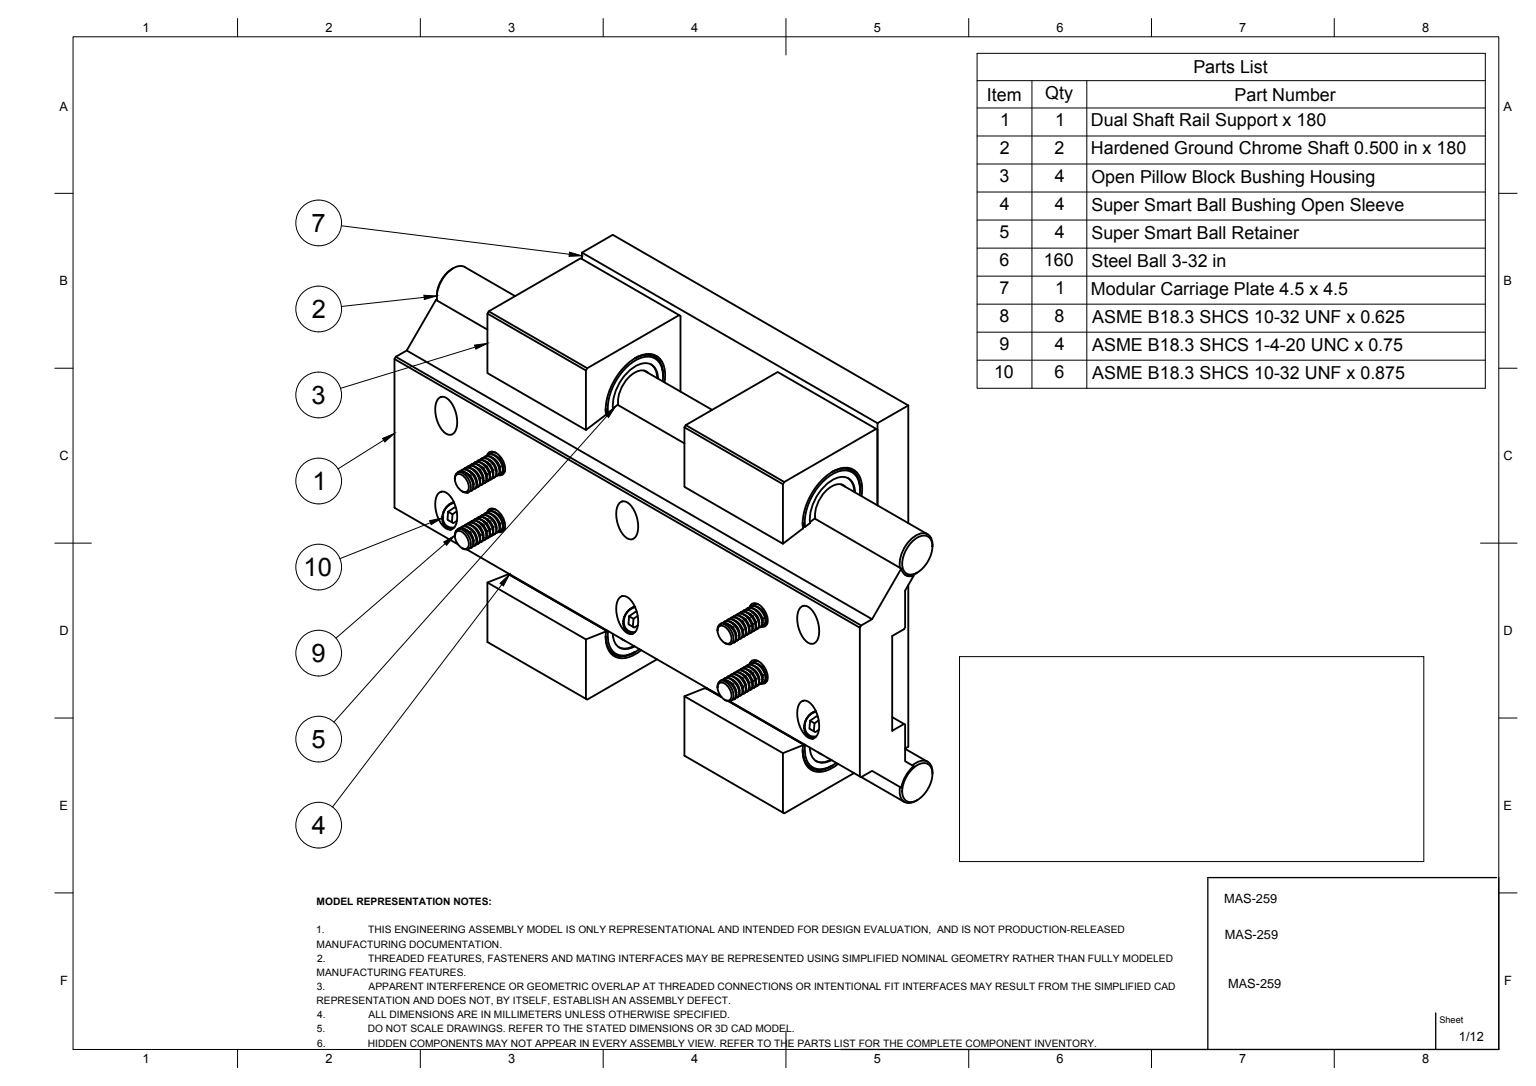
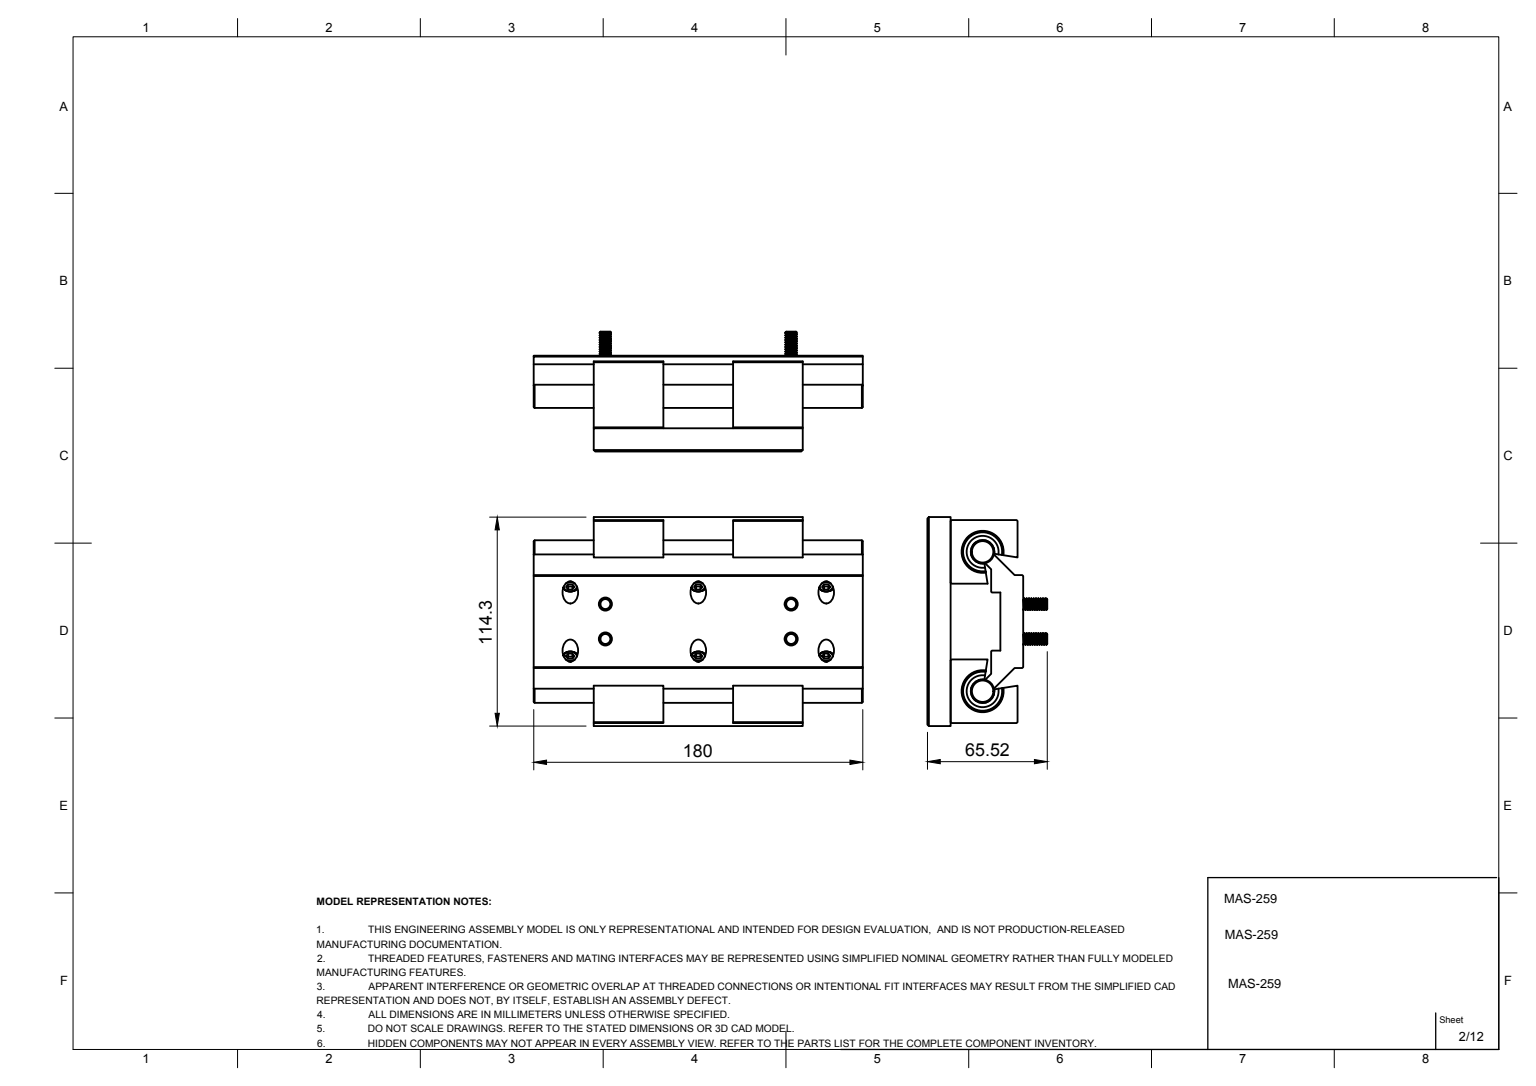
ISO-10303-21;
HEADER;
/* Generated by software containing ST-Developer
 * from STEP Tools, Inc. (www.steptools.com) 
 */

FILE_DESCRIPTION(
/* description */ (''),
/* implementation_level */ '2;1');

FILE_NAME(
/* name */ 'MAS-259',
/* time_stamp */ '2026-10-15T13:30:17-07:00',
/* author */ (''),
/* organization */ (''),
/* preprocessor_version */ 'ST-DEVELOPER v20.2',
/* originating_system */ 'Autodesk Translation Framework v15.15.0.0',
/* authorisation */ '');

FILE_SCHEMA (('AUTOMOTIVE_DESIGN { 1 0 10303 214 3 1 1 }'));
ENDSEC;

DATA;
#10=MECHANICAL_DESIGN_GEOMETRIC_PRESENTATION_REPRESENTATION('',(#1033,#1034,
#1035,#1036,#1037,#1038,#1039,#1040,#1041,#1042),#71795);
#11=ITEM_DEFINED_TRANSFORMATION($,$,#13757,#14849);
#12=ITEM_DEFINED_TRANSFORMATION($,$,#13993,#14850);
#13=ITEM_DEFINED_TRANSFORMATION($,$,#14012,#14851);
#14=ITEM_DEFINED_TRANSFORMATION($,$,#14045,#14852);
#15=ITEM_DEFINED_TRANSFORMATION($,$,#14060,#14853);
#16=ITEM_DEFINED_TRANSFORMATION($,$,#14111,#14854);
#17=ITEM_DEFINED_TRANSFORMATION($,$,#13854,#14855);
#18=ITEM_DEFINED_TRANSFORMATION($,$,#14114,#14856);
#19=ITEM_DEFINED_TRANSFORMATION($,$,#14610,#14857);
#20=ITEM_DEFINED_TRANSFORMATION($,$,#14358,#14858);
#21=ITEM_DEFINED_TRANSFORMATION($,$,#13993,#14859);
#22=ITEM_DEFINED_TRANSFORMATION($,$,#14012,#14860);
#23=ITEM_DEFINED_TRANSFORMATION($,$,#14012,#14861);
#24=ITEM_DEFINED_TRANSFORMATION($,$,#14012,#14862);
#25=ITEM_DEFINED_TRANSFORMATION($,$,#14045,#14863);
#26=ITEM_DEFINED_TRANSFORMATION($,$,#14045,#14864);
#27=ITEM_DEFINED_TRANSFORMATION($,$,#14045,#14865);
#28=ITEM_DEFINED_TRANSFORMATION($,$,#14060,#14866);
#29=ITEM_DEFINED_TRANSFORMATION($,$,#14060,#14867);
#30=ITEM_DEFINED_TRANSFORMATION($,$,#14060,#14868);
#31=ITEM_DEFINED_TRANSFORMATION($,$,#14111,#14869);
#32=ITEM_DEFINED_TRANSFORMATION($,$,#14111,#14870);
#33=ITEM_DEFINED_TRANSFORMATION($,$,#14111,#14871);
#34=ITEM_DEFINED_TRANSFORMATION($,$,#14111,#14872);
#35=ITEM_DEFINED_TRANSFORMATION($,$,#14111,#14873);
#36=ITEM_DEFINED_TRANSFORMATION($,$,#14111,#14874);
#37=ITEM_DEFINED_TRANSFORMATION($,$,#14111,#14875);
#38=ITEM_DEFINED_TRANSFORMATION($,$,#14111,#14876);
#39=ITEM_DEFINED_TRANSFORMATION($,$,#14111,#14877);
#40=ITEM_DEFINED_TRANSFORMATION($,$,#14111,#14878);
#41=ITEM_DEFINED_TRANSFORMATION($,$,#14111,#14879);
#42=ITEM_DEFINED_TRANSFORMATION($,$,#14111,#14880);
#43=ITEM_DEFINED_TRANSFORMATION($,$,#14111,#14881);
#44=ITEM_DEFINED_TRANSFORMATION($,$,#14111,#14882);
#45=ITEM_DEFINED_TRANSFORMATION($,$,#14111,#14883);
#46=ITEM_DEFINED_TRANSFORMATION($,$,#14111,#14884);
#47=ITEM_DEFINED_TRANSFORMATION($,$,#14111,#14885);
#48=ITEM_DEFINED_TRANSFORMATION($,$,#14111,#14886);
#49=ITEM_DEFINED_TRANSFORMATION($,$,#14111,#14887);
#50=ITEM_DEFINED_TRANSFORMATION($,$,#14111,#14888);
#51=ITEM_DEFINED_TRANSFORMATION($,$,#14111,#14889);
#52=ITEM_DEFINED_TRANSFORMATION($,$,#14111,#14890);
#53=ITEM_DEFINED_TRANSFORMATION($,$,#14111,#14891);
#54=ITEM_DEFINED_TRANSFORMATION($,$,#14111,#14892);
#55=ITEM_DEFINED_TRANSFORMATION($,$,#14111,#14893);
#56=ITEM_DEFINED_TRANSFORMATION($,$,#14111,#14894);
#57=ITEM_DEFINED_TRANSFORMATION($,$,#14111,#14895);
#58=ITEM_DEFINED_TRANSFORMATION($,$,#14111,#14896);
#59=ITEM_DEFINED_TRANSFORMATION($,$,#14111,#14897);
#60=ITEM_DEFINED_TRANSFORMATION($,$,#14111,#14898);
#61=ITEM_DEFINED_TRANSFORMATION($,$,#14111,#14899);
#62=ITEM_DEFINED_TRANSFORMATION($,$,#14111,#14900);
#63=ITEM_DEFINED_TRANSFORMATION($,$,#14111,#14901);
#64=ITEM_DEFINED_TRANSFORMATION($,$,#14111,#14902);
#65=ITEM_DEFINED_TRANSFORMATION($,$,#14111,#14903);
#66=ITEM_DEFINED_TRANSFORMATION($,$,#14111,#14904);
#67=ITEM_DEFINED_TRANSFORMATION($,$,#14111,#14905);
#68=ITEM_DEFINED_TRANSFORMATION($,$,#14111,#14906);
#69=ITEM_DEFINED_TRANSFORMATION($,$,#14111,#14907);
#70=ITEM_DEFINED_TRANSFORMATION($,$,#14111,#14908);
#71=ITEM_DEFINED_TRANSFORMATION($,$,#14111,#14909);
#72=ITEM_DEFINED_TRANSFORMATION($,$,#14111,#14910);
#73=ITEM_DEFINED_TRANSFORMATION($,$,#14111,#14911);
#74=ITEM_DEFINED_TRANSFORMATION($,$,#14111,#14912);
#75=ITEM_DEFINED_TRANSFORMATION($,$,#14111,#14913);
#76=ITEM_DEFINED_TRANSFORMATION($,$,#14111,#14914);
#77=ITEM_DEFINED_TRANSFORMATION($,$,#14111,#14915);
#78=ITEM_DEFINED_TRANSFORMATION($,$,#14111,#14916);
#79=ITEM_DEFINED_TRANSFORMATION($,$,#14111,#14917);
#80=ITEM_DEFINED_TRANSFORMATION($,$,#14111,#14918);
#81=ITEM_DEFINED_TRANSFORMATION($,$,#14111,#14919);
#82=ITEM_DEFINED_TRANSFORMATION($,$,#14111,#14920);
#83=ITEM_DEFINED_TRANSFORMATION($,$,#14111,#14921);
#84=ITEM_DEFINED_TRANSFORMATION($,$,#14111,#14922);
#85=ITEM_DEFINED_TRANSFORMATION($,$,#14111,#14923);
#86=ITEM_DEFINED_TRANSFORMATION($,$,#14111,#14924);
#87=ITEM_DEFINED_TRANSFORMATION($,$,#14111,#14925);
#88=ITEM_DEFINED_TRANSFORMATION($,$,#14111,#14926);
#89=ITEM_DEFINED_TRANSFORMATION($,$,#14111,#14927);
#90=ITEM_DEFINED_TRANSFORMATION($,$,#14111,#14928);
#91=ITEM_DEFINED_TRANSFORMATION($,$,#14111,#14929);
#92=ITEM_DEFINED_TRANSFORMATION($,$,#14111,#14930);
#93=ITEM_DEFINED_TRANSFORMATION($,$,#14111,#14931);
#94=ITEM_DEFINED_TRANSFORMATION($,$,#14111,#14932);
#95=ITEM_DEFINED_TRANSFORMATION($,$,#14111,#14933);
#96=ITEM_DEFINED_TRANSFORMATION($,$,#14111,#14934);
#97=ITEM_DEFINED_TRANSFORMATION($,$,#14111,#14935);
#98=ITEM_DEFINED_TRANSFORMATION($,$,#14111,#14936);
#99=ITEM_DEFINED_TRANSFORMATION($,$,#14111,#14937);
#100=ITEM_DEFINED_TRANSFORMATION($,$,#14111,#14938);
#101=ITEM_DEFINED_TRANSFORMATION($,$,#14111,#14939);
#102=ITEM_DEFINED_TRANSFORMATION($,$,#14111,#14940);
#103=ITEM_DEFINED_TRANSFORMATION($,$,#14111,#14941);
#104=ITEM_DEFINED_TRANSFORMATION($,$,#14111,#14942);
#105=ITEM_DEFINED_TRANSFORMATION($,$,#14111,#14943);
#106=ITEM_DEFINED_TRANSFORMATION($,$,#14111,#14944);
#107=ITEM_DEFINED_TRANSFORMATION($,$,#14111,#14945);
#108=ITEM_DEFINED_TRANSFORMATION($,$,#14111,#14946);
#109=ITEM_DEFINED_TRANSFORMATION($,$,#14111,#14947);
#110=ITEM_DEFINED_TRANSFORMATION($,$,#14111,#14948);
#111=ITEM_DEFINED_TRANSFORMATION($,$,#14111,#14949);
#112=ITEM_DEFINED_TRANSFORMATION($,$,#14111,#14950);
#113=ITEM_DEFINED_TRANSFORMATION($,$,#14111,#14951);
#114=ITEM_DEFINED_TRANSFORMATION($,$,#14111,#14952);
#115=ITEM_DEFINED_TRANSFORMATION($,$,#14111,#14953);
#116=ITEM_DEFINED_TRANSFORMATION($,$,#14111,#14954);
#117=ITEM_DEFINED_TRANSFORMATION($,$,#14111,#14955);
#118=ITEM_DEFINED_TRANSFORMATION($,$,#14111,#14956);
#119=ITEM_DEFINED_TRANSFORMATION($,$,#14111,#14957);
#120=ITEM_DEFINED_TRANSFORMATION($,$,#14111,#14958);
#121=ITEM_DEFINED_TRANSFORMATION($,$,#14111,#14959);
#122=ITEM_DEFINED_TRANSFORMATION($,$,#14111,#14960);
#123=ITEM_DEFINED_TRANSFORMATION($,$,#14111,#14961);
#124=ITEM_DEFINED_TRANSFORMATION($,$,#14111,#14962);
#125=ITEM_DEFINED_TRANSFORMATION($,$,#14111,#14963);
#126=ITEM_DEFINED_TRANSFORMATION($,$,#14111,#14964);
#127=ITEM_DEFINED_TRANSFORMATION($,$,#14111,#14965);
#128=ITEM_DEFINED_TRANSFORMATION($,$,#14111,#14966);
#129=ITEM_DEFINED_TRANSFORMATION($,$,#14111,#14967);
#130=ITEM_DEFINED_TRANSFORMATION($,$,#14111,#14968);
#131=ITEM_DEFINED_TRANSFORMATION($,$,#14111,#14969);
#132=ITEM_DEFINED_TRANSFORMATION($,$,#14111,#14970);
#133=ITEM_DEFINED_TRANSFORMATION($,$,#14111,#14971);
#134=ITEM_DEFINED_TRANSFORMATION($,$,#14111,#14972);
#135=ITEM_DEFINED_TRANSFORMATION($,$,#14111,#14973);
#136=ITEM_DEFINED_TRANSFORMATION($,$,#14111,#14974);
#137=ITEM_DEFINED_TRANSFORMATION($,$,#14111,#14975);
#138=ITEM_DEFINED_TRANSFORMATION($,$,#14111,#14976);
#139=ITEM_DEFINED_TRANSFORMATION($,$,#14111,#14977);
#140=ITEM_DEFINED_TRANSFORMATION($,$,#14111,#14978);
#141=ITEM_DEFINED_TRANSFORMATION($,$,#14111,#14979);
#142=ITEM_DEFINED_TRANSFORMATION($,$,#14111,#14980);
#143=ITEM_DEFINED_TRANSFORMATION($,$,#14111,#14981);
#144=ITEM_DEFINED_TRANSFORMATION($,$,#14111,#14982);
#145=ITEM_DEFINED_TRANSFORMATION($,$,#14111,#14983);
#146=ITEM_DEFINED_TRANSFORMATION($,$,#14111,#14984);
#147=ITEM_DEFINED_TRANSFORMATION($,$,#14111,#14985);
#148=ITEM_DEFINED_TRANSFORMATION($,$,#14111,#14986);
#149=ITEM_DEFINED_TRANSFORMATION($,$,#14111,#14987);
#150=ITEM_DEFINED_TRANSFORMATION($,$,#14111,#14988);
#151=ITEM_DEFINED_TRANSFORMATION($,$,#14111,#14989);
#152=ITEM_DEFINED_TRANSFORMATION($,$,#14111,#14990);
#153=ITEM_DEFINED_TRANSFORMATION($,$,#14111,#14991);
#154=ITEM_DEFINED_TRANSFORMATION($,$,#14111,#14992);
#155=ITEM_DEFINED_TRANSFORMATION($,$,#14111,#14993);
#156=ITEM_DEFINED_TRANSFORMATION($,$,#14111,#14994);
#157=ITEM_DEFINED_TRANSFORMATION($,$,#14111,#14995);
#158=ITEM_DEFINED_TRANSFORMATION($,$,#14111,#14996);
#159=ITEM_DEFINED_TRANSFORMATION($,$,#14111,#14997);
#160=ITEM_DEFINED_TRANSFORMATION($,$,#14111,#14998);
#161=ITEM_DEFINED_TRANSFORMATION($,$,#14111,#14999);
#162=ITEM_DEFINED_TRANSFORMATION($,$,#14111,#15000);
#163=ITEM_DEFINED_TRANSFORMATION($,$,#14111,#15001);
#164=ITEM_DEFINED_TRANSFORMATION($,$,#14111,#15002);
#165=ITEM_DEFINED_TRANSFORMATION($,$,#14111,#15003);
#166=ITEM_DEFINED_TRANSFORMATION($,$,#14111,#15004);
#167=ITEM_DEFINED_TRANSFORMATION($,$,#14111,#15005);
#168=ITEM_DEFINED_TRANSFORMATION($,$,#14111,#15006);
#169=ITEM_DEFINED_TRANSFORMATION($,$,#14111,#15007);
#170=ITEM_DEFINED_TRANSFORMATION($,$,#14111,#15008);
#171=ITEM_DEFINED_TRANSFORMATION($,$,#14111,#15009);
#172=ITEM_DEFINED_TRANSFORMATION($,$,#14111,#15010);
#173=ITEM_DEFINED_TRANSFORMATION($,$,#14111,#15011);
#174=ITEM_DEFINED_TRANSFORMATION($,$,#14111,#15012);
#175=ITEM_DEFINED_TRANSFORMATION($,$,#14111,#15013);
#176=ITEM_DEFINED_TRANSFORMATION($,$,#14111,#15014);
#177=ITEM_DEFINED_TRANSFORMATION($,$,#14111,#15015);
#178=ITEM_DEFINED_TRANSFORMATION($,$,#14111,#15016);
#179=ITEM_DEFINED_TRANSFORMATION($,$,#14111,#15017);
#180=ITEM_DEFINED_TRANSFORMATION($,$,#14111,#15018);
#181=ITEM_DEFINED_TRANSFORMATION($,$,#14111,#15019);
#182=ITEM_DEFINED_TRANSFORMATION($,$,#14111,#15020);
#183=ITEM_DEFINED_TRANSFORMATION($,$,#14111,#15021);
#184=ITEM_DEFINED_TRANSFORMATION($,$,#14111,#15022);
#185=ITEM_DEFINED_TRANSFORMATION($,$,#14111,#15023);
#186=ITEM_DEFINED_TRANSFORMATION($,$,#14111,#15024);
#187=ITEM_DEFINED_TRANSFORMATION($,$,#14111,#15025);
#188=ITEM_DEFINED_TRANSFORMATION($,$,#14111,#15026);
#189=ITEM_DEFINED_TRANSFORMATION($,$,#14111,#15027);
#190=ITEM_DEFINED_TRANSFORMATION($,$,#14114,#15028);
#191=ITEM_DEFINED_TRANSFORMATION($,$,#14114,#15029);
#192=ITEM_DEFINED_TRANSFORMATION($,$,#14114,#15030);
#193=ITEM_DEFINED_TRANSFORMATION($,$,#14114,#15031);
#194=ITEM_DEFINED_TRANSFORMATION($,$,#14114,#15032);
#195=ITEM_DEFINED_TRANSFORMATION($,$,#14114,#15033);
#196=ITEM_DEFINED_TRANSFORMATION($,$,#14114,#15034);
#197=ITEM_DEFINED_TRANSFORMATION($,$,#14358,#15035);
#198=ITEM_DEFINED_TRANSFORMATION($,$,#14358,#15036);
#199=ITEM_DEFINED_TRANSFORMATION($,$,#14358,#15037);
#200=ITEM_DEFINED_TRANSFORMATION($,$,#14358,#15038);
#201=ITEM_DEFINED_TRANSFORMATION($,$,#14358,#15039);
#202=ITEM_DEFINED_TRANSFORMATION($,$,#14610,#15040);
#203=ITEM_DEFINED_TRANSFORMATION($,$,#14610,#15041);
#204=ITEM_DEFINED_TRANSFORMATION($,$,#14610,#15042);
#205=(
REPRESENTATION_RELATIONSHIP($,$,#72017,#72016)
REPRESENTATION_RELATIONSHIP_WITH_TRANSFORMATION(#11)
SHAPE_REPRESENTATION_RELATIONSHIP()
);
#206=(
REPRESENTATION_RELATIONSHIP($,$,#72019,#72016)
REPRESENTATION_RELATIONSHIP_WITH_TRANSFORMATION(#12)
SHAPE_REPRESENTATION_RELATIONSHIP()
);
#207=(
REPRESENTATION_RELATIONSHIP($,$,#72020,#72016)
REPRESENTATION_RELATIONSHIP_WITH_TRANSFORMATION(#13)
SHAPE_REPRESENTATION_RELATIONSHIP()
);
#208=(
REPRESENTATION_RELATIONSHIP($,$,#72021,#72016)
REPRESENTATION_RELATIONSHIP_WITH_TRANSFORMATION(#14)
SHAPE_REPRESENTATION_RELATIONSHIP()
);
#209=(
REPRESENTATION_RELATIONSHIP($,$,#72022,#72016)
REPRESENTATION_RELATIONSHIP_WITH_TRANSFORMATION(#15)
SHAPE_REPRESENTATION_RELATIONSHIP()
);
#210=(
REPRESENTATION_RELATIONSHIP($,$,#72023,#72016)
REPRESENTATION_RELATIONSHIP_WITH_TRANSFORMATION(#16)
SHAPE_REPRESENTATION_RELATIONSHIP()
);
#211=(
REPRESENTATION_RELATIONSHIP($,$,#72018,#72016)
REPRESENTATION_RELATIONSHIP_WITH_TRANSFORMATION(#17)
SHAPE_REPRESENTATION_RELATIONSHIP()
);
#212=(
REPRESENTATION_RELATIONSHIP($,$,#72024,#72016)
REPRESENTATION_RELATIONSHIP_WITH_TRANSFORMATION(#18)
SHAPE_REPRESENTATION_RELATIONSHIP()
);
#213=(
REPRESENTATION_RELATIONSHIP($,$,#72026,#72016)
REPRESENTATION_RELATIONSHIP_WITH_TRANSFORMATION(#19)
SHAPE_REPRESENTATION_RELATIONSHIP()
);
#214=(
REPRESENTATION_RELATIONSHIP($,$,#72025,#72016)
REPRESENTATION_RELATIONSHIP_WITH_TRANSFORMATION(#20)
SHAPE_REPRESENTATION_RELATIONSHIP()
);
#215=(
REPRESENTATION_RELATIONSHIP($,$,#72019,#72016)
REPRESENTATION_RELATIONSHIP_WITH_TRANSFORMATION(#21)
SHAPE_REPRESENTATION_RELATIONSHIP()
);
#216=(
REPRESENTATION_RELATIONSHIP($,$,#72020,#72016)
REPRESENTATION_RELATIONSHIP_WITH_TRANSFORMATION(#22)
SHAPE_REPRESENTATION_RELATIONSHIP()
);
#217=(
REPRESENTATION_RELATIONSHIP($,$,#72020,#72016)
REPRESENTATION_RELATIONSHIP_WITH_TRANSFORMATION(#23)
SHAPE_REPRESENTATION_RELATIONSHIP()
);
#218=(
REPRESENTATION_RELATIONSHIP($,$,#72020,#72016)
REPRESENTATION_RELATIONSHIP_WITH_TRANSFORMATION(#24)
SHAPE_REPRESENTATION_RELATIONSHIP()
);
#219=(
REPRESENTATION_RELATIONSHIP($,$,#72021,#72016)
REPRESENTATION_RELATIONSHIP_WITH_TRANSFORMATION(#25)
SHAPE_REPRESENTATION_RELATIONSHIP()
);
#220=(
REPRESENTATION_RELATIONSHIP($,$,#72021,#72016)
REPRESENTATION_RELATIONSHIP_WITH_TRANSFORMATION(#26)
SHAPE_REPRESENTATION_RELATIONSHIP()
);
#221=(
REPRESENTATION_RELATIONSHIP($,$,#72021,#72016)
REPRESENTATION_RELATIONSHIP_WITH_TRANSFORMATION(#27)
SHAPE_REPRESENTATION_RELATIONSHIP()
);
#222=(
REPRESENTATION_RELATIONSHIP($,$,#72022,#72016)
REPRESENTATION_RELATIONSHIP_WITH_TRANSFORMATION(#28)
SHAPE_REPRESENTATION_RELATIONSHIP()
);
#223=(
REPRESENTATION_RELATIONSHIP($,$,#72022,#72016)
REPRESENTATION_RELATIONSHIP_WITH_TRANSFORMATION(#29)
SHAPE_REPRESENTATION_RELATIONSHIP()
);
#224=(
REPRESENTATION_RELATIONSHIP($,$,#72022,#72016)
REPRESENTATION_RELATIONSHIP_WITH_TRANSFORMATION(#30)
SHAPE_REPRESENTATION_RELATIONSHIP()
);
#225=(
REPRESENTATION_RELATIONSHIP($,$,#72023,#72016)
REPRESENTATION_RELATIONSHIP_WITH_TRANSFORMATION(#31)
SHAPE_REPRESENTATION_RELATIONSHIP()
);
#226=(
REPRESENTATION_RELATIONSHIP($,$,#72023,#72016)
REPRESENTATION_RELATIONSHIP_WITH_TRANSFORMATION(#32)
SHAPE_REPRESENTATION_RELATIONSHIP()
);
#227=(
REPRESENTATION_RELATIONSHIP($,$,#72023,#72016)
REPRESENTATION_RELATIONSHIP_WITH_TRANSFORMATION(#33)
SHAPE_REPRESENTATION_RELATIONSHIP()
);
#228=(
REPRESENTATION_RELATIONSHIP($,$,#72023,#72016)
REPRESENTATION_RELATIONSHIP_WITH_TRANSFORMATION(#34)
SHAPE_REPRESENTATION_RELATIONSHIP()
);
#229=(
REPRESENTATION_RELATIONSHIP($,$,#72023,#72016)
REPRESENTATION_RELATIONSHIP_WITH_TRANSFORMATION(#35)
SHAPE_REPRESENTATION_RELATIONSHIP()
);
#230=(
REPRESENTATION_RELATIONSHIP($,$,#72023,#72016)
REPRESENTATION_RELATIONSHIP_WITH_TRANSFORMATION(#36)
SHAPE_REPRESENTATION_RELATIONSHIP()
);
#231=(
REPRESENTATION_RELATIONSHIP($,$,#72023,#72016)
REPRESENTATION_RELATIONSHIP_WITH_TRANSFORMATION(#37)
SHAPE_REPRESENTATION_RELATIONSHIP()
);
#232=(
REPRESENTATION_RELATIONSHIP($,$,#72023,#72016)
REPRESENTATION_RELATIONSHIP_WITH_TRANSFORMATION(#38)
SHAPE_REPRESENTATION_RELATIONSHIP()
);
#233=(
REPRESENTATION_RELATIONSHIP($,$,#72023,#72016)
REPRESENTATION_RELATIONSHIP_WITH_TRANSFORMATION(#39)
SHAPE_REPRESENTATION_RELATIONSHIP()
);
#234=(
REPRESENTATION_RELATIONSHIP($,$,#72023,#72016)
REPRESENTATION_RELATIONSHIP_WITH_TRANSFORMATION(#40)
SHAPE_REPRESENTATION_RELATIONSHIP()
);
#235=(
REPRESENTATION_RELATIONSHIP($,$,#72023,#72016)
REPRESENTATION_RELATIONSHIP_WITH_TRANSFORMATION(#41)
SHAPE_REPRESENTATION_RELATIONSHIP()
);
#236=(
REPRESENTATION_RELATIONSHIP($,$,#72023,#72016)
REPRESENTATION_RELATIONSHIP_WITH_TRANSFORMATION(#42)
SHAPE_REPRESENTATION_RELATIONSHIP()
);
#237=(
REPRESENTATION_RELATIONSHIP($,$,#72023,#72016)
REPRESENTATION_RELATIONSHIP_WITH_TRANSFORMATION(#43)
SHAPE_REPRESENTATION_RELATIONSHIP()
);
#238=(
REPRESENTATION_RELATIONSHIP($,$,#72023,#72016)
REPRESENTATION_RELATIONSHIP_WITH_TRANSFORMATION(#44)
SHAPE_REPRESENTATION_RELATIONSHIP()
);
#239=(
REPRESENTATION_RELATIONSHIP($,$,#72023,#72016)
REPRESENTATION_RELATIONSHIP_WITH_TRANSFORMATION(#45)
SHAPE_REPRESENTATION_RELATIONSHIP()
);
#240=(
REPRESENTATION_RELATIONSHIP($,$,#72023,#72016)
REPRESENTATION_RELATIONSHIP_WITH_TRANSFORMATION(#46)
SHAPE_REPRESENTATION_RELATIONSHIP()
);
#241=(
REPRESENTATION_RELATIONSHIP($,$,#72023,#72016)
REPRESENTATION_RELATIONSHIP_WITH_TRANSFORMATION(#47)
SHAPE_REPRESENTATION_RELATIONSHIP()
);
#242=(
REPRESENTATION_RELATIONSHIP($,$,#72023,#72016)
REPRESENTATION_RELATIONSHIP_WITH_TRANSFORMATION(#48)
SHAPE_REPRESENTATION_RELATIONSHIP()
);
#243=(
REPRESENTATION_RELATIONSHIP($,$,#72023,#72016)
REPRESENTATION_RELATIONSHIP_WITH_TRANSFORMATION(#49)
SHAPE_REPRESENTATION_RELATIONSHIP()
);
#244=(
REPRESENTATION_RELATIONSHIP($,$,#72023,#72016)
REPRESENTATION_RELATIONSHIP_WITH_TRANSFORMATION(#50)
SHAPE_REPRESENTATION_RELATIONSHIP()
);
#245=(
REPRESENTATION_RELATIONSHIP($,$,#72023,#72016)
REPRESENTATION_RELATIONSHIP_WITH_TRANSFORMATION(#51)
SHAPE_REPRESENTATION_RELATIONSHIP()
);
#246=(
REPRESENTATION_RELATIONSHIP($,$,#72023,#72016)
REPRESENTATION_RELATIONSHIP_WITH_TRANSFORMATION(#52)
SHAPE_REPRESENTATION_RELATIONSHIP()
);
#247=(
REPRESENTATION_RELATIONSHIP($,$,#72023,#72016)
REPRESENTATION_RELATIONSHIP_WITH_TRANSFORMATION(#53)
SHAPE_REPRESENTATION_RELATIONSHIP()
);
#248=(
REPRESENTATION_RELATIONSHIP($,$,#72023,#72016)
REPRESENTATION_RELATIONSHIP_WITH_TRANSFORMATION(#54)
SHAPE_REPRESENTATION_RELATIONSHIP()
);
#249=(
REPRESENTATION_RELATIONSHIP($,$,#72023,#72016)
REPRESENTATION_RELATIONSHIP_WITH_TRANSFORMATION(#55)
SHAPE_REPRESENTATION_RELATIONSHIP()
);
#250=(
REPRESENTATION_RELATIONSHIP($,$,#72023,#72016)
REPRESENTATION_RELATIONSHIP_WITH_TRANSFORMATION(#56)
SHAPE_REPRESENTATION_RELATIONSHIP()
);
#251=(
REPRESENTATION_RELATIONSHIP($,$,#72023,#72016)
REPRESENTATION_RELATIONSHIP_WITH_TRANSFORMATION(#57)
SHAPE_REPRESENTATION_RELATIONSHIP()
);
#252=(
REPRESENTATION_RELATIONSHIP($,$,#72023,#72016)
REPRESENTATION_RELATIONSHIP_WITH_TRANSFORMATION(#58)
SHAPE_REPRESENTATION_RELATIONSHIP()
);
#253=(
REPRESENTATION_RELATIONSHIP($,$,#72023,#72016)
REPRESENTATION_RELATIONSHIP_WITH_TRANSFORMATION(#59)
SHAPE_REPRESENTATION_RELATIONSHIP()
);
#254=(
REPRESENTATION_RELATIONSHIP($,$,#72023,#72016)
REPRESENTATION_RELATIONSHIP_WITH_TRANSFORMATION(#60)
SHAPE_REPRESENTATION_RELATIONSHIP()
);
#255=(
REPRESENTATION_RELATIONSHIP($,$,#72023,#72016)
REPRESENTATION_RELATIONSHIP_WITH_TRANSFORMATION(#61)
SHAPE_REPRESENTATION_RELATIONSHIP()
);
#256=(
REPRESENTATION_RELATIONSHIP($,$,#72023,#72016)
REPRESENTATION_RELATIONSHIP_WITH_TRANSFORMATION(#62)
SHAPE_REPRESENTATION_RELATIONSHIP()
);
#257=(
REPRESENTATION_RELATIONSHIP($,$,#72023,#72016)
REPRESENTATION_RELATIONSHIP_WITH_TRANSFORMATION(#63)
SHAPE_REPRESENTATION_RELATIONSHIP()
);
#258=(
REPRESENTATION_RELATIONSHIP($,$,#72023,#72016)
REPRESENTATION_RELATIONSHIP_WITH_TRANSFORMATION(#64)
SHAPE_REPRESENTATION_RELATIONSHIP()
);
#259=(
REPRESENTATION_RELATIONSHIP($,$,#72023,#72016)
REPRESENTATION_RELATIONSHIP_WITH_TRANSFORMATION(#65)
SHAPE_REPRESENTATION_RELATIONSHIP()
);
#260=(
REPRESENTATION_RELATIONSHIP($,$,#72023,#72016)
REPRESENTATION_RELATIONSHIP_WITH_TRANSFORMATION(#66)
SHAPE_REPRESENTATION_RELATIONSHIP()
);
#261=(
REPRESENTATION_RELATIONSHIP($,$,#72023,#72016)
REPRESENTATION_RELATIONSHIP_WITH_TRANSFORMATION(#67)
SHAPE_REPRESENTATION_RELATIONSHIP()
);
#262=(
REPRESENTATION_RELATIONSHIP($,$,#72023,#72016)
REPRESENTATION_RELATIONSHIP_WITH_TRANSFORMATION(#68)
SHAPE_REPRESENTATION_RELATIONSHIP()
);
#263=(
REPRESENTATION_RELATIONSHIP($,$,#72023,#72016)
REPRESENTATION_RELATIONSHIP_WITH_TRANSFORMATION(#69)
SHAPE_REPRESENTATION_RELATIONSHIP()
);
#264=(
REPRESENTATION_RELATIONSHIP($,$,#72023,#72016)
REPRESENTATION_RELATIONSHIP_WITH_TRANSFORMATION(#70)
SHAPE_REPRESENTATION_RELATIONSHIP()
);
#265=(
REPRESENTATION_RELATIONSHIP($,$,#72023,#72016)
REPRESENTATION_RELATIONSHIP_WITH_TRANSFORMATION(#71)
SHAPE_REPRESENTATION_RELATIONSHIP()
);
#266=(
REPRESENTATION_RELATIONSHIP($,$,#72023,#72016)
REPRESENTATION_RELATIONSHIP_WITH_TRANSFORMATION(#72)
SHAPE_REPRESENTATION_RELATIONSHIP()
);
#267=(
REPRESENTATION_RELATIONSHIP($,$,#72023,#72016)
REPRESENTATION_RELATIONSHIP_WITH_TRANSFORMATION(#73)
SHAPE_REPRESENTATION_RELATIONSHIP()
);
#268=(
REPRESENTATION_RELATIONSHIP($,$,#72023,#72016)
REPRESENTATION_RELATIONSHIP_WITH_TRANSFORMATION(#74)
SHAPE_REPRESENTATION_RELATIONSHIP()
);
#269=(
REPRESENTATION_RELATIONSHIP($,$,#72023,#72016)
REPRESENTATION_RELATIONSHIP_WITH_TRANSFORMATION(#75)
SHAPE_REPRESENTATION_RELATIONSHIP()
);
#270=(
REPRESENTATION_RELATIONSHIP($,$,#72023,#72016)
REPRESENTATION_RELATIONSHIP_WITH_TRANSFORMATION(#76)
SHAPE_REPRESENTATION_RELATIONSHIP()
);
#271=(
REPRESENTATION_RELATIONSHIP($,$,#72023,#72016)
REPRESENTATION_RELATIONSHIP_WITH_TRANSFORMATION(#77)
SHAPE_REPRESENTATION_RELATIONSHIP()
);
#272=(
REPRESENTATION_RELATIONSHIP($,$,#72023,#72016)
REPRESENTATION_RELATIONSHIP_WITH_TRANSFORMATION(#78)
SHAPE_REPRESENTATION_RELATIONSHIP()
);
#273=(
REPRESENTATION_RELATIONSHIP($,$,#72023,#72016)
REPRESENTATION_RELATIONSHIP_WITH_TRANSFORMATION(#79)
SHAPE_REPRESENTATION_RELATIONSHIP()
);
#274=(
REPRESENTATION_RELATIONSHIP($,$,#72023,#72016)
REPRESENTATION_RELATIONSHIP_WITH_TRANSFORMATION(#80)
SHAPE_REPRESENTATION_RELATIONSHIP()
);
#275=(
REPRESENTATION_RELATIONSHIP($,$,#72023,#72016)
REPRESENTATION_RELATIONSHIP_WITH_TRANSFORMATION(#81)
SHAPE_REPRESENTATION_RELATIONSHIP()
);
#276=(
REPRESENTATION_RELATIONSHIP($,$,#72023,#72016)
REPRESENTATION_RELATIONSHIP_WITH_TRANSFORMATION(#82)
SHAPE_REPRESENTATION_RELATIONSHIP()
);
#277=(
REPRESENTATION_RELATIONSHIP($,$,#72023,#72016)
REPRESENTATION_RELATIONSHIP_WITH_TRANSFORMATION(#83)
SHAPE_REPRESENTATION_RELATIONSHIP()
);
#278=(
REPRESENTATION_RELATIONSHIP($,$,#72023,#72016)
REPRESENTATION_RELATIONSHIP_WITH_TRANSFORMATION(#84)
SHAPE_REPRESENTATION_RELATIONSHIP()
);
#279=(
REPRESENTATION_RELATIONSHIP($,$,#72023,#72016)
REPRESENTATION_RELATIONSHIP_WITH_TRANSFORMATION(#85)
SHAPE_REPRESENTATION_RELATIONSHIP()
);
#280=(
REPRESENTATION_RELATIONSHIP($,$,#72023,#72016)
REPRESENTATION_RELATIONSHIP_WITH_TRANSFORMATION(#86)
SHAPE_REPRESENTATION_RELATIONSHIP()
);
#281=(
REPRESENTATION_RELATIONSHIP($,$,#72023,#72016)
REPRESENTATION_RELATIONSHIP_WITH_TRANSFORMATION(#87)
SHAPE_REPRESENTATION_RELATIONSHIP()
);
#282=(
REPRESENTATION_RELATIONSHIP($,$,#72023,#72016)
REPRESENTATION_RELATIONSHIP_WITH_TRANSFORMATION(#88)
SHAPE_REPRESENTATION_RELATIONSHIP()
);
#283=(
REPRESENTATION_RELATIONSHIP($,$,#72023,#72016)
REPRESENTATION_RELATIONSHIP_WITH_TRANSFORMATION(#89)
SHAPE_REPRESENTATION_RELATIONSHIP()
);
#284=(
REPRESENTATION_RELATIONSHIP($,$,#72023,#72016)
REPRESENTATION_RELATIONSHIP_WITH_TRANSFORMATION(#90)
SHAPE_REPRESENTATION_RELATIONSHIP()
);
#285=(
REPRESENTATION_RELATIONSHIP($,$,#72023,#72016)
REPRESENTATION_RELATIONSHIP_WITH_TRANSFORMATION(#91)
SHAPE_REPRESENTATION_RELATIONSHIP()
);
#286=(
REPRESENTATION_RELATIONSHIP($,$,#72023,#72016)
REPRESENTATION_RELATIONSHIP_WITH_TRANSFORMATION(#92)
SHAPE_REPRESENTATION_RELATIONSHIP()
);
#287=(
REPRESENTATION_RELATIONSHIP($,$,#72023,#72016)
REPRESENTATION_RELATIONSHIP_WITH_TRANSFORMATION(#93)
SHAPE_REPRESENTATION_RELATIONSHIP()
);
#288=(
REPRESENTATION_RELATIONSHIP($,$,#72023,#72016)
REPRESENTATION_RELATIONSHIP_WITH_TRANSFORMATION(#94)
SHAPE_REPRESENTATION_RELATIONSHIP()
);
#289=(
REPRESENTATION_RELATIONSHIP($,$,#72023,#72016)
REPRESENTATION_RELATIONSHIP_WITH_TRANSFORMATION(#95)
SHAPE_REPRESENTATION_RELATIONSHIP()
);
#290=(
REPRESENTATION_RELATIONSHIP($,$,#72023,#72016)
REPRESENTATION_RELATIONSHIP_WITH_TRANSFORMATION(#96)
SHAPE_REPRESENTATION_RELATIONSHIP()
);
#291=(
REPRESENTATION_RELATIONSHIP($,$,#72023,#72016)
REPRESENTATION_RELATIONSHIP_WITH_TRANSFORMATION(#97)
SHAPE_REPRESENTATION_RELATIONSHIP()
);
#292=(
REPRESENTATION_RELATIONSHIP($,$,#72023,#72016)
REPRESENTATION_RELATIONSHIP_WITH_TRANSFORMATION(#98)
SHAPE_REPRESENTATION_RELATIONSHIP()
);
#293=(
REPRESENTATION_RELATIONSHIP($,$,#72023,#72016)
REPRESENTATION_RELATIONSHIP_WITH_TRANSFORMATION(#99)
SHAPE_REPRESENTATION_RELATIONSHIP()
);
#294=(
REPRESENTATION_RELATIONSHIP($,$,#72023,#72016)
REPRESENTATION_RELATIONSHIP_WITH_TRANSFORMATION(#100)
SHAPE_REPRESENTATION_RELATIONSHIP()
);
#295=(
REPRESENTATION_RELATIONSHIP($,$,#72023,#72016)
REPRESENTATION_RELATIONSHIP_WITH_TRANSFORMATION(#101)
SHAPE_REPRESENTATION_RELATIONSHIP()
);
#296=(
REPRESENTATION_RELATIONSHIP($,$,#72023,#72016)
REPRESENTATION_RELATIONSHIP_WITH_TRANSFORMATION(#102)
SHAPE_REPRESENTATION_RELATIONSHIP()
);
#297=(
REPRESENTATION_RELATIONSHIP($,$,#72023,#72016)
REPRESENTATION_RELATIONSHIP_WITH_TRANSFORMATION(#103)
SHAPE_REPRESENTATION_RELATIONSHIP()
);
#298=(
REPRESENTATION_RELATIONSHIP($,$,#72023,#72016)
REPRESENTATION_RELATIONSHIP_WITH_TRANSFORMATION(#104)
SHAPE_REPRESENTATION_RELATIONSHIP()
);
#299=(
REPRESENTATION_RELATIONSHIP($,$,#72023,#72016)
REPRESENTATION_RELATIONSHIP_WITH_TRANSFORMATION(#105)
SHAPE_REPRESENTATION_RELATIONSHIP()
);
#300=(
REPRESENTATION_RELATIONSHIP($,$,#72023,#72016)
REPRESENTATION_RELATIONSHIP_WITH_TRANSFORMATION(#106)
SHAPE_REPRESENTATION_RELATIONSHIP()
);
#301=(
REPRESENTATION_RELATIONSHIP($,$,#72023,#72016)
REPRESENTATION_RELATIONSHIP_WITH_TRANSFORMATION(#107)
SHAPE_REPRESENTATION_RELATIONSHIP()
);
#302=(
REPRESENTATION_RELATIONSHIP($,$,#72023,#72016)
REPRESENTATION_RELATIONSHIP_WITH_TRANSFORMATION(#108)
SHAPE_REPRESENTATION_RELATIONSHIP()
);
#303=(
REPRESENTATION_RELATIONSHIP($,$,#72023,#72016)
REPRESENTATION_RELATIONSHIP_WITH_TRANSFORMATION(#109)
SHAPE_REPRESENTATION_RELATIONSHIP()
);
#304=(
REPRESENTATION_RELATIONSHIP($,$,#72023,#72016)
REPRESENTATION_RELATIONSHIP_WITH_TRANSFORMATION(#110)
SHAPE_REPRESENTATION_RELATIONSHIP()
);
#305=(
REPRESENTATION_RELATIONSHIP($,$,#72023,#72016)
REPRESENTATION_RELATIONSHIP_WITH_TRANSFORMATION(#111)
SHAPE_REPRESENTATION_RELATIONSHIP()
);
#306=(
REPRESENTATION_RELATIONSHIP($,$,#72023,#72016)
REPRESENTATION_RELATIONSHIP_WITH_TRANSFORMATION(#112)
SHAPE_REPRESENTATION_RELATIONSHIP()
);
#307=(
REPRESENTATION_RELATIONSHIP($,$,#72023,#72016)
REPRESENTATION_RELATIONSHIP_WITH_TRANSFORMATION(#113)
SHAPE_REPRESENTATION_RELATIONSHIP()
);
#308=(
REPRESENTATION_RELATIONSHIP($,$,#72023,#72016)
REPRESENTATION_RELATIONSHIP_WITH_TRANSFORMATION(#114)
SHAPE_REPRESENTATION_RELATIONSHIP()
);
#309=(
REPRESENTATION_RELATIONSHIP($,$,#72023,#72016)
REPRESENTATION_RELATIONSHIP_WITH_TRANSFORMATION(#115)
SHAPE_REPRESENTATION_RELATIONSHIP()
);
#310=(
REPRESENTATION_RELATIONSHIP($,$,#72023,#72016)
REPRESENTATION_RELATIONSHIP_WITH_TRANSFORMATION(#116)
SHAPE_REPRESENTATION_RELATIONSHIP()
);
#311=(
REPRESENTATION_RELATIONSHIP($,$,#72023,#72016)
REPRESENTATION_RELATIONSHIP_WITH_TRANSFORMATION(#117)
SHAPE_REPRESENTATION_RELATIONSHIP()
);
#312=(
REPRESENTATION_RELATIONSHIP($,$,#72023,#72016)
REPRESENTATION_RELATIONSHIP_WITH_TRANSFORMATION(#118)
SHAPE_REPRESENTATION_RELATIONSHIP()
);
#313=(
REPRESENTATION_RELATIONSHIP($,$,#72023,#72016)
REPRESENTATION_RELATIONSHIP_WITH_TRANSFORMATION(#119)
SHAPE_REPRESENTATION_RELATIONSHIP()
);
#314=(
REPRESENTATION_RELATIONSHIP($,$,#72023,#72016)
REPRESENTATION_RELATIONSHIP_WITH_TRANSFORMATION(#120)
SHAPE_REPRESENTATION_RELATIONSHIP()
);
#315=(
REPRESENTATION_RELATIONSHIP($,$,#72023,#72016)
REPRESENTATION_RELATIONSHIP_WITH_TRANSFORMATION(#121)
SHAPE_REPRESENTATION_RELATIONSHIP()
);
#316=(
REPRESENTATION_RELATIONSHIP($,$,#72023,#72016)
REPRESENTATION_RELATIONSHIP_WITH_TRANSFORMATION(#122)
SHAPE_REPRESENTATION_RELATIONSHIP()
);
#317=(
REPRESENTATION_RELATIONSHIP($,$,#72023,#72016)
REPRESENTATION_RELATIONSHIP_WITH_TRANSFORMATION(#123)
SHAPE_REPRESENTATION_RELATIONSHIP()
);
#318=(
REPRESENTATION_RELATIONSHIP($,$,#72023,#72016)
REPRESENTATION_RELATIONSHIP_WITH_TRANSFORMATION(#124)
SHAPE_REPRESENTATION_RELATIONSHIP()
);
#319=(
REPRESENTATION_RELATIONSHIP($,$,#72023,#72016)
REPRESENTATION_RELATIONSHIP_WITH_TRANSFORMATION(#125)
SHAPE_REPRESENTATION_RELATIONSHIP()
);
#320=(
REPRESENTATION_RELATIONSHIP($,$,#72023,#72016)
REPRESENTATION_RELATIONSHIP_WITH_TRANSFORMATION(#126)
SHAPE_REPRESENTATION_RELATIONSHIP()
);
#321=(
REPRESENTATION_RELATIONSHIP($,$,#72023,#72016)
REPRESENTATION_RELATIONSHIP_WITH_TRANSFORMATION(#127)
SHAPE_REPRESENTATION_RELATIONSHIP()
);
#322=(
REPRESENTATION_RELATIONSHIP($,$,#72023,#72016)
REPRESENTATION_RELATIONSHIP_WITH_TRANSFORMATION(#128)
SHAPE_REPRESENTATION_RELATIONSHIP()
);
#323=(
REPRESENTATION_RELATIONSHIP($,$,#72023,#72016)
REPRESENTATION_RELATIONSHIP_WITH_TRANSFORMATION(#129)
SHAPE_REPRESENTATION_RELATIONSHIP()
);
#324=(
REPRESENTATION_RELATIONSHIP($,$,#72023,#72016)
REPRESENTATION_RELATIONSHIP_WITH_TRANSFORMATION(#130)
SHAPE_REPRESENTATION_RELATIONSHIP()
);
#325=(
REPRESENTATION_RELATIONSHIP($,$,#72023,#72016)
REPRESENTATION_RELATIONSHIP_WITH_TRANSFORMATION(#131)
SHAPE_REPRESENTATION_RELATIONSHIP()
);
#326=(
REPRESENTATION_RELATIONSHIP($,$,#72023,#72016)
REPRESENTATION_RELATIONSHIP_WITH_TRANSFORMATION(#132)
SHAPE_REPRESENTATION_RELATIONSHIP()
);
#327=(
REPRESENTATION_RELATIONSHIP($,$,#72023,#72016)
REPRESENTATION_RELATIONSHIP_WITH_TRANSFORMATION(#133)
SHAPE_REPRESENTATION_RELATIONSHIP()
);
#328=(
REPRESENTATION_RELATIONSHIP($,$,#72023,#72016)
REPRESENTATION_RELATIONSHIP_WITH_TRANSFORMATION(#134)
SHAPE_REPRESENTATION_RELATIONSHIP()
);
#329=(
REPRESENTATION_RELATIONSHIP($,$,#72023,#72016)
REPRESENTATION_RELATIONSHIP_WITH_TRANSFORMATION(#135)
SHAPE_REPRESENTATION_RELATIONSHIP()
);
#330=(
REPRESENTATION_RELATIONSHIP($,$,#72023,#72016)
REPRESENTATION_RELATIONSHIP_WITH_TRANSFORMATION(#136)
SHAPE_REPRESENTATION_RELATIONSHIP()
);
#331=(
REPRESENTATION_RELATIONSHIP($,$,#72023,#72016)
REPRESENTATION_RELATIONSHIP_WITH_TRANSFORMATION(#137)
SHAPE_REPRESENTATION_RELATIONSHIP()
);
#332=(
REPRESENTATION_RELATIONSHIP($,$,#72023,#72016)
REPRESENTATION_RELATIONSHIP_WITH_TRANSFORMATION(#138)
SHAPE_REPRESENTATION_RELATIONSHIP()
);
#333=(
REPRESENTATION_RELATIONSHIP($,$,#72023,#72016)
REPRESENTATION_RELATIONSHIP_WITH_TRANSFORMATION(#139)
SHAPE_REPRESENTATION_RELATIONSHIP()
);
#334=(
REPRESENTATION_RELATIONSHIP($,$,#72023,#72016)
REPRESENTATION_RELATIONSHIP_WITH_TRANSFORMATION(#140)
SHAPE_REPRESENTATION_RELATIONSHIP()
);
#335=(
REPRESENTATION_RELATIONSHIP($,$,#72023,#72016)
REPRESENTATION_RELATIONSHIP_WITH_TRANSFORMATION(#141)
SHAPE_REPRESENTATION_RELATIONSHIP()
);
#336=(
REPRESENTATION_RELATIONSHIP($,$,#72023,#72016)
REPRESENTATION_RELATIONSHIP_WITH_TRANSFORMATION(#142)
SHAPE_REPRESENTATION_RELATIONSHIP()
);
#337=(
REPRESENTATION_RELATIONSHIP($,$,#72023,#72016)
REPRESENTATION_RELATIONSHIP_WITH_TRANSFORMATION(#143)
SHAPE_REPRESENTATION_RELATIONSHIP()
);
#338=(
REPRESENTATION_RELATIONSHIP($,$,#72023,#72016)
REPRESENTATION_RELATIONSHIP_WITH_TRANSFORMATION(#144)
SHAPE_REPRESENTATION_RELATIONSHIP()
);
#339=(
REPRESENTATION_RELATIONSHIP($,$,#72023,#72016)
REPRESENTATION_RELATIONSHIP_WITH_TRANSFORMATION(#145)
SHAPE_REPRESENTATION_RELATIONSHIP()
);
#340=(
REPRESENTATION_RELATIONSHIP($,$,#72023,#72016)
REPRESENTATION_RELATIONSHIP_WITH_TRANSFORMATION(#146)
SHAPE_REPRESENTATION_RELATIONSHIP()
);
#341=(
REPRESENTATION_RELATIONSHIP($,$,#72023,#72016)
REPRESENTATION_RELATIONSHIP_WITH_TRANSFORMATION(#147)
SHAPE_REPRESENTATION_RELATIONSHIP()
);
#342=(
REPRESENTATION_RELATIONSHIP($,$,#72023,#72016)
REPRESENTATION_RELATIONSHIP_WITH_TRANSFORMATION(#148)
SHAPE_REPRESENTATION_RELATIONSHIP()
);
#343=(
REPRESENTATION_RELATIONSHIP($,$,#72023,#72016)
REPRESENTATION_RELATIONSHIP_WITH_TRANSFORMATION(#149)
SHAPE_REPRESENTATION_RELATIONSHIP()
);
#344=(
REPRESENTATION_RELATIONSHIP($,$,#72023,#72016)
REPRESENTATION_RELATIONSHIP_WITH_TRANSFORMATION(#150)
SHAPE_REPRESENTATION_RELATIONSHIP()
);
#345=(
REPRESENTATION_RELATIONSHIP($,$,#72023,#72016)
REPRESENTATION_RELATIONSHIP_WITH_TRANSFORMATION(#151)
SHAPE_REPRESENTATION_RELATIONSHIP()
);
#346=(
REPRESENTATION_RELATIONSHIP($,$,#72023,#72016)
REPRESENTATION_RELATIONSHIP_WITH_TRANSFORMATION(#152)
SHAPE_REPRESENTATION_RELATIONSHIP()
);
#347=(
REPRESENTATION_RELATIONSHIP($,$,#72023,#72016)
REPRESENTATION_RELATIONSHIP_WITH_TRANSFORMATION(#153)
SHAPE_REPRESENTATION_RELATIONSHIP()
);
#348=(
REPRESENTATION_RELATIONSHIP($,$,#72023,#72016)
REPRESENTATION_RELATIONSHIP_WITH_TRANSFORMATION(#154)
SHAPE_REPRESENTATION_RELATIONSHIP()
);
#349=(
REPRESENTATION_RELATIONSHIP($,$,#72023,#72016)
REPRESENTATION_RELATIONSHIP_WITH_TRANSFORMATION(#155)
SHAPE_REPRESENTATION_RELATIONSHIP()
);
#350=(
REPRESENTATION_RELATIONSHIP($,$,#72023,#72016)
REPRESENTATION_RELATIONSHIP_WITH_TRANSFORMATION(#156)
SHAPE_REPRESENTATION_RELATIONSHIP()
);
#351=(
REPRESENTATION_RELATIONSHIP($,$,#72023,#72016)
REPRESENTATION_RELATIONSHIP_WITH_TRANSFORMATION(#157)
SHAPE_REPRESENTATION_RELATIONSHIP()
);
#352=(
REPRESENTATION_RELATIONSHIP($,$,#72023,#72016)
REPRESENTATION_RELATIONSHIP_WITH_TRANSFORMATION(#158)
SHAPE_REPRESENTATION_RELATIONSHIP()
);
#353=(
REPRESENTATION_RELATIONSHIP($,$,#72023,#72016)
REPRESENTATION_RELATIONSHIP_WITH_TRANSFORMATION(#159)
SHAPE_REPRESENTATION_RELATIONSHIP()
);
#354=(
REPRESENTATION_RELATIONSHIP($,$,#72023,#72016)
REPRESENTATION_RELATIONSHIP_WITH_TRANSFORMATION(#160)
SHAPE_REPRESENTATION_RELATIONSHIP()
);
#355=(
REPRESENTATION_RELATIONSHIP($,$,#72023,#72016)
REPRESENTATION_RELATIONSHIP_WITH_TRANSFORMATION(#161)
SHAPE_REPRESENTATION_RELATIONSHIP()
);
#356=(
REPRESENTATION_RELATIONSHIP($,$,#72023,#72016)
REPRESENTATION_RELATIONSHIP_WITH_TRANSFORMATION(#162)
SHAPE_REPRESENTATION_RELATIONSHIP()
);
#357=(
REPRESENTATION_RELATIONSHIP($,$,#72023,#72016)
REPRESENTATION_RELATIONSHIP_WITH_TRANSFORMATION(#163)
SHAPE_REPRESENTATION_RELATIONSHIP()
);
#358=(
REPRESENTATION_RELATIONSHIP($,$,#72023,#72016)
REPRESENTATION_RELATIONSHIP_WITH_TRANSFORMATION(#164)
SHAPE_REPRESENTATION_RELATIONSHIP()
);
#359=(
REPRESENTATION_RELATIONSHIP($,$,#72023,#72016)
REPRESENTATION_RELATIONSHIP_WITH_TRANSFORMATION(#165)
SHAPE_REPRESENTATION_RELATIONSHIP()
);
#360=(
REPRESENTATION_RELATIONSHIP($,$,#72023,#72016)
REPRESENTATION_RELATIONSHIP_WITH_TRANSFORMATION(#166)
SHAPE_REPRESENTATION_RELATIONSHIP()
);
#361=(
REPRESENTATION_RELATIONSHIP($,$,#72023,#72016)
REPRESENTATION_RELATIONSHIP_WITH_TRANSFORMATION(#167)
SHAPE_REPRESENTATION_RELATIONSHIP()
);
#362=(
REPRESENTATION_RELATIONSHIP($,$,#72023,#72016)
REPRESENTATION_RELATIONSHIP_WITH_TRANSFORMATION(#168)
SHAPE_REPRESENTATION_RELATIONSHIP()
);
#363=(
REPRESENTATION_RELATIONSHIP($,$,#72023,#72016)
REPRESENTATION_RELATIONSHIP_WITH_TRANSFORMATION(#169)
SHAPE_REPRESENTATION_RELATIONSHIP()
);
#364=(
REPRESENTATION_RELATIONSHIP($,$,#72023,#72016)
REPRESENTATION_RELATIONSHIP_WITH_TRANSFORMATION(#170)
SHAPE_REPRESENTATION_RELATIONSHIP()
);
#365=(
REPRESENTATION_RELATIONSHIP($,$,#72023,#72016)
REPRESENTATION_RELATIONSHIP_WITH_TRANSFORMATION(#171)
SHAPE_REPRESENTATION_RELATIONSHIP()
);
#366=(
REPRESENTATION_RELATIONSHIP($,$,#72023,#72016)
REPRESENTATION_RELATIONSHIP_WITH_TRANSFORMATION(#172)
SHAPE_REPRESENTATION_RELATIONSHIP()
);
#367=(
REPRESENTATION_RELATIONSHIP($,$,#72023,#72016)
REPRESENTATION_RELATIONSHIP_WITH_TRANSFORMATION(#173)
SHAPE_REPRESENTATION_RELATIONSHIP()
);
#368=(
REPRESENTATION_RELATIONSHIP($,$,#72023,#72016)
REPRESENTATION_RELATIONSHIP_WITH_TRANSFORMATION(#174)
SHAPE_REPRESENTATION_RELATIONSHIP()
);
#369=(
REPRESENTATION_RELATIONSHIP($,$,#72023,#72016)
REPRESENTATION_RELATIONSHIP_WITH_TRANSFORMATION(#175)
SHAPE_REPRESENTATION_RELATIONSHIP()
);
#370=(
REPRESENTATION_RELATIONSHIP($,$,#72023,#72016)
REPRESENTATION_RELATIONSHIP_WITH_TRANSFORMATION(#176)
SHAPE_REPRESENTATION_RELATIONSHIP()
);
#371=(
REPRESENTATION_RELATIONSHIP($,$,#72023,#72016)
REPRESENTATION_RELATIONSHIP_WITH_TRANSFORMATION(#177)
SHAPE_REPRESENTATION_RELATIONSHIP()
);
#372=(
REPRESENTATION_RELATIONSHIP($,$,#72023,#72016)
REPRESENTATION_RELATIONSHIP_WITH_TRANSFORMATION(#178)
SHAPE_REPRESENTATION_RELATIONSHIP()
);
#373=(
REPRESENTATION_RELATIONSHIP($,$,#72023,#72016)
REPRESENTATION_RELATIONSHIP_WITH_TRANSFORMATION(#179)
SHAPE_REPRESENTATION_RELATIONSHIP()
);
#374=(
REPRESENTATION_RELATIONSHIP($,$,#72023,#72016)
REPRESENTATION_RELATIONSHIP_WITH_TRANSFORMATION(#180)
SHAPE_REPRESENTATION_RELATIONSHIP()
);
#375=(
REPRESENTATION_RELATIONSHIP($,$,#72023,#72016)
REPRESENTATION_RELATIONSHIP_WITH_TRANSFORMATION(#181)
SHAPE_REPRESENTATION_RELATIONSHIP()
);
#376=(
REPRESENTATION_RELATIONSHIP($,$,#72023,#72016)
REPRESENTATION_RELATIONSHIP_WITH_TRANSFORMATION(#182)
SHAPE_REPRESENTATION_RELATIONSHIP()
);
#377=(
REPRESENTATION_RELATIONSHIP($,$,#72023,#72016)
REPRESENTATION_RELATIONSHIP_WITH_TRANSFORMATION(#183)
SHAPE_REPRESENTATION_RELATIONSHIP()
);
#378=(
REPRESENTATION_RELATIONSHIP($,$,#72023,#72016)
REPRESENTATION_RELATIONSHIP_WITH_TRANSFORMATION(#184)
SHAPE_REPRESENTATION_RELATIONSHIP()
);
#379=(
REPRESENTATION_RELATIONSHIP($,$,#72023,#72016)
REPRESENTATION_RELATIONSHIP_WITH_TRANSFORMATION(#185)
SHAPE_REPRESENTATION_RELATIONSHIP()
);
#380=(
REPRESENTATION_RELATIONSHIP($,$,#72023,#72016)
REPRESENTATION_RELATIONSHIP_WITH_TRANSFORMATION(#186)
SHAPE_REPRESENTATION_RELATIONSHIP()
);
#381=(
REPRESENTATION_RELATIONSHIP($,$,#72023,#72016)
REPRESENTATION_RELATIONSHIP_WITH_TRANSFORMATION(#187)
SHAPE_REPRESENTATION_RELATIONSHIP()
);
#382=(
REPRESENTATION_RELATIONSHIP($,$,#72023,#72016)
REPRESENTATION_RELATIONSHIP_WITH_TRANSFORMATION(#188)
SHAPE_REPRESENTATION_RELATIONSHIP()
);
#383=(
REPRESENTATION_RELATIONSHIP($,$,#72023,#72016)
REPRESENTATION_RELATIONSHIP_WITH_TRANSFORMATION(#189)
SHAPE_REPRESENTATION_RELATIONSHIP()
);
#384=(
REPRESENTATION_RELATIONSHIP($,$,#72024,#72016)
REPRESENTATION_RELATIONSHIP_WITH_TRANSFORMATION(#190)
SHAPE_REPRESENTATION_RELATIONSHIP()
);
#385=(
REPRESENTATION_RELATIONSHIP($,$,#72024,#72016)
REPRESENTATION_RELATIONSHIP_WITH_TRANSFORMATION(#191)
SHAPE_REPRESENTATION_RELATIONSHIP()
);
#386=(
REPRESENTATION_RELATIONSHIP($,$,#72024,#72016)
REPRESENTATION_RELATIONSHIP_WITH_TRANSFORMATION(#192)
SHAPE_REPRESENTATION_RELATIONSHIP()
);
#387=(
REPRESENTATION_RELATIONSHIP($,$,#72024,#72016)
REPRESENTATION_RELATIONSHIP_WITH_TRANSFORMATION(#193)
SHAPE_REPRESENTATION_RELATIONSHIP()
);
#388=(
REPRESENTATION_RELATIONSHIP($,$,#72024,#72016)
REPRESENTATION_RELATIONSHIP_WITH_TRANSFORMATION(#194)
SHAPE_REPRESENTATION_RELATIONSHIP()
);
#389=(
REPRESENTATION_RELATIONSHIP($,$,#72024,#72016)
REPRESENTATION_RELATIONSHIP_WITH_TRANSFORMATION(#195)
SHAPE_REPRESENTATION_RELATIONSHIP()
);
#390=(
REPRESENTATION_RELATIONSHIP($,$,#72024,#72016)
REPRESENTATION_RELATIONSHIP_WITH_TRANSFORMATION(#196)
SHAPE_REPRESENTATION_RELATIONSHIP()
);
#391=(
REPRESENTATION_RELATIONSHIP($,$,#72025,#72016)
REPRESENTATION_RELATIONSHIP_WITH_TRANSFORMATION(#197)
SHAPE_REPRESENTATION_RELATIONSHIP()
);
#392=(
REPRESENTATION_RELATIONSHIP($,$,#72025,#72016)
REPRESENTATION_RELATIONSHIP_WITH_TRANSFORMATION(#198)
SHAPE_REPRESENTATION_RELATIONSHIP()
);
#393=(
REPRESENTATION_RELATIONSHIP($,$,#72025,#72016)
REPRESENTATION_RELATIONSHIP_WITH_TRANSFORMATION(#199)
SHAPE_REPRESENTATION_RELATIONSHIP()
);
#394=(
REPRESENTATION_RELATIONSHIP($,$,#72025,#72016)
REPRESENTATION_RELATIONSHIP_WITH_TRANSFORMATION(#200)
SHAPE_REPRESENTATION_RELATIONSHIP()
);
#395=(
REPRESENTATION_RELATIONSHIP($,$,#72025,#72016)
REPRESENTATION_RELATIONSHIP_WITH_TRANSFORMATION(#201)
SHAPE_REPRESENTATION_RELATIONSHIP()
);
#396=(
REPRESENTATION_RELATIONSHIP($,$,#72026,#72016)
REPRESENTATION_RELATIONSHIP_WITH_TRANSFORMATION(#202)
SHAPE_REPRESENTATION_RELATIONSHIP()
);
#397=(
REPRESENTATION_RELATIONSHIP($,$,#72026,#72016)
REPRESENTATION_RELATIONSHIP_WITH_TRANSFORMATION(#203)
SHAPE_REPRESENTATION_RELATIONSHIP()
);
#398=(
REPRESENTATION_RELATIONSHIP($,$,#72026,#72016)
REPRESENTATION_RELATIONSHIP_WITH_TRANSFORMATION(#204)
SHAPE_REPRESENTATION_RELATIONSHIP()
);
#399=CONTEXT_DEPENDENT_SHAPE_REPRESENTATION(#205,#71822);
#400=CONTEXT_DEPENDENT_SHAPE_REPRESENTATION(#206,#71823);
#401=CONTEXT_DEPENDENT_SHAPE_REPRESENTATION(#207,#71824);
#402=CONTEXT_DEPENDENT_SHAPE_REPRESENTATION(#208,#71825);
#403=CONTEXT_DEPENDENT_SHAPE_REPRESENTATION(#209,#71826);
#404=CONTEXT_DEPENDENT_SHAPE_REPRESENTATION(#210,#71827);
#405=CONTEXT_DEPENDENT_SHAPE_REPRESENTATION(#211,#71828);
#406=CONTEXT_DEPENDENT_SHAPE_REPRESENTATION(#212,#71829);
#407=CONTEXT_DEPENDENT_SHAPE_REPRESENTATION(#213,#71830);
#408=CONTEXT_DEPENDENT_SHAPE_REPRESENTATION(#214,#71831);
#409=CONTEXT_DEPENDENT_SHAPE_REPRESENTATION(#215,#71832);
#410=CONTEXT_DEPENDENT_SHAPE_REPRESENTATION(#216,#71833);
#411=CONTEXT_DEPENDENT_SHAPE_REPRESENTATION(#217,#71834);
#412=CONTEXT_DEPENDENT_SHAPE_REPRESENTATION(#218,#71835);
#413=CONTEXT_DEPENDENT_SHAPE_REPRESENTATION(#219,#71836);
#414=CONTEXT_DEPENDENT_SHAPE_REPRESENTATION(#220,#71837);
#415=CONTEXT_DEPENDENT_SHAPE_REPRESENTATION(#221,#71838);
#416=CONTEXT_DEPENDENT_SHAPE_REPRESENTATION(#222,#71839);
#417=CONTEXT_DEPENDENT_SHAPE_REPRESENTATION(#223,#71840);
#418=CONTEXT_DEPENDENT_SHAPE_REPRESENTATION(#224,#71841);
#419=CONTEXT_DEPENDENT_SHAPE_REPRESENTATION(#225,#71842);
#420=CONTEXT_DEPENDENT_SHAPE_REPRESENTATION(#226,#71843);
#421=CONTEXT_DEPENDENT_SHAPE_REPRESENTATION(#227,#71844);
#422=CONTEXT_DEPENDENT_SHAPE_REPRESENTATION(#228,#71845);
#423=CONTEXT_DEPENDENT_SHAPE_REPRESENTATION(#229,#71846);
#424=CONTEXT_DEPENDENT_SHAPE_REPRESENTATION(#230,#71847);
#425=CONTEXT_DEPENDENT_SHAPE_REPRESENTATION(#231,#71848);
#426=CONTEXT_DEPENDENT_SHAPE_REPRESENTATION(#232,#71849);
#427=CONTEXT_DEPENDENT_SHAPE_REPRESENTATION(#233,#71850);
#428=CONTEXT_DEPENDENT_SHAPE_REPRESENTATION(#234,#71851);
#429=CONTEXT_DEPENDENT_SHAPE_REPRESENTATION(#235,#71852);
#430=CONTEXT_DEPENDENT_SHAPE_REPRESENTATION(#236,#71853);
#431=CONTEXT_DEPENDENT_SHAPE_REPRESENTATION(#237,#71854);
#432=CONTEXT_DEPENDENT_SHAPE_REPRESENTATION(#238,#71855);
#433=CONTEXT_DEPENDENT_SHAPE_REPRESENTATION(#239,#71856);
#434=CONTEXT_DEPENDENT_SHAPE_REPRESENTATION(#240,#71857);
#435=CONTEXT_DEPENDENT_SHAPE_REPRESENTATION(#241,#71858);
#436=CONTEXT_DEPENDENT_SHAPE_REPRESENTATION(#242,#71859);
#437=CONTEXT_DEPENDENT_SHAPE_REPRESENTATION(#243,#71860);
#438=CONTEXT_DEPENDENT_SHAPE_REPRESENTATION(#244,#71861);
#439=CONTEXT_DEPENDENT_SHAPE_REPRESENTATION(#245,#71862);
#440=CONTEXT_DEPENDENT_SHAPE_REPRESENTATION(#246,#71863);
#441=CONTEXT_DEPENDENT_SHAPE_REPRESENTATION(#247,#71864);
#442=CONTEXT_DEPENDENT_SHAPE_REPRESENTATION(#248,#71865);
#443=CONTEXT_DEPENDENT_SHAPE_REPRESENTATION(#249,#71866);
#444=CONTEXT_DEPENDENT_SHAPE_REPRESENTATION(#250,#71867);
#445=CONTEXT_DEPENDENT_SHAPE_REPRESENTATION(#251,#71868);
#446=CONTEXT_DEPENDENT_SHAPE_REPRESENTATION(#252,#71869);
#447=CONTEXT_DEPENDENT_SHAPE_REPRESENTATION(#253,#71870);
#448=CONTEXT_DEPENDENT_SHAPE_REPRESENTATION(#254,#71871);
#449=CONTEXT_DEPENDENT_SHAPE_REPRESENTATION(#255,#71872);
#450=CONTEXT_DEPENDENT_SHAPE_REPRESENTATION(#256,#71873);
#451=CONTEXT_DEPENDENT_SHAPE_REPRESENTATION(#257,#71874);
#452=CONTEXT_DEPENDENT_SHAPE_REPRESENTATION(#258,#71875);
#453=CONTEXT_DEPENDENT_SHAPE_REPRESENTATION(#259,#71876);
#454=CONTEXT_DEPENDENT_SHAPE_REPRESENTATION(#260,#71877);
#455=CONTEXT_DEPENDENT_SHAPE_REPRESENTATION(#261,#71878);
#456=CONTEXT_DEPENDENT_SHAPE_REPRESENTATION(#262,#71879);
#457=CONTEXT_DEPENDENT_SHAPE_REPRESENTATION(#263,#71880);
#458=CONTEXT_DEPENDENT_SHAPE_REPRESENTATION(#264,#71881);
#459=CONTEXT_DEPENDENT_SHAPE_REPRESENTATION(#265,#71882);
#460=CONTEXT_DEPENDENT_SHAPE_REPRESENTATION(#266,#71883);
#461=CONTEXT_DEPENDENT_SHAPE_REPRESENTATION(#267,#71884);
#462=CONTEXT_DEPENDENT_SHAPE_REPRESENTATION(#268,#71885);
#463=CONTEXT_DEPENDENT_SHAPE_REPRESENTATION(#269,#71886);
#464=CONTEXT_DEPENDENT_SHAPE_REPRESENTATION(#270,#71887);
#465=CONTEXT_DEPENDENT_SHAPE_REPRESENTATION(#271,#71888);
#466=CONTEXT_DEPENDENT_SHAPE_REPRESENTATION(#272,#71889);
#467=CONTEXT_DEPENDENT_SHAPE_REPRESENTATION(#273,#71890);
#468=CONTEXT_DEPENDENT_SHAPE_REPRESENTATION(#274,#71891);
#469=CONTEXT_DEPENDENT_SHAPE_REPRESENTATION(#275,#71892);
#470=CONTEXT_DEPENDENT_SHAPE_REPRESENTATION(#276,#71893);
#471=CONTEXT_DEPENDENT_SHAPE_REPRESENTATION(#277,#71894);
#472=CONTEXT_DEPENDENT_SHAPE_REPRESENTATION(#278,#71895);
#473=CONTEXT_DEPENDENT_SHAPE_REPRESENTATION(#279,#71896);
#474=CONTEXT_DEPENDENT_SHAPE_REPRESENTATION(#280,#71897);
#475=CONTEXT_DEPENDENT_SHAPE_REPRESENTATION(#281,#71898);
#476=CONTEXT_DEPENDENT_SHAPE_REPRESENTATION(#282,#71899);
#477=CONTEXT_DEPENDENT_SHAPE_REPRESENTATION(#283,#71900);
#478=CONTEXT_DEPENDENT_SHAPE_REPRESENTATION(#284,#71901);
#479=CONTEXT_DEPENDENT_SHAPE_REPRESENTATION(#285,#71902);
#480=CONTEXT_DEPENDENT_SHAPE_REPRESENTATION(#286,#71903);
#481=CONTEXT_DEPENDENT_SHAPE_REPRESENTATION(#287,#71904);
#482=CONTEXT_DEPENDENT_SHAPE_REPRESENTATION(#288,#71905);
#483=CONTEXT_DEPENDENT_SHAPE_REPRESENTATION(#289,#71906);
#484=CONTEXT_DEPENDENT_SHAPE_REPRESENTATION(#290,#71907);
#485=CONTEXT_DEPENDENT_SHAPE_REPRESENTATION(#291,#71908);
#486=CONTEXT_DEPENDENT_SHAPE_REPRESENTATION(#292,#71909);
#487=CONTEXT_DEPENDENT_SHAPE_REPRESENTATION(#293,#71910);
#488=CONTEXT_DEPENDENT_SHAPE_REPRESENTATION(#294,#71911);
#489=CONTEXT_DEPENDENT_SHAPE_REPRESENTATION(#295,#71912);
#490=CONTEXT_DEPENDENT_SHAPE_REPRESENTATION(#296,#71913);
#491=CONTEXT_DEPENDENT_SHAPE_REPRESENTATION(#297,#71914);
#492=CONTEXT_DEPENDENT_SHAPE_REPRESENTATION(#298,#71915);
#493=CONTEXT_DEPENDENT_SHAPE_REPRESENTATION(#299,#71916);
#494=CONTEXT_DEPENDENT_SHAPE_REPRESENTATION(#300,#71917);
#495=CONTEXT_DEPENDENT_SHAPE_REPRESENTATION(#301,#71918);
#496=CONTEXT_DEPENDENT_SHAPE_REPRESENTATION(#302,#71919);
#497=CONTEXT_DEPENDENT_SHAPE_REPRESENTATION(#303,#71920);
#498=CONTEXT_DEPENDENT_SHAPE_REPRESENTATION(#304,#71921);
#499=CONTEXT_DEPENDENT_SHAPE_REPRESENTATION(#305,#71922);
#500=CONTEXT_DEPENDENT_SHAPE_REPRESENTATION(#306,#71923);
#501=CONTEXT_DEPENDENT_SHAPE_REPRESENTATION(#307,#71924);
#502=CONTEXT_DEPENDENT_SHAPE_REPRESENTATION(#308,#71925);
#503=CONTEXT_DEPENDENT_SHAPE_REPRESENTATION(#309,#71926);
#504=CONTEXT_DEPENDENT_SHAPE_REPRESENTATION(#310,#71927);
#505=CONTEXT_DEPENDENT_SHAPE_REPRESENTATION(#311,#71928);
#506=CONTEXT_DEPENDENT_SHAPE_REPRESENTATION(#312,#71929);
#507=CONTEXT_DEPENDENT_SHAPE_REPRESENTATION(#313,#71930);
#508=CONTEXT_DEPENDENT_SHAPE_REPRESENTATION(#314,#71931);
#509=CONTEXT_DEPENDENT_SHAPE_REPRESENTATION(#315,#71932);
#510=CONTEXT_DEPENDENT_SHAPE_REPRESENTATION(#316,#71933);
#511=CONTEXT_DEPENDENT_SHAPE_REPRESENTATION(#317,#71934);
#512=CONTEXT_DEPENDENT_SHAPE_REPRESENTATION(#318,#71935);
#513=CONTEXT_DEPENDENT_SHAPE_REPRESENTATION(#319,#71936);
#514=CONTEXT_DEPENDENT_SHAPE_REPRESENTATION(#320,#71937);
#515=CONTEXT_DEPENDENT_SHAPE_REPRESENTATION(#321,#71938);
#516=CONTEXT_DEPENDENT_SHAPE_REPRESENTATION(#322,#71939);
#517=CONTEXT_DEPENDENT_SHAPE_REPRESENTATION(#323,#71940);
#518=CONTEXT_DEPENDENT_SHAPE_REPRESENTATION(#324,#71941);
#519=CONTEXT_DEPENDENT_SHAPE_REPRESENTATION(#325,#71942);
#520=CONTEXT_DEPENDENT_SHAPE_REPRESENTATION(#326,#71943);
#521=CONTEXT_DEPENDENT_SHAPE_REPRESENTATION(#327,#71944);
#522=CONTEXT_DEPENDENT_SHAPE_REPRESENTATION(#328,#71945);
#523=CONTEXT_DEPENDENT_SHAPE_REPRESENTATION(#329,#71946);
#524=CONTEXT_DEPENDENT_SHAPE_REPRESENTATION(#330,#71947);
#525=CONTEXT_DEPENDENT_SHAPE_REPRESENTATION(#331,#71948);
#526=CONTEXT_DEPENDENT_SHAPE_REPRESENTATION(#332,#71949);
#527=CONTEXT_DEPENDENT_SHAPE_REPRESENTATION(#333,#71950);
#528=CONTEXT_DEPENDENT_SHAPE_REPRESENTATION(#334,#71951);
#529=CONTEXT_DEPENDENT_SHAPE_REPRESENTATION(#335,#71952);
#530=CONTEXT_DEPENDENT_SHAPE_REPRESENTATION(#336,#71953);
#531=CONTEXT_DEPENDENT_SHAPE_REPRESENTATION(#337,#71954);
#532=CONTEXT_DEPENDENT_SHAPE_REPRESENTATION(#338,#71955);
#533=CONTEXT_DEPENDENT_SHAPE_REPRESENTATION(#339,#71956);
#534=CONTEXT_DEPENDENT_SHAPE_REPRESENTATION(#340,#71957);
#535=CONTEXT_DEPENDENT_SHAPE_REPRESENTATION(#341,#71958);
#536=CONTEXT_DEPENDENT_SHAPE_REPRESENTATION(#342,#71959);
#537=CONTEXT_DEPENDENT_SHAPE_REPRESENTATION(#343,#71960);
#538=CONTEXT_DEPENDENT_SHAPE_REPRESENTATION(#344,#71961);
#539=CONTEXT_DEPENDENT_SHAPE_REPRESENTATION(#345,#71962);
#540=CONTEXT_DEPENDENT_SHAPE_REPRESENTATION(#346,#71963);
#541=CONTEXT_DEPENDENT_SHAPE_REPRESENTATION(#347,#71964);
#542=CONTEXT_DEPENDENT_SHAPE_REPRESENTATION(#348,#71965);
#543=CONTEXT_DEPENDENT_SHAPE_REPRESENTATION(#349,#71966);
#544=CONTEXT_DEPENDENT_SHAPE_REPRESENTATION(#350,#71967);
#545=CONTEXT_DEPENDENT_SHAPE_REPRESENTATION(#351,#71968);
#546=CONTEXT_DEPENDENT_SHAPE_REPRESENTATION(#352,#71969);
#547=CONTEXT_DEPENDENT_SHAPE_REPRESENTATION(#353,#71970);
#548=CONTEXT_DEPENDENT_SHAPE_REPRESENTATION(#354,#71971);
#549=CONTEXT_DEPENDENT_SHAPE_REPRESENTATION(#355,#71972);
#550=CONTEXT_DEPENDENT_SHAPE_REPRESENTATION(#356,#71973);
#551=CONTEXT_DEPENDENT_SHAPE_REPRESENTATION(#357,#71974);
#552=CONTEXT_DEPENDENT_SHAPE_REPRESENTATION(#358,#71975);
#553=CONTEXT_DEPENDENT_SHAPE_REPRESENTATION(#359,#71976);
#554=CONTEXT_DEPENDENT_SHAPE_REPRESENTATION(#360,#71977);
#555=CONTEXT_DEPENDENT_SHAPE_REPRESENTATION(#361,#71978);
#556=CONTEXT_DEPENDENT_SHAPE_REPRESENTATION(#362,#71979);
#557=CONTEXT_DEPENDENT_SHAPE_REPRESENTATION(#363,#71980);
#558=CONTEXT_DEPENDENT_SHAPE_REPRESENTATION(#364,#71981);
#559=CONTEXT_DEPENDENT_SHAPE_REPRESENTATION(#365,#71982);
#560=CONTEXT_DEPENDENT_SHAPE_REPRESENTATION(#366,#71983);
#561=CONTEXT_DEPENDENT_SHAPE_REPRESENTATION(#367,#71984);
#562=CONTEXT_DEPENDENT_SHAPE_REPRESENTATION(#368,#71985);
#563=CONTEXT_DEPENDENT_SHAPE_REPRESENTATION(#369,#71986);
#564=CONTEXT_DEPENDENT_SHAPE_REPRESENTATION(#370,#71987);
#565=CONTEXT_DEPENDENT_SHAPE_REPRESENTATION(#371,#71988);
#566=CONTEXT_DEPENDENT_SHAPE_REPRESENTATION(#372,#71989);
#567=CONTEXT_DEPENDENT_SHAPE_REPRESENTATION(#373,#71990);
#568=CONTEXT_DEPENDENT_SHAPE_REPRESENTATION(#374,#71991);
#569=CONTEXT_DEPENDENT_SHAPE_REPRESENTATION(#375,#71992);
#570=CONTEXT_DEPENDENT_SHAPE_REPRESENTATION(#376,#71993);
#571=CONTEXT_DEPENDENT_SHAPE_REPRESENTATION(#377,#71994);
#572=CONTEXT_DEPENDENT_SHAPE_REPRESENTATION(#378,#71995);
#573=CONTEXT_DEPENDENT_SHAPE_REPRESENTATION(#379,#71996);
#574=CONTEXT_DEPENDENT_SHAPE_REPRESENTATION(#380,#71997);
#575=CONTEXT_DEPENDENT_SHAPE_REPRESENTATION(#381,#71998);
#576=CONTEXT_DEPENDENT_SHAPE_REPRESENTATION(#382,#71999);
#577=CONTEXT_DEPENDENT_SHAPE_REPRESENTATION(#383,#72000);
#578=CONTEXT_DEPENDENT_SHAPE_REPRESENTATION(#384,#72001);
#579=CONTEXT_DEPENDENT_SHAPE_REPRESENTATION(#385,#72002);
#580=CONTEXT_DEPENDENT_SHAPE_REPRESENTATION(#386,#72003);
#581=CONTEXT_DEPENDENT_SHAPE_REPRESENTATION(#387,#72004);
#582=CONTEXT_DEPENDENT_SHAPE_REPRESENTATION(#388,#72005);
#583=CONTEXT_DEPENDENT_SHAPE_REPRESENTATION(#389,#72006);
#584=CONTEXT_DEPENDENT_SHAPE_REPRESENTATION(#390,#72007);
#585=CONTEXT_DEPENDENT_SHAPE_REPRESENTATION(#391,#72008);
#586=CONTEXT_DEPENDENT_SHAPE_REPRESENTATION(#392,#72009);
#587=CONTEXT_DEPENDENT_SHAPE_REPRESENTATION(#393,#72010);
#588=CONTEXT_DEPENDENT_SHAPE_REPRESENTATION(#394,#72011);
#589=CONTEXT_DEPENDENT_SHAPE_REPRESENTATION(#395,#72012);
#590=CONTEXT_DEPENDENT_SHAPE_REPRESENTATION(#396,#72013);
#591=CONTEXT_DEPENDENT_SHAPE_REPRESENTATION(#397,#72014);
#592=CONTEXT_DEPENDENT_SHAPE_REPRESENTATION(#398,#72015);
#593=NEXT_ASSEMBLY_USAGE_OCCURRENCE('Dual Shaft Rail Support x 180:1',
'Dual Shaft Rail Support x 180:1','Dual Shaft Rail Support x 180:1',#72028,
#72029,'Dual Shaft Rail Support x 180:1');
#594=NEXT_ASSEMBLY_USAGE_OCCURRENCE(
'Hardened Ground Chrome Shaft 0.500 in x 180:1',
'Hardened Ground Chrome Shaft 0.500 in x 180:1',
'Hardened Ground Chrome Shaft 0.500 in x 180:1',#72028,#72031,
'Hardened Ground Chrome Shaft 0.500 in x 180:1');
#595=NEXT_ASSEMBLY_USAGE_OCCURRENCE(
'Open Pillow Block Bushing Housing:1',
'Open Pillow Block Bushing Housing:1',
'Open Pillow Block Bushing Housing:1',#72028,#72032,
'Open Pillow Block Bushing Housing:1');
#596=NEXT_ASSEMBLY_USAGE_OCCURRENCE(
'Super Smart Ball Bushing Open Sleeve:1',
'Super Smart Ball Bushing Open Sleeve:1',
'Super Smart Ball Bushing Open Sleeve:1',#72028,#72033,
'Super Smart Ball Bushing Open Sleeve:1');
#597=NEXT_ASSEMBLY_USAGE_OCCURRENCE('Super Smart Ball Retainer:1',
'Super Smart Ball Retainer:1','Super Smart Ball Retainer:1',#72028,#72034,
'Super Smart Ball Retainer:1');
#598=NEXT_ASSEMBLY_USAGE_OCCURRENCE('Steel Ball 3-32 in:1',
'Steel Ball 3-32 in:1','Steel Ball 3-32 in:1',#72028,#72035,
'Steel Ball 3-32 in:1');
#599=NEXT_ASSEMBLY_USAGE_OCCURRENCE(
'Modular Carriage Plate 4.5 x 4.5:1',
'Modular Carriage Plate 4.5 x 4.5:1',
'Modular Carriage Plate 4.5 x 4.5:1',#72028,#72030,
'Modular Carriage Plate 4.5 x 4.5:1');
#600=NEXT_ASSEMBLY_USAGE_OCCURRENCE(
'ASME B18.3 SHCS 10-32 UNF x 0.625:1',
'ASME B18.3 SHCS 10-32 UNF x 0.625:1',
'ASME B18.3 SHCS 10-32 UNF x 0.625:1',#72028,#72036,
'ASME B18.3 SHCS 10-32 UNF x 0.625:1');
#601=NEXT_ASSEMBLY_USAGE_OCCURRENCE(
'ASME B18.3 SHCS 1-4-20 UNC x 0.75:1',
'ASME B18.3 SHCS 1-4-20 UNC x 0.75:1',
'ASME B18.3 SHCS 1-4-20 UNC x 0.75:1',#72028,#72038,
'ASME B18.3 SHCS 1-4-20 UNC x 0.75:1');
#602=NEXT_ASSEMBLY_USAGE_OCCURRENCE(
'ASME B18.3 SHCS 10-32 UNF x 0.875:1',
'ASME B18.3 SHCS 10-32 UNF x 0.875:1',
'ASME B18.3 SHCS 10-32 UNF x 0.875:1',#72028,#72037,
'ASME B18.3 SHCS 10-32 UNF x 0.875:1');
#603=NEXT_ASSEMBLY_USAGE_OCCURRENCE(
'Hardened Ground Chrome Shaft 0.500 in x 180:2',
'Hardened Ground Chrome Shaft 0.500 in x 180:2',
'Hardened Ground Chrome Shaft 0.500 in x 180:2',#72028,#72031,
'Hardened Ground Chrome Shaft 0.500 in x 180:2');
#604=NEXT_ASSEMBLY_USAGE_OCCURRENCE(
'Open Pillow Block Bushing Housing:2',
'Open Pillow Block Bushing Housing:2',
'Open Pillow Block Bushing Housing:2',#72028,#72032,
'Open Pillow Block Bushing Housing:2');
#605=NEXT_ASSEMBLY_USAGE_OCCURRENCE(
'Open Pillow Block Bushing Housing:3',
'Open Pillow Block Bushing Housing:3',
'Open Pillow Block Bushing Housing:3',#72028,#72032,
'Open Pillow Block Bushing Housing:3');
#606=NEXT_ASSEMBLY_USAGE_OCCURRENCE(
'Open Pillow Block Bushing Housing:4',
'Open Pillow Block Bushing Housing:4',
'Open Pillow Block Bushing Housing:4',#72028,#72032,
'Open Pillow Block Bushing Housing:4');
#607=NEXT_ASSEMBLY_USAGE_OCCURRENCE(
'Super Smart Ball Bushing Open Sleeve:2',
'Super Smart Ball Bushing Open Sleeve:2',
'Super Smart Ball Bushing Open Sleeve:2',#72028,#72033,
'Super Smart Ball Bushing Open Sleeve:2');
#608=NEXT_ASSEMBLY_USAGE_OCCURRENCE(
'Super Smart Ball Bushing Open Sleeve:3',
'Super Smart Ball Bushing Open Sleeve:3',
'Super Smart Ball Bushing Open Sleeve:3',#72028,#72033,
'Super Smart Ball Bushing Open Sleeve:3');
#609=NEXT_ASSEMBLY_USAGE_OCCURRENCE(
'Super Smart Ball Bushing Open Sleeve:4',
'Super Smart Ball Bushing Open Sleeve:4',
'Super Smart Ball Bushing Open Sleeve:4',#72028,#72033,
'Super Smart Ball Bushing Open Sleeve:4');
#610=NEXT_ASSEMBLY_USAGE_OCCURRENCE('Super Smart Ball Retainer:2',
'Super Smart Ball Retainer:2','Super Smart Ball Retainer:2',#72028,#72034,
'Super Smart Ball Retainer:2');
#611=NEXT_ASSEMBLY_USAGE_OCCURRENCE('Super Smart Ball Retainer:3',
'Super Smart Ball Retainer:3','Super Smart Ball Retainer:3',#72028,#72034,
'Super Smart Ball Retainer:3');
#612=NEXT_ASSEMBLY_USAGE_OCCURRENCE('Super Smart Ball Retainer:4',
'Super Smart Ball Retainer:4','Super Smart Ball Retainer:4',#72028,#72034,
'Super Smart Ball Retainer:4');
#613=NEXT_ASSEMBLY_USAGE_OCCURRENCE('Steel Ball 3-32 in:2',
'Steel Ball 3-32 in:2','Steel Ball 3-32 in:2',#72028,#72035,
'Steel Ball 3-32 in:2');
#614=NEXT_ASSEMBLY_USAGE_OCCURRENCE('Steel Ball 3-32 in:3',
'Steel Ball 3-32 in:3','Steel Ball 3-32 in:3',#72028,#72035,
'Steel Ball 3-32 in:3');
#615=NEXT_ASSEMBLY_USAGE_OCCURRENCE('Steel Ball 3-32 in:4',
'Steel Ball 3-32 in:4','Steel Ball 3-32 in:4',#72028,#72035,
'Steel Ball 3-32 in:4');
#616=NEXT_ASSEMBLY_USAGE_OCCURRENCE('Steel Ball 3-32 in:5',
'Steel Ball 3-32 in:5','Steel Ball 3-32 in:5',#72028,#72035,
'Steel Ball 3-32 in:5');
#617=NEXT_ASSEMBLY_USAGE_OCCURRENCE('Steel Ball 3-32 in:6',
'Steel Ball 3-32 in:6','Steel Ball 3-32 in:6',#72028,#72035,
'Steel Ball 3-32 in:6');
#618=NEXT_ASSEMBLY_USAGE_OCCURRENCE('Steel Ball 3-32 in:7',
'Steel Ball 3-32 in:7','Steel Ball 3-32 in:7',#72028,#72035,
'Steel Ball 3-32 in:7');
#619=NEXT_ASSEMBLY_USAGE_OCCURRENCE('Steel Ball 3-32 in:8',
'Steel Ball 3-32 in:8','Steel Ball 3-32 in:8',#72028,#72035,
'Steel Ball 3-32 in:8');
#620=NEXT_ASSEMBLY_USAGE_OCCURRENCE('Steel Ball 3-32 in:9',
'Steel Ball 3-32 in:9','Steel Ball 3-32 in:9',#72028,#72035,
'Steel Ball 3-32 in:9');
#621=NEXT_ASSEMBLY_USAGE_OCCURRENCE('Steel Ball 3-32 in:10',
'Steel Ball 3-32 in:10','Steel Ball 3-32 in:10',#72028,#72035,
'Steel Ball 3-32 in:10');
#622=NEXT_ASSEMBLY_USAGE_OCCURRENCE('Steel Ball 3-32 in:11',
'Steel Ball 3-32 in:11','Steel Ball 3-32 in:11',#72028,#72035,
'Steel Ball 3-32 in:11');
#623=NEXT_ASSEMBLY_USAGE_OCCURRENCE('Steel Ball 3-32 in:12',
'Steel Ball 3-32 in:12','Steel Ball 3-32 in:12',#72028,#72035,
'Steel Ball 3-32 in:12');
#624=NEXT_ASSEMBLY_USAGE_OCCURRENCE('Steel Ball 3-32 in:13',
'Steel Ball 3-32 in:13','Steel Ball 3-32 in:13',#72028,#72035,
'Steel Ball 3-32 in:13');
#625=NEXT_ASSEMBLY_USAGE_OCCURRENCE('Steel Ball 3-32 in:14',
'Steel Ball 3-32 in:14','Steel Ball 3-32 in:14',#72028,#72035,
'Steel Ball 3-32 in:14');
#626=NEXT_ASSEMBLY_USAGE_OCCURRENCE('Steel Ball 3-32 in:15',
'Steel Ball 3-32 in:15','Steel Ball 3-32 in:15',#72028,#72035,
'Steel Ball 3-32 in:15');
#627=NEXT_ASSEMBLY_USAGE_OCCURRENCE('Steel Ball 3-32 in:16',
'Steel Ball 3-32 in:16','Steel Ball 3-32 in:16',#72028,#72035,
'Steel Ball 3-32 in:16');
#628=NEXT_ASSEMBLY_USAGE_OCCURRENCE('Steel Ball 3-32 in:17',
'Steel Ball 3-32 in:17','Steel Ball 3-32 in:17',#72028,#72035,
'Steel Ball 3-32 in:17');
#629=NEXT_ASSEMBLY_USAGE_OCCURRENCE('Steel Ball 3-32 in:18',
'Steel Ball 3-32 in:18','Steel Ball 3-32 in:18',#72028,#72035,
'Steel Ball 3-32 in:18');
#630=NEXT_ASSEMBLY_USAGE_OCCURRENCE('Steel Ball 3-32 in:19',
'Steel Ball 3-32 in:19','Steel Ball 3-32 in:19',#72028,#72035,
'Steel Ball 3-32 in:19');
#631=NEXT_ASSEMBLY_USAGE_OCCURRENCE('Steel Ball 3-32 in:20',
'Steel Ball 3-32 in:20','Steel Ball 3-32 in:20',#72028,#72035,
'Steel Ball 3-32 in:20');
#632=NEXT_ASSEMBLY_USAGE_OCCURRENCE('Steel Ball 3-32 in:21',
'Steel Ball 3-32 in:21','Steel Ball 3-32 in:21',#72028,#72035,
'Steel Ball 3-32 in:21');
#633=NEXT_ASSEMBLY_USAGE_OCCURRENCE('Steel Ball 3-32 in:22',
'Steel Ball 3-32 in:22','Steel Ball 3-32 in:22',#72028,#72035,
'Steel Ball 3-32 in:22');
#634=NEXT_ASSEMBLY_USAGE_OCCURRENCE('Steel Ball 3-32 in:23',
'Steel Ball 3-32 in:23','Steel Ball 3-32 in:23',#72028,#72035,
'Steel Ball 3-32 in:23');
#635=NEXT_ASSEMBLY_USAGE_OCCURRENCE('Steel Ball 3-32 in:24',
'Steel Ball 3-32 in:24','Steel Ball 3-32 in:24',#72028,#72035,
'Steel Ball 3-32 in:24');
#636=NEXT_ASSEMBLY_USAGE_OCCURRENCE('Steel Ball 3-32 in:25',
'Steel Ball 3-32 in:25','Steel Ball 3-32 in:25',#72028,#72035,
'Steel Ball 3-32 in:25');
#637=NEXT_ASSEMBLY_USAGE_OCCURRENCE('Steel Ball 3-32 in:26',
'Steel Ball 3-32 in:26','Steel Ball 3-32 in:26',#72028,#72035,
'Steel Ball 3-32 in:26');
#638=NEXT_ASSEMBLY_USAGE_OCCURRENCE('Steel Ball 3-32 in:27',
'Steel Ball 3-32 in:27','Steel Ball 3-32 in:27',#72028,#72035,
'Steel Ball 3-32 in:27');
#639=NEXT_ASSEMBLY_USAGE_OCCURRENCE('Steel Ball 3-32 in:28',
'Steel Ball 3-32 in:28','Steel Ball 3-32 in:28',#72028,#72035,
'Steel Ball 3-32 in:28');
#640=NEXT_ASSEMBLY_USAGE_OCCURRENCE('Steel Ball 3-32 in:29',
'Steel Ball 3-32 in:29','Steel Ball 3-32 in:29',#72028,#72035,
'Steel Ball 3-32 in:29');
#641=NEXT_ASSEMBLY_USAGE_OCCURRENCE('Steel Ball 3-32 in:30',
'Steel Ball 3-32 in:30','Steel Ball 3-32 in:30',#72028,#72035,
'Steel Ball 3-32 in:30');
#642=NEXT_ASSEMBLY_USAGE_OCCURRENCE('Steel Ball 3-32 in:31',
'Steel Ball 3-32 in:31','Steel Ball 3-32 in:31',#72028,#72035,
'Steel Ball 3-32 in:31');
#643=NEXT_ASSEMBLY_USAGE_OCCURRENCE('Steel Ball 3-32 in:32',
'Steel Ball 3-32 in:32','Steel Ball 3-32 in:32',#72028,#72035,
'Steel Ball 3-32 in:32');
#644=NEXT_ASSEMBLY_USAGE_OCCURRENCE('Steel Ball 3-32 in:33',
'Steel Ball 3-32 in:33','Steel Ball 3-32 in:33',#72028,#72035,
'Steel Ball 3-32 in:33');
#645=NEXT_ASSEMBLY_USAGE_OCCURRENCE('Steel Ball 3-32 in:34',
'Steel Ball 3-32 in:34','Steel Ball 3-32 in:34',#72028,#72035,
'Steel Ball 3-32 in:34');
#646=NEXT_ASSEMBLY_USAGE_OCCURRENCE('Steel Ball 3-32 in:35',
'Steel Ball 3-32 in:35','Steel Ball 3-32 in:35',#72028,#72035,
'Steel Ball 3-32 in:35');
#647=NEXT_ASSEMBLY_USAGE_OCCURRENCE('Steel Ball 3-32 in:36',
'Steel Ball 3-32 in:36','Steel Ball 3-32 in:36',#72028,#72035,
'Steel Ball 3-32 in:36');
#648=NEXT_ASSEMBLY_USAGE_OCCURRENCE('Steel Ball 3-32 in:37',
'Steel Ball 3-32 in:37','Steel Ball 3-32 in:37',#72028,#72035,
'Steel Ball 3-32 in:37');
#649=NEXT_ASSEMBLY_USAGE_OCCURRENCE('Steel Ball 3-32 in:38',
'Steel Ball 3-32 in:38','Steel Ball 3-32 in:38',#72028,#72035,
'Steel Ball 3-32 in:38');
#650=NEXT_ASSEMBLY_USAGE_OCCURRENCE('Steel Ball 3-32 in:39',
'Steel Ball 3-32 in:39','Steel Ball 3-32 in:39',#72028,#72035,
'Steel Ball 3-32 in:39');
#651=NEXT_ASSEMBLY_USAGE_OCCURRENCE('Steel Ball 3-32 in:40',
'Steel Ball 3-32 in:40','Steel Ball 3-32 in:40',#72028,#72035,
'Steel Ball 3-32 in:40');
#652=NEXT_ASSEMBLY_USAGE_OCCURRENCE('Steel Ball 3-32 in:41',
'Steel Ball 3-32 in:41','Steel Ball 3-32 in:41',#72028,#72035,
'Steel Ball 3-32 in:41');
#653=NEXT_ASSEMBLY_USAGE_OCCURRENCE('Steel Ball 3-32 in:42',
'Steel Ball 3-32 in:42','Steel Ball 3-32 in:42',#72028,#72035,
'Steel Ball 3-32 in:42');
#654=NEXT_ASSEMBLY_USAGE_OCCURRENCE('Steel Ball 3-32 in:43',
'Steel Ball 3-32 in:43','Steel Ball 3-32 in:43',#72028,#72035,
'Steel Ball 3-32 in:43');
#655=NEXT_ASSEMBLY_USAGE_OCCURRENCE('Steel Ball 3-32 in:44',
'Steel Ball 3-32 in:44','Steel Ball 3-32 in:44',#72028,#72035,
'Steel Ball 3-32 in:44');
#656=NEXT_ASSEMBLY_USAGE_OCCURRENCE('Steel Ball 3-32 in:45',
'Steel Ball 3-32 in:45','Steel Ball 3-32 in:45',#72028,#72035,
'Steel Ball 3-32 in:45');
#657=NEXT_ASSEMBLY_USAGE_OCCURRENCE('Steel Ball 3-32 in:46',
'Steel Ball 3-32 in:46','Steel Ball 3-32 in:46',#72028,#72035,
'Steel Ball 3-32 in:46');
#658=NEXT_ASSEMBLY_USAGE_OCCURRENCE('Steel Ball 3-32 in:47',
'Steel Ball 3-32 in:47','Steel Ball 3-32 in:47',#72028,#72035,
'Steel Ball 3-32 in:47');
#659=NEXT_ASSEMBLY_USAGE_OCCURRENCE('Steel Ball 3-32 in:48',
'Steel Ball 3-32 in:48','Steel Ball 3-32 in:48',#72028,#72035,
'Steel Ball 3-32 in:48');
#660=NEXT_ASSEMBLY_USAGE_OCCURRENCE('Steel Ball 3-32 in:49',
'Steel Ball 3-32 in:49','Steel Ball 3-32 in:49',#72028,#72035,
'Steel Ball 3-32 in:49');
#661=NEXT_ASSEMBLY_USAGE_OCCURRENCE('Steel Ball 3-32 in:50',
'Steel Ball 3-32 in:50','Steel Ball 3-32 in:50',#72028,#72035,
'Steel Ball 3-32 in:50');
#662=NEXT_ASSEMBLY_USAGE_OCCURRENCE('Steel Ball 3-32 in:51',
'Steel Ball 3-32 in:51','Steel Ball 3-32 in:51',#72028,#72035,
'Steel Ball 3-32 in:51');
#663=NEXT_ASSEMBLY_USAGE_OCCURRENCE('Steel Ball 3-32 in:52',
'Steel Ball 3-32 in:52','Steel Ball 3-32 in:52',#72028,#72035,
'Steel Ball 3-32 in:52');
#664=NEXT_ASSEMBLY_USAGE_OCCURRENCE('Steel Ball 3-32 in:53',
'Steel Ball 3-32 in:53','Steel Ball 3-32 in:53',#72028,#72035,
'Steel Ball 3-32 in:53');
#665=NEXT_ASSEMBLY_USAGE_OCCURRENCE('Steel Ball 3-32 in:54',
'Steel Ball 3-32 in:54','Steel Ball 3-32 in:54',#72028,#72035,
'Steel Ball 3-32 in:54');
#666=NEXT_ASSEMBLY_USAGE_OCCURRENCE('Steel Ball 3-32 in:55',
'Steel Ball 3-32 in:55','Steel Ball 3-32 in:55',#72028,#72035,
'Steel Ball 3-32 in:55');
#667=NEXT_ASSEMBLY_USAGE_OCCURRENCE('Steel Ball 3-32 in:56',
'Steel Ball 3-32 in:56','Steel Ball 3-32 in:56',#72028,#72035,
'Steel Ball 3-32 in:56');
#668=NEXT_ASSEMBLY_USAGE_OCCURRENCE('Steel Ball 3-32 in:57',
'Steel Ball 3-32 in:57','Steel Ball 3-32 in:57',#72028,#72035,
'Steel Ball 3-32 in:57');
#669=NEXT_ASSEMBLY_USAGE_OCCURRENCE('Steel Ball 3-32 in:58',
'Steel Ball 3-32 in:58','Steel Ball 3-32 in:58',#72028,#72035,
'Steel Ball 3-32 in:58');
#670=NEXT_ASSEMBLY_USAGE_OCCURRENCE('Steel Ball 3-32 in:59',
'Steel Ball 3-32 in:59','Steel Ball 3-32 in:59',#72028,#72035,
'Steel Ball 3-32 in:59');
#671=NEXT_ASSEMBLY_USAGE_OCCURRENCE('Steel Ball 3-32 in:60',
'Steel Ball 3-32 in:60','Steel Ball 3-32 in:60',#72028,#72035,
'Steel Ball 3-32 in:60');
#672=NEXT_ASSEMBLY_USAGE_OCCURRENCE('Steel Ball 3-32 in:61',
'Steel Ball 3-32 in:61','Steel Ball 3-32 in:61',#72028,#72035,
'Steel Ball 3-32 in:61');
#673=NEXT_ASSEMBLY_USAGE_OCCURRENCE('Steel Ball 3-32 in:62',
'Steel Ball 3-32 in:62','Steel Ball 3-32 in:62',#72028,#72035,
'Steel Ball 3-32 in:62');
#674=NEXT_ASSEMBLY_USAGE_OCCURRENCE('Steel Ball 3-32 in:63',
'Steel Ball 3-32 in:63','Steel Ball 3-32 in:63',#72028,#72035,
'Steel Ball 3-32 in:63');
#675=NEXT_ASSEMBLY_USAGE_OCCURRENCE('Steel Ball 3-32 in:64',
'Steel Ball 3-32 in:64','Steel Ball 3-32 in:64',#72028,#72035,
'Steel Ball 3-32 in:64');
#676=NEXT_ASSEMBLY_USAGE_OCCURRENCE('Steel Ball 3-32 in:65',
'Steel Ball 3-32 in:65','Steel Ball 3-32 in:65',#72028,#72035,
'Steel Ball 3-32 in:65');
#677=NEXT_ASSEMBLY_USAGE_OCCURRENCE('Steel Ball 3-32 in:66',
'Steel Ball 3-32 in:66','Steel Ball 3-32 in:66',#72028,#72035,
'Steel Ball 3-32 in:66');
#678=NEXT_ASSEMBLY_USAGE_OCCURRENCE('Steel Ball 3-32 in:67',
'Steel Ball 3-32 in:67','Steel Ball 3-32 in:67',#72028,#72035,
'Steel Ball 3-32 in:67');
#679=NEXT_ASSEMBLY_USAGE_OCCURRENCE('Steel Ball 3-32 in:68',
'Steel Ball 3-32 in:68','Steel Ball 3-32 in:68',#72028,#72035,
'Steel Ball 3-32 in:68');
#680=NEXT_ASSEMBLY_USAGE_OCCURRENCE('Steel Ball 3-32 in:69',
'Steel Ball 3-32 in:69','Steel Ball 3-32 in:69',#72028,#72035,
'Steel Ball 3-32 in:69');
#681=NEXT_ASSEMBLY_USAGE_OCCURRENCE('Steel Ball 3-32 in:70',
'Steel Ball 3-32 in:70','Steel Ball 3-32 in:70',#72028,#72035,
'Steel Ball 3-32 in:70');
#682=NEXT_ASSEMBLY_USAGE_OCCURRENCE('Steel Ball 3-32 in:71',
'Steel Ball 3-32 in:71','Steel Ball 3-32 in:71',#72028,#72035,
'Steel Ball 3-32 in:71');
#683=NEXT_ASSEMBLY_USAGE_OCCURRENCE('Steel Ball 3-32 in:72',
'Steel Ball 3-32 in:72','Steel Ball 3-32 in:72',#72028,#72035,
'Steel Ball 3-32 in:72');
#684=NEXT_ASSEMBLY_USAGE_OCCURRENCE('Steel Ball 3-32 in:73',
'Steel Ball 3-32 in:73','Steel Ball 3-32 in:73',#72028,#72035,
'Steel Ball 3-32 in:73');
#685=NEXT_ASSEMBLY_USAGE_OCCURRENCE('Steel Ball 3-32 in:74',
'Steel Ball 3-32 in:74','Steel Ball 3-32 in:74',#72028,#72035,
'Steel Ball 3-32 in:74');
#686=NEXT_ASSEMBLY_USAGE_OCCURRENCE('Steel Ball 3-32 in:75',
'Steel Ball 3-32 in:75','Steel Ball 3-32 in:75',#72028,#72035,
'Steel Ball 3-32 in:75');
#687=NEXT_ASSEMBLY_USAGE_OCCURRENCE('Steel Ball 3-32 in:76',
'Steel Ball 3-32 in:76','Steel Ball 3-32 in:76',#72028,#72035,
'Steel Ball 3-32 in:76');
#688=NEXT_ASSEMBLY_USAGE_OCCURRENCE('Steel Ball 3-32 in:77',
'Steel Ball 3-32 in:77','Steel Ball 3-32 in:77',#72028,#72035,
'Steel Ball 3-32 in:77');
#689=NEXT_ASSEMBLY_USAGE_OCCURRENCE('Steel Ball 3-32 in:78',
'Steel Ball 3-32 in:78','Steel Ball 3-32 in:78',#72028,#72035,
'Steel Ball 3-32 in:78');
#690=NEXT_ASSEMBLY_USAGE_OCCURRENCE('Steel Ball 3-32 in:79',
'Steel Ball 3-32 in:79','Steel Ball 3-32 in:79',#72028,#72035,
'Steel Ball 3-32 in:79');
#691=NEXT_ASSEMBLY_USAGE_OCCURRENCE('Steel Ball 3-32 in:80',
'Steel Ball 3-32 in:80','Steel Ball 3-32 in:80',#72028,#72035,
'Steel Ball 3-32 in:80');
#692=NEXT_ASSEMBLY_USAGE_OCCURRENCE('Steel Ball 3-32 in:81',
'Steel Ball 3-32 in:81','Steel Ball 3-32 in:81',#72028,#72035,
'Steel Ball 3-32 in:81');
#693=NEXT_ASSEMBLY_USAGE_OCCURRENCE('Steel Ball 3-32 in:82',
'Steel Ball 3-32 in:82','Steel Ball 3-32 in:82',#72028,#72035,
'Steel Ball 3-32 in:82');
#694=NEXT_ASSEMBLY_USAGE_OCCURRENCE('Steel Ball 3-32 in:83',
'Steel Ball 3-32 in:83','Steel Ball 3-32 in:83',#72028,#72035,
'Steel Ball 3-32 in:83');
#695=NEXT_ASSEMBLY_USAGE_OCCURRENCE('Steel Ball 3-32 in:84',
'Steel Ball 3-32 in:84','Steel Ball 3-32 in:84',#72028,#72035,
'Steel Ball 3-32 in:84');
#696=NEXT_ASSEMBLY_USAGE_OCCURRENCE('Steel Ball 3-32 in:85',
'Steel Ball 3-32 in:85','Steel Ball 3-32 in:85',#72028,#72035,
'Steel Ball 3-32 in:85');
#697=NEXT_ASSEMBLY_USAGE_OCCURRENCE('Steel Ball 3-32 in:86',
'Steel Ball 3-32 in:86','Steel Ball 3-32 in:86',#72028,#72035,
'Steel Ball 3-32 in:86');
#698=NEXT_ASSEMBLY_USAGE_OCCURRENCE('Steel Ball 3-32 in:87',
'Steel Ball 3-32 in:87','Steel Ball 3-32 in:87',#72028,#72035,
'Steel Ball 3-32 in:87');
#699=NEXT_ASSEMBLY_USAGE_OCCURRENCE('Steel Ball 3-32 in:88',
'Steel Ball 3-32 in:88','Steel Ball 3-32 in:88',#72028,#72035,
'Steel Ball 3-32 in:88');
#700=NEXT_ASSEMBLY_USAGE_OCCURRENCE('Steel Ball 3-32 in:89',
'Steel Ball 3-32 in:89','Steel Ball 3-32 in:89',#72028,#72035,
'Steel Ball 3-32 in:89');
#701=NEXT_ASSEMBLY_USAGE_OCCURRENCE('Steel Ball 3-32 in:90',
'Steel Ball 3-32 in:90','Steel Ball 3-32 in:90',#72028,#72035,
'Steel Ball 3-32 in:90');
#702=NEXT_ASSEMBLY_USAGE_OCCURRENCE('Steel Ball 3-32 in:91',
'Steel Ball 3-32 in:91','Steel Ball 3-32 in:91',#72028,#72035,
'Steel Ball 3-32 in:91');
#703=NEXT_ASSEMBLY_USAGE_OCCURRENCE('Steel Ball 3-32 in:92',
'Steel Ball 3-32 in:92','Steel Ball 3-32 in:92',#72028,#72035,
'Steel Ball 3-32 in:92');
#704=NEXT_ASSEMBLY_USAGE_OCCURRENCE('Steel Ball 3-32 in:93',
'Steel Ball 3-32 in:93','Steel Ball 3-32 in:93',#72028,#72035,
'Steel Ball 3-32 in:93');
#705=NEXT_ASSEMBLY_USAGE_OCCURRENCE('Steel Ball 3-32 in:94',
'Steel Ball 3-32 in:94','Steel Ball 3-32 in:94',#72028,#72035,
'Steel Ball 3-32 in:94');
#706=NEXT_ASSEMBLY_USAGE_OCCURRENCE('Steel Ball 3-32 in:95',
'Steel Ball 3-32 in:95','Steel Ball 3-32 in:95',#72028,#72035,
'Steel Ball 3-32 in:95');
#707=NEXT_ASSEMBLY_USAGE_OCCURRENCE('Steel Ball 3-32 in:96',
'Steel Ball 3-32 in:96','Steel Ball 3-32 in:96',#72028,#72035,
'Steel Ball 3-32 in:96');
#708=NEXT_ASSEMBLY_USAGE_OCCURRENCE('Steel Ball 3-32 in:97',
'Steel Ball 3-32 in:97','Steel Ball 3-32 in:97',#72028,#72035,
'Steel Ball 3-32 in:97');
#709=NEXT_ASSEMBLY_USAGE_OCCURRENCE('Steel Ball 3-32 in:98',
'Steel Ball 3-32 in:98','Steel Ball 3-32 in:98',#72028,#72035,
'Steel Ball 3-32 in:98');
#710=NEXT_ASSEMBLY_USAGE_OCCURRENCE('Steel Ball 3-32 in:99',
'Steel Ball 3-32 in:99','Steel Ball 3-32 in:99',#72028,#72035,
'Steel Ball 3-32 in:99');
#711=NEXT_ASSEMBLY_USAGE_OCCURRENCE('Steel Ball 3-32 in:100',
'Steel Ball 3-32 in:100','Steel Ball 3-32 in:100',#72028,#72035,
'Steel Ball 3-32 in:100');
#712=NEXT_ASSEMBLY_USAGE_OCCURRENCE('Steel Ball 3-32 in:101',
'Steel Ball 3-32 in:101','Steel Ball 3-32 in:101',#72028,#72035,
'Steel Ball 3-32 in:101');
#713=NEXT_ASSEMBLY_USAGE_OCCURRENCE('Steel Ball 3-32 in:102',
'Steel Ball 3-32 in:102','Steel Ball 3-32 in:102',#72028,#72035,
'Steel Ball 3-32 in:102');
#714=NEXT_ASSEMBLY_USAGE_OCCURRENCE('Steel Ball 3-32 in:103',
'Steel Ball 3-32 in:103','Steel Ball 3-32 in:103',#72028,#72035,
'Steel Ball 3-32 in:103');
#715=NEXT_ASSEMBLY_USAGE_OCCURRENCE('Steel Ball 3-32 in:104',
'Steel Ball 3-32 in:104','Steel Ball 3-32 in:104',#72028,#72035,
'Steel Ball 3-32 in:104');
#716=NEXT_ASSEMBLY_USAGE_OCCURRENCE('Steel Ball 3-32 in:105',
'Steel Ball 3-32 in:105','Steel Ball 3-32 in:105',#72028,#72035,
'Steel Ball 3-32 in:105');
#717=NEXT_ASSEMBLY_USAGE_OCCURRENCE('Steel Ball 3-32 in:106',
'Steel Ball 3-32 in:106','Steel Ball 3-32 in:106',#72028,#72035,
'Steel Ball 3-32 in:106');
#718=NEXT_ASSEMBLY_USAGE_OCCURRENCE('Steel Ball 3-32 in:107',
'Steel Ball 3-32 in:107','Steel Ball 3-32 in:107',#72028,#72035,
'Steel Ball 3-32 in:107');
#719=NEXT_ASSEMBLY_USAGE_OCCURRENCE('Steel Ball 3-32 in:108',
'Steel Ball 3-32 in:108','Steel Ball 3-32 in:108',#72028,#72035,
'Steel Ball 3-32 in:108');
#720=NEXT_ASSEMBLY_USAGE_OCCURRENCE('Steel Ball 3-32 in:109',
'Steel Ball 3-32 in:109','Steel Ball 3-32 in:109',#72028,#72035,
'Steel Ball 3-32 in:109');
#721=NEXT_ASSEMBLY_USAGE_OCCURRENCE('Steel Ball 3-32 in:110',
'Steel Ball 3-32 in:110','Steel Ball 3-32 in:110',#72028,#72035,
'Steel Ball 3-32 in:110');
#722=NEXT_ASSEMBLY_USAGE_OCCURRENCE('Steel Ball 3-32 in:111',
'Steel Ball 3-32 in:111','Steel Ball 3-32 in:111',#72028,#72035,
'Steel Ball 3-32 in:111');
#723=NEXT_ASSEMBLY_USAGE_OCCURRENCE('Steel Ball 3-32 in:112',
'Steel Ball 3-32 in:112','Steel Ball 3-32 in:112',#72028,#72035,
'Steel Ball 3-32 in:112');
#724=NEXT_ASSEMBLY_USAGE_OCCURRENCE('Steel Ball 3-32 in:113',
'Steel Ball 3-32 in:113','Steel Ball 3-32 in:113',#72028,#72035,
'Steel Ball 3-32 in:113');
#725=NEXT_ASSEMBLY_USAGE_OCCURRENCE('Steel Ball 3-32 in:114',
'Steel Ball 3-32 in:114','Steel Ball 3-32 in:114',#72028,#72035,
'Steel Ball 3-32 in:114');
#726=NEXT_ASSEMBLY_USAGE_OCCURRENCE('Steel Ball 3-32 in:115',
'Steel Ball 3-32 in:115','Steel Ball 3-32 in:115',#72028,#72035,
'Steel Ball 3-32 in:115');
#727=NEXT_ASSEMBLY_USAGE_OCCURRENCE('Steel Ball 3-32 in:116',
'Steel Ball 3-32 in:116','Steel Ball 3-32 in:116',#72028,#72035,
'Steel Ball 3-32 in:116');
#728=NEXT_ASSEMBLY_USAGE_OCCURRENCE('Steel Ball 3-32 in:117',
'Steel Ball 3-32 in:117','Steel Ball 3-32 in:117',#72028,#72035,
'Steel Ball 3-32 in:117');
#729=NEXT_ASSEMBLY_USAGE_OCCURRENCE('Steel Ball 3-32 in:118',
'Steel Ball 3-32 in:118','Steel Ball 3-32 in:118',#72028,#72035,
'Steel Ball 3-32 in:118');
#730=NEXT_ASSEMBLY_USAGE_OCCURRENCE('Steel Ball 3-32 in:119',
'Steel Ball 3-32 in:119','Steel Ball 3-32 in:119',#72028,#72035,
'Steel Ball 3-32 in:119');
#731=NEXT_ASSEMBLY_USAGE_OCCURRENCE('Steel Ball 3-32 in:120',
'Steel Ball 3-32 in:120','Steel Ball 3-32 in:120',#72028,#72035,
'Steel Ball 3-32 in:120');
#732=NEXT_ASSEMBLY_USAGE_OCCURRENCE('Steel Ball 3-32 in:121',
'Steel Ball 3-32 in:121','Steel Ball 3-32 in:121',#72028,#72035,
'Steel Ball 3-32 in:121');
#733=NEXT_ASSEMBLY_USAGE_OCCURRENCE('Steel Ball 3-32 in:122',
'Steel Ball 3-32 in:122','Steel Ball 3-32 in:122',#72028,#72035,
'Steel Ball 3-32 in:122');
#734=NEXT_ASSEMBLY_USAGE_OCCURRENCE('Steel Ball 3-32 in:123',
'Steel Ball 3-32 in:123','Steel Ball 3-32 in:123',#72028,#72035,
'Steel Ball 3-32 in:123');
#735=NEXT_ASSEMBLY_USAGE_OCCURRENCE('Steel Ball 3-32 in:124',
'Steel Ball 3-32 in:124','Steel Ball 3-32 in:124',#72028,#72035,
'Steel Ball 3-32 in:124');
#736=NEXT_ASSEMBLY_USAGE_OCCURRENCE('Steel Ball 3-32 in:125',
'Steel Ball 3-32 in:125','Steel Ball 3-32 in:125',#72028,#72035,
'Steel Ball 3-32 in:125');
#737=NEXT_ASSEMBLY_USAGE_OCCURRENCE('Steel Ball 3-32 in:126',
'Steel Ball 3-32 in:126','Steel Ball 3-32 in:126',#72028,#72035,
'Steel Ball 3-32 in:126');
#738=NEXT_ASSEMBLY_USAGE_OCCURRENCE('Steel Ball 3-32 in:127',
'Steel Ball 3-32 in:127','Steel Ball 3-32 in:127',#72028,#72035,
'Steel Ball 3-32 in:127');
#739=NEXT_ASSEMBLY_USAGE_OCCURRENCE('Steel Ball 3-32 in:128',
'Steel Ball 3-32 in:128','Steel Ball 3-32 in:128',#72028,#72035,
'Steel Ball 3-32 in:128');
#740=NEXT_ASSEMBLY_USAGE_OCCURRENCE('Steel Ball 3-32 in:129',
'Steel Ball 3-32 in:129','Steel Ball 3-32 in:129',#72028,#72035,
'Steel Ball 3-32 in:129');
#741=NEXT_ASSEMBLY_USAGE_OCCURRENCE('Steel Ball 3-32 in:130',
'Steel Ball 3-32 in:130','Steel Ball 3-32 in:130',#72028,#72035,
'Steel Ball 3-32 in:130');
#742=NEXT_ASSEMBLY_USAGE_OCCURRENCE('Steel Ball 3-32 in:131',
'Steel Ball 3-32 in:131','Steel Ball 3-32 in:131',#72028,#72035,
'Steel Ball 3-32 in:131');
#743=NEXT_ASSEMBLY_USAGE_OCCURRENCE('Steel Ball 3-32 in:132',
'Steel Ball 3-32 in:132','Steel Ball 3-32 in:132',#72028,#72035,
'Steel Ball 3-32 in:132');
#744=NEXT_ASSEMBLY_USAGE_OCCURRENCE('Steel Ball 3-32 in:133',
'Steel Ball 3-32 in:133','Steel Ball 3-32 in:133',#72028,#72035,
'Steel Ball 3-32 in:133');
#745=NEXT_ASSEMBLY_USAGE_OCCURRENCE('Steel Ball 3-32 in:134',
'Steel Ball 3-32 in:134','Steel Ball 3-32 in:134',#72028,#72035,
'Steel Ball 3-32 in:134');
#746=NEXT_ASSEMBLY_USAGE_OCCURRENCE('Steel Ball 3-32 in:135',
'Steel Ball 3-32 in:135','Steel Ball 3-32 in:135',#72028,#72035,
'Steel Ball 3-32 in:135');
#747=NEXT_ASSEMBLY_USAGE_OCCURRENCE('Steel Ball 3-32 in:136',
'Steel Ball 3-32 in:136','Steel Ball 3-32 in:136',#72028,#72035,
'Steel Ball 3-32 in:136');
#748=NEXT_ASSEMBLY_USAGE_OCCURRENCE('Steel Ball 3-32 in:137',
'Steel Ball 3-32 in:137','Steel Ball 3-32 in:137',#72028,#72035,
'Steel Ball 3-32 in:137');
#749=NEXT_ASSEMBLY_USAGE_OCCURRENCE('Steel Ball 3-32 in:138',
'Steel Ball 3-32 in:138','Steel Ball 3-32 in:138',#72028,#72035,
'Steel Ball 3-32 in:138');
#750=NEXT_ASSEMBLY_USAGE_OCCURRENCE('Steel Ball 3-32 in:139',
'Steel Ball 3-32 in:139','Steel Ball 3-32 in:139',#72028,#72035,
'Steel Ball 3-32 in:139');
#751=NEXT_ASSEMBLY_USAGE_OCCURRENCE('Steel Ball 3-32 in:140',
'Steel Ball 3-32 in:140','Steel Ball 3-32 in:140',#72028,#72035,
'Steel Ball 3-32 in:140');
#752=NEXT_ASSEMBLY_USAGE_OCCURRENCE('Steel Ball 3-32 in:141',
'Steel Ball 3-32 in:141','Steel Ball 3-32 in:141',#72028,#72035,
'Steel Ball 3-32 in:141');
#753=NEXT_ASSEMBLY_USAGE_OCCURRENCE('Steel Ball 3-32 in:142',
'Steel Ball 3-32 in:142','Steel Ball 3-32 in:142',#72028,#72035,
'Steel Ball 3-32 in:142');
#754=NEXT_ASSEMBLY_USAGE_OCCURRENCE('Steel Ball 3-32 in:143',
'Steel Ball 3-32 in:143','Steel Ball 3-32 in:143',#72028,#72035,
'Steel Ball 3-32 in:143');
#755=NEXT_ASSEMBLY_USAGE_OCCURRENCE('Steel Ball 3-32 in:144',
'Steel Ball 3-32 in:144','Steel Ball 3-32 in:144',#72028,#72035,
'Steel Ball 3-32 in:144');
#756=NEXT_ASSEMBLY_USAGE_OCCURRENCE('Steel Ball 3-32 in:145',
'Steel Ball 3-32 in:145','Steel Ball 3-32 in:145',#72028,#72035,
'Steel Ball 3-32 in:145');
#757=NEXT_ASSEMBLY_USAGE_OCCURRENCE('Steel Ball 3-32 in:146',
'Steel Ball 3-32 in:146','Steel Ball 3-32 in:146',#72028,#72035,
'Steel Ball 3-32 in:146');
#758=NEXT_ASSEMBLY_USAGE_OCCURRENCE('Steel Ball 3-32 in:147',
'Steel Ball 3-32 in:147','Steel Ball 3-32 in:147',#72028,#72035,
'Steel Ball 3-32 in:147');
#759=NEXT_ASSEMBLY_USAGE_OCCURRENCE('Steel Ball 3-32 in:148',
'Steel Ball 3-32 in:148','Steel Ball 3-32 in:148',#72028,#72035,
'Steel Ball 3-32 in:148');
#760=NEXT_ASSEMBLY_USAGE_OCCURRENCE('Steel Ball 3-32 in:149',
'Steel Ball 3-32 in:149','Steel Ball 3-32 in:149',#72028,#72035,
'Steel Ball 3-32 in:149');
#761=NEXT_ASSEMBLY_USAGE_OCCURRENCE('Steel Ball 3-32 in:150',
'Steel Ball 3-32 in:150','Steel Ball 3-32 in:150',#72028,#72035,
'Steel Ball 3-32 in:150');
#762=NEXT_ASSEMBLY_USAGE_OCCURRENCE('Steel Ball 3-32 in:151',
'Steel Ball 3-32 in:151','Steel Ball 3-32 in:151',#72028,#72035,
'Steel Ball 3-32 in:151');
#763=NEXT_ASSEMBLY_USAGE_OCCURRENCE('Steel Ball 3-32 in:152',
'Steel Ball 3-32 in:152','Steel Ball 3-32 in:152',#72028,#72035,
'Steel Ball 3-32 in:152');
#764=NEXT_ASSEMBLY_USAGE_OCCURRENCE('Steel Ball 3-32 in:153',
'Steel Ball 3-32 in:153','Steel Ball 3-32 in:153',#72028,#72035,
'Steel Ball 3-32 in:153');
#765=NEXT_ASSEMBLY_USAGE_OCCURRENCE('Steel Ball 3-32 in:154',
'Steel Ball 3-32 in:154','Steel Ball 3-32 in:154',#72028,#72035,
'Steel Ball 3-32 in:154');
#766=NEXT_ASSEMBLY_USAGE_OCCURRENCE('Steel Ball 3-32 in:155',
'Steel Ball 3-32 in:155','Steel Ball 3-32 in:155',#72028,#72035,
'Steel Ball 3-32 in:155');
#767=NEXT_ASSEMBLY_USAGE_OCCURRENCE('Steel Ball 3-32 in:156',
'Steel Ball 3-32 in:156','Steel Ball 3-32 in:156',#72028,#72035,
'Steel Ball 3-32 in:156');
#768=NEXT_ASSEMBLY_USAGE_OCCURRENCE('Steel Ball 3-32 in:157',
'Steel Ball 3-32 in:157','Steel Ball 3-32 in:157',#72028,#72035,
'Steel Ball 3-32 in:157');
#769=NEXT_ASSEMBLY_USAGE_OCCURRENCE('Steel Ball 3-32 in:158',
'Steel Ball 3-32 in:158','Steel Ball 3-32 in:158',#72028,#72035,
'Steel Ball 3-32 in:158');
#770=NEXT_ASSEMBLY_USAGE_OCCURRENCE('Steel Ball 3-32 in:159',
'Steel Ball 3-32 in:159','Steel Ball 3-32 in:159',#72028,#72035,
'Steel Ball 3-32 in:159');
#771=NEXT_ASSEMBLY_USAGE_OCCURRENCE('Steel Ball 3-32 in:160',
'Steel Ball 3-32 in:160','Steel Ball 3-32 in:160',#72028,#72035,
'Steel Ball 3-32 in:160');
#772=NEXT_ASSEMBLY_USAGE_OCCURRENCE(
'ASME B18.3 SHCS 10-32 UNF x 0.625:2',
'ASME B18.3 SHCS 10-32 UNF x 0.625:2',
'ASME B18.3 SHCS 10-32 UNF x 0.625:2',#72028,#72036,
'ASME B18.3 SHCS 10-32 UNF x 0.625:2');
#773=NEXT_ASSEMBLY_USAGE_OCCURRENCE(
'ASME B18.3 SHCS 10-32 UNF x 0.625:3',
'ASME B18.3 SHCS 10-32 UNF x 0.625:3',
'ASME B18.3 SHCS 10-32 UNF x 0.625:3',#72028,#72036,
'ASME B18.3 SHCS 10-32 UNF x 0.625:3');
#774=NEXT_ASSEMBLY_USAGE_OCCURRENCE(
'ASME B18.3 SHCS 10-32 UNF x 0.625:4',
'ASME B18.3 SHCS 10-32 UNF x 0.625:4',
'ASME B18.3 SHCS 10-32 UNF x 0.625:4',#72028,#72036,
'ASME B18.3 SHCS 10-32 UNF x 0.625:4');
#775=NEXT_ASSEMBLY_USAGE_OCCURRENCE(
'ASME B18.3 SHCS 10-32 UNF x 0.625:5',
'ASME B18.3 SHCS 10-32 UNF x 0.625:5',
'ASME B18.3 SHCS 10-32 UNF x 0.625:5',#72028,#72036,
'ASME B18.3 SHCS 10-32 UNF x 0.625:5');
#776=NEXT_ASSEMBLY_USAGE_OCCURRENCE(
'ASME B18.3 SHCS 10-32 UNF x 0.625:6',
'ASME B18.3 SHCS 10-32 UNF x 0.625:6',
'ASME B18.3 SHCS 10-32 UNF x 0.625:6',#72028,#72036,
'ASME B18.3 SHCS 10-32 UNF x 0.625:6');
#777=NEXT_ASSEMBLY_USAGE_OCCURRENCE(
'ASME B18.3 SHCS 10-32 UNF x 0.625:7',
'ASME B18.3 SHCS 10-32 UNF x 0.625:7',
'ASME B18.3 SHCS 10-32 UNF x 0.625:7',#72028,#72036,
'ASME B18.3 SHCS 10-32 UNF x 0.625:7');
#778=NEXT_ASSEMBLY_USAGE_OCCURRENCE(
'ASME B18.3 SHCS 10-32 UNF x 0.625:8',
'ASME B18.3 SHCS 10-32 UNF x 0.625:8',
'ASME B18.3 SHCS 10-32 UNF x 0.625:8',#72028,#72036,
'ASME B18.3 SHCS 10-32 UNF x 0.625:8');
#779=NEXT_ASSEMBLY_USAGE_OCCURRENCE(
'ASME B18.3 SHCS 10-32 UNF x 0.875:2',
'ASME B18.3 SHCS 10-32 UNF x 0.875:2',
'ASME B18.3 SHCS 10-32 UNF x 0.875:2',#72028,#72037,
'ASME B18.3 SHCS 10-32 UNF x 0.875:2');
#780=NEXT_ASSEMBLY_USAGE_OCCURRENCE(
'ASME B18.3 SHCS 10-32 UNF x 0.875:3',
'ASME B18.3 SHCS 10-32 UNF x 0.875:3',
'ASME B18.3 SHCS 10-32 UNF x 0.875:3',#72028,#72037,
'ASME B18.3 SHCS 10-32 UNF x 0.875:3');
#781=NEXT_ASSEMBLY_USAGE_OCCURRENCE(
'ASME B18.3 SHCS 10-32 UNF x 0.875:4',
'ASME B18.3 SHCS 10-32 UNF x 0.875:4',
'ASME B18.3 SHCS 10-32 UNF x 0.875:4',#72028,#72037,
'ASME B18.3 SHCS 10-32 UNF x 0.875:4');
#782=NEXT_ASSEMBLY_USAGE_OCCURRENCE(
'ASME B18.3 SHCS 10-32 UNF x 0.875:5',
'ASME B18.3 SHCS 10-32 UNF x 0.875:5',
'ASME B18.3 SHCS 10-32 UNF x 0.875:5',#72028,#72037,
'ASME B18.3 SHCS 10-32 UNF x 0.875:5');
#783=NEXT_ASSEMBLY_USAGE_OCCURRENCE(
'ASME B18.3 SHCS 10-32 UNF x 0.875:6',
'ASME B18.3 SHCS 10-32 UNF x 0.875:6',
'ASME B18.3 SHCS 10-32 UNF x 0.875:6',#72028,#72037,
'ASME B18.3 SHCS 10-32 UNF x 0.875:6');
#784=NEXT_ASSEMBLY_USAGE_OCCURRENCE(
'ASME B18.3 SHCS 1-4-20 UNC x 0.75:2',
'ASME B18.3 SHCS 1-4-20 UNC x 0.75:2',
'ASME B18.3 SHCS 1-4-20 UNC x 0.75:2',#72028,#72038,
'ASME B18.3 SHCS 1-4-20 UNC x 0.75:2');
#785=NEXT_ASSEMBLY_USAGE_OCCURRENCE(
'ASME B18.3 SHCS 1-4-20 UNC x 0.75:3',
'ASME B18.3 SHCS 1-4-20 UNC x 0.75:3',
'ASME B18.3 SHCS 1-4-20 UNC x 0.75:3',#72028,#72038,
'ASME B18.3 SHCS 1-4-20 UNC x 0.75:3');
#786=NEXT_ASSEMBLY_USAGE_OCCURRENCE(
'ASME B18.3 SHCS 1-4-20 UNC x 0.75:4',
'ASME B18.3 SHCS 1-4-20 UNC x 0.75:4',
'ASME B18.3 SHCS 1-4-20 UNC x 0.75:4',#72028,#72038,
'ASME B18.3 SHCS 1-4-20 UNC x 0.75:4');
#787=(
BOUNDED_CURVE()
B_SPLINE_CURVE(2,(#36530,#36531,#36532),.UNSPECIFIED.,.F.,.F.)
B_SPLINE_CURVE_WITH_KNOTS((3,3),(0.,0.021388782715503),.UNSPECIFIED.)
CURVE()
GEOMETRIC_REPRESENTATION_ITEM()
RATIONAL_B_SPLINE_CURVE((1.,1.00061453665269,1.00078646015663))
REPRESENTATION_ITEM('')
);
#788=(
BOUNDED_CURVE()
B_SPLINE_CURVE(2,(#36537,#36538,#36539),.UNSPECIFIED.,.F.,.F.)
B_SPLINE_CURVE_WITH_KNOTS((3,3),(0.0380048027322982,0.0593935854477557),
 .UNSPECIFIED.)
CURVE()
GEOMETRIC_REPRESENTATION_ITEM()
RATIONAL_B_SPLINE_CURVE((1.00078646015529,1.00061453665164,1.))
REPRESENTATION_ITEM('')
);
#789=(
BOUNDED_CURVE()
B_SPLINE_CURVE(2,(#36546,#36547,#36548),.UNSPECIFIED.,.F.,.F.)
B_SPLINE_CURVE_WITH_KNOTS((3,3),(0.0380048027323146,0.0593935854477557),
 .UNSPECIFIED.)
CURVE()
GEOMETRIC_REPRESENTATION_ITEM()
RATIONAL_B_SPLINE_CURVE((1.00078646015801,1.00061453665376,1.))
REPRESENTATION_ITEM('')
);
#790=(
BOUNDED_CURVE()
B_SPLINE_CURVE(2,(#36552,#36553,#36554),.UNSPECIFIED.,.F.,.F.)
B_SPLINE_CURVE_WITH_KNOTS((3,3),(0.,0.0213887827155079),.UNSPECIFIED.)
CURVE()
GEOMETRIC_REPRESENTATION_ITEM()
RATIONAL_B_SPLINE_CURVE((1.,1.00061453665303,1.00078646015707))
REPRESENTATION_ITEM('')
);
#791=(
BOUNDED_CURVE()
B_SPLINE_CURVE(2,(#36556,#36557,#36558),.UNSPECIFIED.,.F.,.F.)
B_SPLINE_CURVE_WITH_KNOTS((3,3),(0.03800480273222,0.0593935854477558),
 .UNSPECIFIED.)
CURVE()
GEOMETRIC_REPRESENTATION_ITEM()
RATIONAL_B_SPLINE_CURVE((1.00078646015217,1.0006145366492,1.))
REPRESENTATION_ITEM('')
);
#792=(
BOUNDED_CURVE()
B_SPLINE_CURVE(2,(#36562,#36563,#36564),.UNSPECIFIED.,.F.,.F.)
B_SPLINE_CURVE_WITH_KNOTS((3,3),(0.,0.0213887827155065),.UNSPECIFIED.)
CURVE()
GEOMETRIC_REPRESENTATION_ITEM()
RATIONAL_B_SPLINE_CURVE((1.,1.00061453664751,1.00078646015))
REPRESENTATION_ITEM('')
);
#793=(
BOUNDED_CURVE()
B_SPLINE_CURVE(2,(#36566,#36567,#36568),.UNSPECIFIED.,.F.,.F.)
B_SPLINE_CURVE_WITH_KNOTS((3,3),(0.0380048027322497,0.0593935854477559),
 .UNSPECIFIED.)
CURVE()
GEOMETRIC_REPRESENTATION_ITEM()
RATIONAL_B_SPLINE_CURVE((1.00078646015691,1.00061453665291,1.))
REPRESENTATION_ITEM('')
);
#794=(
BOUNDED_CURVE()
B_SPLINE_CURVE(2,(#36572,#36573,#36574),.UNSPECIFIED.,.F.,.F.)
B_SPLINE_CURVE_WITH_KNOTS((3,3),(0.,0.0213887827155146),.UNSPECIFIED.)
CURVE()
GEOMETRIC_REPRESENTATION_ITEM()
RATIONAL_B_SPLINE_CURVE((1.,1.00061453665095,1.00078646015441))
REPRESENTATION_ITEM('')
);
#795=(
BOUNDED_CURVE()
B_SPLINE_CURVE(2,(#36576,#36577,#36578),.UNSPECIFIED.,.F.,.F.)
B_SPLINE_CURVE_WITH_KNOTS((3,3),(0.0380048027321657,0.0593935854477561),
 .UNSPECIFIED.)
CURVE()
GEOMETRIC_REPRESENTATION_ITEM()
RATIONAL_B_SPLINE_CURVE((1.00078646014826,1.00061453664614,1.))
REPRESENTATION_ITEM('')
);
#796=(
BOUNDED_CURVE()
B_SPLINE_CURVE(2,(#36582,#36583,#36584),.UNSPECIFIED.,.F.,.F.)
B_SPLINE_CURVE_WITH_KNOTS((3,3),(0.,0.0213887827154277),.UNSPECIFIED.)
CURVE()
GEOMETRIC_REPRESENTATION_ITEM()
RATIONAL_B_SPLINE_CURVE((1.,1.00061453665233,1.00078646015617))
REPRESENTATION_ITEM('')
);
#797=(
BOUNDED_CURVE()
B_SPLINE_CURVE(2,(#36586,#36587,#36588),.UNSPECIFIED.,.F.,.F.)
B_SPLINE_CURVE_WITH_KNOTS((3,3),(0.0380048027322445,0.0593935854477552),
 .UNSPECIFIED.)
CURVE()
GEOMETRIC_REPRESENTATION_ITEM()
RATIONAL_B_SPLINE_CURVE((1.00078646015087,1.00061453664819,1.))
REPRESENTATION_ITEM('')
);
#798=(
BOUNDED_CURVE()
B_SPLINE_CURVE(2,(#36592,#36593,#36594),.UNSPECIFIED.,.F.,.F.)
B_SPLINE_CURVE_WITH_KNOTS((3,3),(0.,0.0213887827154996),.UNSPECIFIED.)
CURVE()
GEOMETRIC_REPRESENTATION_ITEM()
RATIONAL_B_SPLINE_CURVE((1.,1.00061453665179,1.00078646015549))
REPRESENTATION_ITEM('')
);
#799=(
BOUNDED_CURVE()
B_SPLINE_CURVE(2,(#36596,#36597,#36598),.UNSPECIFIED.,.F.,.F.)
B_SPLINE_CURVE_WITH_KNOTS((3,3),(0.0380048027322845,0.0593935854477556),
 .UNSPECIFIED.)
CURVE()
GEOMETRIC_REPRESENTATION_ITEM()
RATIONAL_B_SPLINE_CURVE((1.00078646015637,1.00061453665248,1.))
REPRESENTATION_ITEM('')
);
#800=(
BOUNDED_CURVE()
B_SPLINE_CURVE(2,(#36602,#36603,#36604),.UNSPECIFIED.,.F.,.F.)
B_SPLINE_CURVE_WITH_KNOTS((3,3),(0.,0.0213887827155547),.UNSPECIFIED.)
CURVE()
GEOMETRIC_REPRESENTATION_ITEM()
RATIONAL_B_SPLINE_CURVE((1.,1.00061453664528,1.00078646014716))
REPRESENTATION_ITEM('')
);
#801=(
BOUNDED_CURVE()
B_SPLINE_CURVE(2,(#36606,#36607,#36608),.UNSPECIFIED.,.F.,.F.)
B_SPLINE_CURVE_WITH_KNOTS((3,3),(0.0380048027322622,0.0593935854477563),
 .UNSPECIFIED.)
CURVE()
GEOMETRIC_REPRESENTATION_ITEM()
RATIONAL_B_SPLINE_CURVE((1.0007864601608,1.00061453665594,1.))
REPRESENTATION_ITEM('')
);
#802=(
BOUNDED_CURVE()
B_SPLINE_CURVE(2,(#36612,#36613,#36614),.UNSPECIFIED.,.F.,.F.)
B_SPLINE_CURVE_WITH_KNOTS((3,3),(0.,0.021388782715527),.UNSPECIFIED.)
CURVE()
GEOMETRIC_REPRESENTATION_ITEM()
RATIONAL_B_SPLINE_CURVE((1.,1.00061453664858,1.00078646015138))
REPRESENTATION_ITEM('')
);
#803=(
BOUNDED_CURVE()
B_SPLINE_CURVE(2,(#36616,#36617,#36618),.UNSPECIFIED.,.F.,.F.)
B_SPLINE_CURVE_WITH_KNOTS((3,3),(0.0380048027322087,0.0593935854477563),
 .UNSPECIFIED.)
CURVE()
GEOMETRIC_REPRESENTATION_ITEM()
RATIONAL_B_SPLINE_CURVE((1.00078646015349,1.00061453665023,1.))
REPRESENTATION_ITEM('')
);
#804=(
BOUNDED_CURVE()
B_SPLINE_CURVE(2,(#36622,#36623,#36624),.UNSPECIFIED.,.F.,.F.)
B_SPLINE_CURVE_WITH_KNOTS((3,3),(0.,0.0213887827155107),.UNSPECIFIED.)
CURVE()
GEOMETRIC_REPRESENTATION_ITEM()
RATIONAL_B_SPLINE_CURVE((1.,1.00061453665077,1.00078646015419))
REPRESENTATION_ITEM('')
);
#805=(
BOUNDED_CURVE()
B_SPLINE_CURVE(2,(#36626,#36627,#36628),.UNSPECIFIED.,.F.,.F.)
B_SPLINE_CURVE_WITH_KNOTS((3,3),(0.0380048027321878,0.0593935854477555),
 .UNSPECIFIED.)
CURVE()
GEOMETRIC_REPRESENTATION_ITEM()
RATIONAL_B_SPLINE_CURVE((1.00078646014641,1.0006145366447,1.))
REPRESENTATION_ITEM('')
);
#806=(
BOUNDED_CURVE()
B_SPLINE_CURVE(2,(#36632,#36633,#36634),.UNSPECIFIED.,.F.,.F.)
B_SPLINE_CURVE_WITH_KNOTS((3,3),(0.,0.0213887827154949),.UNSPECIFIED.)
CURVE()
GEOMETRIC_REPRESENTATION_ITEM()
RATIONAL_B_SPLINE_CURVE((1.,1.00061453665079,1.00078646015421))
REPRESENTATION_ITEM('')
);
#807=(
BOUNDED_CURVE()
B_SPLINE_CURVE(2,(#36636,#36637,#36638),.UNSPECIFIED.,.F.,.F.)
B_SPLINE_CURVE_WITH_KNOTS((3,3),(0.038004802732195,0.0593935854477556),
 .UNSPECIFIED.)
CURVE()
GEOMETRIC_REPRESENTATION_ITEM()
RATIONAL_B_SPLINE_CURVE((1.0007864601493,1.00061453664696,1.))
REPRESENTATION_ITEM('')
);
#808=(
BOUNDED_CURVE()
B_SPLINE_CURVE(2,(#36642,#36643,#36644),.UNSPECIFIED.,.F.,.F.)
B_SPLINE_CURVE_WITH_KNOTS((3,3),(0.,0.0213887827155322),.UNSPECIFIED.)
CURVE()
GEOMETRIC_REPRESENTATION_ITEM()
RATIONAL_B_SPLINE_CURVE((1.,1.00061453664703,1.00078646014939))
REPRESENTATION_ITEM('')
);
#809=(
BOUNDED_CURVE()
B_SPLINE_CURVE(2,(#36646,#36647,#36648),.UNSPECIFIED.,.F.,.F.)
B_SPLINE_CURVE_WITH_KNOTS((3,3),(0.0380048027322535,0.0593935854477551),
 .UNSPECIFIED.)
CURVE()
GEOMETRIC_REPRESENTATION_ITEM()
RATIONAL_B_SPLINE_CURVE((1.00078646015018,1.00061453664765,1.))
REPRESENTATION_ITEM('')
);
#810=(
BOUNDED_CURVE()
B_SPLINE_CURVE(2,(#36652,#36653,#36654),.UNSPECIFIED.,.F.,.F.)
B_SPLINE_CURVE_WITH_KNOTS((3,3),(0.,0.0213887827155291),.UNSPECIFIED.)
CURVE()
GEOMETRIC_REPRESENTATION_ITEM()
RATIONAL_B_SPLINE_CURVE((1.,1.00061453664596,1.00078646014803))
REPRESENTATION_ITEM('')
);
#811=(
BOUNDED_CURVE()
B_SPLINE_CURVE(2,(#36656,#36657,#36658),.UNSPECIFIED.,.F.,.F.)
B_SPLINE_CURVE_WITH_KNOTS((3,3),(0.0380048027322346,0.0593935854477561),
 .UNSPECIFIED.)
CURVE()
GEOMETRIC_REPRESENTATION_ITEM()
RATIONAL_B_SPLINE_CURVE((1.00078646015205,1.00061453664911,1.))
REPRESENTATION_ITEM('')
);
#812=(
BOUNDED_CURVE()
B_SPLINE_CURVE(2,(#36662,#36663,#36664),.UNSPECIFIED.,.F.,.F.)
B_SPLINE_CURVE_WITH_KNOTS((3,3),(0.,0.0213887827155096),.UNSPECIFIED.)
CURVE()
GEOMETRIC_REPRESENTATION_ITEM()
RATIONAL_B_SPLINE_CURVE((1.,1.00061453664827,1.00078646015098))
REPRESENTATION_ITEM('')
);
#813=(
BOUNDED_CURVE()
B_SPLINE_CURVE(2,(#36666,#36667,#36668),.UNSPECIFIED.,.F.,.F.)
B_SPLINE_CURVE_WITH_KNOTS((3,3),(0.0380048027322829,0.0593935854477556),
 .UNSPECIFIED.)
CURVE()
GEOMETRIC_REPRESENTATION_ITEM()
RATIONAL_B_SPLINE_CURVE((1.00078646015816,1.00061453665388,1.))
REPRESENTATION_ITEM('')
);
#814=(
BOUNDED_CURVE()
B_SPLINE_CURVE(2,(#36672,#36673,#36674),.UNSPECIFIED.,.F.,.F.)
B_SPLINE_CURVE_WITH_KNOTS((3,3),(0.,0.0213887827155543),.UNSPECIFIED.)
CURVE()
GEOMETRIC_REPRESENTATION_ITEM()
RATIONAL_B_SPLINE_CURVE((1.,1.00061453664662,1.00078646014886))
REPRESENTATION_ITEM('')
);
#815=(
BOUNDED_CURVE()
B_SPLINE_CURVE(2,(#36676,#36677,#36678),.UNSPECIFIED.,.F.,.F.)
B_SPLINE_CURVE_WITH_KNOTS((3,3),(0.038004802732242,0.0593935854477554),
 .UNSPECIFIED.)
CURVE()
GEOMETRIC_REPRESENTATION_ITEM()
RATIONAL_B_SPLINE_CURVE((1.00078646015479,1.00061453665125,1.))
REPRESENTATION_ITEM('')
);
#816=(
BOUNDED_CURVE()
B_SPLINE_CURVE(2,(#36682,#36683,#36684),.UNSPECIFIED.,.F.,.F.)
B_SPLINE_CURVE_WITH_KNOTS((3,3),(0.,0.0213887827155011),.UNSPECIFIED.)
CURVE()
GEOMETRIC_REPRESENTATION_ITEM()
RATIONAL_B_SPLINE_CURVE((1.,1.00061453665297,1.000786460157))
REPRESENTATION_ITEM('')
);
#817=(
BOUNDED_CURVE()
B_SPLINE_CURVE(2,(#36686,#36687,#36688),.UNSPECIFIED.,.F.,.F.)
B_SPLINE_CURVE_WITH_KNOTS((3,3),(0.0380048027323167,0.0593935854477549),
 .UNSPECIFIED.)
CURVE()
GEOMETRIC_REPRESENTATION_ITEM()
RATIONAL_B_SPLINE_CURVE((1.00078646015665,1.0006145366527,1.))
REPRESENTATION_ITEM('')
);
#818=(
BOUNDED_CURVE()
B_SPLINE_CURVE(2,(#36692,#36693,#36694),.UNSPECIFIED.,.F.,.F.)
B_SPLINE_CURVE_WITH_KNOTS((3,3),(0.,0.0213887827155084),.UNSPECIFIED.)
CURVE()
GEOMETRIC_REPRESENTATION_ITEM()
RATIONAL_B_SPLINE_CURVE((1.,1.00061453665162,1.00078646015527))
REPRESENTATION_ITEM('')
);
#819=(
BOUNDED_CURVE()
B_SPLINE_CURVE(2,(#36696,#36697,#36698),.UNSPECIFIED.,.F.,.F.)
B_SPLINE_CURVE_WITH_KNOTS((3,3),(0.0380048027322826,0.0593935854477556),
 .UNSPECIFIED.)
CURVE()
GEOMETRIC_REPRESENTATION_ITEM()
RATIONAL_B_SPLINE_CURVE((1.00078646015745,1.00061453665332,1.))
REPRESENTATION_ITEM('')
);
#820=(
BOUNDED_CURVE()
B_SPLINE_CURVE(2,(#36702,#36703,#36704),.UNSPECIFIED.,.F.,.F.)
B_SPLINE_CURVE_WITH_KNOTS((3,3),(0.,0.0213887827154213),.UNSPECIFIED.)
CURVE()
GEOMETRIC_REPRESENTATION_ITEM()
RATIONAL_B_SPLINE_CURVE((1.,1.00061453665618,1.00078646016111))
REPRESENTATION_ITEM('')
);
#821=(
BOUNDED_CURVE()
B_SPLINE_CURVE(2,(#36706,#36707,#36708),.UNSPECIFIED.,.F.,.F.)
B_SPLINE_CURVE_WITH_KNOTS((3,3),(0.0380048027322973,0.0593935854477563),
 .UNSPECIFIED.)
CURVE()
GEOMETRIC_REPRESENTATION_ITEM()
RATIONAL_B_SPLINE_CURVE((1.00078646016316,1.00061453665778,1.))
REPRESENTATION_ITEM('')
);
#822=(
BOUNDED_CURVE()
B_SPLINE_CURVE(2,(#36712,#36713,#36714),.UNSPECIFIED.,.F.,.F.)
B_SPLINE_CURVE_WITH_KNOTS((3,3),(0.,0.0213887827154844),.UNSPECIFIED.)
CURVE()
GEOMETRIC_REPRESENTATION_ITEM()
RATIONAL_B_SPLINE_CURVE((1.,1.00061453665096,1.00078646015442))
REPRESENTATION_ITEM('')
);
#823=(
BOUNDED_CURVE()
B_SPLINE_CURVE(2,(#36716,#36717,#36718),.UNSPECIFIED.,.F.,.F.)
B_SPLINE_CURVE_WITH_KNOTS((3,3),(0.0380048027322098,0.0593935854477563),
 .UNSPECIFIED.)
CURVE()
GEOMETRIC_REPRESENTATION_ITEM()
RATIONAL_B_SPLINE_CURVE((1.0007864601532,1.00061453665,1.))
REPRESENTATION_ITEM('')
);
#824=(
BOUNDED_CURVE()
B_SPLINE_CURVE(2,(#36722,#36723,#36724),.UNSPECIFIED.,.F.,.F.)
B_SPLINE_CURVE_WITH_KNOTS((3,3),(0.,0.0213887827154289),.UNSPECIFIED.)
CURVE()
GEOMETRIC_REPRESENTATION_ITEM()
RATIONAL_B_SPLINE_CURVE((1.,1.00061453665625,1.0007864601612))
REPRESENTATION_ITEM('')
);
#825=(
BOUNDED_CURVE()
B_SPLINE_CURVE(2,(#36726,#36727,#36728),.UNSPECIFIED.,.F.,.F.)
B_SPLINE_CURVE_WITH_KNOTS((3,3),(0.0380048027322686,0.0593935854477554),
 .UNSPECIFIED.)
CURVE()
GEOMETRIC_REPRESENTATION_ITEM()
RATIONAL_B_SPLINE_CURVE((1.00078646015899,1.00061453665453,1.))
REPRESENTATION_ITEM('')
);
#826=(
BOUNDED_CURVE()
B_SPLINE_CURVE(2,(#36733,#36734,#36735),.UNSPECIFIED.,.F.,.F.)
B_SPLINE_CURVE_WITH_KNOTS((3,3),(0.,0.0213887827155324),.UNSPECIFIED.)
CURVE()
GEOMETRIC_REPRESENTATION_ITEM()
RATIONAL_B_SPLINE_CURVE((1.,1.00061453664729,1.00078646014973))
REPRESENTATION_ITEM('')
);
#827=(
BOUNDED_CURVE()
B_SPLINE_CURVE(2,(#36737,#36738,#36739),.UNSPECIFIED.,.F.,.F.)
B_SPLINE_CURVE_WITH_KNOTS((3,3),(0.0380048027322402,0.0593935854477561),
 .UNSPECIFIED.)
CURVE()
GEOMETRIC_REPRESENTATION_ITEM()
RATIONAL_B_SPLINE_CURVE((1.00078646015472,1.00061453665119,1.))
REPRESENTATION_ITEM('')
);
#828=(
BOUNDED_CURVE()
B_SPLINE_CURVE(2,(#36743,#36744,#36745),.UNSPECIFIED.,.F.,.F.)
B_SPLINE_CURVE_WITH_KNOTS((3,3),(0.,0.0213887827154487),.UNSPECIFIED.)
CURVE()
GEOMETRIC_REPRESENTATION_ITEM()
RATIONAL_B_SPLINE_CURVE((1.,1.00061453665353,1.00078646015771))
REPRESENTATION_ITEM('')
);
#829=(
BOUNDED_CURVE()
B_SPLINE_CURVE(2,(#36747,#36748,#36749),.UNSPECIFIED.,.F.,.F.)
B_SPLINE_CURVE_WITH_KNOTS((3,3),(0.0380048027323105,0.0593935854477551),
 .UNSPECIFIED.)
CURVE()
GEOMETRIC_REPRESENTATION_ITEM()
RATIONAL_B_SPLINE_CURVE((1.00078646015948,1.00061453665491,1.))
REPRESENTATION_ITEM('')
);
#830=(
BOUNDED_CURVE()
B_SPLINE_CURVE(2,(#36753,#36754,#36755),.UNSPECIFIED.,.F.,.F.)
B_SPLINE_CURVE_WITH_KNOTS((3,3),(0.,0.0213887827154801),.UNSPECIFIED.)
CURVE()
GEOMETRIC_REPRESENTATION_ITEM()
RATIONAL_B_SPLINE_CURVE((1.,1.00061453665439,1.00078646015881))
REPRESENTATION_ITEM('')
);
#831=(
BOUNDED_CURVE()
B_SPLINE_CURVE(2,(#36757,#36758,#36759),.UNSPECIFIED.,.F.,.F.)
B_SPLINE_CURVE_WITH_KNOTS((3,3),(0.0380048027322703,0.0593935854477551),
 .UNSPECIFIED.)
CURVE()
GEOMETRIC_REPRESENTATION_ITEM()
RATIONAL_B_SPLINE_CURVE((1.00078646015419,1.00061453665078,1.))
REPRESENTATION_ITEM('')
);
#832=(
BOUNDED_CURVE()
B_SPLINE_CURVE(2,(#36763,#36764,#36765),.UNSPECIFIED.,.F.,.F.)
B_SPLINE_CURVE_WITH_KNOTS((3,3),(0.,0.0213887827154732),.UNSPECIFIED.)
CURVE()
GEOMETRIC_REPRESENTATION_ITEM()
RATIONAL_B_SPLINE_CURVE((1.,1.00061453665189,1.00078646015561))
REPRESENTATION_ITEM('')
);
#833=(
BOUNDED_CURVE()
B_SPLINE_CURVE(2,(#36767,#36768,#36769),.UNSPECIFIED.,.F.,.F.)
B_SPLINE_CURVE_WITH_KNOTS((3,3),(0.0380048027323814,0.0593935854477557),
 .UNSPECIFIED.)
CURVE()
GEOMETRIC_REPRESENTATION_ITEM()
RATIONAL_B_SPLINE_CURVE((1.00078646016718,1.00061453666093,1.))
REPRESENTATION_ITEM('')
);
#834=(
BOUNDED_CURVE()
B_SPLINE_CURVE(2,(#36773,#36774,#36775),.UNSPECIFIED.,.F.,.F.)
B_SPLINE_CURVE_WITH_KNOTS((3,3),(0.,0.0213887827155284),.UNSPECIFIED.)
CURVE()
GEOMETRIC_REPRESENTATION_ITEM()
RATIONAL_B_SPLINE_CURVE((1.,1.00061453664637,1.00078646014855))
REPRESENTATION_ITEM('')
);
#835=(
BOUNDED_CURVE()
B_SPLINE_CURVE(2,(#36777,#36778,#36779),.UNSPECIFIED.,.F.,.F.)
B_SPLINE_CURVE_WITH_KNOTS((3,3),(0.0380048027322513,0.0593935854477563),
 .UNSPECIFIED.)
CURVE()
GEOMETRIC_REPRESENTATION_ITEM()
RATIONAL_B_SPLINE_CURVE((1.00078646015572,1.00061453665197,1.))
REPRESENTATION_ITEM('')
);
#836=(
BOUNDED_CURVE()
B_SPLINE_CURVE(2,(#36783,#36784,#36785),.UNSPECIFIED.,.F.,.F.)
B_SPLINE_CURVE_WITH_KNOTS((3,3),(0.,0.0213887827154905),.UNSPECIFIED.)
CURVE()
GEOMETRIC_REPRESENTATION_ITEM()
RATIONAL_B_SPLINE_CURVE((1.,1.00061453665389,1.00078646015818))
REPRESENTATION_ITEM('')
);
#837=(
BOUNDED_CURVE()
B_SPLINE_CURVE(2,(#36787,#36788,#36789),.UNSPECIFIED.,.F.,.F.)
B_SPLINE_CURVE_WITH_KNOTS((3,3),(0.0380048027322515,0.0593935854477557),
 .UNSPECIFIED.)
CURVE()
GEOMETRIC_REPRESENTATION_ITEM()
RATIONAL_B_SPLINE_CURVE((1.00078646015577,1.00061453665201,1.))
REPRESENTATION_ITEM('')
);
#838=(
BOUNDED_CURVE()
B_SPLINE_CURVE(2,(#36793,#36794,#36795),.UNSPECIFIED.,.F.,.F.)
B_SPLINE_CURVE_WITH_KNOTS((3,3),(0.,0.0213887827155349),.UNSPECIFIED.)
CURVE()
GEOMETRIC_REPRESENTATION_ITEM()
RATIONAL_B_SPLINE_CURVE((1.,1.00061453664595,1.000786460148))
REPRESENTATION_ITEM('')
);
#839=(
BOUNDED_CURVE()
B_SPLINE_CURVE(2,(#36797,#36798,#36799),.UNSPECIFIED.,.F.,.F.)
B_SPLINE_CURVE_WITH_KNOTS((3,3),(0.0380048027322051,0.0593935854477563),
 .UNSPECIFIED.)
CURVE()
GEOMETRIC_REPRESENTATION_ITEM()
RATIONAL_B_SPLINE_CURVE((1.00078646015312,1.00061453664994,1.))
REPRESENTATION_ITEM('')
);
#840=(
BOUNDED_CURVE()
B_SPLINE_CURVE(2,(#36803,#36804,#36805),.UNSPECIFIED.,.F.,.F.)
B_SPLINE_CURVE_WITH_KNOTS((3,3),(0.,0.0213887827155927),.UNSPECIFIED.)
CURVE()
GEOMETRIC_REPRESENTATION_ITEM()
RATIONAL_B_SPLINE_CURVE((1.,1.00061453664415,1.0007864601457))
REPRESENTATION_ITEM('')
);
#841=(
BOUNDED_CURVE()
B_SPLINE_CURVE(2,(#36807,#36808,#36809),.UNSPECIFIED.,.F.,.F.)
B_SPLINE_CURVE_WITH_KNOTS((3,3),(0.038004802732226,0.0593935854477556),
 .UNSPECIFIED.)
CURVE()
GEOMETRIC_REPRESENTATION_ITEM()
RATIONAL_B_SPLINE_CURVE((1.0007864601527,1.00061453664962,1.))
REPRESENTATION_ITEM('')
);
#842=(
BOUNDED_CURVE()
B_SPLINE_CURVE(2,(#36813,#36814,#36815),.UNSPECIFIED.,.F.,.F.)
B_SPLINE_CURVE_WITH_KNOTS((3,3),(0.,0.0213887827155911),.UNSPECIFIED.)
CURVE()
GEOMETRIC_REPRESENTATION_ITEM()
RATIONAL_B_SPLINE_CURVE((1.,1.00061453664496,1.00078646014675))
REPRESENTATION_ITEM('')
);
#843=(
BOUNDED_CURVE()
B_SPLINE_CURVE(2,(#36817,#36818,#36819),.UNSPECIFIED.,.F.,.F.)
B_SPLINE_CURVE_WITH_KNOTS((3,3),(0.0380048027321543,0.059393585447757),
 .UNSPECIFIED.)
CURVE()
GEOMETRIC_REPRESENTATION_ITEM()
RATIONAL_B_SPLINE_CURVE((1.0007864601479,1.00061453664586,1.))
REPRESENTATION_ITEM('')
);
#844=(
BOUNDED_CURVE()
B_SPLINE_CURVE(2,(#36823,#36824,#36825),.UNSPECIFIED.,.F.,.F.)
B_SPLINE_CURVE_WITH_KNOTS((3,3),(0.,0.0213887827155128),.UNSPECIFIED.)
CURVE()
GEOMETRIC_REPRESENTATION_ITEM()
RATIONAL_B_SPLINE_CURVE((1.,1.00061453664886,1.00078646015173))
REPRESENTATION_ITEM('')
);
#845=(
BOUNDED_CURVE()
B_SPLINE_CURVE(2,(#36827,#36828,#36829),.UNSPECIFIED.,.F.,.F.)
B_SPLINE_CURVE_WITH_KNOTS((3,3),(0.0380048027322768,0.0593935854477557),
 .UNSPECIFIED.)
CURVE()
GEOMETRIC_REPRESENTATION_ITEM()
RATIONAL_B_SPLINE_CURVE((1.00078646015618,1.00061453665233,1.))
REPRESENTATION_ITEM('')
);
#846=(
BOUNDED_CURVE()
B_SPLINE_CURVE(2,(#36833,#36834,#36835),.UNSPECIFIED.,.F.,.F.)
B_SPLINE_CURVE_WITH_KNOTS((3,3),(0.,0.0213887827155095),.UNSPECIFIED.)
CURVE()
GEOMETRIC_REPRESENTATION_ITEM()
RATIONAL_B_SPLINE_CURVE((1.,1.00061453664827,1.00078646015098))
REPRESENTATION_ITEM('')
);
#847=(
BOUNDED_CURVE()
B_SPLINE_CURVE(2,(#36837,#36838,#36839),.UNSPECIFIED.,.F.,.F.)
B_SPLINE_CURVE_WITH_KNOTS((3,3),(0.0380048027321875,0.0593935854477551),
 .UNSPECIFIED.)
CURVE()
GEOMETRIC_REPRESENTATION_ITEM()
RATIONAL_B_SPLINE_CURVE((1.00078646014592,1.00061453664432,1.))
REPRESENTATION_ITEM('')
);
#848=(
BOUNDED_CURVE()
B_SPLINE_CURVE(2,(#36843,#36844,#36845),.UNSPECIFIED.,.F.,.F.)
B_SPLINE_CURVE_WITH_KNOTS((3,3),(0.,0.0213887827154677),.UNSPECIFIED.)
CURVE()
GEOMETRIC_REPRESENTATION_ITEM()
RATIONAL_B_SPLINE_CURVE((1.,1.00061453665162,1.00078646015527))
REPRESENTATION_ITEM('')
);
#849=(
BOUNDED_CURVE()
B_SPLINE_CURVE(2,(#36847,#36848,#36849),.UNSPECIFIED.,.F.,.F.)
B_SPLINE_CURVE_WITH_KNOTS((3,3),(0.0380048027322803,0.059393585447756),
 .UNSPECIFIED.)
CURVE()
GEOMETRIC_REPRESENTATION_ITEM()
RATIONAL_B_SPLINE_CURVE((1.00078646015832,1.000614536654,1.))
REPRESENTATION_ITEM('')
);
#850=(
BOUNDED_CURVE()
B_SPLINE_CURVE(2,(#36853,#36854,#36855),.UNSPECIFIED.,.F.,.F.)
B_SPLINE_CURVE_WITH_KNOTS((3,3),(0.,0.0213887827154919),.UNSPECIFIED.)
CURVE()
GEOMETRIC_REPRESENTATION_ITEM()
RATIONAL_B_SPLINE_CURVE((1.,1.00061453665363,1.00078646015784))
REPRESENTATION_ITEM('')
);
#851=(
BOUNDED_CURVE()
B_SPLINE_CURVE(2,(#36857,#36858,#36859),.UNSPECIFIED.,.F.,.F.)
B_SPLINE_CURVE_WITH_KNOTS((3,3),(0.0380048027322449,0.0593935854477551),
 .UNSPECIFIED.)
CURVE()
GEOMETRIC_REPRESENTATION_ITEM()
RATIONAL_B_SPLINE_CURVE((1.00078646015292,1.00061453664979,1.))
REPRESENTATION_ITEM('')
);
#852=(
BOUNDED_CURVE()
B_SPLINE_CURVE(2,(#36863,#36864,#36865),.UNSPECIFIED.,.F.,.F.)
B_SPLINE_CURVE_WITH_KNOTS((3,3),(0.,0.021388782715506),.UNSPECIFIED.)
CURVE()
GEOMETRIC_REPRESENTATION_ITEM()
RATIONAL_B_SPLINE_CURVE((1.,1.00061453665225,1.00078646015607))
REPRESENTATION_ITEM('')
);
#853=(
BOUNDED_CURVE()
B_SPLINE_CURVE(2,(#36867,#36868,#36869),.UNSPECIFIED.,.F.,.F.)
B_SPLINE_CURVE_WITH_KNOTS((3,3),(0.0380048027322685,0.0593935854477556),
 .UNSPECIFIED.)
CURVE()
GEOMETRIC_REPRESENTATION_ITEM()
RATIONAL_B_SPLINE_CURVE((1.00078646015217,1.0006145366492,1.))
REPRESENTATION_ITEM('')
);
#854=(
BOUNDED_CURVE()
B_SPLINE_CURVE(2,(#36873,#36874,#36875),.UNSPECIFIED.,.F.,.F.)
B_SPLINE_CURVE_WITH_KNOTS((3,3),(0.,0.0213887827154673),.UNSPECIFIED.)
CURVE()
GEOMETRIC_REPRESENTATION_ITEM()
RATIONAL_B_SPLINE_CURVE((1.,1.00061453665233,1.00078646015618))
REPRESENTATION_ITEM('')
);
#855=(
BOUNDED_CURVE()
B_SPLINE_CURVE(2,(#36877,#36878,#36879),.UNSPECIFIED.,.F.,.F.)
B_SPLINE_CURVE_WITH_KNOTS((3,3),(0.0380048027322247,0.059393585447756),
 .UNSPECIFIED.)
CURVE()
GEOMETRIC_REPRESENTATION_ITEM()
RATIONAL_B_SPLINE_CURVE((1.00078646015399,1.00061453665062,1.))
REPRESENTATION_ITEM('')
);
#856=(
BOUNDED_CURVE()
B_SPLINE_CURVE(2,(#36883,#36884,#36885),.UNSPECIFIED.,.F.,.F.)
B_SPLINE_CURVE_WITH_KNOTS((3,3),(0.,0.0213887827154374),.UNSPECIFIED.)
CURVE()
GEOMETRIC_REPRESENTATION_ITEM()
RATIONAL_B_SPLINE_CURVE((1.,1.00061453665411,1.00078646015846))
REPRESENTATION_ITEM('')
);
#857=(
BOUNDED_CURVE()
B_SPLINE_CURVE(2,(#36887,#36888,#36889),.UNSPECIFIED.,.F.,.F.)
B_SPLINE_CURVE_WITH_KNOTS((3,3),(0.0380048027322071,0.0593935854477556),
 .UNSPECIFIED.)
CURVE()
GEOMETRIC_REPRESENTATION_ITEM()
RATIONAL_B_SPLINE_CURVE((1.00078646015371,1.0006145366504,1.))
REPRESENTATION_ITEM('')
);
#858=(
BOUNDED_CURVE()
B_SPLINE_CURVE(2,(#36892,#36893,#36894),.UNSPECIFIED.,.F.,.F.)
B_SPLINE_CURVE_WITH_KNOTS((3,3),(0.,0.0213887827155641),.UNSPECIFIED.)
CURVE()
GEOMETRIC_REPRESENTATION_ITEM()
RATIONAL_B_SPLINE_CURVE((1.,1.00061453664786,1.00078646015045))
REPRESENTATION_ITEM('')
);
#859=(
BOUNDED_CURVE()
B_SPLINE_CURVE(2,(#58913,#58914,#58915),.UNSPECIFIED.,.F.,.F.)
B_SPLINE_CURVE_WITH_KNOTS((3,3),(0.,0.0213887827154485),.UNSPECIFIED.)
CURVE()
GEOMETRIC_REPRESENTATION_ITEM()
RATIONAL_B_SPLINE_CURVE((1.,1.0006145366538,1.00078646015806))
REPRESENTATION_ITEM('')
);
#860=(
BOUNDED_CURVE()
B_SPLINE_CURVE(2,(#58918,#58919,#58920),.UNSPECIFIED.,.F.,.F.)
B_SPLINE_CURVE_WITH_KNOTS((3,3),(0.0380048027322743,0.0593935854477577),
 .UNSPECIFIED.)
CURVE()
GEOMETRIC_REPRESENTATION_ITEM()
RATIONAL_B_SPLINE_CURVE((1.00078646015726,1.00061453665318,1.))
REPRESENTATION_ITEM('')
);
#861=(
BOUNDED_CURVE()
B_SPLINE_CURVE(2,(#58929,#58930,#58931),.UNSPECIFIED.,.F.,.F.)
B_SPLINE_CURVE_WITH_KNOTS((3,3),(0.0380048027323083,0.0593935854477567),
 .UNSPECIFIED.)
CURVE()
GEOMETRIC_REPRESENTATION_ITEM()
RATIONAL_B_SPLINE_CURVE((1.00078646016055,1.00061453665575,1.))
REPRESENTATION_ITEM('')
);
#862=(
BOUNDED_CURVE()
B_SPLINE_CURVE(2,(#58935,#58936,#58937),.UNSPECIFIED.,.F.,.F.)
B_SPLINE_CURVE_WITH_KNOTS((3,3),(0.,0.0213887827154447),.UNSPECIFIED.)
CURVE()
GEOMETRIC_REPRESENTATION_ITEM()
RATIONAL_B_SPLINE_CURVE((1.,1.00061453665542,1.00078646016013))
REPRESENTATION_ITEM('')
);
#863=(
BOUNDED_CURVE()
B_SPLINE_CURVE(2,(#58939,#58940,#58941),.UNSPECIFIED.,.F.,.F.)
B_SPLINE_CURVE_WITH_KNOTS((3,3),(0.0380048027323192,0.0593935854477567),
 .UNSPECIFIED.)
CURVE()
GEOMETRIC_REPRESENTATION_ITEM()
RATIONAL_B_SPLINE_CURVE((1.0007864601593,1.00061453665477,1.))
REPRESENTATION_ITEM('')
);
#864=(
BOUNDED_CURVE()
B_SPLINE_CURVE(2,(#58945,#58946,#58947),.UNSPECIFIED.,.F.,.F.)
B_SPLINE_CURVE_WITH_KNOTS((3,3),(0.,0.0213887827154334),.UNSPECIFIED.)
CURVE()
GEOMETRIC_REPRESENTATION_ITEM()
RATIONAL_B_SPLINE_CURVE((1.,1.00061453665449,1.00078646015894))
REPRESENTATION_ITEM('')
);
#865=(
BOUNDED_CURVE()
B_SPLINE_CURVE(2,(#58949,#58950,#58951),.UNSPECIFIED.,.F.,.F.)
B_SPLINE_CURVE_WITH_KNOTS((3,3),(0.0380048027322763,0.0593935854477568),
 .UNSPECIFIED.)
CURVE()
GEOMETRIC_REPRESENTATION_ITEM()
RATIONAL_B_SPLINE_CURVE((1.00078646015818,1.00061453665389,1.))
REPRESENTATION_ITEM('')
);
#866=(
BOUNDED_CURVE()
B_SPLINE_CURVE(2,(#58955,#58956,#58957),.UNSPECIFIED.,.F.,.F.)
B_SPLINE_CURVE_WITH_KNOTS((3,3),(0.,0.0213887827154747),.UNSPECIFIED.)
CURVE()
GEOMETRIC_REPRESENTATION_ITEM()
RATIONAL_B_SPLINE_CURVE((1.,1.00061453665232,1.00078646015616))
REPRESENTATION_ITEM('')
);
#867=(
BOUNDED_CURVE()
B_SPLINE_CURVE(2,(#58959,#58960,#58961),.UNSPECIFIED.,.F.,.F.)
B_SPLINE_CURVE_WITH_KNOTS((3,3),(0.0380048027322871,0.0593935854477566),
 .UNSPECIFIED.)
CURVE()
GEOMETRIC_REPRESENTATION_ITEM()
RATIONAL_B_SPLINE_CURVE((1.00078646015913,1.00061453665464,1.))
REPRESENTATION_ITEM('')
);
#868=(
BOUNDED_CURVE()
B_SPLINE_CURVE(2,(#58965,#58966,#58967),.UNSPECIFIED.,.F.,.F.)
B_SPLINE_CURVE_WITH_KNOTS((3,3),(0.,0.0213887827154556),.UNSPECIFIED.)
CURVE()
GEOMETRIC_REPRESENTATION_ITEM()
RATIONAL_B_SPLINE_CURVE((1.,1.00061453665459,1.00078646015907))
REPRESENTATION_ITEM('')
);
#869=(
BOUNDED_CURVE()
B_SPLINE_CURVE(2,(#58969,#58970,#58971),.UNSPECIFIED.,.F.,.F.)
B_SPLINE_CURVE_WITH_KNOTS((3,3),(0.0380048027322698,0.0593935854477568),
 .UNSPECIFIED.)
CURVE()
GEOMETRIC_REPRESENTATION_ITEM()
RATIONAL_B_SPLINE_CURVE((1.000786460157,1.00061453665298,1.))
REPRESENTATION_ITEM('')
);
#870=(
BOUNDED_CURVE()
B_SPLINE_CURVE(2,(#58975,#58976,#58977),.UNSPECIFIED.,.F.,.F.)
B_SPLINE_CURVE_WITH_KNOTS((3,3),(0.,0.0213887827154226),.UNSPECIFIED.)
CURVE()
GEOMETRIC_REPRESENTATION_ITEM()
RATIONAL_B_SPLINE_CURVE((1.,1.00061453665557,1.00078646016033))
REPRESENTATION_ITEM('')
);
#871=(
BOUNDED_CURVE()
B_SPLINE_CURVE(2,(#58979,#58980,#58981),.UNSPECIFIED.,.F.,.F.)
B_SPLINE_CURVE_WITH_KNOTS((3,3),(0.0380048027322981,0.0593935854477561),
 .UNSPECIFIED.)
CURVE()
GEOMETRIC_REPRESENTATION_ITEM()
RATIONAL_B_SPLINE_CURVE((1.00078646015658,1.00061453665264,1.))
REPRESENTATION_ITEM('')
);
#872=(
BOUNDED_CURVE()
B_SPLINE_CURVE(2,(#58985,#58986,#58987),.UNSPECIFIED.,.F.,.F.)
B_SPLINE_CURVE_WITH_KNOTS((3,3),(0.,0.0213887827154885),.UNSPECIFIED.)
CURVE()
GEOMETRIC_REPRESENTATION_ITEM()
RATIONAL_B_SPLINE_CURVE((1.,1.00061453665414,1.00078646015849))
REPRESENTATION_ITEM('')
);
#873=(
BOUNDED_CURVE()
B_SPLINE_CURVE(2,(#58989,#58990,#58991),.UNSPECIFIED.,.F.,.F.)
B_SPLINE_CURVE_WITH_KNOTS((3,3),(0.0380048027323009,0.0593935854477566),
 .UNSPECIFIED.)
CURVE()
GEOMETRIC_REPRESENTATION_ITEM()
RATIONAL_B_SPLINE_CURVE((1.00078646015915,1.00061453665465,1.))
REPRESENTATION_ITEM('')
);
#874=(
BOUNDED_CURVE()
B_SPLINE_CURVE(2,(#58995,#58996,#58997),.UNSPECIFIED.,.F.,.F.)
B_SPLINE_CURVE_WITH_KNOTS((3,3),(0.,0.0213887827154357),.UNSPECIFIED.)
CURVE()
GEOMETRIC_REPRESENTATION_ITEM()
RATIONAL_B_SPLINE_CURVE((1.,1.00061453665688,1.000786460162))
REPRESENTATION_ITEM('')
);
#875=(
BOUNDED_CURVE()
B_SPLINE_CURVE(2,(#58999,#59000,#59001),.UNSPECIFIED.,.F.,.F.)
B_SPLINE_CURVE_WITH_KNOTS((3,3),(0.0380048027323154,0.059393585447756),
 .UNSPECIFIED.)
CURVE()
GEOMETRIC_REPRESENTATION_ITEM()
RATIONAL_B_SPLINE_CURVE((1.00078646016079,1.00061453665593,1.))
REPRESENTATION_ITEM('')
);
#876=(
BOUNDED_CURVE()
B_SPLINE_CURVE(2,(#59005,#59006,#59007),.UNSPECIFIED.,.F.,.F.)
B_SPLINE_CURVE_WITH_KNOTS((3,3),(0.,0.0213887827154912),.UNSPECIFIED.)
CURVE()
GEOMETRIC_REPRESENTATION_ITEM()
RATIONAL_B_SPLINE_CURVE((1.,1.00061453665086,1.0007864601543))
REPRESENTATION_ITEM('')
);
#877=(
BOUNDED_CURVE()
B_SPLINE_CURVE(2,(#59009,#59010,#59011),.UNSPECIFIED.,.F.,.F.)
B_SPLINE_CURVE_WITH_KNOTS((3,3),(0.0380048027322925,0.0593935854477561),
 .UNSPECIFIED.)
CURVE()
GEOMETRIC_REPRESENTATION_ITEM()
RATIONAL_B_SPLINE_CURVE((1.00078646015764,1.00061453665347,1.))
REPRESENTATION_ITEM('')
);
#878=(
BOUNDED_CURVE()
B_SPLINE_CURVE(2,(#59015,#59016,#59017),.UNSPECIFIED.,.F.,.F.)
B_SPLINE_CURVE_WITH_KNOTS((3,3),(0.,0.0213887827155107),.UNSPECIFIED.)
CURVE()
GEOMETRIC_REPRESENTATION_ITEM()
RATIONAL_B_SPLINE_CURVE((1.,1.00061453665119,1.00078646015471))
REPRESENTATION_ITEM('')
);
#879=(
BOUNDED_CURVE()
B_SPLINE_CURVE(2,(#59019,#59020,#59021),.UNSPECIFIED.,.F.,.F.)
B_SPLINE_CURVE_WITH_KNOTS((3,3),(0.038004802732295,0.0593935854477563),
 .UNSPECIFIED.)
CURVE()
GEOMETRIC_REPRESENTATION_ITEM()
RATIONAL_B_SPLINE_CURVE((1.00078646016111,1.00061453665618,1.))
REPRESENTATION_ITEM('')
);
#880=(
BOUNDED_CURVE()
B_SPLINE_CURVE(2,(#59025,#59026,#59027),.UNSPECIFIED.,.F.,.F.)
B_SPLINE_CURVE_WITH_KNOTS((3,3),(0.,0.0213887827154503),.UNSPECIFIED.)
CURVE()
GEOMETRIC_REPRESENTATION_ITEM()
RATIONAL_B_SPLINE_CURVE((1.,1.00061453665305,1.00078646015709))
REPRESENTATION_ITEM('')
);
#881=(
BOUNDED_CURVE()
B_SPLINE_CURVE(2,(#59029,#59030,#59031),.UNSPECIFIED.,.F.,.F.)
B_SPLINE_CURVE_WITH_KNOTS((3,3),(0.0380048027323246,0.059393585447756),
 .UNSPECIFIED.)
CURVE()
GEOMETRIC_REPRESENTATION_ITEM()
RATIONAL_B_SPLINE_CURVE((1.00078646015741,1.00061453665329,1.))
REPRESENTATION_ITEM('')
);
#882=(
BOUNDED_CURVE()
B_SPLINE_CURVE(2,(#59035,#59036,#59037),.UNSPECIFIED.,.F.,.F.)
B_SPLINE_CURVE_WITH_KNOTS((3,3),(0.,0.0213887827154455),.UNSPECIFIED.)
CURVE()
GEOMETRIC_REPRESENTATION_ITEM()
RATIONAL_B_SPLINE_CURVE((1.,1.00061453665435,1.00078646015877))
REPRESENTATION_ITEM('')
);
#883=(
BOUNDED_CURVE()
B_SPLINE_CURVE(2,(#59039,#59040,#59041),.UNSPECIFIED.,.F.,.F.)
B_SPLINE_CURVE_WITH_KNOTS((3,3),(0.0380048027322671,0.0593935854477559),
 .UNSPECIFIED.)
CURVE()
GEOMETRIC_REPRESENTATION_ITEM()
RATIONAL_B_SPLINE_CURVE((1.00078646015673,1.00061453665277,1.))
REPRESENTATION_ITEM('')
);
#884=(
BOUNDED_CURVE()
B_SPLINE_CURVE(2,(#59045,#59046,#59047),.UNSPECIFIED.,.F.,.F.)
B_SPLINE_CURVE_WITH_KNOTS((3,3),(0.,0.0213887827154328),.UNSPECIFIED.)
CURVE()
GEOMETRIC_REPRESENTATION_ITEM()
RATIONAL_B_SPLINE_CURVE((1.,1.0006145366569,1.00078646016203))
REPRESENTATION_ITEM('')
);
#885=(
BOUNDED_CURVE()
B_SPLINE_CURVE(2,(#59049,#59050,#59051),.UNSPECIFIED.,.F.,.F.)
B_SPLINE_CURVE_WITH_KNOTS((3,3),(0.0380048027322495,0.0593935854477564),
 .UNSPECIFIED.)
CURVE()
GEOMETRIC_REPRESENTATION_ITEM()
RATIONAL_B_SPLINE_CURVE((1.0007864601568,1.00061453665282,1.))
REPRESENTATION_ITEM('')
);
#886=(
BOUNDED_CURVE()
B_SPLINE_CURVE(2,(#59055,#59056,#59057),.UNSPECIFIED.,.F.,.F.)
B_SPLINE_CURVE_WITH_KNOTS((3,3),(0.,0.0213887827154736),.UNSPECIFIED.)
CURVE()
GEOMETRIC_REPRESENTATION_ITEM()
RATIONAL_B_SPLINE_CURVE((1.,1.0006145366516,1.00078646015525))
REPRESENTATION_ITEM('')
);
#887=(
BOUNDED_CURVE()
B_SPLINE_CURVE(2,(#59059,#59060,#59061),.UNSPECIFIED.,.F.,.F.)
B_SPLINE_CURVE_WITH_KNOTS((3,3),(0.0380048027322323,0.0593935854477557),
 .UNSPECIFIED.)
CURVE()
GEOMETRIC_REPRESENTATION_ITEM()
RATIONAL_B_SPLINE_CURVE((1.00078646015266,1.00061453664958,1.))
REPRESENTATION_ITEM('')
);
#888=(
BOUNDED_CURVE()
B_SPLINE_CURVE(2,(#59065,#59066,#59067),.UNSPECIFIED.,.F.,.F.)
B_SPLINE_CURVE_WITH_KNOTS((3,3),(0.,0.0213887827154861),.UNSPECIFIED.)
CURVE()
GEOMETRIC_REPRESENTATION_ITEM()
RATIONAL_B_SPLINE_CURVE((1.,1.00061453665221,1.00078646015603))
REPRESENTATION_ITEM('')
);
#889=(
BOUNDED_CURVE()
B_SPLINE_CURVE(2,(#59069,#59070,#59071),.UNSPECIFIED.,.F.,.F.)
B_SPLINE_CURVE_WITH_KNOTS((3,3),(0.038004802732259,0.0593935854477563),
 .UNSPECIFIED.)
CURVE()
GEOMETRIC_REPRESENTATION_ITEM()
RATIONAL_B_SPLINE_CURVE((1.00078646015598,1.00061453665218,1.))
REPRESENTATION_ITEM('')
);
#890=(
BOUNDED_CURVE()
B_SPLINE_CURVE(2,(#59075,#59076,#59077),.UNSPECIFIED.,.F.,.F.)
B_SPLINE_CURVE_WITH_KNOTS((3,3),(0.,0.0213887827154904),.UNSPECIFIED.)
CURVE()
GEOMETRIC_REPRESENTATION_ITEM()
RATIONAL_B_SPLINE_CURVE((1.,1.00061453665374,1.00078646015798))
REPRESENTATION_ITEM('')
);
#891=(
BOUNDED_CURVE()
B_SPLINE_CURVE(2,(#59079,#59080,#59081),.UNSPECIFIED.,.F.,.F.)
B_SPLINE_CURVE_WITH_KNOTS((3,3),(0.0380048027322369,0.0593935854477557),
 .UNSPECIFIED.)
CURVE()
GEOMETRIC_REPRESENTATION_ITEM()
RATIONAL_B_SPLINE_CURVE((1.00078646015409,1.0006145366507,1.))
REPRESENTATION_ITEM('')
);
#892=(
BOUNDED_CURVE()
B_SPLINE_CURVE(2,(#59085,#59086,#59087),.UNSPECIFIED.,.F.,.F.)
B_SPLINE_CURVE_WITH_KNOTS((3,3),(0.,0.0213887827154539),.UNSPECIFIED.)
CURVE()
GEOMETRIC_REPRESENTATION_ITEM()
RATIONAL_B_SPLINE_CURVE((1.,1.00061453665704,1.0007864601622))
REPRESENTATION_ITEM('')
);
#893=(
BOUNDED_CURVE()
B_SPLINE_CURVE(2,(#59089,#59090,#59091),.UNSPECIFIED.,.F.,.F.)
B_SPLINE_CURVE_WITH_KNOTS((3,3),(0.0380048027323148,0.0593935854477558),
 .UNSPECIFIED.)
CURVE()
GEOMETRIC_REPRESENTATION_ITEM()
RATIONAL_B_SPLINE_CURVE((1.00078646015925,1.00061453665473,1.))
REPRESENTATION_ITEM('')
);
#894=(
BOUNDED_CURVE()
B_SPLINE_CURVE(2,(#59095,#59096,#59097),.UNSPECIFIED.,.F.,.F.)
B_SPLINE_CURVE_WITH_KNOTS((3,3),(0.,0.0213887827154462),.UNSPECIFIED.)
CURVE()
GEOMETRIC_REPRESENTATION_ITEM()
RATIONAL_B_SPLINE_CURVE((1.,1.00061453665421,1.00078646015858))
REPRESENTATION_ITEM('')
);
#895=(
BOUNDED_CURVE()
B_SPLINE_CURVE(2,(#59099,#59100,#59101),.UNSPECIFIED.,.F.,.F.)
B_SPLINE_CURVE_WITH_KNOTS((3,3),(0.038004802732261,0.0593935854477558),
 .UNSPECIFIED.)
CURVE()
GEOMETRIC_REPRESENTATION_ITEM()
RATIONAL_B_SPLINE_CURVE((1.0007864601574,1.00061453665329,1.))
REPRESENTATION_ITEM('')
);
#896=(
BOUNDED_CURVE()
B_SPLINE_CURVE(2,(#59105,#59106,#59107),.UNSPECIFIED.,.F.,.F.)
B_SPLINE_CURVE_WITH_KNOTS((3,3),(0.,0.021388782715505),.UNSPECIFIED.)
CURVE()
GEOMETRIC_REPRESENTATION_ITEM()
RATIONAL_B_SPLINE_CURVE((1.,1.00061453665229,1.00078646015612))
REPRESENTATION_ITEM('')
);
#897=(
BOUNDED_CURVE()
B_SPLINE_CURVE(2,(#59109,#59110,#59111),.UNSPECIFIED.,.F.,.F.)
B_SPLINE_CURVE_WITH_KNOTS((3,3),(0.0380048027323058,0.0593935854477558),
 .UNSPECIFIED.)
CURVE()
GEOMETRIC_REPRESENTATION_ITEM()
RATIONAL_B_SPLINE_CURVE((1.00078646016102,1.00061453665611,1.))
REPRESENTATION_ITEM('')
);
#898=(
BOUNDED_CURVE()
B_SPLINE_CURVE(2,(#59116,#59117,#59118),.UNSPECIFIED.,.F.,.F.)
B_SPLINE_CURVE_WITH_KNOTS((3,3),(0.,0.0213887827154293),.UNSPECIFIED.)
CURVE()
GEOMETRIC_REPRESENTATION_ITEM()
RATIONAL_B_SPLINE_CURVE((1.,1.00061453665639,1.00078646016138))
REPRESENTATION_ITEM('')
);
#899=(
BOUNDED_CURVE()
B_SPLINE_CURVE(2,(#59120,#59121,#59122),.UNSPECIFIED.,.F.,.F.)
B_SPLINE_CURVE_WITH_KNOTS((3,3),(0.0380048027323149,0.0593935854477581),
 .UNSPECIFIED.)
CURVE()
GEOMETRIC_REPRESENTATION_ITEM()
RATIONAL_B_SPLINE_CURVE((1.00078646016138,1.0006145366564,1.))
REPRESENTATION_ITEM('')
);
#900=(
BOUNDED_CURVE()
B_SPLINE_CURVE(2,(#59126,#59127,#59128),.UNSPECIFIED.,.F.,.F.)
B_SPLINE_CURVE_WITH_KNOTS((3,3),(0.,0.0213887827154979),.UNSPECIFIED.)
CURVE()
GEOMETRIC_REPRESENTATION_ITEM()
RATIONAL_B_SPLINE_CURVE((1.,1.00061453665225,1.00078646015608))
REPRESENTATION_ITEM('')
);
#901=(
BOUNDED_CURVE()
B_SPLINE_CURVE(2,(#59130,#59131,#59132),.UNSPECIFIED.,.F.,.F.)
B_SPLINE_CURVE_WITH_KNOTS((3,3),(0.0380048027322422,0.059393585447758),
 .UNSPECIFIED.)
CURVE()
GEOMETRIC_REPRESENTATION_ITEM()
RATIONAL_B_SPLINE_CURVE((1.00078646015494,1.00061453665137,1.))
REPRESENTATION_ITEM('')
);
#902=(
BOUNDED_CURVE()
B_SPLINE_CURVE(2,(#59136,#59137,#59138),.UNSPECIFIED.,.F.,.F.)
B_SPLINE_CURVE_WITH_KNOTS((3,3),(0.,0.0213887827154959),.UNSPECIFIED.)
CURVE()
GEOMETRIC_REPRESENTATION_ITEM()
RATIONAL_B_SPLINE_CURVE((1.,1.00061453665238,1.00078646015624))
REPRESENTATION_ITEM('')
);
#903=(
BOUNDED_CURVE()
B_SPLINE_CURVE(2,(#59140,#59141,#59142),.UNSPECIFIED.,.F.,.F.)
B_SPLINE_CURVE_WITH_KNOTS((3,3),(0.0380048027323219,0.0593935854477577),
 .UNSPECIFIED.)
CURVE()
GEOMETRIC_REPRESENTATION_ITEM()
RATIONAL_B_SPLINE_CURVE((1.00078646016013,1.00061453665542,1.))
REPRESENTATION_ITEM('')
);
#904=(
BOUNDED_CURVE()
B_SPLINE_CURVE(2,(#59146,#59147,#59148),.UNSPECIFIED.,.F.,.F.)
B_SPLINE_CURVE_WITH_KNOTS((3,3),(0.,0.021388782715533),.UNSPECIFIED.)
CURVE()
GEOMETRIC_REPRESENTATION_ITEM()
RATIONAL_B_SPLINE_CURVE((1.,1.00061453664963,1.00078646015272))
REPRESENTATION_ITEM('')
);
#905=(
BOUNDED_CURVE()
B_SPLINE_CURVE(2,(#59150,#59151,#59152),.UNSPECIFIED.,.F.,.F.)
B_SPLINE_CURVE_WITH_KNOTS((3,3),(0.0380048027324089,0.0593935854477567),
 .UNSPECIFIED.)
CURVE()
GEOMETRIC_REPRESENTATION_ITEM()
RATIONAL_B_SPLINE_CURVE((1.00078646016585,1.00061453665989,1.))
REPRESENTATION_ITEM('')
);
#906=(
BOUNDED_CURVE()
B_SPLINE_CURVE(2,(#59156,#59157,#59158),.UNSPECIFIED.,.F.,.F.)
B_SPLINE_CURVE_WITH_KNOTS((3,3),(0.,0.0213887827154936),.UNSPECIFIED.)
CURVE()
GEOMETRIC_REPRESENTATION_ITEM()
RATIONAL_B_SPLINE_CURVE((1.,1.00061453665172,1.00078646015539))
REPRESENTATION_ITEM('')
);
#907=(
BOUNDED_CURVE()
B_SPLINE_CURVE(2,(#59160,#59161,#59162),.UNSPECIFIED.,.F.,.F.)
B_SPLINE_CURVE_WITH_KNOTS((3,3),(0.038004802732325,0.0593935854477579),
 .UNSPECIFIED.)
CURVE()
GEOMETRIC_REPRESENTATION_ITEM()
RATIONAL_B_SPLINE_CURVE((1.00078646016394,1.0006145366584,1.))
REPRESENTATION_ITEM('')
);
#908=(
BOUNDED_CURVE()
B_SPLINE_CURVE(2,(#59166,#59167,#59168),.UNSPECIFIED.,.F.,.F.)
B_SPLINE_CURVE_WITH_KNOTS((3,3),(0.,0.0213887827154531),.UNSPECIFIED.)
CURVE()
GEOMETRIC_REPRESENTATION_ITEM()
RATIONAL_B_SPLINE_CURVE((1.,1.00061453665483,1.00078646015938))
REPRESENTATION_ITEM('')
);
#909=(
BOUNDED_CURVE()
B_SPLINE_CURVE(2,(#59170,#59171,#59172),.UNSPECIFIED.,.F.,.F.)
B_SPLINE_CURVE_WITH_KNOTS((3,3),(0.03800480273219,0.0593935854477586),
 .UNSPECIFIED.)
CURVE()
GEOMETRIC_REPRESENTATION_ITEM()
RATIONAL_B_SPLINE_CURVE((1.00078646015297,1.00061453664982,1.))
REPRESENTATION_ITEM('')
);
#910=(
BOUNDED_CURVE()
B_SPLINE_CURVE(2,(#59176,#59177,#59178),.UNSPECIFIED.,.F.,.F.)
B_SPLINE_CURVE_WITH_KNOTS((3,3),(0.,0.0213887827154683),.UNSPECIFIED.)
CURVE()
GEOMETRIC_REPRESENTATION_ITEM()
RATIONAL_B_SPLINE_CURVE((1.,1.00061453665169,1.00078646015536))
REPRESENTATION_ITEM('')
);
#911=(
BOUNDED_CURVE()
B_SPLINE_CURVE(2,(#59180,#59181,#59182),.UNSPECIFIED.,.F.,.F.)
B_SPLINE_CURVE_WITH_KNOTS((3,3),(0.0380048027322755,0.0593935854477574),
 .UNSPECIFIED.)
CURVE()
GEOMETRIC_REPRESENTATION_ITEM()
RATIONAL_B_SPLINE_CURVE((1.00078646016181,1.00061453665673,1.))
REPRESENTATION_ITEM('')
);
#912=(
BOUNDED_CURVE()
B_SPLINE_CURVE(2,(#59186,#59187,#59188),.UNSPECIFIED.,.F.,.F.)
B_SPLINE_CURVE_WITH_KNOTS((3,3),(0.,0.0213887827154684),.UNSPECIFIED.)
CURVE()
GEOMETRIC_REPRESENTATION_ITEM()
RATIONAL_B_SPLINE_CURVE((1.,1.0006145366546,1.00078646015908))
REPRESENTATION_ITEM('')
);
#913=(
BOUNDED_CURVE()
B_SPLINE_CURVE(2,(#59190,#59191,#59192),.UNSPECIFIED.,.F.,.F.)
B_SPLINE_CURVE_WITH_KNOTS((3,3),(0.0380048027323105,0.0593935854477581),
 .UNSPECIFIED.)
CURVE()
GEOMETRIC_REPRESENTATION_ITEM()
RATIONAL_B_SPLINE_CURVE((1.00078646015979,1.00061453665516,1.))
REPRESENTATION_ITEM('')
);
#914=(
BOUNDED_CURVE()
B_SPLINE_CURVE(2,(#59196,#59197,#59198),.UNSPECIFIED.,.F.,.F.)
B_SPLINE_CURVE_WITH_KNOTS((3,3),(0.,0.0213887827154438),.UNSPECIFIED.)
CURVE()
GEOMETRIC_REPRESENTATION_ITEM()
RATIONAL_B_SPLINE_CURVE((1.,1.00061453665793,1.00078646016334))
REPRESENTATION_ITEM('')
);
#915=(
BOUNDED_CURVE()
B_SPLINE_CURVE(2,(#59200,#59201,#59202),.UNSPECIFIED.,.F.,.F.)
B_SPLINE_CURVE_WITH_KNOTS((3,3),(0.0380048027322779,0.0593935854477573),
 .UNSPECIFIED.)
CURVE()
GEOMETRIC_REPRESENTATION_ITEM()
RATIONAL_B_SPLINE_CURVE((1.00078646015484,1.00061453665129,1.))
REPRESENTATION_ITEM('')
);
#916=(
BOUNDED_CURVE()
B_SPLINE_CURVE(2,(#59206,#59207,#59208),.UNSPECIFIED.,.F.,.F.)
B_SPLINE_CURVE_WITH_KNOTS((3,3),(0.,0.0213887827154012),.UNSPECIFIED.)
CURVE()
GEOMETRIC_REPRESENTATION_ITEM()
RATIONAL_B_SPLINE_CURVE((1.,1.00061453665908,1.00078646016482))
REPRESENTATION_ITEM('')
);
#917=(
BOUNDED_CURVE()
B_SPLINE_CURVE(2,(#59210,#59211,#59212),.UNSPECIFIED.,.F.,.F.)
B_SPLINE_CURVE_WITH_KNOTS((3,3),(0.0380048027322933,0.0593935854477573),
 .UNSPECIFIED.)
CURVE()
GEOMETRIC_REPRESENTATION_ITEM()
RATIONAL_B_SPLINE_CURVE((1.00078646015827,1.00061453665397,1.))
REPRESENTATION_ITEM('')
);
#918=(
BOUNDED_CURVE()
B_SPLINE_CURVE(2,(#59216,#59217,#59218),.UNSPECIFIED.,.F.,.F.)
B_SPLINE_CURVE_WITH_KNOTS((3,3),(0.,0.0213887827154559),.UNSPECIFIED.)
CURVE()
GEOMETRIC_REPRESENTATION_ITEM()
RATIONAL_B_SPLINE_CURVE((1.,1.00061453665602,1.0007864601609))
REPRESENTATION_ITEM('')
);
#919=(
BOUNDED_CURVE()
B_SPLINE_CURVE(2,(#59220,#59221,#59222),.UNSPECIFIED.,.F.,.F.)
B_SPLINE_CURVE_WITH_KNOTS((3,3),(0.038004802732396,0.0593935854477571),
 .UNSPECIFIED.)
CURVE()
GEOMETRIC_REPRESENTATION_ITEM()
RATIONAL_B_SPLINE_CURVE((1.00078646016815,1.00061453666168,1.))
REPRESENTATION_ITEM('')
);
#920=(
BOUNDED_CURVE()
B_SPLINE_CURVE(2,(#59226,#59227,#59228),.UNSPECIFIED.,.F.,.F.)
B_SPLINE_CURVE_WITH_KNOTS((3,3),(0.,0.0213887827154657),.UNSPECIFIED.)
CURVE()
GEOMETRIC_REPRESENTATION_ITEM()
RATIONAL_B_SPLINE_CURVE((1.,1.00061453665296,1.00078646015698))
REPRESENTATION_ITEM('')
);
#921=(
BOUNDED_CURVE()
B_SPLINE_CURVE(2,(#59230,#59231,#59232),.UNSPECIFIED.,.F.,.F.)
B_SPLINE_CURVE_WITH_KNOTS((3,3),(0.0380048027322985,0.059393585447757),
 .UNSPECIFIED.)
CURVE()
GEOMETRIC_REPRESENTATION_ITEM()
RATIONAL_B_SPLINE_CURVE((1.00078646016081,1.00061453665595,1.))
REPRESENTATION_ITEM('')
);
#922=(
BOUNDED_CURVE()
B_SPLINE_CURVE(2,(#59236,#59237,#59238),.UNSPECIFIED.,.F.,.F.)
B_SPLINE_CURVE_WITH_KNOTS((3,3),(0.,0.0213887827154679),.UNSPECIFIED.)
CURVE()
GEOMETRIC_REPRESENTATION_ITEM()
RATIONAL_B_SPLINE_CURVE((1.,1.00061453665517,1.00078646015981))
REPRESENTATION_ITEM('')
);
#923=(
BOUNDED_CURVE()
B_SPLINE_CURVE(2,(#59240,#59241,#59242),.UNSPECIFIED.,.F.,.F.)
B_SPLINE_CURVE_WITH_KNOTS((3,3),(0.0380048027322456,0.0593935854477571),
 .UNSPECIFIED.)
CURVE()
GEOMETRIC_REPRESENTATION_ITEM()
RATIONAL_B_SPLINE_CURVE((1.00078646015223,1.00061453664925,1.))
REPRESENTATION_ITEM('')
);
#924=(
BOUNDED_CURVE()
B_SPLINE_CURVE(2,(#59246,#59247,#59248),.UNSPECIFIED.,.F.,.F.)
B_SPLINE_CURVE_WITH_KNOTS((3,3),(0.,0.0213887827154763),.UNSPECIFIED.)
CURVE()
GEOMETRIC_REPRESENTATION_ITEM()
RATIONAL_B_SPLINE_CURVE((1.,1.00061453665236,1.00078646015621))
REPRESENTATION_ITEM('')
);
#925=(
BOUNDED_CURVE()
B_SPLINE_CURVE(2,(#59250,#59251,#59252),.UNSPECIFIED.,.F.,.F.)
B_SPLINE_CURVE_WITH_KNOTS((3,3),(0.0380048027323043,0.0593935854477561),
 .UNSPECIFIED.)
CURVE()
GEOMETRIC_REPRESENTATION_ITEM()
RATIONAL_B_SPLINE_CURVE((1.00078646015985,1.0006145366552,1.))
REPRESENTATION_ITEM('')
);
#926=(
BOUNDED_CURVE()
B_SPLINE_CURVE(2,(#59256,#59257,#59258),.UNSPECIFIED.,.F.,.F.)
B_SPLINE_CURVE_WITH_KNOTS((3,3),(0.,0.0213887827154303),.UNSPECIFIED.)
CURVE()
GEOMETRIC_REPRESENTATION_ITEM()
RATIONAL_B_SPLINE_CURVE((1.,1.00061453665563,1.0007864601604))
REPRESENTATION_ITEM('')
);
#927=(
BOUNDED_CURVE()
B_SPLINE_CURVE(2,(#59260,#59261,#59262),.UNSPECIFIED.,.F.,.F.)
B_SPLINE_CURVE_WITH_KNOTS((3,3),(0.0380048027323154,0.0593935854477565),
 .UNSPECIFIED.)
CURVE()
GEOMETRIC_REPRESENTATION_ITEM()
RATIONAL_B_SPLINE_CURVE((1.00078646015761,1.00061453665345,1.))
REPRESENTATION_ITEM('')
);
#928=(
BOUNDED_CURVE()
B_SPLINE_CURVE(2,(#59266,#59267,#59268),.UNSPECIFIED.,.F.,.F.)
B_SPLINE_CURVE_WITH_KNOTS((3,3),(0.,0.0213887827154477),.UNSPECIFIED.)
CURVE()
GEOMETRIC_REPRESENTATION_ITEM()
RATIONAL_B_SPLINE_CURVE((1.,1.00061453665389,1.00078646015818))
REPRESENTATION_ITEM('')
);
#929=(
BOUNDED_CURVE()
B_SPLINE_CURVE(2,(#59270,#59271,#59272),.UNSPECIFIED.,.F.,.F.)
B_SPLINE_CURVE_WITH_KNOTS((3,3),(0.0380048027322823,0.0593935854477568),
 .UNSPECIFIED.)
CURVE()
GEOMETRIC_REPRESENTATION_ITEM()
RATIONAL_B_SPLINE_CURVE((1.00078646015752,1.00061453665338,1.))
REPRESENTATION_ITEM('')
);
#930=(
BOUNDED_CURVE()
B_SPLINE_CURVE(2,(#59275,#59276,#59277),.UNSPECIFIED.,.F.,.F.)
B_SPLINE_CURVE_WITH_KNOTS((3,3),(0.,0.0213887827154623),.UNSPECIFIED.)
CURVE()
GEOMETRIC_REPRESENTATION_ITEM()
RATIONAL_B_SPLINE_CURVE((1.,1.00061453665359,1.00078646015779))
REPRESENTATION_ITEM('')
);
#931=(
BOUNDED_CURVE()
B_SPLINE_CURVE(2,(#70734,#70735,#70736),.UNSPECIFIED.,.F.,.F.)
B_SPLINE_CURVE_WITH_KNOTS((3,3),(0.,0.0215367144649105),.UNSPECIFIED.)
CURVE()
GEOMETRIC_REPRESENTATION_ITEM()
RATIONAL_B_SPLINE_CURVE((1.,1.00042008979832,1.00053542481542))
REPRESENTATION_ITEM('')
);
#932=(
BOUNDED_CURVE()
B_SPLINE_CURVE(2,(#70741,#70742,#70743),.UNSPECIFIED.,.F.,.F.)
B_SPLINE_CURVE_WITH_KNOTS((3,3),(0.0378379342266191,0.0593746486914489),
 .UNSPECIFIED.)
CURVE()
GEOMETRIC_REPRESENTATION_ITEM()
RATIONAL_B_SPLINE_CURVE((1.00053542482002,1.00042008980193,1.))
REPRESENTATION_ITEM('')
);
#933=(
BOUNDED_CURVE()
B_SPLINE_CURVE(2,(#70750,#70751,#70752),.UNSPECIFIED.,.F.,.F.)
B_SPLINE_CURVE_WITH_KNOTS((3,3),(0.0378379342265495,0.0593746486914482),
 .UNSPECIFIED.)
CURVE()
GEOMETRIC_REPRESENTATION_ITEM()
RATIONAL_B_SPLINE_CURVE((1.00053542481289,1.00042008979634,1.))
REPRESENTATION_ITEM('')
);
#934=(
BOUNDED_CURVE()
B_SPLINE_CURVE(2,(#70756,#70757,#70758),.UNSPECIFIED.,.F.,.F.)
B_SPLINE_CURVE_WITH_KNOTS((3,3),(0.,0.0215367144649402),.UNSPECIFIED.)
CURVE()
GEOMETRIC_REPRESENTATION_ITEM()
RATIONAL_B_SPLINE_CURVE((1.,1.00042008979471,1.00053542481081))
REPRESENTATION_ITEM('')
);
#935=(
BOUNDED_CURVE()
B_SPLINE_CURVE(2,(#70760,#70761,#70762),.UNSPECIFIED.,.F.,.F.)
B_SPLINE_CURVE_WITH_KNOTS((3,3),(0.0378379342265241,0.0593746486914486),
 .UNSPECIFIED.)
CURVE()
GEOMETRIC_REPRESENTATION_ITEM()
RATIONAL_B_SPLINE_CURVE((1.00053542481258,1.0004200897961,1.))
REPRESENTATION_ITEM('')
);
#936=(
BOUNDED_CURVE()
B_SPLINE_CURVE(2,(#70766,#70767,#70768),.UNSPECIFIED.,.F.,.F.)
B_SPLINE_CURVE_WITH_KNOTS((3,3),(0.,0.0215367144649098),.UNSPECIFIED.)
CURVE()
GEOMETRIC_REPRESENTATION_ITEM()
RATIONAL_B_SPLINE_CURVE((1.,1.00042008979542,1.00053542481172))
REPRESENTATION_ITEM('')
);
#937=(
BOUNDED_CURVE()
B_SPLINE_CURVE(2,(#70770,#70771,#70772),.UNSPECIFIED.,.F.,.F.)
B_SPLINE_CURVE_WITH_KNOTS((3,3),(0.0378379342265049,0.0593746486914484),
 .UNSPECIFIED.)
CURVE()
GEOMETRIC_REPRESENTATION_ITEM()
RATIONAL_B_SPLINE_CURVE((1.00053542481297,1.0004200897964,1.))
REPRESENTATION_ITEM('')
);
#938=(
BOUNDED_CURVE()
B_SPLINE_CURVE(2,(#70776,#70777,#70778),.UNSPECIFIED.,.F.,.F.)
B_SPLINE_CURVE_WITH_KNOTS((3,3),(0.,0.0215367144648988),.UNSPECIFIED.)
CURVE()
GEOMETRIC_REPRESENTATION_ITEM()
RATIONAL_B_SPLINE_CURVE((1.,1.00042008979632,1.00053542481287))
REPRESENTATION_ITEM('')
);
#939=(
BOUNDED_CURVE()
B_SPLINE_CURVE(2,(#70780,#70781,#70782),.UNSPECIFIED.,.F.,.F.)
B_SPLINE_CURVE_WITH_KNOTS((3,3),(0.0378379342265885,0.0593746486914481),
 .UNSPECIFIED.)
CURVE()
GEOMETRIC_REPRESENTATION_ITEM()
RATIONAL_B_SPLINE_CURVE((1.00053542481452,1.00042008979762,1.))
REPRESENTATION_ITEM('')
);
#940=(
BOUNDED_CURVE()
B_SPLINE_CURVE(2,(#70786,#70787,#70788),.UNSPECIFIED.,.F.,.F.)
B_SPLINE_CURVE_WITH_KNOTS((3,3),(0.,0.021536714464922),.UNSPECIFIED.)
CURVE()
GEOMETRIC_REPRESENTATION_ITEM()
RATIONAL_B_SPLINE_CURVE((1.,1.0004200897977,1.00053542481463))
REPRESENTATION_ITEM('')
);
#941=(
BOUNDED_CURVE()
B_SPLINE_CURVE(2,(#70790,#70791,#70792),.UNSPECIFIED.,.F.,.F.)
B_SPLINE_CURVE_WITH_KNOTS((3,3),(0.0378379342265092,0.0593746486914482),
 .UNSPECIFIED.)
CURVE()
GEOMETRIC_REPRESENTATION_ITEM()
RATIONAL_B_SPLINE_CURVE((1.00053542481205,1.00042008979567,1.))
REPRESENTATION_ITEM('')
);
#942=(
BOUNDED_CURVE()
B_SPLINE_CURVE(2,(#70796,#70797,#70798),.UNSPECIFIED.,.F.,.F.)
B_SPLINE_CURVE_WITH_KNOTS((3,3),(0.,0.0215367144648869),.UNSPECIFIED.)
CURVE()
GEOMETRIC_REPRESENTATION_ITEM()
RATIONAL_B_SPLINE_CURVE((1.,1.00042008979756,1.00053542481445))
REPRESENTATION_ITEM('')
);
#943=(
BOUNDED_CURVE()
B_SPLINE_CURVE(2,(#70800,#70801,#70802),.UNSPECIFIED.,.F.,.F.)
B_SPLINE_CURVE_WITH_KNOTS((3,3),(0.0378379342265307,0.0593746486914478),
 .UNSPECIFIED.)
CURVE()
GEOMETRIC_REPRESENTATION_ITEM()
RATIONAL_B_SPLINE_CURVE((1.00053542481432,1.00042008979746,1.))
REPRESENTATION_ITEM('')
);
#944=(
BOUNDED_CURVE()
B_SPLINE_CURVE(2,(#70806,#70807,#70808),.UNSPECIFIED.,.F.,.F.)
B_SPLINE_CURVE_WITH_KNOTS((3,3),(0.,0.0215367144649457),.UNSPECIFIED.)
CURVE()
GEOMETRIC_REPRESENTATION_ITEM()
RATIONAL_B_SPLINE_CURVE((1.,1.00042008979626,1.00053542481279))
REPRESENTATION_ITEM('')
);
#945=(
BOUNDED_CURVE()
B_SPLINE_CURVE(2,(#70810,#70811,#70812),.UNSPECIFIED.,.F.,.F.)
B_SPLINE_CURVE_WITH_KNOTS((3,3),(0.0378379342264978,0.0593746486914476),
 .UNSPECIFIED.)
CURVE()
GEOMETRIC_REPRESENTATION_ITEM()
RATIONAL_B_SPLINE_CURVE((1.00053542480725,1.00042008979192,1.))
REPRESENTATION_ITEM('')
);
#946=(
BOUNDED_CURVE()
B_SPLINE_CURVE(2,(#70816,#70817,#70818),.UNSPECIFIED.,.F.,.F.)
B_SPLINE_CURVE_WITH_KNOTS((3,3),(0.,0.0215367144648818),.UNSPECIFIED.)
CURVE()
GEOMETRIC_REPRESENTATION_ITEM()
RATIONAL_B_SPLINE_CURVE((1.,1.00042008979656,1.00053542481317))
REPRESENTATION_ITEM('')
);
#947=(
BOUNDED_CURVE()
B_SPLINE_CURVE(2,(#70820,#70821,#70822),.UNSPECIFIED.,.F.,.F.)
B_SPLINE_CURVE_WITH_KNOTS((3,3),(0.0378379342265614,0.0593746486914475),
 .UNSPECIFIED.)
CURVE()
GEOMETRIC_REPRESENTATION_ITEM()
RATIONAL_B_SPLINE_CURVE((1.00053542481625,1.00042008979897,1.))
REPRESENTATION_ITEM('')
);
#948=(
BOUNDED_CURVE()
B_SPLINE_CURVE(2,(#70826,#70827,#70828),.UNSPECIFIED.,.F.,.F.)
B_SPLINE_CURVE_WITH_KNOTS((3,3),(0.,0.0215367144648944),.UNSPECIFIED.)
CURVE()
GEOMETRIC_REPRESENTATION_ITEM()
RATIONAL_B_SPLINE_CURVE((1.,1.00042008979746,1.00053542481432))
REPRESENTATION_ITEM('')
);
#949=(
BOUNDED_CURVE()
B_SPLINE_CURVE(2,(#70830,#70831,#70832),.UNSPECIFIED.,.F.,.F.)
B_SPLINE_CURVE_WITH_KNOTS((3,3),(0.0378379342265643,0.0593746486914474),
 .UNSPECIFIED.)
CURVE()
GEOMETRIC_REPRESENTATION_ITEM()
RATIONAL_B_SPLINE_CURVE((1.00053542481547,1.00042008979836,1.))
REPRESENTATION_ITEM('')
);
#950=(
BOUNDED_CURVE()
B_SPLINE_CURVE(2,(#70836,#70837,#70838),.UNSPECIFIED.,.F.,.F.)
B_SPLINE_CURVE_WITH_KNOTS((3,3),(0.,0.0215367144648979),.UNSPECIFIED.)
CURVE()
GEOMETRIC_REPRESENTATION_ITEM()
RATIONAL_B_SPLINE_CURVE((1.,1.00042008979658,1.00053542481321))
REPRESENTATION_ITEM('')
);
#951=(
BOUNDED_CURVE()
B_SPLINE_CURVE(2,(#70840,#70841,#70842),.UNSPECIFIED.,.F.,.F.)
B_SPLINE_CURVE_WITH_KNOTS((3,3),(0.037837934226498,0.0593746486914474),
 .UNSPECIFIED.)
CURVE()
GEOMETRIC_REPRESENTATION_ITEM()
RATIONAL_B_SPLINE_CURVE((1.00053542481105,1.0004200897949,1.))
REPRESENTATION_ITEM('')
);
#952=(
BOUNDED_CURVE()
B_SPLINE_CURVE(2,(#70846,#70847,#70848),.UNSPECIFIED.,.F.,.F.)
B_SPLINE_CURVE_WITH_KNOTS((3,3),(0.,0.021536714464896),.UNSPECIFIED.)
CURVE()
GEOMETRIC_REPRESENTATION_ITEM()
RATIONAL_B_SPLINE_CURVE((1.,1.00042008979607,1.00053542481255))
REPRESENTATION_ITEM('')
);
#953=(
BOUNDED_CURVE()
B_SPLINE_CURVE(2,(#70850,#70851,#70852),.UNSPECIFIED.,.F.,.F.)
B_SPLINE_CURVE_WITH_KNOTS((3,3),(0.0378379342264847,0.0593746486914478),
 .UNSPECIFIED.)
CURVE()
GEOMETRIC_REPRESENTATION_ITEM()
RATIONAL_B_SPLINE_CURVE((1.00053542480987,1.00042008979397,1.))
REPRESENTATION_ITEM('')
);
#954=(
BOUNDED_CURVE()
B_SPLINE_CURVE(2,(#70856,#70857,#70858),.UNSPECIFIED.,.F.,.F.)
B_SPLINE_CURVE_WITH_KNOTS((3,3),(0.,0.0215367144649515),.UNSPECIFIED.)
CURVE()
GEOMETRIC_REPRESENTATION_ITEM()
RATIONAL_B_SPLINE_CURVE((1.,1.00042008979379,1.00053542480965))
REPRESENTATION_ITEM('')
);
#955=(
BOUNDED_CURVE()
B_SPLINE_CURVE(2,(#70860,#70861,#70862),.UNSPECIFIED.,.F.,.F.)
B_SPLINE_CURVE_WITH_KNOTS((3,3),(0.0378379342265934,0.0593746486914471),
 .UNSPECIFIED.)
CURVE()
GEOMETRIC_REPRESENTATION_ITEM()
RATIONAL_B_SPLINE_CURVE((1.00053542481303,1.00042008979644,1.))
REPRESENTATION_ITEM('')
);
#956=(
BOUNDED_CURVE()
B_SPLINE_CURVE(2,(#70866,#70867,#70868),.UNSPECIFIED.,.F.,.F.)
B_SPLINE_CURVE_WITH_KNOTS((3,3),(0.,0.0215367144649196),.UNSPECIFIED.)
CURVE()
GEOMETRIC_REPRESENTATION_ITEM()
RATIONAL_B_SPLINE_CURVE((1.,1.00042008979619,1.00053542481271))
REPRESENTATION_ITEM('')
);
#957=(
BOUNDED_CURVE()
B_SPLINE_CURVE(2,(#70870,#70871,#70872),.UNSPECIFIED.,.F.,.F.)
B_SPLINE_CURVE_WITH_KNOTS((3,3),(0.0378379342265594,0.0593746486914476),
 .UNSPECIFIED.)
CURVE()
GEOMETRIC_REPRESENTATION_ITEM()
RATIONAL_B_SPLINE_CURVE((1.00053542481439,1.00042008979752,1.))
REPRESENTATION_ITEM('')
);
#958=(
BOUNDED_CURVE()
B_SPLINE_CURVE(2,(#70876,#70877,#70878),.UNSPECIFIED.,.F.,.F.)
B_SPLINE_CURVE_WITH_KNOTS((3,3),(0.,0.0215367144649124),.UNSPECIFIED.)
CURVE()
GEOMETRIC_REPRESENTATION_ITEM()
RATIONAL_B_SPLINE_CURVE((1.,1.00042008979906,1.00053542481637))
REPRESENTATION_ITEM('')
);
#959=(
BOUNDED_CURVE()
B_SPLINE_CURVE(2,(#70880,#70881,#70882),.UNSPECIFIED.,.F.,.F.)
B_SPLINE_CURVE_WITH_KNOTS((3,3),(0.0378379342265818,0.0593746486914467),
 .UNSPECIFIED.)
CURVE()
GEOMETRIC_REPRESENTATION_ITEM()
RATIONAL_B_SPLINE_CURVE((1.00053542480684,1.00042008979159,1.))
REPRESENTATION_ITEM('')
);
#960=(
BOUNDED_CURVE()
B_SPLINE_CURVE(2,(#70886,#70887,#70888),.UNSPECIFIED.,.F.,.F.)
B_SPLINE_CURVE_WITH_KNOTS((3,3),(0.,0.021536714464952),.UNSPECIFIED.)
CURVE()
GEOMETRIC_REPRESENTATION_ITEM()
RATIONAL_B_SPLINE_CURVE((1.,1.00042008979707,1.00053542481383))
REPRESENTATION_ITEM('')
);
#961=(
BOUNDED_CURVE()
B_SPLINE_CURVE(2,(#70890,#70891,#70892),.UNSPECIFIED.,.F.,.F.)
B_SPLINE_CURVE_WITH_KNOTS((3,3),(0.0378379342265293,0.0593746486914474),
 .UNSPECIFIED.)
CURVE()
GEOMETRIC_REPRESENTATION_ITEM()
RATIONAL_B_SPLINE_CURVE((1.00053542480889,1.0004200897932,1.))
REPRESENTATION_ITEM('')
);
#962=(
BOUNDED_CURVE()
B_SPLINE_CURVE(2,(#70896,#70897,#70898),.UNSPECIFIED.,.F.,.F.)
B_SPLINE_CURVE_WITH_KNOTS((3,3),(0.,0.0215367144649713),.UNSPECIFIED.)
CURVE()
GEOMETRIC_REPRESENTATION_ITEM()
RATIONAL_B_SPLINE_CURVE((1.,1.00042008978867,1.00053542480312))
REPRESENTATION_ITEM('')
);
#963=(
BOUNDED_CURVE()
B_SPLINE_CURVE(2,(#70900,#70901,#70902),.UNSPECIFIED.,.F.,.F.)
B_SPLINE_CURVE_WITH_KNOTS((3,3),(0.0378379342265233,0.0593746486914479),
 .UNSPECIFIED.)
CURVE()
GEOMETRIC_REPRESENTATION_ITEM()
RATIONAL_B_SPLINE_CURVE((1.00053542481454,1.00042008979763,1.))
REPRESENTATION_ITEM('')
);
#964=(
BOUNDED_CURVE()
B_SPLINE_CURVE(2,(#70906,#70907,#70908),.UNSPECIFIED.,.F.,.F.)
B_SPLINE_CURVE_WITH_KNOTS((3,3),(0.,0.0215367144648066),.UNSPECIFIED.)
CURVE()
GEOMETRIC_REPRESENTATION_ITEM()
RATIONAL_B_SPLINE_CURVE((1.,1.00042008980092,1.00053542481873))
REPRESENTATION_ITEM('')
);
#965=(
BOUNDED_CURVE()
B_SPLINE_CURVE(2,(#70910,#70911,#70912),.UNSPECIFIED.,.F.,.F.)
B_SPLINE_CURVE_WITH_KNOTS((3,3),(0.0378379342265035,0.0593746486914475),
 .UNSPECIFIED.)
CURVE()
GEOMETRIC_REPRESENTATION_ITEM()
RATIONAL_B_SPLINE_CURVE((1.00053542481437,1.0004200897975,1.))
REPRESENTATION_ITEM('')
);
#966=(
BOUNDED_CURVE()
B_SPLINE_CURVE(2,(#70916,#70917,#70918),.UNSPECIFIED.,.F.,.F.)
B_SPLINE_CURVE_WITH_KNOTS((3,3),(0.,0.0215367144649832),.UNSPECIFIED.)
CURVE()
GEOMETRIC_REPRESENTATION_ITEM()
RATIONAL_B_SPLINE_CURVE((1.,1.00042008978849,1.00053542480288))
REPRESENTATION_ITEM('')
);
#967=(
BOUNDED_CURVE()
B_SPLINE_CURVE(2,(#70920,#70921,#70922),.UNSPECIFIED.,.F.,.F.)
B_SPLINE_CURVE_WITH_KNOTS((3,3),(0.0378379342264869,0.0593746486914472),
 .UNSPECIFIED.)
CURVE()
GEOMETRIC_REPRESENTATION_ITEM()
RATIONAL_B_SPLINE_CURVE((1.00053542480856,1.00042008979294,1.))
REPRESENTATION_ITEM('')
);
#968=(
BOUNDED_CURVE()
B_SPLINE_CURVE(2,(#70926,#70927,#70928),.UNSPECIFIED.,.F.,.F.)
B_SPLINE_CURVE_WITH_KNOTS((3,3),(0.,0.0215367144648701),.UNSPECIFIED.)
CURVE()
GEOMETRIC_REPRESENTATION_ITEM()
RATIONAL_B_SPLINE_CURVE((1.,1.00042008979633,1.00053542481289))
REPRESENTATION_ITEM('')
);
#969=(
BOUNDED_CURVE()
B_SPLINE_CURVE(2,(#70930,#70931,#70932),.UNSPECIFIED.,.F.,.F.)
B_SPLINE_CURVE_WITH_KNOTS((3,3),(0.0378379342266196,0.0593746486914466),
 .UNSPECIFIED.)
CURVE()
GEOMETRIC_REPRESENTATION_ITEM()
RATIONAL_B_SPLINE_CURVE((1.00053542481627,1.00042008979899,1.))
REPRESENTATION_ITEM('')
);
#970=(
BOUNDED_CURVE()
B_SPLINE_CURVE(2,(#70937,#70938,#70939),.UNSPECIFIED.,.F.,.F.)
B_SPLINE_CURVE_WITH_KNOTS((3,3),(0.,0.0215367144649364),.UNSPECIFIED.)
CURVE()
GEOMETRIC_REPRESENTATION_ITEM()
RATIONAL_B_SPLINE_CURVE((1.,1.00042008979495,1.00053542481112))
REPRESENTATION_ITEM('')
);
#971=(
BOUNDED_CURVE()
B_SPLINE_CURVE(2,(#70941,#70942,#70943),.UNSPECIFIED.,.F.,.F.)
B_SPLINE_CURVE_WITH_KNOTS((3,3),(0.0378379342265907,0.0593746486914489),
 .UNSPECIFIED.)
CURVE()
GEOMETRIC_REPRESENTATION_ITEM()
RATIONAL_B_SPLINE_CURVE((1.00053542481339,1.00042008979673,1.))
REPRESENTATION_ITEM('')
);
#972=(
BOUNDED_CURVE()
B_SPLINE_CURVE(2,(#70947,#70948,#70949),.UNSPECIFIED.,.F.,.F.)
B_SPLINE_CURVE_WITH_KNOTS((3,3),(0.,0.0215367144648983),.UNSPECIFIED.)
CURVE()
GEOMETRIC_REPRESENTATION_ITEM()
RATIONAL_B_SPLINE_CURVE((1.,1.00042008979758,1.00053542481447))
REPRESENTATION_ITEM('')
);
#973=(
BOUNDED_CURVE()
B_SPLINE_CURVE(2,(#70951,#70952,#70953),.UNSPECIFIED.,.F.,.F.)
B_SPLINE_CURVE_WITH_KNOTS((3,3),(0.0378379342266009,0.0593746486914487),
 .UNSPECIFIED.)
CURVE()
GEOMETRIC_REPRESENTATION_ITEM()
RATIONAL_B_SPLINE_CURVE((1.00053542481762,1.00042008980005,1.))
REPRESENTATION_ITEM('')
);
#974=(
BOUNDED_CURVE()
B_SPLINE_CURVE(2,(#70957,#70958,#70959),.UNSPECIFIED.,.F.,.F.)
B_SPLINE_CURVE_WITH_KNOTS((3,3),(0.,0.0215367144648523),.UNSPECIFIED.)
CURVE()
GEOMETRIC_REPRESENTATION_ITEM()
RATIONAL_B_SPLINE_CURVE((1.,1.00042008980162,1.00053542481963))
REPRESENTATION_ITEM('')
);
#975=(
BOUNDED_CURVE()
B_SPLINE_CURVE(2,(#70961,#70962,#70963),.UNSPECIFIED.,.F.,.F.)
B_SPLINE_CURVE_WITH_KNOTS((3,3),(0.0378379342266166,0.0593746486914488),
 .UNSPECIFIED.)
CURVE()
GEOMETRIC_REPRESENTATION_ITEM()
RATIONAL_B_SPLINE_CURVE((1.00053542482459,1.00042008980551,1.))
REPRESENTATION_ITEM('')
);
#976=(
BOUNDED_CURVE()
B_SPLINE_CURVE(2,(#70967,#70968,#70969),.UNSPECIFIED.,.F.,.F.)
B_SPLINE_CURVE_WITH_KNOTS((3,3),(0.,0.0215367144649508),.UNSPECIFIED.)
CURVE()
GEOMETRIC_REPRESENTATION_ITEM()
RATIONAL_B_SPLINE_CURVE((1.,1.00042008979412,1.00053542481006))
REPRESENTATION_ITEM('')
);
#977=(
BOUNDED_CURVE()
B_SPLINE_CURVE(2,(#70971,#70972,#70973),.UNSPECIFIED.,.F.,.F.)
B_SPLINE_CURVE_WITH_KNOTS((3,3),(0.0378379342265848,0.0593746486914484),
 .UNSPECIFIED.)
CURVE()
GEOMETRIC_REPRESENTATION_ITEM()
RATIONAL_B_SPLINE_CURVE((1.00053542481552,1.0004200897984,1.))
REPRESENTATION_ITEM('')
);
#978=(
BOUNDED_CURVE()
B_SPLINE_CURVE(2,(#70977,#70978,#70979),.UNSPECIFIED.,.F.,.F.)
B_SPLINE_CURVE_WITH_KNOTS((3,3),(0.,0.0215367144649591),.UNSPECIFIED.)
CURVE()
GEOMETRIC_REPRESENTATION_ITEM()
RATIONAL_B_SPLINE_CURVE((1.,1.00042008979621,1.00053542481272))
REPRESENTATION_ITEM('')
);
#979=(
BOUNDED_CURVE()
B_SPLINE_CURVE(2,(#70981,#70982,#70983),.UNSPECIFIED.,.F.,.F.)
B_SPLINE_CURVE_WITH_KNOTS((3,3),(0.037837934226528,0.0593746486914486),
 .UNSPECIFIED.)
CURVE()
GEOMETRIC_REPRESENTATION_ITEM()
RATIONAL_B_SPLINE_CURVE((1.00053542481249,1.00042008979602,1.))
REPRESENTATION_ITEM('')
);
#980=(
BOUNDED_CURVE()
B_SPLINE_CURVE(2,(#70987,#70988,#70989),.UNSPECIFIED.,.F.,.F.)
B_SPLINE_CURVE_WITH_KNOTS((3,3),(0.,0.0215367144649439),.UNSPECIFIED.)
CURVE()
GEOMETRIC_REPRESENTATION_ITEM()
RATIONAL_B_SPLINE_CURVE((1.,1.00042008979311,1.00053542480878))
REPRESENTATION_ITEM('')
);
#981=(
BOUNDED_CURVE()
B_SPLINE_CURVE(2,(#70991,#70992,#70993),.UNSPECIFIED.,.F.,.F.)
B_SPLINE_CURVE_WITH_KNOTS((3,3),(0.0378379342265471,0.0593746486914486),
 .UNSPECIFIED.)
CURVE()
GEOMETRIC_REPRESENTATION_ITEM()
RATIONAL_B_SPLINE_CURVE((1.00053542480963,1.00042008979378,1.))
REPRESENTATION_ITEM('')
);
#982=(
BOUNDED_CURVE()
B_SPLINE_CURVE(2,(#70997,#70998,#70999),.UNSPECIFIED.,.F.,.F.)
B_SPLINE_CURVE_WITH_KNOTS((3,3),(0.,0.0215367144649546),.UNSPECIFIED.)
CURVE()
GEOMETRIC_REPRESENTATION_ITEM()
RATIONAL_B_SPLINE_CURVE((1.,1.00042008979267,1.00053542480822))
REPRESENTATION_ITEM('')
);
#983=(
BOUNDED_CURVE()
B_SPLINE_CURVE(2,(#71001,#71002,#71003),.UNSPECIFIED.,.F.,.F.)
B_SPLINE_CURVE_WITH_KNOTS((3,3),(0.0378379342265707,0.0593746486914487),
 .UNSPECIFIED.)
CURVE()
GEOMETRIC_REPRESENTATION_ITEM()
RATIONAL_B_SPLINE_CURVE((1.0005354248134,1.00042008979673,1.))
REPRESENTATION_ITEM('')
);
#984=(
BOUNDED_CURVE()
B_SPLINE_CURVE(2,(#71007,#71008,#71009),.UNSPECIFIED.,.F.,.F.)
B_SPLINE_CURVE_WITH_KNOTS((3,3),(0.,0.0215367144649525),.UNSPECIFIED.)
CURVE()
GEOMETRIC_REPRESENTATION_ITEM()
RATIONAL_B_SPLINE_CURVE((1.,1.0004200897947,1.0005354248108))
REPRESENTATION_ITEM('')
);
#985=(
BOUNDED_CURVE()
B_SPLINE_CURVE(2,(#71011,#71012,#71013),.UNSPECIFIED.,.F.,.F.)
B_SPLINE_CURVE_WITH_KNOTS((3,3),(0.0378379342265302,0.059374648691449),
 .UNSPECIFIED.)
CURVE()
GEOMETRIC_REPRESENTATION_ITEM()
RATIONAL_B_SPLINE_CURVE((1.00053542480972,1.00042008979385,1.))
REPRESENTATION_ITEM('')
);
#986=(
BOUNDED_CURVE()
B_SPLINE_CURVE(2,(#71017,#71018,#71019),.UNSPECIFIED.,.F.,.F.)
B_SPLINE_CURVE_WITH_KNOTS((3,3),(0.,0.0215367144649366),.UNSPECIFIED.)
CURVE()
GEOMETRIC_REPRESENTATION_ITEM()
RATIONAL_B_SPLINE_CURVE((1.,1.00042008979726,1.00053542481407))
REPRESENTATION_ITEM('')
);
#987=(
BOUNDED_CURVE()
B_SPLINE_CURVE(2,(#71021,#71022,#71023),.UNSPECIFIED.,.F.,.F.)
B_SPLINE_CURVE_WITH_KNOTS((3,3),(0.0378379342265197,0.0593746486914487),
 .UNSPECIFIED.)
CURVE()
GEOMETRIC_REPRESENTATION_ITEM()
RATIONAL_B_SPLINE_CURVE((1.00053542480866,1.00042008979301,1.))
REPRESENTATION_ITEM('')
);
#988=(
BOUNDED_CURVE()
B_SPLINE_CURVE(2,(#71027,#71028,#71029),.UNSPECIFIED.,.F.,.F.)
B_SPLINE_CURVE_WITH_KNOTS((3,3),(0.,0.0215367144649012),.UNSPECIFIED.)
CURVE()
GEOMETRIC_REPRESENTATION_ITEM()
RATIONAL_B_SPLINE_CURVE((1.,1.00042008979525,1.0005354248115))
REPRESENTATION_ITEM('')
);
#989=(
BOUNDED_CURVE()
B_SPLINE_CURVE(2,(#71031,#71032,#71033),.UNSPECIFIED.,.F.,.F.)
B_SPLINE_CURVE_WITH_KNOTS((3,3),(0.0378379342265321,0.0593746486914488),
 .UNSPECIFIED.)
CURVE()
GEOMETRIC_REPRESENTATION_ITEM()
RATIONAL_B_SPLINE_CURVE((1.00053542481087,1.00042008979475,1.))
REPRESENTATION_ITEM('')
);
#990=(
BOUNDED_CURVE()
B_SPLINE_CURVE(2,(#71037,#71038,#71039),.UNSPECIFIED.,.F.,.F.)
B_SPLINE_CURVE_WITH_KNOTS((3,3),(0.,0.0215367144649128),.UNSPECIFIED.)
CURVE()
GEOMETRIC_REPRESENTATION_ITEM()
RATIONAL_B_SPLINE_CURVE((1.,1.00042008979245,1.00053542480793))
REPRESENTATION_ITEM('')
);
#991=(
BOUNDED_CURVE()
B_SPLINE_CURVE(2,(#71041,#71042,#71043),.UNSPECIFIED.,.F.,.F.)
B_SPLINE_CURVE_WITH_KNOTS((3,3),(0.0378379342265115,0.0593746486914485),
 .UNSPECIFIED.)
CURVE()
GEOMETRIC_REPRESENTATION_ITEM()
RATIONAL_B_SPLINE_CURVE((1.0005354248112,1.00042008979501,1.))
REPRESENTATION_ITEM('')
);
#992=(
BOUNDED_CURVE()
B_SPLINE_CURVE(2,(#71047,#71048,#71049),.UNSPECIFIED.,.F.,.F.)
B_SPLINE_CURVE_WITH_KNOTS((3,3),(0.,0.0215367144649508),.UNSPECIFIED.)
CURVE()
GEOMETRIC_REPRESENTATION_ITEM()
RATIONAL_B_SPLINE_CURVE((1.,1.00042008979591,1.00053542481235))
REPRESENTATION_ITEM('')
);
#993=(
BOUNDED_CURVE()
B_SPLINE_CURVE(2,(#71051,#71052,#71053),.UNSPECIFIED.,.F.,.F.)
B_SPLINE_CURVE_WITH_KNOTS((3,3),(0.0378379342265331,0.0593746486914485),
 .UNSPECIFIED.)
CURVE()
GEOMETRIC_REPRESENTATION_ITEM()
RATIONAL_B_SPLINE_CURVE((1.00053542481272,1.0004200897962,1.))
REPRESENTATION_ITEM('')
);
#994=(
BOUNDED_CURVE()
B_SPLINE_CURVE(2,(#71057,#71058,#71059),.UNSPECIFIED.,.F.,.F.)
B_SPLINE_CURVE_WITH_KNOTS((3,3),(0.,0.0215367144649045),.UNSPECIFIED.)
CURVE()
GEOMETRIC_REPRESENTATION_ITEM()
RATIONAL_B_SPLINE_CURVE((1.,1.0004200897958,1.00053542481221))
REPRESENTATION_ITEM('')
);
#995=(
BOUNDED_CURVE()
B_SPLINE_CURVE(2,(#71061,#71062,#71063),.UNSPECIFIED.,.F.,.F.)
B_SPLINE_CURVE_WITH_KNOTS((3,3),(0.0378379342265301,0.0593746486914479),
 .UNSPECIFIED.)
CURVE()
GEOMETRIC_REPRESENTATION_ITEM()
RATIONAL_B_SPLINE_CURVE((1.00053542481236,1.00042008979592,1.))
REPRESENTATION_ITEM('')
);
#996=(
BOUNDED_CURVE()
B_SPLINE_CURVE(2,(#71067,#71068,#71069),.UNSPECIFIED.,.F.,.F.)
B_SPLINE_CURVE_WITH_KNOTS((3,3),(0.,0.0215367144649068),.UNSPECIFIED.)
CURVE()
GEOMETRIC_REPRESENTATION_ITEM()
RATIONAL_B_SPLINE_CURVE((1.,1.00042008979466,1.00053542481075))
REPRESENTATION_ITEM('')
);
#997=(
BOUNDED_CURVE()
B_SPLINE_CURVE(2,(#71071,#71072,#71073),.UNSPECIFIED.,.F.,.F.)
B_SPLINE_CURVE_WITH_KNOTS((3,3),(0.0378379342265604,0.0593746486914483),
 .UNSPECIFIED.)
CURVE()
GEOMETRIC_REPRESENTATION_ITEM()
RATIONAL_B_SPLINE_CURVE((1.00053542481646,1.00042008979914,1.))
REPRESENTATION_ITEM('')
);
#998=(
BOUNDED_CURVE()
B_SPLINE_CURVE(2,(#71077,#71078,#71079),.UNSPECIFIED.,.F.,.F.)
B_SPLINE_CURVE_WITH_KNOTS((3,3),(0.,0.0215367144649594),.UNSPECIFIED.)
CURVE()
GEOMETRIC_REPRESENTATION_ITEM()
RATIONAL_B_SPLINE_CURVE((1.,1.00042008979357,1.00053542480936))
REPRESENTATION_ITEM('')
);
#999=(
BOUNDED_CURVE()
B_SPLINE_CURVE(2,(#71081,#71082,#71083),.UNSPECIFIED.,.F.,.F.)
B_SPLINE_CURVE_WITH_KNOTS((3,3),(0.0378379342265812,0.0593746486914485),
 .UNSPECIFIED.)
CURVE()
GEOMETRIC_REPRESENTATION_ITEM()
RATIONAL_B_SPLINE_CURVE((1.00053542481548,1.00042008979837,1.))
REPRESENTATION_ITEM('')
);
#1000=(
BOUNDED_CURVE()
B_SPLINE_CURVE(2,(#71087,#71088,#71089),.UNSPECIFIED.,.F.,.F.)
B_SPLINE_CURVE_WITH_KNOTS((3,3),(0.,0.0215367144649258),.UNSPECIFIED.)
CURVE()
GEOMETRIC_REPRESENTATION_ITEM()
RATIONAL_B_SPLINE_CURVE((1.,1.00042008979633,1.00053542481288))
REPRESENTATION_ITEM('')
);
#1001=(
BOUNDED_CURVE()
B_SPLINE_CURVE(2,(#71091,#71092,#71093),.UNSPECIFIED.,.F.,.F.)
B_SPLINE_CURVE_WITH_KNOTS((3,3),(0.0378379342265631,0.0593746486914488),
 .UNSPECIFIED.)
CURVE()
GEOMETRIC_REPRESENTATION_ITEM()
RATIONAL_B_SPLINE_CURVE((1.00053542481617,1.00042008979891,1.))
REPRESENTATION_ITEM('')
);
#1002=(
BOUNDED_CURVE()
B_SPLINE_CURVE(2,(#71096,#71097,#71098),.UNSPECIFIED.,.F.,.F.)
B_SPLINE_CURVE_WITH_KNOTS((3,3),(0.,0.0215367144650048),.UNSPECIFIED.)
CURVE()
GEOMETRIC_REPRESENTATION_ITEM()
RATIONAL_B_SPLINE_CURVE((1.,1.00042008979356,1.00053542480934))
REPRESENTATION_ITEM('')
);
#1003=TOROIDAL_SURFACE('',#14146,2.56347,0.2);
#1004=TOROIDAL_SURFACE('',#14398,2.56347,0.2);
#1005=TOROIDAL_SURFACE('',#14637,3.31023,0.2);
#1006=B_SPLINE_SURFACE_WITH_KNOTS('',3,3,((#35331,#35332,#35333,#35334,
#35335,#35336,#35337,#35338,#35339,#35340,#35341,#35342,#35343,#35344,#35345,
#35346,#35347,#35348,#35349,#35350,#35351,#35352,#35353,#35354,#35355,#35356,
#35357,#35358,#35359,#35360,#35361,#35362,#35363,#35364,#35365,#35366,#35367,
#35368,#35369,#35370,#35371,#35372,#35373,#35374,#35375,#35376,#35377,#35378,
#35379,#35380,#35381,#35382,#35383,#35384,#35385,#35386,#35387,#35388,#35389,
#35390,#35391,#35392,#35393,#35394,#35395,#35396,#35397,#35398,#35399,#35400,
#35401,#35402,#35403,#35404,#35405,#35406,#35407,#35408,#35409,#35410,#35411,
#35412,#35413,#35414,#35415,#35416,#35417,#35418,#35419,#35420,#35421,#35422,
#35423,#35424,#35425,#35426,#35427,#35428,#35429,#35430,#35431,#35432,#35433,
#35434,#35435,#35436,#35437,#35438,#35439,#35440,#35441,#35442,#35443,#35444,
#35445,#35446,#35447,#35448,#35449,#35450,#35451,#35452,#35453,#35454,#35455,
#35456),(#35457,#35458,#35459,#35460,#35461,#35462,#35463,#35464,#35465,
#35466,#35467,#35468,#35469,#35470,#35471,#35472,#35473,#35474,#35475,#35476,
#35477,#35478,#35479,#35480,#35481,#35482,#35483,#35484,#35485,#35486,#35487,
#35488,#35489,#35490,#35491,#35492,#35493,#35494,#35495,#35496,#35497,#35498,
#35499,#35500,#35501,#35502,#35503,#35504,#35505,#35506,#35507,#35508,#35509,
#35510,#35511,#35512,#35513,#35514,#35515,#35516,#35517,#35518,#35519,#35520,
#35521,#35522,#35523,#35524,#35525,#35526,#35527,#35528,#35529,#35530,#35531,
#35532,#35533,#35534,#35535,#35536,#35537,#35538,#35539,#35540,#35541,#35542,
#35543,#35544,#35545,#35546,#35547,#35548,#35549,#35550,#35551,#35552,#35553,
#35554,#35555,#35556,#35557,#35558,#35559,#35560,#35561,#35562,#35563,#35564,
#35565,#35566,#35567,#35568,#35569,#35570,#35571,#35572,#35573,#35574,#35575,
#35576,#35577,#35578,#35579,#35580,#35581,#35582),(#35583,#35584,#35585,
#35586,#35587,#35588,#35589,#35590,#35591,#35592,#35593,#35594,#35595,#35596,
#35597,#35598,#35599,#35600,#35601,#35602,#35603,#35604,#35605,#35606,#35607,
#35608,#35609,#35610,#35611,#35612,#35613,#35614,#35615,#35616,#35617,#35618,
#35619,#35620,#35621,#35622,#35623,#35624,#35625,#35626,#35627,#35628,#35629,
#35630,#35631,#35632,#35633,#35634,#35635,#35636,#35637,#35638,#35639,#35640,
#35641,#35642,#35643,#35644,#35645,#35646,#35647,#35648,#35649,#35650,#35651,
#35652,#35653,#35654,#35655,#35656,#35657,#35658,#35659,#35660,#35661,#35662,
#35663,#35664,#35665,#35666,#35667,#35668,#35669,#35670,#35671,#35672,#35673,
#35674,#35675,#35676,#35677,#35678,#35679,#35680,#35681,#35682,#35683,#35684,
#35685,#35686,#35687,#35688,#35689,#35690,#35691,#35692,#35693,#35694,#35695,
#35696,#35697,#35698,#35699,#35700,#35701,#35702,#35703,#35704,#35705,#35706,
#35707,#35708),(#35709,#35710,#35711,#35712,#35713,#35714,#35715,#35716,
#35717,#35718,#35719,#35720,#35721,#35722,#35723,#35724,#35725,#35726,#35727,
#35728,#35729,#35730,#35731,#35732,#35733,#35734,#35735,#35736,#35737,#35738,
#35739,#35740,#35741,#35742,#35743,#35744,#35745,#35746,#35747,#35748,#35749,
#35750,#35751,#35752,#35753,#35754,#35755,#35756,#35757,#35758,#35759,#35760,
#35761,#35762,#35763,#35764,#35765,#35766,#35767,#35768,#35769,#35770,#35771,
#35772,#35773,#35774,#35775,#35776,#35777,#35778,#35779,#35780,#35781,#35782,
#35783,#35784,#35785,#35786,#35787,#35788,#35789,#35790,#35791,#35792,#35793,
#35794,#35795,#35796,#35797,#35798,#35799,#35800,#35801,#35802,#35803,#35804,
#35805,#35806,#35807,#35808,#35809,#35810,#35811,#35812,#35813,#35814,#35815,
#35816,#35817,#35818,#35819,#35820,#35821,#35822,#35823,#35824,#35825,#35826,
#35827,#35828,#35829,#35830,#35831,#35832,#35833,#35834)),.UNSPECIFIED.,
 .F.,.F.,.F.,(4,4),(4,1,1,1,1,1,1,1,1,1,1,1,1,1,1,1,1,1,1,1,1,1,1,1,1,1,
1,1,1,1,1,1,1,1,1,1,1,1,1,1,1,1,1,1,1,1,1,1,1,1,1,1,1,1,1,1,1,1,1,1,1,1,
1,1,1,1,1,1,1,1,1,1,1,1,1,1,1,1,1,1,1,1,1,1,1,1,1,1,1,1,1,1,1,1,1,1,1,1,
1,1,1,1,1,1,1,1,1,1,1,1,1,1,1,1,1,1,1,1,1,1,1,1,1,4),(-0.000406578931768313,
0.050511877590733),(8.33359626324588,9.33277702554168,10.3319577878375,
11.3311385501333,12.3303193124291,13.3295000747249,14.3286808370206,15.3278615993164,
16.3270423616122,17.326223123908,18.3254038862038,19.3245846484996,20.3237654107954,
21.3229461730912,22.322126935387,23.3213076976828,24.3204884599786,25.3196692222744,
26.3188499845702,27.318030746866,28.3172115091618,29.3163922714576,30.3155730337533,
31.3147537960491,32.3139345583449,33.3131153206407,34.3122960829365,35.3114768452323,
36.3106576075281,37.3098383698239,38.3090191321197,39.3081998944155,40.3073806567113,
41.3065614190071,42.3057421813029,43.3049229435987,44.3041037058945,45.3032844681902,
46.302465230486,47.3016459927818,48.3008267550776,49.3000075173734,50.2991882796692,
51.298369041965,52.2975498042608,53.2967305665566,54.2959113288524,55.2950920911482,
56.294272853444,57.2934536157398,58.2926343780356,59.2918151403314,60.2909959026272,
61.290176664923,62.2893574272187,63.2885381895145,64.2877189518103,65.2868997141061,
66.2860804764019,67.2852612386977,68.2844420009935,69.2836227632893,70.2828035255851,
71.2819842878809,72.2811650501767,73.2803458124725,74.2795265747683,75.2787073370641,
76.2778880993599,77.2770688616556,78.2762496239514,79.2754303862472,80.274611148543,
81.2737919108388,82.2729726731346,83.2721534354304,84.2713341977262,85.270514960022,
86.2696957223178,87.2688764846136,88.2680572469094,89.2672380092052,90.266418771501,
91.2655995337968,92.2647802960926,93.2639610583883,94.2631418206841,95.2623225829799,
96.2615033452757,97.2606841075715,98.2598648698673,99.2590456321631,100.258226394459,
101.257407156755,102.25658791905,103.255768681346,104.254949443642,105.254130205938,
106.253310968234,107.252491730529,108.251672492825,109.250853255121,110.250034017417,
111.249214779713,112.248395542008,113.247576304304,114.2467570666,115.245937828896,
116.245118591192,117.244299353487,118.243480115783,119.242660878079,120.241841640375,
121.241022402671,122.240203164966,123.239383927262,124.238564689558,125.237745451854,
126.23692621415,127.236106976445,128.235287738741,129.234468501037,130.233649263333,
131.233236604561),.UNSPECIFIED.);
#1007=B_SPLINE_SURFACE_WITH_KNOTS('',3,3,((#36002,#36003,#36004,#36005,
#36006,#36007,#36008,#36009,#36010,#36011,#36012,#36013,#36014,#36015,#36016,
#36017,#36018,#36019,#36020,#36021,#36022,#36023,#36024,#36025,#36026,#36027,
#36028,#36029,#36030,#36031,#36032,#36033,#36034,#36035,#36036,#36037,#36038,
#36039,#36040,#36041,#36042,#36043,#36044,#36045,#36046,#36047,#36048,#36049,
#36050,#36051,#36052,#36053,#36054,#36055,#36056,#36057,#36058,#36059,#36060,
#36061,#36062,#36063,#36064,#36065,#36066,#36067,#36068,#36069,#36070,#36071,
#36072,#36073,#36074,#36075,#36076,#36077,#36078,#36079,#36080,#36081,#36082,
#36083,#36084,#36085,#36086,#36087,#36088,#36089,#36090,#36091,#36092,#36093,
#36094,#36095,#36096,#36097,#36098,#36099,#36100,#36101,#36102,#36103,#36104,
#36105,#36106,#36107,#36108,#36109,#36110,#36111,#36112,#36113,#36114,#36115,
#36116,#36117,#36118,#36119,#36120,#36121,#36122,#36123,#36124,#36125,#36126,
#36127),(#36128,#36129,#36130,#36131,#36132,#36133,#36134,#36135,#36136,
#36137,#36138,#36139,#36140,#36141,#36142,#36143,#36144,#36145,#36146,#36147,
#36148,#36149,#36150,#36151,#36152,#36153,#36154,#36155,#36156,#36157,#36158,
#36159,#36160,#36161,#36162,#36163,#36164,#36165,#36166,#36167,#36168,#36169,
#36170,#36171,#36172,#36173,#36174,#36175,#36176,#36177,#36178,#36179,#36180,
#36181,#36182,#36183,#36184,#36185,#36186,#36187,#36188,#36189,#36190,#36191,
#36192,#36193,#36194,#36195,#36196,#36197,#36198,#36199,#36200,#36201,#36202,
#36203,#36204,#36205,#36206,#36207,#36208,#36209,#36210,#36211,#36212,#36213,
#36214,#36215,#36216,#36217,#36218,#36219,#36220,#36221,#36222,#36223,#36224,
#36225,#36226,#36227,#36228,#36229,#36230,#36231,#36232,#36233,#36234,#36235,
#36236,#36237,#36238,#36239,#36240,#36241,#36242,#36243,#36244,#36245,#36246,
#36247,#36248,#36249,#36250,#36251,#36252,#36253),(#36254,#36255,#36256,
#36257,#36258,#36259,#36260,#36261,#36262,#36263,#36264,#36265,#36266,#36267,
#36268,#36269,#36270,#36271,#36272,#36273,#36274,#36275,#36276,#36277,#36278,
#36279,#36280,#36281,#36282,#36283,#36284,#36285,#36286,#36287,#36288,#36289,
#36290,#36291,#36292,#36293,#36294,#36295,#36296,#36297,#36298,#36299,#36300,
#36301,#36302,#36303,#36304,#36305,#36306,#36307,#36308,#36309,#36310,#36311,
#36312,#36313,#36314,#36315,#36316,#36317,#36318,#36319,#36320,#36321,#36322,
#36323,#36324,#36325,#36326,#36327,#36328,#36329,#36330,#36331,#36332,#36333,
#36334,#36335,#36336,#36337,#36338,#36339,#36340,#36341,#36342,#36343,#36344,
#36345,#36346,#36347,#36348,#36349,#36350,#36351,#36352,#36353,#36354,#36355,
#36356,#36357,#36358,#36359,#36360,#36361,#36362,#36363,#36364,#36365,#36366,
#36367,#36368,#36369,#36370,#36371,#36372,#36373,#36374,#36375,#36376,#36377,
#36378,#36379),(#36380,#36381,#36382,#36383,#36384,#36385,#36386,#36387,
#36388,#36389,#36390,#36391,#36392,#36393,#36394,#36395,#36396,#36397,#36398,
#36399,#36400,#36401,#36402,#36403,#36404,#36405,#36406,#36407,#36408,#36409,
#36410,#36411,#36412,#36413,#36414,#36415,#36416,#36417,#36418,#36419,#36420,
#36421,#36422,#36423,#36424,#36425,#36426,#36427,#36428,#36429,#36430,#36431,
#36432,#36433,#36434,#36435,#36436,#36437,#36438,#36439,#36440,#36441,#36442,
#36443,#36444,#36445,#36446,#36447,#36448,#36449,#36450,#36451,#36452,#36453,
#36454,#36455,#36456,#36457,#36458,#36459,#36460,#36461,#36462,#36463,#36464,
#36465,#36466,#36467,#36468,#36469,#36470,#36471,#36472,#36473,#36474,#36475,
#36476,#36477,#36478,#36479,#36480,#36481,#36482,#36483,#36484,#36485,#36486,
#36487,#36488,#36489,#36490,#36491,#36492,#36493,#36494,#36495,#36496,#36497,
#36498,#36499,#36500,#36501,#36502,#36503,#36504,#36505)),.UNSPECIFIED.,
 .F.,.F.,.F.,(4,4),(4,1,1,1,1,1,1,1,1,1,1,1,1,1,1,1,1,1,1,1,1,1,1,1,1,1,
1,1,1,1,1,1,1,1,1,1,1,1,1,1,1,1,1,1,1,1,1,1,1,1,1,1,1,1,1,1,1,1,1,1,1,1,
1,1,1,1,1,1,1,1,1,1,1,1,1,1,1,1,1,1,1,1,1,1,1,1,1,1,1,1,1,1,1,1,1,1,1,1,
1,1,1,1,1,1,1,1,1,1,1,1,1,1,1,1,1,1,1,1,1,1,1,1,1,4),(-0.000343459060642306,
0.0505598735282669),(11.6721236773201,12.6717110499602,13.670891812256,
14.6700725745517,15.6692533368475,16.6684340991433,17.6676148614391,18.6667956237349,
19.6659763860307,20.6651571483265,21.6643379106223,22.6635186729181,23.6626994352139,
24.6618801975097,25.6610609598055,26.6602417221013,27.6594224843971,28.6586032466929,
29.6577840089887,30.6569647712845,31.6561455335802,32.655326295876,33.6545070581718,
34.6536878204676,35.6528685827634,36.6520493450592,37.651230107355,38.6504108696508,
39.6495916319466,40.6487723942424,41.6479531565382,42.647133918834,43.6463146811298,
44.6454954434256,45.6446762057214,46.6438569680172,47.643037730313,48.6422184926087,
49.6413992549045,50.6405800172003,51.6397607794961,52.6389415417919,53.6381223040877,
54.6373030663835,55.6364838286793,56.6356645909751,57.6348453532709,58.6340261155667,
59.6332068778625,60.6323876401583,61.6315684024541,62.6307491647499,63.6299299270457,
64.6291106893415,65.6282914516373,66.627472213933,67.6266529762288,68.6258337385246,
69.6250145008204,70.6241952631162,71.623376025412,72.6225567877078,73.6217375500036,
74.6209183122994,75.6200990745952,76.619279836891,77.6184605991868,78.6176413614826,
79.6168221237784,80.6160028860742,81.6151836483699,82.6143644106657,83.6135451729615,
84.6127259352573,85.6119066975531,86.6110874598489,87.6102682221447,88.6094489844405,
89.6086297467363,90.6078105090321,91.6069912713279,92.6061720336237,93.6053527959195,
94.6045335582153,95.6037143205111,96.6028950828069,97.6020758451027,98.6012566073985,
99.6004373696942,100.59961813199,101.598798894286,102.597979656582,103.597160418877,
104.596341181173,105.595521943469,106.594702705765,107.593883468061,108.593064230356,
109.592244992652,110.591425754948,111.590606517244,112.58978727954,113.588968041835,
114.588148804131,115.587329566427,116.586510328723,117.585691091019,118.584871853314,
119.58405261561,120.583233377906,121.582414140202,122.581594902498,123.580775664793,
124.579956427089,125.579137189385,126.578317951681,127.577498713976,128.576679476272,
129.575860238568,130.575041000864,131.57422176316,132.573402525455,133.572583287751,
134.571764050047),.UNSPECIFIED.);
#1008=B_SPLINE_SURFACE_WITH_KNOTS('',3,3,((#57303,#57304,#57305,#57306,
#57307,#57308,#57309,#57310,#57311,#57312,#57313,#57314,#57315,#57316,#57317,
#57318,#57319,#57320,#57321,#57322,#57323,#57324,#57325,#57326,#57327,#57328,
#57329,#57330,#57331,#57332,#57333,#57334,#57335,#57336,#57337,#57338,#57339,
#57340,#57341,#57342,#57343,#57344,#57345,#57346,#57347,#57348,#57349,#57350,
#57351,#57352,#57353,#57354,#57355,#57356,#57357,#57358,#57359,#57360,#57361,
#57362,#57363,#57364,#57365,#57366,#57367,#57368,#57369,#57370,#57371,#57372,
#57373,#57374,#57375,#57376,#57377,#57378,#57379,#57380,#57381,#57382,#57383,
#57384,#57385,#57386,#57387,#57388,#57389,#57390,#57391,#57392,#57393,#57394,
#57395,#57396,#57397,#57398,#57399,#57400,#57401,#57402,#57403,#57404,#57405,
#57406,#57407,#57408,#57409,#57410,#57411,#57412,#57413,#57414,#57415,#57416,
#57417,#57418,#57419,#57420,#57421,#57422,#57423,#57424,#57425,#57426,#57427,
#57428,#57429,#57430,#57431,#57432,#57433,#57434,#57435,#57436,#57437,#57438,
#57439,#57440,#57441,#57442,#57443,#57444,#57445,#57446,#57447,#57448,#57449,
#57450,#57451,#57452,#57453,#57454,#57455,#57456,#57457,#57458,#57459,#57460,
#57461,#57462,#57463,#57464,#57465,#57466,#57467,#57468,#57469,#57470,#57471,
#57472,#57473,#57474,#57475,#57476,#57477,#57478,#57479),(#57480,#57481,
#57482,#57483,#57484,#57485,#57486,#57487,#57488,#57489,#57490,#57491,#57492,
#57493,#57494,#57495,#57496,#57497,#57498,#57499,#57500,#57501,#57502,#57503,
#57504,#57505,#57506,#57507,#57508,#57509,#57510,#57511,#57512,#57513,#57514,
#57515,#57516,#57517,#57518,#57519,#57520,#57521,#57522,#57523,#57524,#57525,
#57526,#57527,#57528,#57529,#57530,#57531,#57532,#57533,#57534,#57535,#57536,
#57537,#57538,#57539,#57540,#57541,#57542,#57543,#57544,#57545,#57546,#57547,
#57548,#57549,#57550,#57551,#57552,#57553,#57554,#57555,#57556,#57557,#57558,
#57559,#57560,#57561,#57562,#57563,#57564,#57565,#57566,#57567,#57568,#57569,
#57570,#57571,#57572,#57573,#57574,#57575,#57576,#57577,#57578,#57579,#57580,
#57581,#57582,#57583,#57584,#57585,#57586,#57587,#57588,#57589,#57590,#57591,
#57592,#57593,#57594,#57595,#57596,#57597,#57598,#57599,#57600,#57601,#57602,
#57603,#57604,#57605,#57606,#57607,#57608,#57609,#57610,#57611,#57612,#57613,
#57614,#57615,#57616,#57617,#57618,#57619,#57620,#57621,#57622,#57623,#57624,
#57625,#57626,#57627,#57628,#57629,#57630,#57631,#57632,#57633,#57634,#57635,
#57636,#57637,#57638,#57639,#57640,#57641,#57642,#57643,#57644,#57645,#57646,
#57647,#57648,#57649,#57650,#57651,#57652,#57653,#57654,#57655,#57656),
(#57657,#57658,#57659,#57660,#57661,#57662,#57663,#57664,#57665,#57666,
#57667,#57668,#57669,#57670,#57671,#57672,#57673,#57674,#57675,#57676,#57677,
#57678,#57679,#57680,#57681,#57682,#57683,#57684,#57685,#57686,#57687,#57688,
#57689,#57690,#57691,#57692,#57693,#57694,#57695,#57696,#57697,#57698,#57699,
#57700,#57701,#57702,#57703,#57704,#57705,#57706,#57707,#57708,#57709,#57710,
#57711,#57712,#57713,#57714,#57715,#57716,#57717,#57718,#57719,#57720,#57721,
#57722,#57723,#57724,#57725,#57726,#57727,#57728,#57729,#57730,#57731,#57732,
#57733,#57734,#57735,#57736,#57737,#57738,#57739,#57740,#57741,#57742,#57743,
#57744,#57745,#57746,#57747,#57748,#57749,#57750,#57751,#57752,#57753,#57754,
#57755,#57756,#57757,#57758,#57759,#57760,#57761,#57762,#57763,#57764,#57765,
#57766,#57767,#57768,#57769,#57770,#57771,#57772,#57773,#57774,#57775,#57776,
#57777,#57778,#57779,#57780,#57781,#57782,#57783,#57784,#57785,#57786,#57787,
#57788,#57789,#57790,#57791,#57792,#57793,#57794,#57795,#57796,#57797,#57798,
#57799,#57800,#57801,#57802,#57803,#57804,#57805,#57806,#57807,#57808,#57809,
#57810,#57811,#57812,#57813,#57814,#57815,#57816,#57817,#57818,#57819,#57820,
#57821,#57822,#57823,#57824,#57825,#57826,#57827,#57828,#57829,#57830,#57831,
#57832,#57833),(#57834,#57835,#57836,#57837,#57838,#57839,#57840,#57841,
#57842,#57843,#57844,#57845,#57846,#57847,#57848,#57849,#57850,#57851,#57852,
#57853,#57854,#57855,#57856,#57857,#57858,#57859,#57860,#57861,#57862,#57863,
#57864,#57865,#57866,#57867,#57868,#57869,#57870,#57871,#57872,#57873,#57874,
#57875,#57876,#57877,#57878,#57879,#57880,#57881,#57882,#57883,#57884,#57885,
#57886,#57887,#57888,#57889,#57890,#57891,#57892,#57893,#57894,#57895,#57896,
#57897,#57898,#57899,#57900,#57901,#57902,#57903,#57904,#57905,#57906,#57907,
#57908,#57909,#57910,#57911,#57912,#57913,#57914,#57915,#57916,#57917,#57918,
#57919,#57920,#57921,#57922,#57923,#57924,#57925,#57926,#57927,#57928,#57929,
#57930,#57931,#57932,#57933,#57934,#57935,#57936,#57937,#57938,#57939,#57940,
#57941,#57942,#57943,#57944,#57945,#57946,#57947,#57948,#57949,#57950,#57951,
#57952,#57953,#57954,#57955,#57956,#57957,#57958,#57959,#57960,#57961,#57962,
#57963,#57964,#57965,#57966,#57967,#57968,#57969,#57970,#57971,#57972,#57973,
#57974,#57975,#57976,#57977,#57978,#57979,#57980,#57981,#57982,#57983,#57984,
#57985,#57986,#57987,#57988,#57989,#57990,#57991,#57992,#57993,#57994,#57995,
#57996,#57997,#57998,#57999,#58000,#58001,#58002,#58003,#58004,#58005,#58006,
#58007,#58008,#58009,#58010)),.UNSPECIFIED.,.F.,.F.,.F.,(4,4),(4,1,1,1,
1,1,1,1,1,1,1,1,1,1,1,1,1,1,1,1,1,1,1,1,1,1,1,1,1,1,1,1,1,1,1,1,1,1,1,1,
1,1,1,1,1,1,1,1,1,1,1,1,1,1,1,1,1,1,1,1,1,1,1,1,1,1,1,1,1,1,1,1,1,1,1,1,
1,1,1,1,1,1,1,1,1,1,1,1,1,1,1,1,1,1,1,1,1,1,1,1,1,1,1,1,1,1,1,1,1,1,1,1,
1,1,1,1,1,1,1,1,1,1,1,1,1,1,1,1,1,1,1,1,1,1,1,1,1,1,1,1,1,1,1,1,1,1,1,1,
1,1,1,1,1,1,1,1,1,1,1,1,1,1,1,1,1,1,1,1,1,1,1,1,1,1,4),(-0.000395455933507198,
0.0505042896976108),(8.33359626324614,9.32879578175085,10.3239953002556,
11.3191948187603,12.314394337265,13.3095938557697,14.3047933742744,15.2999928927791,
16.2951924112838,17.2903919297885,18.2855914482932,19.2807909667979,20.2759904853026,
21.2711900038073,22.2663895223121,23.2615890408168,24.2567885593215,25.2519880778262,
26.2471875963309,27.2423871148356,28.2375866333403,29.232786151845,30.2279856703497,
31.2231851888544,32.2183847073591,33.2135842258639,34.2087837443686,35.2039832628733,
36.199182781378,37.1943822998827,38.1895818183874,39.1847813368921,40.1799808553968,
41.1751803739015,42.1703798924062,43.1655794109109,44.1607789294156,45.1559784479203,
46.1511779664251,47.1463774849298,48.1415770034345,49.1367765219392,50.1319760404439,
51.1271755589486,52.1223750774533,53.117574595958,54.1127741144627,55.1079736329674,
56.1031731514721,57.0983726699769,58.0935721884816,59.0887717069863,60.083971225491,
61.0791707439957,62.0743702625004,63.0695697810051,64.0647692995098,65.0599688180145,
66.0551683365192,67.0503678550239,68.0455673735286,69.0407668920334,70.0359664105381,
71.0311659290428,72.0263654475475,73.0215649660522,74.0167644845569,75.0119640030616,
76.0071635215663,77.002363040071,77.9975625585757,78.9927620770804,79.9879615955851,
80.9831611140899,81.9783606325946,82.9735601510993,83.968759669604,84.9639591881087,
85.9591587066134,86.9543582251181,87.9495577436228,88.9447572621275,89.9399567806322,
90.9351562991369,91.9303558176416,92.9255553361464,93.9207548546511,94.9159543731558,
95.9111538916605,96.9063534101652,97.9015529286699,98.8967524471746,99.8919519656793,
100.887151484184,101.882351002689,102.877550521193,103.872750039698,104.867949558203,
105.863149076708,106.858348595212,107.853548113717,108.848747632222,109.843947150726,
110.839146669231,111.834346187736,112.829545706241,113.824745224745,114.81994474325,
115.815144261755,116.810343780259,117.805543298764,118.800742817269,119.795942335773,
120.791141854278,121.786341372783,122.781540891288,123.776740409792,124.771939928297,
125.767139446802,126.762338965306,127.757538483811,128.752738002316,129.747937520821,
130.743137039325,131.73833655783,132.733536076335,133.728735594839,134.723935113344,
135.719134631849,136.714334150354,137.709533668858,138.704733187363,139.699932705868,
140.695132224372,141.690331742877,142.685531261382,143.680730779886,144.675930298391,
145.671129816896,146.666329335401,147.661528853905,148.65672837241,149.651927890915,
150.647127409419,151.642326927924,152.637526446429,153.632725964934,154.627925483438,
155.623125001943,156.618324520448,157.613524038952,158.608723557457,159.603923075962,
160.599122594467,161.594322112971,162.589521631476,163.584721149981,164.579920668485,
165.57512018699,166.570319705495,167.565519224,168.560718742504,169.555918261009,
170.551117779514,171.546317298018,172.541516816523,173.536716335028,174.531915853532,
175.527115372037,176.522314890542,177.517514409047,178.512713927551,179.507913446056,
180.503112964561,181.498707938999),.UNSPECIFIED.);
#1009=B_SPLINE_SURFACE_WITH_KNOTS('',3,3,((#58181,#58182,#58183,#58184,
#58185,#58186,#58187,#58188,#58189,#58190,#58191,#58192,#58193,#58194,#58195,
#58196,#58197,#58198,#58199,#58200,#58201,#58202,#58203,#58204,#58205,#58206,
#58207,#58208,#58209,#58210,#58211,#58212,#58213,#58214,#58215,#58216,#58217,
#58218,#58219,#58220,#58221,#58222,#58223,#58224,#58225,#58226,#58227,#58228,
#58229,#58230,#58231,#58232,#58233,#58234,#58235,#58236,#58237,#58238,#58239,
#58240,#58241,#58242,#58243,#58244,#58245,#58246,#58247,#58248,#58249,#58250,
#58251,#58252,#58253,#58254,#58255,#58256,#58257,#58258,#58259,#58260,#58261,
#58262,#58263,#58264,#58265,#58266,#58267,#58268,#58269,#58270,#58271,#58272,
#58273,#58274,#58275,#58276,#58277,#58278,#58279,#58280,#58281,#58282,#58283,
#58284,#58285,#58286,#58287,#58288,#58289,#58290,#58291,#58292,#58293,#58294,
#58295,#58296,#58297,#58298,#58299,#58300,#58301,#58302,#58303,#58304,#58305,
#58306,#58307,#58308,#58309,#58310,#58311,#58312,#58313,#58314,#58315,#58316,
#58317,#58318,#58319,#58320,#58321,#58322,#58323,#58324,#58325,#58326,#58327,
#58328,#58329,#58330,#58331,#58332,#58333,#58334,#58335,#58336,#58337,#58338,
#58339,#58340,#58341,#58342,#58343,#58344,#58345,#58346,#58347,#58348,#58349,
#58350,#58351,#58352,#58353,#58354,#58355,#58356,#58357),(#58358,#58359,
#58360,#58361,#58362,#58363,#58364,#58365,#58366,#58367,#58368,#58369,#58370,
#58371,#58372,#58373,#58374,#58375,#58376,#58377,#58378,#58379,#58380,#58381,
#58382,#58383,#58384,#58385,#58386,#58387,#58388,#58389,#58390,#58391,#58392,
#58393,#58394,#58395,#58396,#58397,#58398,#58399,#58400,#58401,#58402,#58403,
#58404,#58405,#58406,#58407,#58408,#58409,#58410,#58411,#58412,#58413,#58414,
#58415,#58416,#58417,#58418,#58419,#58420,#58421,#58422,#58423,#58424,#58425,
#58426,#58427,#58428,#58429,#58430,#58431,#58432,#58433,#58434,#58435,#58436,
#58437,#58438,#58439,#58440,#58441,#58442,#58443,#58444,#58445,#58446,#58447,
#58448,#58449,#58450,#58451,#58452,#58453,#58454,#58455,#58456,#58457,#58458,
#58459,#58460,#58461,#58462,#58463,#58464,#58465,#58466,#58467,#58468,#58469,
#58470,#58471,#58472,#58473,#58474,#58475,#58476,#58477,#58478,#58479,#58480,
#58481,#58482,#58483,#58484,#58485,#58486,#58487,#58488,#58489,#58490,#58491,
#58492,#58493,#58494,#58495,#58496,#58497,#58498,#58499,#58500,#58501,#58502,
#58503,#58504,#58505,#58506,#58507,#58508,#58509,#58510,#58511,#58512,#58513,
#58514,#58515,#58516,#58517,#58518,#58519,#58520,#58521,#58522,#58523,#58524,
#58525,#58526,#58527,#58528,#58529,#58530,#58531,#58532,#58533,#58534),
(#58535,#58536,#58537,#58538,#58539,#58540,#58541,#58542,#58543,#58544,
#58545,#58546,#58547,#58548,#58549,#58550,#58551,#58552,#58553,#58554,#58555,
#58556,#58557,#58558,#58559,#58560,#58561,#58562,#58563,#58564,#58565,#58566,
#58567,#58568,#58569,#58570,#58571,#58572,#58573,#58574,#58575,#58576,#58577,
#58578,#58579,#58580,#58581,#58582,#58583,#58584,#58585,#58586,#58587,#58588,
#58589,#58590,#58591,#58592,#58593,#58594,#58595,#58596,#58597,#58598,#58599,
#58600,#58601,#58602,#58603,#58604,#58605,#58606,#58607,#58608,#58609,#58610,
#58611,#58612,#58613,#58614,#58615,#58616,#58617,#58618,#58619,#58620,#58621,
#58622,#58623,#58624,#58625,#58626,#58627,#58628,#58629,#58630,#58631,#58632,
#58633,#58634,#58635,#58636,#58637,#58638,#58639,#58640,#58641,#58642,#58643,
#58644,#58645,#58646,#58647,#58648,#58649,#58650,#58651,#58652,#58653,#58654,
#58655,#58656,#58657,#58658,#58659,#58660,#58661,#58662,#58663,#58664,#58665,
#58666,#58667,#58668,#58669,#58670,#58671,#58672,#58673,#58674,#58675,#58676,
#58677,#58678,#58679,#58680,#58681,#58682,#58683,#58684,#58685,#58686,#58687,
#58688,#58689,#58690,#58691,#58692,#58693,#58694,#58695,#58696,#58697,#58698,
#58699,#58700,#58701,#58702,#58703,#58704,#58705,#58706,#58707,#58708,#58709,
#58710,#58711),(#58712,#58713,#58714,#58715,#58716,#58717,#58718,#58719,
#58720,#58721,#58722,#58723,#58724,#58725,#58726,#58727,#58728,#58729,#58730,
#58731,#58732,#58733,#58734,#58735,#58736,#58737,#58738,#58739,#58740,#58741,
#58742,#58743,#58744,#58745,#58746,#58747,#58748,#58749,#58750,#58751,#58752,
#58753,#58754,#58755,#58756,#58757,#58758,#58759,#58760,#58761,#58762,#58763,
#58764,#58765,#58766,#58767,#58768,#58769,#58770,#58771,#58772,#58773,#58774,
#58775,#58776,#58777,#58778,#58779,#58780,#58781,#58782,#58783,#58784,#58785,
#58786,#58787,#58788,#58789,#58790,#58791,#58792,#58793,#58794,#58795,#58796,
#58797,#58798,#58799,#58800,#58801,#58802,#58803,#58804,#58805,#58806,#58807,
#58808,#58809,#58810,#58811,#58812,#58813,#58814,#58815,#58816,#58817,#58818,
#58819,#58820,#58821,#58822,#58823,#58824,#58825,#58826,#58827,#58828,#58829,
#58830,#58831,#58832,#58833,#58834,#58835,#58836,#58837,#58838,#58839,#58840,
#58841,#58842,#58843,#58844,#58845,#58846,#58847,#58848,#58849,#58850,#58851,
#58852,#58853,#58854,#58855,#58856,#58857,#58858,#58859,#58860,#58861,#58862,
#58863,#58864,#58865,#58866,#58867,#58868,#58869,#58870,#58871,#58872,#58873,
#58874,#58875,#58876,#58877,#58878,#58879,#58880,#58881,#58882,#58883,#58884,
#58885,#58886,#58887,#58888)),.UNSPECIFIED.,.F.,.F.,.F.,(4,4),(4,1,1,1,
1,1,1,1,1,1,1,1,1,1,1,1,1,1,1,1,1,1,1,1,1,1,1,1,1,1,1,1,1,1,1,1,1,1,1,1,
1,1,1,1,1,1,1,1,1,1,1,1,1,1,1,1,1,1,1,1,1,1,1,1,1,1,1,1,1,1,1,1,1,1,1,1,
1,1,1,1,1,1,1,1,1,1,1,1,1,1,1,1,1,1,1,1,1,1,1,1,1,1,1,1,1,1,1,1,1,1,1,1,
1,1,1,1,1,1,1,1,1,1,1,1,1,1,1,1,1,1,1,1,1,1,1,1,1,1,1,1,1,1,1,1,1,1,1,1,
1,1,1,1,1,1,1,1,1,1,1,1,1,1,1,1,1,1,1,1,1,1,1,1,1,1,4),(-0.000351020118781134,
0.0505486889477217),(11.6721348619008,12.6677298061693,13.662929324674,
14.6581288431788,15.6533283616835,16.6485278801882,17.6437273986929,18.6389269171976,
19.6341264357023,20.629325954207,21.6245254727117,22.6197249912164,23.6149245097211,
24.6101240282258,25.6053235467305,26.6005230652353,27.59572258374,28.5909221022447,
29.5861216207494,30.5813211392541,31.5765206577588,32.5717201762635,33.5669196947682,
34.5621192132729,35.5573187317776,36.5525182502823,37.5477177687871,38.5429172872918,
39.5381168057965,40.5333163243012,41.5285158428059,42.5237153613106,43.5189148798153,
44.51411439832,45.5093139168247,46.5045134353294,47.4997129538341,48.4949124723388,
49.4901119908436,50.4853115093483,51.480511027853,52.4757105463577,53.4709100648624,
54.4661095833671,55.4613091018718,56.4565086203765,57.4517081388812,58.4469076573859,
59.4421071758906,60.4373066943953,61.4325062129001,62.4277057314048,63.4229052499095,
64.4181047684142,65.4133042869189,66.4085038054236,67.4037033239283,68.398902842433,
69.3941023609377,70.3893018794424,71.3845013979471,72.3797009164519,73.3749004349566,
74.3700999534613,75.365299471966,76.3604989904707,77.3556985089754,78.3508980274801,
79.3460975459848,80.3412970644895,81.3364965829942,82.3316961014989,83.3268956200036,
84.3220951385084,85.3172946570131,86.3124941755178,87.3076936940225,88.3028932125272,
89.2980927310319,90.2932922495366,91.2884917680413,92.283691286546,93.2788908050507,
94.2740903235554,95.2692898420601,96.2644893605649,97.2596888790696,98.2548883975743,
99.250087916079,100.245287434584,101.240486953088,102.235686471593,103.230885990098,
104.226085508603,105.221285027107,106.216484545612,107.211684064117,108.206883582621,
109.202083101126,110.197282619631,111.192482138135,112.18768165664,113.182881175145,
114.17808069365,115.173280212154,116.168479730659,117.163679249164,118.158878767668,
119.154078286173,120.149277804678,121.144477323183,122.139676841687,123.134876360192,
124.130075878697,125.125275397201,126.120474915706,127.115674434211,128.110873952716,
129.10607347122,130.101272989725,131.09647250823,132.091672026734,133.086871545239,
134.082071063744,135.077270582249,136.072470100753,137.067669619258,138.062869137763,
139.058068656267,140.053268174772,141.048467693277,142.043667211781,143.038866730286,
144.034066248791,145.029265767296,146.0244652858,147.019664804305,148.01486432281,
149.010063841314,150.005263359819,151.000462878324,151.995662396829,152.990861915333,
153.986061433838,154.981260952343,155.976460470847,156.971659989352,157.966859507857,
158.962059026361,159.957258544866,160.952458063371,161.947657581876,162.94285710038,
163.938056618885,164.93325613739,165.928455655894,166.923655174399,167.918854692904,
168.914054211409,169.909253729913,170.904453248418,171.899652766923,172.894852285427,
173.890051803932,174.885251322437,175.880450840942,176.875650359446,177.870849877951,
178.866049396456,179.86124891496,180.856448433465,181.85164795197,182.846847470474,
183.842046988979,184.837597527603),.UNSPECIFIED.);
#1010=B_SPLINE_SURFACE_WITH_KNOTS('',3,3,((#69746,#69747,#69748,#69749,
#69750,#69751,#69752,#69753,#69754,#69755,#69756,#69757,#69758,#69759,#69760,
#69761,#69762,#69763,#69764,#69765,#69766,#69767,#69768,#69769,#69770,#69771,
#69772,#69773,#69774,#69775,#69776,#69777,#69778,#69779,#69780,#69781,#69782,
#69783,#69784,#69785,#69786,#69787,#69788,#69789,#69790,#69791,#69792,#69793,
#69794,#69795,#69796,#69797,#69798,#69799,#69800,#69801,#69802,#69803,#69804,
#69805,#69806,#69807,#69808,#69809,#69810,#69811,#69812,#69813,#69814,#69815,
#69816,#69817,#69818,#69819,#69820,#69821,#69822,#69823,#69824,#69825,#69826,
#69827,#69828,#69829,#69830,#69831,#69832,#69833,#69834,#69835,#69836,#69837,
#69838,#69839,#69840,#69841,#69842),(#69843,#69844,#69845,#69846,#69847,
#69848,#69849,#69850,#69851,#69852,#69853,#69854,#69855,#69856,#69857,#69858,
#69859,#69860,#69861,#69862,#69863,#69864,#69865,#69866,#69867,#69868,#69869,
#69870,#69871,#69872,#69873,#69874,#69875,#69876,#69877,#69878,#69879,#69880,
#69881,#69882,#69883,#69884,#69885,#69886,#69887,#69888,#69889,#69890,#69891,
#69892,#69893,#69894,#69895,#69896,#69897,#69898,#69899,#69900,#69901,#69902,
#69903,#69904,#69905,#69906,#69907,#69908,#69909,#69910,#69911,#69912,#69913,
#69914,#69915,#69916,#69917,#69918,#69919,#69920,#69921,#69922,#69923,#69924,
#69925,#69926,#69927,#69928,#69929,#69930,#69931,#69932,#69933,#69934,#69935,
#69936,#69937,#69938,#69939),(#69940,#69941,#69942,#69943,#69944,#69945,
#69946,#69947,#69948,#69949,#69950,#69951,#69952,#69953,#69954,#69955,#69956,
#69957,#69958,#69959,#69960,#69961,#69962,#69963,#69964,#69965,#69966,#69967,
#69968,#69969,#69970,#69971,#69972,#69973,#69974,#69975,#69976,#69977,#69978,
#69979,#69980,#69981,#69982,#69983,#69984,#69985,#69986,#69987,#69988,#69989,
#69990,#69991,#69992,#69993,#69994,#69995,#69996,#69997,#69998,#69999,#70000,
#70001,#70002,#70003,#70004,#70005,#70006,#70007,#70008,#70009,#70010,#70011,
#70012,#70013,#70014,#70015,#70016,#70017,#70018,#70019,#70020,#70021,#70022,
#70023,#70024,#70025,#70026,#70027,#70028,#70029,#70030,#70031,#70032,#70033,
#70034,#70035,#70036),(#70037,#70038,#70039,#70040,#70041,#70042,#70043,
#70044,#70045,#70046,#70047,#70048,#70049,#70050,#70051,#70052,#70053,#70054,
#70055,#70056,#70057,#70058,#70059,#70060,#70061,#70062,#70063,#70064,#70065,
#70066,#70067,#70068,#70069,#70070,#70071,#70072,#70073,#70074,#70075,#70076,
#70077,#70078,#70079,#70080,#70081,#70082,#70083,#70084,#70085,#70086,#70087,
#70088,#70089,#70090,#70091,#70092,#70093,#70094,#70095,#70096,#70097,#70098,
#70099,#70100,#70101,#70102,#70103,#70104,#70105,#70106,#70107,#70108,#70109,
#70110,#70111,#70112,#70113,#70114,#70115,#70116,#70117,#70118,#70119,#70120,
#70121,#70122,#70123,#70124,#70125,#70126,#70127,#70128,#70129,#70130,#70131,
#70132,#70133)),.UNSPECIFIED.,.F.,.F.,.F.,(4,4),(4,1,1,1,1,1,1,1,1,1,1,
1,1,1,1,1,1,1,1,1,1,1,1,1,1,1,1,1,1,1,1,1,1,1,1,1,1,1,1,1,1,1,1,1,1,1,1,
1,1,1,1,1,1,1,1,1,1,1,1,1,1,1,1,1,1,1,1,1,1,1,1,1,1,1,1,1,1,1,1,1,1,1,1,
1,1,1,1,1,1,1,1,1,1,1,4),(-0.000489567166405237,0.0818460149219149),(8.32561554604337,
9.31809068326254,10.3105658204817,11.3030409577009,12.29551609492,13.2879912321392,
14.2804663693584,15.2729415065776,16.2654166437967,17.2578917810159,18.2503669182351,
19.2428420554542,20.2353171926734,21.2277923298926,22.2202674671117,23.2127426043309,
24.2052177415501,25.1976928787692,26.1901680159884,27.1826431532076,28.1751182904267,
29.1675934276459,30.1600685648651,31.1525437020842,32.1450188393034,33.1374939765226,
34.1299691137418,35.1224442509609,36.1149193881801,37.1073945253993,38.0998696626184,
39.0923447998376,40.0848199370568,41.0772950742759,42.0697702114951,43.0622453487143,
44.0547204859334,45.0471956231526,46.0396707603718,47.032145897591,48.0246210348101,
49.0170961720293,50.0095713092485,51.0020464464676,51.9945215836868,52.986996720906,
53.9794718581251,54.9719469953443,55.9644221325635,56.9568972697826,57.9493724070018,
58.941847544221,59.9343226814401,60.9267978186593,61.9192729558785,62.9117480930976,
63.9042232303168,64.896698367536,65.8891735047551,66.8816486419743,67.8741237791935,
68.8665989164127,69.8590740536318,70.851549190851,71.8440243280702,72.8364994652893,
73.8289746025085,74.8214497397277,75.8139248769468,76.806400014166,77.7988751513852,
78.7913502886043,79.7838254258235,80.7763005630427,81.7687757002619,82.761250837481,
83.7537259747002,84.7462011119194,85.7386762491385,86.7311513863577,87.7236265235769,
88.716101660796,89.7085767980152,90.7010519352344,91.6935270724535,92.6860022096727,
93.6784773468919,94.670952484111,95.6634276213302,96.6559027585494,97.6483778957685,
98.6408530329877,99.6333281702069,100.625803307426,101.618768011811),
 .UNSPECIFIED.);
#1011=B_SPLINE_SURFACE_WITH_KNOTS('',3,3,((#70322,#70323,#70324,#70325,
#70326,#70327,#70328,#70329,#70330,#70331,#70332,#70333,#70334,#70335,#70336,
#70337,#70338,#70339,#70340,#70341,#70342,#70343,#70344,#70345,#70346,#70347,
#70348,#70349,#70350,#70351,#70352,#70353,#70354,#70355,#70356,#70357,#70358,
#70359,#70360,#70361,#70362,#70363,#70364,#70365,#70366,#70367,#70368,#70369,
#70370,#70371,#70372,#70373,#70374,#70375,#70376,#70377,#70378,#70379,#70380,
#70381,#70382,#70383,#70384,#70385,#70386,#70387,#70388,#70389,#70390,#70391,
#70392,#70393,#70394,#70395,#70396,#70397,#70398,#70399,#70400,#70401,#70402,
#70403,#70404,#70405,#70406,#70407,#70408,#70409,#70410,#70411,#70412,#70413,
#70414,#70415,#70416,#70417,#70418),(#70419,#70420,#70421,#70422,#70423,
#70424,#70425,#70426,#70427,#70428,#70429,#70430,#70431,#70432,#70433,#70434,
#70435,#70436,#70437,#70438,#70439,#70440,#70441,#70442,#70443,#70444,#70445,
#70446,#70447,#70448,#70449,#70450,#70451,#70452,#70453,#70454,#70455,#70456,
#70457,#70458,#70459,#70460,#70461,#70462,#70463,#70464,#70465,#70466,#70467,
#70468,#70469,#70470,#70471,#70472,#70473,#70474,#70475,#70476,#70477,#70478,
#70479,#70480,#70481,#70482,#70483,#70484,#70485,#70486,#70487,#70488,#70489,
#70490,#70491,#70492,#70493,#70494,#70495,#70496,#70497,#70498,#70499,#70500,
#70501,#70502,#70503,#70504,#70505,#70506,#70507,#70508,#70509,#70510,#70511,
#70512,#70513,#70514,#70515),(#70516,#70517,#70518,#70519,#70520,#70521,
#70522,#70523,#70524,#70525,#70526,#70527,#70528,#70529,#70530,#70531,#70532,
#70533,#70534,#70535,#70536,#70537,#70538,#70539,#70540,#70541,#70542,#70543,
#70544,#70545,#70546,#70547,#70548,#70549,#70550,#70551,#70552,#70553,#70554,
#70555,#70556,#70557,#70558,#70559,#70560,#70561,#70562,#70563,#70564,#70565,
#70566,#70567,#70568,#70569,#70570,#70571,#70572,#70573,#70574,#70575,#70576,
#70577,#70578,#70579,#70580,#70581,#70582,#70583,#70584,#70585,#70586,#70587,
#70588,#70589,#70590,#70591,#70592,#70593,#70594,#70595,#70596,#70597,#70598,
#70599,#70600,#70601,#70602,#70603,#70604,#70605,#70606,#70607,#70608,#70609,
#70610,#70611,#70612),(#70613,#70614,#70615,#70616,#70617,#70618,#70619,
#70620,#70621,#70622,#70623,#70624,#70625,#70626,#70627,#70628,#70629,#70630,
#70631,#70632,#70633,#70634,#70635,#70636,#70637,#70638,#70639,#70640,#70641,
#70642,#70643,#70644,#70645,#70646,#70647,#70648,#70649,#70650,#70651,#70652,
#70653,#70654,#70655,#70656,#70657,#70658,#70659,#70660,#70661,#70662,#70663,
#70664,#70665,#70666,#70667,#70668,#70669,#70670,#70671,#70672,#70673,#70674,
#70675,#70676,#70677,#70678,#70679,#70680,#70681,#70682,#70683,#70684,#70685,
#70686,#70687,#70688,#70689,#70690,#70691,#70692,#70693,#70694,#70695,#70696,
#70697,#70698,#70699,#70700,#70701,#70702,#70703,#70704,#70705,#70706,#70707,
#70708,#70709)),.UNSPECIFIED.,.F.,.F.,.F.,(4,4),(4,1,1,1,1,1,1,1,1,1,1,
1,1,1,1,1,1,1,1,1,1,1,1,1,1,1,1,1,1,1,1,1,1,1,1,1,1,1,1,1,1,1,1,1,1,1,1,
1,1,1,1,1,1,1,1,1,1,1,1,1,1,1,1,1,1,1,1,1,1,1,1,1,1,1,1,1,1,1,1,1,1,1,1,
1,1,1,1,1,1,1,1,1,1,1,4),(-0.000437088768894676,0.0818785329593794),(11.6517262692733,
12.6446908720042,13.6371660092234,14.6296411464425,15.6221162836617,16.6145914208809,
17.6070665581,18.5995416953192,19.5920168325384,20.5844919697575,21.5769671069767,
22.5694422441959,23.5619173814151,24.5543925186342,25.5468676558534,26.5393427930726,
27.5318179302917,28.5242930675109,29.5167682047301,30.5092433419492,31.5017184791684,
32.4941936163876,33.4866687536067,34.4791438908259,35.4716190280451,36.4640941652642,
37.4565693024834,38.4490444397026,39.4415195769218,40.4339947141409,41.4264698513601,
42.4189449885793,43.4114201257984,44.4038952630176,45.3963704002368,46.3888455374559,
47.3813206746751,48.3737958118943,49.3662709491134,50.3587460863326,51.3512212235518,
52.3436963607709,53.3361714979901,54.3286466352093,55.3211217724285,56.3135969096476,
57.3060720468668,58.298547184086,59.2910223213051,60.2834974585243,61.2759725957435,
62.2684477329626,63.2609228701818,64.253398007401,65.2458731446201,66.2383482818393,
67.2308234190585,68.2232985562776,69.2157736934968,70.208248830716,71.2007239679351,
72.1931991051543,73.1856742423735,74.1781493795927,75.1706245168118,76.163099654031,
77.1555747912502,78.1480499284693,79.1405250656885,80.1330002029077,81.1254753401268,
82.117950477346,83.1104256145652,84.1029007517843,85.0953758890035,86.0878510262227,
87.0803261634419,88.072801300661,89.0652764378802,90.0577515750994,91.0502267123185,
92.0427018495377,93.0351769867569,94.027652123976,95.0201272611952,96.0126023984144,
97.0050775356335,97.9975526728527,98.9900278100719,99.982502947291,100.97497808451,
101.967453221729,102.959928358949,103.952403496168,104.944878633387),
 .UNSPECIFIED.);
#1012=SPHERICAL_SURFACE('',#14112,1.190625);
#1013=SHAPE_REPRESENTATION_RELATIONSHIP('SRR','None',#72017,#1023);
#1014=SHAPE_REPRESENTATION_RELATIONSHIP('SRR','None',#72018,#1024);
#1015=SHAPE_REPRESENTATION_RELATIONSHIP('SRR','None',#72019,#1025);
#1016=SHAPE_REPRESENTATION_RELATIONSHIP('SRR','None',#72020,#1026);
#1017=SHAPE_REPRESENTATION_RELATIONSHIP('SRR','None',#72021,#1027);
#1018=SHAPE_REPRESENTATION_RELATIONSHIP('SRR','None',#72022,#1028);
#1019=SHAPE_REPRESENTATION_RELATIONSHIP('SRR','None',#72023,#1029);
#1020=SHAPE_REPRESENTATION_RELATIONSHIP('SRR','None',#72024,#1030);
#1021=SHAPE_REPRESENTATION_RELATIONSHIP('SRR','None',#72025,#1031);
#1022=SHAPE_REPRESENTATION_RELATIONSHIP('SRR','None',#72026,#1032);
#1023=ADVANCED_BREP_SHAPE_REPRESENTATION('',(#1043),#71785);
#1024=ADVANCED_BREP_SHAPE_REPRESENTATION('',(#1044),#71786);
#1025=ADVANCED_BREP_SHAPE_REPRESENTATION('',(#1045),#71787);
#1026=ADVANCED_BREP_SHAPE_REPRESENTATION('',(#1046),#71788);
#1027=ADVANCED_BREP_SHAPE_REPRESENTATION('',(#1047),#71789);
#1028=ADVANCED_BREP_SHAPE_REPRESENTATION('',(#1048),#71790);
#1029=ADVANCED_BREP_SHAPE_REPRESENTATION('',(#1049),#71791);
#1030=ADVANCED_BREP_SHAPE_REPRESENTATION('',(#1050),#71792);
#1031=ADVANCED_BREP_SHAPE_REPRESENTATION('',(#1051),#71793);
#1032=ADVANCED_BREP_SHAPE_REPRESENTATION('',(#1052),#71794);
#1033=STYLED_ITEM('',(#72076),#1043);
#1034=STYLED_ITEM('',(#72077),#1044);
#1035=STYLED_ITEM('',(#72078),#1045);
#1036=STYLED_ITEM('',(#72079),#1046);
#1037=STYLED_ITEM('',(#72080),#1047);
#1038=STYLED_ITEM('',(#72081),#1048);
#1039=STYLED_ITEM('',(#72082),#1049);
#1040=STYLED_ITEM('',(#72083),#1050);
#1041=STYLED_ITEM('',(#72084),#1051);
#1042=STYLED_ITEM('',(#72085),#1052);
#1043=MANIFOLD_SOLID_BREP('Body1',#13635);
#1044=MANIFOLD_SOLID_BREP('Body1',#13636);
#1045=MANIFOLD_SOLID_BREP('Body1',#13637);
#1046=MANIFOLD_SOLID_BREP('Body1',#13638);
#1047=MANIFOLD_SOLID_BREP('Body1',#13639);
#1048=MANIFOLD_SOLID_BREP('Body1',#13640);
#1049=MANIFOLD_SOLID_BREP('Body1',#13641);
#1050=MANIFOLD_SOLID_BREP('Body1',#13642);
#1051=MANIFOLD_SOLID_BREP('Body1',#13643);
#1052=MANIFOLD_SOLID_BREP('Body1',#13644);
#1053=CONICAL_SURFACE('',#13794,5.5,0.785398163397437);
#1054=CONICAL_SURFACE('',#13803,5.5,0.785398163397452);
#1055=CONICAL_SURFACE('',#13807,5.5,0.785398163397452);
#1056=CONICAL_SURFACE('',#13811,5.5,0.785398163397437);
#1057=CONICAL_SURFACE('',#13855,4.40000000000001,0.785398163397447);
#1058=CONICAL_SURFACE('',#13874,4.4,0.785398163397434);
#1059=CONICAL_SURFACE('',#13878,4.4,0.78539816339744);
#1060=CONICAL_SURFACE('',#13880,4.4,0.785398163397448);
#1061=CONICAL_SURFACE('',#13884,4.4,0.78539816339744);
#1062=CONICAL_SURFACE('',#13886,4.4,0.785398163397448);
#1063=CONICAL_SURFACE('',#13890,4.4,0.785398163397434);
#1064=CONICAL_SURFACE('',#13894,4.40000000000001,0.785398163397447);
#1065=CONICAL_SURFACE('',#13924,3.42499999999999,0.785398163397437);
#1066=CONICAL_SURFACE('',#13927,3.425,0.785398163397448);
#1067=CONICAL_SURFACE('',#13930,3.425,0.785398163397448);
#1068=CONICAL_SURFACE('',#13933,3.42499999999999,0.785398163397437);
#1069=CONICAL_SURFACE('',#13952,3.42499999999999,0.785398163397437);
#1070=CONICAL_SURFACE('',#13956,3.425,0.785398163397448);
#1071=CONICAL_SURFACE('',#13968,3.425,0.785398163397448);
#1072=CONICAL_SURFACE('',#13972,3.42499999999999,0.785398163397437);
#1073=CONICAL_SURFACE('',#13976,3.225,1.02974425867665);
#1074=CONICAL_SURFACE('',#13977,3.225,1.02974425867665);
#1075=CONICAL_SURFACE('',#13978,3.225,1.02974425867665);
#1076=CONICAL_SURFACE('',#13979,3.225,1.02974425867665);
#1077=CONICAL_SURFACE('',#13980,3.22499999999998,1.02974425867665);
#1078=CONICAL_SURFACE('',#13981,3.22499999999998,1.02974425867665);
#1079=CONICAL_SURFACE('',#13982,3.225,1.02974425867665);
#1080=CONICAL_SURFACE('',#13983,3.225,1.02974425867665);
#1081=CONICAL_SURFACE('',#13996,2.464,1.02395598729616);
#1082=CONICAL_SURFACE('',#13999,2.464,1.02395598729616);
#1083=CONICAL_SURFACE('',#14002,2.464,1.02395598729616);
#1084=CONICAL_SURFACE('',#14005,6.1,0.785398163397447);
#1085=CONICAL_SURFACE('',#14009,6.1,0.785398163397439);
#1086=CONICAL_SURFACE('',#14013,2.61400000000001,0.785398163397456);
#1087=CONICAL_SURFACE('',#14021,2.61400000000001,0.785398163397456);
#1088=CONICAL_SURFACE('',#14026,2.464,1.02974425867666);
#1089=CONICAL_SURFACE('',#14030,2.464,1.02974425867665);
#1090=CONICAL_SURFACE('',#14031,11.3,0.785398163397451);
#1091=CONICAL_SURFACE('',#14035,11.3,0.785398163397451);
#1092=CONICAL_SURFACE('',#14048,10.9,0.785398163397437);
#1093=CONICAL_SURFACE('',#14057,10.9,0.785398163397448);
#1094=CONICAL_SURFACE('',#14151,2.16347,0.785398163397448);
#1095=CONICAL_SURFACE('',#14158,3.7624,0.785398163397448);
#1096=CONICAL_SURFACE('',#14351,2.29135888084632,1.02974425867665);
#1097=CONICAL_SURFACE('',#14403,2.16347,0.785398163397448);
#1098=CONICAL_SURFACE('',#14410,3.7624,0.785398163397448);
#1099=CONICAL_SURFACE('',#14603,1.14567944042316,1.02974425867665);
#1100=CONICAL_SURFACE('',#14642,2.91023,0.785398163397448);
#1101=CONICAL_SURFACE('',#14649,4.5625,0.785398163397448);
#1102=CONICAL_SURFACE('',#14842,2.74963065701559,1.02974425867665);
#1103=B_SPLINE_CURVE_WITH_KNOTS('',3,(#18543,#18544,#18545,#18546,#18547,
#18548,#18549,#18550,#18551,#18552,#18553,#18554,#18555,#18556,#18557,#18558,
#18559,#18560),.UNSPECIFIED.,.F.,.F.,(4,2,2,2,2,2,2,2,4),(-1.58749465662543,
-1.48822066272646,-1.3889466688275,-1.28978383064828,-1.19062099246907,
-1.09145815428986,-0.992295316110649,-0.893021322211684,-0.793747328312718),
 .UNSPECIFIED.);
#1104=B_SPLINE_CURVE_WITH_KNOTS('',3,(#18561,#18562,#18563,#18564,#18565,
#18566,#18567,#18568,#18569,#18570,#18571,#18572,#18573,#18574,#18575,#18576,
#18577,#18578),.UNSPECIFIED.,.F.,.F.,(4,2,2,2,2,2,2,2,4),(-0.793747328312718,
-0.694473334413751,-0.595199340514785,-0.496036502335572,-0.39687366415636,
-0.297710825977147,-0.198547987797934,-0.0992739938989668,0.),
 .UNSPECIFIED.);
#1105=B_SPLINE_CURVE_WITH_KNOTS('',3,(#18592,#18593,#18594,#18595,#18596,
#18597,#18598,#18599,#18600,#18601,#18602,#18603,#18604,#18605,#18606,#18607,
#18608,#18609),.UNSPECIFIED.,.F.,.F.,(4,2,2,2,2,2,2,2,4),(-1.58749465662543,
-1.48822066272646,-1.38894666882749,-1.28978383064828,-1.19062099246907,
-1.09145815428986,-0.992295316110645,-0.893021322211679,-0.793747328312713),
 .UNSPECIFIED.);
#1106=B_SPLINE_CURVE_WITH_KNOTS('',3,(#18610,#18611,#18612,#18613,#18614,
#18615,#18616,#18617,#18618,#18619,#18620,#18621,#18622,#18623,#18624,#18625,
#18626,#18627),.UNSPECIFIED.,.F.,.F.,(4,2,2,2,2,2,2,2,4),(-0.793747328312713,
-0.694473334413747,-0.595199340514781,-0.496036502335569,-0.396873664156357,
-0.297710825977144,-0.198547987797932,-0.0992739938989662,0.),
 .UNSPECIFIED.);
#1107=B_SPLINE_CURVE_WITH_KNOTS('',3,(#18641,#18642,#18643,#18644,#18645,
#18646,#18647,#18648,#18649,#18650,#18651,#18652,#18653,#18654,#18655,#18656,
#18657,#18658),.UNSPECIFIED.,.F.,.F.,(4,2,2,2,2,2,2,2,4),(-1.58749465662542,
-1.48822066272646,-1.38894666882749,-1.28978383064828,-1.19062099246907,
-1.09145815428986,-0.992295316110644,-0.893021322211679,-0.793747328312713),
 .UNSPECIFIED.);
#1108=B_SPLINE_CURVE_WITH_KNOTS('',3,(#18659,#18660,#18661,#18662,#18663,
#18664,#18665,#18666,#18667,#18668,#18669,#18670,#18671,#18672,#18673,#18674,
#18675,#18676),.UNSPECIFIED.,.F.,.F.,(4,2,2,2,2,2,2,2,4),(-0.793747328312713,
-0.694473334413747,-0.595199340514781,-0.496036502335569,-0.396873664156357,
-0.297710825977144,-0.198547987797932,-0.099273993898966,0.),
 .UNSPECIFIED.);
#1109=B_SPLINE_CURVE_WITH_KNOTS('',3,(#18690,#18691,#18692,#18693,#18694,
#18695,#18696,#18697,#18698,#18699,#18700,#18701,#18702,#18703,#18704,#18705,
#18706,#18707),.UNSPECIFIED.,.F.,.F.,(4,2,2,2,2,2,2,2,4),(-1.58749465662543,
-1.48822066272646,-1.3889466688275,-1.28978383064828,-1.19062099246907,
-1.09145815428986,-0.992295316110649,-0.893021322211684,-0.793747328312718),
 .UNSPECIFIED.);
#1110=B_SPLINE_CURVE_WITH_KNOTS('',3,(#18708,#18709,#18710,#18711,#18712,
#18713,#18714,#18715,#18716,#18717,#18718,#18719,#18720,#18721,#18722,#18723,
#18724,#18725),.UNSPECIFIED.,.F.,.F.,(4,2,2,2,2,2,2,2,4),(-0.793747328312718,
-0.694473334413751,-0.595199340514785,-0.496036502335572,-0.396873664156359,
-0.297710825977146,-0.198547987797934,-0.0992739938989669,0.),
 .UNSPECIFIED.);
#1111=B_SPLINE_CURVE_WITH_KNOTS('',3,(#18739,#18740,#18741,#18742,#18743,
#18744,#18745,#18746,#18747,#18748,#18749,#18750,#18751,#18752,#18753,#18754,
#18755,#18756),.UNSPECIFIED.,.F.,.F.,(4,2,2,2,2,2,2,2,4),(-1.58749465662543,
-1.48822066272646,-1.38894666882749,-1.28978383064828,-1.19062099246907,
-1.09145815428986,-0.992295316110645,-0.893021322211679,-0.793747328312713),
 .UNSPECIFIED.);
#1112=B_SPLINE_CURVE_WITH_KNOTS('',3,(#18757,#18758,#18759,#18760,#18761,
#18762,#18763,#18764,#18765,#18766,#18767,#18768,#18769,#18770,#18771,#18772,
#18773,#18774),.UNSPECIFIED.,.F.,.F.,(4,2,2,2,2,2,2,2,4),(-0.793747328312713,
-0.694473334413747,-0.595199340514781,-0.496036502335568,-0.396873664156356,
-0.297710825977144,-0.198547987797932,-0.099273993898966,0.),
 .UNSPECIFIED.);
#1113=B_SPLINE_CURVE_WITH_KNOTS('',3,(#18788,#18789,#18790,#18791,#18792,
#18793,#18794,#18795,#18796,#18797,#18798,#18799,#18800,#18801,#18802,#18803,
#18804,#18805),.UNSPECIFIED.,.F.,.F.,(4,2,2,2,2,2,2,2,4),(-1.58749465662543,
-1.48822066272646,-1.38894666882749,-1.28978383064828,-1.19062099246907,
-1.09145815428986,-0.992295316110644,-0.893021322211679,-0.793747328312713),
 .UNSPECIFIED.);
#1114=B_SPLINE_CURVE_WITH_KNOTS('',3,(#18806,#18807,#18808,#18809,#18810,
#18811,#18812,#18813,#18814,#18815,#18816,#18817,#18818,#18819,#18820,#18821,
#18822,#18823),.UNSPECIFIED.,.F.,.F.,(4,2,2,2,2,2,2,2,4),(-0.793747328312713,
-0.694473334413747,-0.595199340514781,-0.496036502335569,-0.396873664156356,
-0.297710825977144,-0.198547987797932,-0.0992739938989659,0.),
 .UNSPECIFIED.);
#1115=B_SPLINE_CURVE_WITH_KNOTS('',3,(#19006,#19007,#19008,#19009,#19010,
#19011),.UNSPECIFIED.,.F.,.F.,(4,2,4),(2.00778188532846,2.05631559190232,
2.12443391712942),.UNSPECIFIED.);
#1116=B_SPLINE_CURVE_WITH_KNOTS('',3,(#19015,#19016,#19017,#19018,#19019,
#19020),.UNSPECIFIED.,.F.,.F.,(4,2,4),(1.74660138399546,1.81470102727558,
1.86325481657749),.UNSPECIFIED.);
#1117=B_SPLINE_CURVE_WITH_KNOTS('',3,(#19070,#19071,#19072,#19073,#19074,
#19075),.UNSPECIFIED.,.F.,.F.,(4,2,4),(2.00778188532849,2.05631559190233,
2.1244339171294),.UNSPECIFIED.);
#1118=B_SPLINE_CURVE_WITH_KNOTS('',3,(#19077,#19078,#19079,#19080,#19081,
#19082),.UNSPECIFIED.,.F.,.F.,(4,2,4),(1.74660138399545,1.81470102727557,
1.86325481657748),.UNSPECIFIED.);
#1119=B_SPLINE_CURVE_WITH_KNOTS('',3,(#19094,#19095,#19096,#19097,#19098,
#19099),.UNSPECIFIED.,.F.,.F.,(4,2,4),(2.00778188532849,2.05631559190233,
2.12443391712941),.UNSPECIFIED.);
#1120=B_SPLINE_CURVE_WITH_KNOTS('',3,(#19101,#19102,#19103,#19104,#19105,
#19106),.UNSPECIFIED.,.F.,.F.,(4,2,4),(1.74660138399546,1.81470102727557,
1.86325481657748),.UNSPECIFIED.);
#1121=B_SPLINE_CURVE_WITH_KNOTS('',3,(#19126,#19127,#19128,#19129,#19130,
#19131),.UNSPECIFIED.,.F.,.F.,(4,2,4),(2.00778188532849,2.05631559190232,
2.1244339171294),.UNSPECIFIED.);
#1122=B_SPLINE_CURVE_WITH_KNOTS('',3,(#19133,#19134,#19135,#19136,#19137,
#19138),.UNSPECIFIED.,.F.,.F.,(4,2,4),(1.74660138399543,1.81470102727559,
1.86325481657752),.UNSPECIFIED.);
#1123=B_SPLINE_CURVE_WITH_KNOTS('',3,(#19142,#19143,#19144,#19145),
 .UNSPECIFIED.,.F.,.F.,(4,4),(-0.456883774528942,-0.419587727931792),
 .UNSPECIFIED.);
#1124=B_SPLINE_CURVE_WITH_KNOTS('',3,(#19152,#19153,#19154,#19155),
 .UNSPECIFIED.,.F.,.F.,(4,4),(-0.557381628443529,-0.520085581846348),
 .UNSPECIFIED.);
#1125=B_SPLINE_CURVE_WITH_KNOTS('',3,(#19168,#19169,#19170,#19171),
 .UNSPECIFIED.,.F.,.F.,(4,4),(-0.456883774528974,-0.419587727931764),
 .UNSPECIFIED.);
#1126=B_SPLINE_CURVE_WITH_KNOTS('',3,(#19178,#19179,#19180,#19181),
 .UNSPECIFIED.,.F.,.F.,(4,4),(-0.557381628443525,-0.520085581846325),
 .UNSPECIFIED.);
#1127=B_SPLINE_CURVE_WITH_KNOTS('',3,(#19191,#19192,#19193,#19194),
 .UNSPECIFIED.,.F.,.F.,(4,4),(-0.456883774528968,-0.419587727931769),
 .UNSPECIFIED.);
#1128=B_SPLINE_CURVE_WITH_KNOTS('',3,(#19201,#19202,#19203,#19204),
 .UNSPECIFIED.,.F.,.F.,(4,4),(-0.557381628443528,-0.52008558184632),
 .UNSPECIFIED.);
#1129=B_SPLINE_CURVE_WITH_KNOTS('',3,(#19214,#19215,#19216,#19217),
 .UNSPECIFIED.,.F.,.F.,(4,4),(-0.456883774528947,-0.419587727931763),
 .UNSPECIFIED.);
#1130=B_SPLINE_CURVE_WITH_KNOTS('',3,(#19224,#19225,#19226,#19227),
 .UNSPECIFIED.,.F.,.F.,(4,4),(-0.557381628443516,-0.520085581846359),
 .UNSPECIFIED.);
#1131=B_SPLINE_CURVE_WITH_KNOTS('',3,(#19389,#19390,#19391,#19392,#19393,
#19394,#19395,#19396,#19397,#19398,#19399,#19400,#19401,#19402,#19403,#19404,
#19405,#19406),.UNSPECIFIED.,.F.,.F.,(4,2,2,2,2,2,2,2,4),(0.,0.0939363144605702,
0.18787262892114,0.281725618013245,0.37557860710535,0.469431596197455,0.563284585289559,
0.657220899750131,0.751157214210703),.UNSPECIFIED.);
#1132=B_SPLINE_CURVE_WITH_KNOTS('',3,(#19407,#19408,#19409,#19410,#19411,
#19412,#19413,#19414,#19415,#19416,#19417,#19418,#19419,#19420,#19421,#19422,
#19423,#19424),.UNSPECIFIED.,.F.,.F.,(4,2,2,2,2,2,2,2,4),(0.751157214210703,
0.845093528671274,0.939029843131846,1.03288283222395,1.12673582131605,1.22058881040816,
1.31444179950026,1.40837811396083,1.50231442842141),.UNSPECIFIED.);
#1133=B_SPLINE_CURVE_WITH_KNOTS('',3,(#19434,#19435,#19436,#19437,#19438,
#19439,#19440,#19441,#19442,#19443,#19444,#19445,#19446,#19447,#19448,#19449,
#19450,#19451),.UNSPECIFIED.,.F.,.F.,(4,2,2,2,2,2,2,2,4),(0.,0.0939363144605709,
0.187872628921142,0.281725618013246,0.375578607105351,0.469431596197456,
0.56328458528956,0.657220899750131,0.751157214210702),.UNSPECIFIED.);
#1134=B_SPLINE_CURVE_WITH_KNOTS('',3,(#19452,#19453,#19454,#19455,#19456,
#19457,#19458,#19459,#19460,#19461,#19462,#19463,#19464,#19465,#19466,#19467,
#19468,#19469),.UNSPECIFIED.,.F.,.F.,(4,2,2,2,2,2,2,2,4),(0.751157214210702,
0.845093528671273,0.939029843131844,1.03288283222395,1.12673582131605,1.22058881040816,
1.31444179950026,1.40837811396083,1.5023144284214),.UNSPECIFIED.);
#1135=B_SPLINE_CURVE_WITH_KNOTS('',3,(#19479,#19480,#19481,#19482,#19483,
#19484,#19485,#19486,#19487,#19488,#19489,#19490,#19491,#19492,#19493,#19494,
#19495,#19496),.UNSPECIFIED.,.F.,.F.,(4,2,2,2,2,2,2,2,4),(0.,0.0939363144605713,
0.187872628921143,0.281725618013247,0.375578607105351,0.469431596197456,
0.56328458528956,0.657220899750132,0.751157214210703),.UNSPECIFIED.);
#1136=B_SPLINE_CURVE_WITH_KNOTS('',3,(#19497,#19498,#19499,#19500,#19501,
#19502,#19503,#19504,#19505,#19506,#19507,#19508,#19509,#19510,#19511,#19512,
#19513,#19514),.UNSPECIFIED.,.F.,.F.,(4,2,2,2,2,2,2,2,4),(0.751157214210703,
0.845093528671273,0.939029843131844,1.03288283222395,1.12673582131605,1.22058881040816,
1.31444179950026,1.40837811396083,1.5023144284214),.UNSPECIFIED.);
#1137=B_SPLINE_CURVE_WITH_KNOTS('',3,(#19561,#19562,#19563,#19564,#19565,
#19566,#19567,#19568,#19569,#19570,#19571,#19572,#19573,#19574),
 .UNSPECIFIED.,.F.,.F.,(4,2,2,2,2,2,4),(-1.14599907215265,-1.14082829651813,
-1.08169405294193,-1.02255980936573,-0.963425565789533,-0.904291322213332,
-0.899120546578817),.UNSPECIFIED.);
#1138=B_SPLINE_CURVE_WITH_KNOTS('',3,(#19586,#19587,#19588,#19589,#19590,
#19591,#19592,#19593,#19594,#19595,#19596,#19597,#19598,#19599),
 .UNSPECIFIED.,.F.,.F.,(4,2,2,2,2,2,4),(-1.14599907215265,-1.14082829651813,
-1.08169405294193,-1.02255980936573,-0.963425565789533,-0.904291322213332,
-0.899120546578816),.UNSPECIFIED.);
#1139=B_SPLINE_CURVE_WITH_KNOTS('',3,(#19604,#19605,#19606,#19607,#19608,
#19609,#19610,#19611,#19612,#19613,#19614,#19615,#19616,#19617),
 .UNSPECIFIED.,.F.,.F.,(4,2,2,2,2,2,4),(-0.440637337632516,-0.41817718819756,
-0.36956984330978,-0.309581883490714,-0.249593923671647,-0.200986578783867,
-0.178526429348912),.UNSPECIFIED.);
#1140=B_SPLINE_CURVE_WITH_KNOTS('',3,(#19627,#19628,#19629,#19630,#19631,
#19632,#19633,#19634,#19635,#19636,#19637,#19638,#19639,#19640),
 .UNSPECIFIED.,.F.,.F.,(4,2,2,2,2,2,4),(0.787224364416541,0.851680919549612,
0.89358137447704,0.935481829404467,0.977382284331895,1.01928273925932,1.08373929439239),
 .UNSPECIFIED.);
#1141=B_SPLINE_CURVE_WITH_KNOTS('',3,(#19897,#19898,#19899,#19900,#19901,
#19902,#19903,#19904,#19905,#19906,#19907,#19908,#19909,#19910,#19911,#19912,
#19913,#19914,#19915,#19916,#19917,#19918,#19919,#19920,#19921,#19922,#19923,
#19924,#19925,#19926,#19927,#19928,#19929,#19930,#19931,#19932,#19933,#19934,
#19935,#19936,#19937,#19938,#19939,#19940,#19941,#19942,#19943,#19944,#19945,
#19946,#19947,#19948,#19949,#19950,#19951,#19952,#19953,#19954,#19955,#19956,
#19957,#19958,#19959,#19960,#19961,#19962,#19963,#19964,#19965,#19966,#19967,
#19968,#19969,#19970,#19971,#19972,#19973,#19974,#19975,#19976,#19977,#19978,
#19979,#19980,#19981,#19982,#19983,#19984,#19985,#19986,#19987,#19988,#19989,
#19990,#19991,#19992,#19993,#19994,#19995,#19996,#19997,#19998,#19999,#20000,
#20001,#20002,#20003,#20004,#20005,#20006,#20007,#20008,#20009,#20010,#20011,
#20012,#20013,#20014,#20015,#20016,#20017,#20018,#20019,#20020,#20021,#20022,
#20023,#20024,#20025,#20026),.UNSPECIFIED.,.F.,.F.,(4,3,3,3,3,3,3,3,3,3,
3,3,3,3,3,3,3,3,3,3,3,3,3,3,3,3,3,3,3,3,3,3,3,3,3,3,3,3,3,3,3,3,3,4),(10.3186182874638,
10.3319577878375,10.4378652798471,10.5436115957539,10.6492313119882,10.754783484694,
10.8603044745869,10.9658305963425,11.0714672342109,11.1771663451116,11.2830457101334,
11.3311385501333,11.4371331467285,11.5429710322994,11.648688489881,11.7543421829616,
11.8599683212614,11.9656030723555,12.071352874328,12.1771679068059,12.2831662388787,
12.3303193124291,12.4360258213461,12.5415702665319,12.6469878201331,12.7523377706301,
12.8576567942629,12.9629815213307,13.0684190300506,13.1739200138675,13.2796048951218,
13.3295000747249,13.4353384967336,13.5410165329372,13.6465695041155,13.7520559304393,
13.8575122821743,13.9629749846754,14.0685505048566,14.1741897271739,14.2800117420941,
14.3286808370206,14.4345182698765,14.4571413871433),.UNSPECIFIED.);
#1142=B_SPLINE_CURVE_WITH_KNOTS('',3,(#20029,#20030,#20031,#20032,#20033,
#20034,#20035,#20036,#20037,#20038,#20039,#20040,#20041,#20042,#20043,#20044,
#20045,#20046,#20047,#20048,#20049,#20050,#20051,#20052,#20053,#20054,#20055,
#20056,#20057,#20058,#20059,#20060,#20061,#20062,#20063,#20064,#20065,#20066,
#20067,#20068,#20069,#20070,#20071,#20072,#20073,#20074,#20075,#20076,#20077,
#20078,#20079,#20080,#20081,#20082,#20083,#20084,#20085,#20086,#20087,#20088,
#20089,#20090,#20091,#20092,#20093,#20094,#20095,#20096,#20097,#20098,#20099,
#20100,#20101,#20102,#20103,#20104,#20105,#20106,#20107,#20108,#20109,#20110,
#20111,#20112,#20113),.UNSPECIFIED.,.F.,.F.,(4,3,3,3,3,3,3,3,3,3,3,3,3,
3,3,3,3,3,3,3,3,3,3,3,3,3,3,3,4),(11.6725302876644,11.7807318723834,11.8921042695805,
12.0002215149502,12.1083396087937,12.2164883956815,12.3302940592512,12.4386767884211,
12.5471600419772,12.6558426310807,12.6717110499602,12.7765953511984,12.8813042105095,
12.9858701824119,13.0903589546267,13.1948083587627,13.2992561685555,13.4038114660646,
13.5084257386862,13.6132263099785,13.670891812256,13.776767494232,13.8824961979185,
13.988114518063,14.0936589161058,14.1991952494382,14.3047263271779,14.4103355213707,
14.4560074704634),.UNSPECIFIED.);
#1143=B_SPLINE_CURVE_WITH_KNOTS('',3,(#20119,#20120,#20121,#20122,#20123,
#20124,#20125,#20126,#20127,#20128,#20129,#20130,#20131,#20132,#20133,#20134,
#20135,#20136,#20137,#20138,#20139,#20140,#20141,#20142,#20143,#20144,#20145,
#20146,#20147,#20148,#20149,#20150,#20151,#20152,#20153,#20154,#20155,#20156,
#20157,#20158,#20159,#20160,#20161,#20162,#20163,#20164,#20165,#20166,#20167,
#20168,#20169,#20170,#20171,#20172,#20173,#20174,#20175,#20176,#20177,#20178,
#20179,#20180,#20181,#20182,#20183,#20184,#20185,#20186,#20187,#20188,#20189,
#20190,#20191,#20192,#20193,#20194,#20195,#20196,#20197,#20198,#20199,#20200,
#20201,#20202,#20203,#20204,#20205,#20206,#20207,#20208,#20209,#20210,#20211,
#20212,#20213,#20214,#20215,#20216,#20217,#20218,#20219,#20220,#20221,#20222,
#20223,#20224,#20225,#20226,#20227,#20228,#20229,#20230,#20231,#20232,#20233,
#20234,#20235,#20236,#20237,#20238,#20239,#20240,#20241,#20242,#20243,#20244,
#20245,#20246,#20247,#20248,#20249,#20250,#20251,#20252,#20253,#20254,#20255,
#20256,#20257,#20258,#20259,#20260,#20261,#20262,#20263,#20264,#20265,#20266,
#20267,#20268,#20269,#20270,#20271,#20272,#20273,#20274,#20275,#20276,#20277,
#20278,#20279,#20280,#20281,#20282,#20283,#20284,#20285,#20286,#20287,#20288,
#20289,#20290,#20291,#20292),.UNSPECIFIED.,.F.,.F.,(4,2,2,2,2,2,2,2,2,2,
2,2,2,2,2,2,2,2,2,2,2,2,2,2,2,2,2,2,2,2,2,2,2,2,2,2,2,2,2,2,2,2,2,2,2,2,
2,2,2,2,2,2,2,2,2,2,2,2,2,2,2,2,2,2,2,2,2,2,2,2,2,2,2,2,2,2,2,2,2,2,2,2,
2,2,2,2,4),(-0.973925068013576,-0.950916583618217,-0.905493200642175,-0.897753475521733,
-0.895184606050773,-0.893569427576055,-0.892024446877122,-0.889786345933224,
-0.883889448500355,-0.874927077808174,-0.842219678413613,-0.80692732268821,
-0.801784811841754,-0.798469610807626,-0.795803022878436,-0.792756597718315,
-0.787481654381162,-0.762329534815237,-0.729121193154261,-0.706165152782175,
-0.703027155427136,-0.701098928412001,-0.699600423889519,-0.697838800859491,
-0.694600828591246,-0.675779806694615,-0.637626900347504,-0.613177506659964,
-0.607819097580816,-0.60472347344611,-0.602061397413686,-0.598812124107507,
-0.592573771645881,-0.584649060931421,-0.566096074873262,-0.551753034556585,
-0.5150749684563,-0.510296877551879,-0.508385065260786,-0.506986508852542,
-0.505420267177212,-0.503076841056701,-0.496430331527037,-0.485859790756768,
-0.457667412673531,-0.420400942771593,-0.415279877300816,-0.411971173955281,
-0.409305076770745,-0.406254041491245,-0.400957798416744,-0.375375298975841,
-0.340102743761475,-0.31963218995123,-0.316521775388175,-0.314601626586024,
-0.31310330189229,-0.311334476348705,-0.30806554049338,-0.28842640564689,
-0.249316487113877,-0.226588624374065,-0.221307279244302,-0.218228385153227,
-0.21561712082627,-0.212448536261234,-0.209019416422941,-0.203577302512313,
-0.192881957982826,-0.14201590139986,-0.126040406731366,-0.122827049071309,
-0.121050717977937,-0.119554140856589,-0.11764657635809,-0.1136902832442,
-0.108401372273103,-0.0949827972572126,-0.0528096305379754,-0.0343385982899319,
-0.0289664209109278,-0.0255832861349313,-0.0229122525890893,-0.0204127395629368,
-0.0174678607068047,-0.010814646247928,-0.000575867290469521),
 .UNSPECIFIED.);
#1144=B_SPLINE_CURVE_WITH_KNOTS('',3,(#20293,#20294,#20295,#20296,#20297,
#20298,#20299,#20300,#20301,#20302,#20303,#20304,#20305,#20306,#20307,#20308,
#20309,#20310,#20311,#20312,#20313,#20314,#20315,#20316,#20317,#20318,#20319,
#20320,#20321,#20322,#20323,#20324,#20325,#20326,#20327,#20328,#20329,#20330,
#20331,#20332),.UNSPECIFIED.,.F.,.F.,(4,3,3,3,3,3,3,3,3,3,3,3,3,4),(14.4571413871433,
14.5659814136649,14.6715168831504,14.7769950977482,14.8824525106465,14.9879255397584,
15.0935173624096,15.1991811965176,15.3050207279912,15.3278615993164,15.4471321116664,
15.5659385083076,15.6839855814566,15.7079632675659),.UNSPECIFIED.);
#1145=B_SPLINE_CURVE_WITH_KNOTS('',3,(#20334,#20335,#20336,#20337,#20338,
#20339,#20340,#20341,#20342,#20343,#20344,#20345,#20346,#20347,#20348,#20349,
#20350,#20351,#20352,#20353,#20354,#20355,#20356,#20357,#20358,#20359,#20360,
#20361,#20362,#20363,#20364,#20365,#20366,#20367,#20368,#20369,#20370,#20371,
#20372,#20373),.UNSPECIFIED.,.F.,.F.,(4,3,3,3,3,3,3,3,3,3,3,3,3,4),(14.4560074704634,
14.5630400225075,14.6700725745517,14.776067128075,14.8819049692828,14.9876223807981,
15.0932760267801,15.1989021170178,15.3045368191538,15.410286571138,15.516101552966,
15.6220998338911,15.6692533368475,15.7079632679489),.UNSPECIFIED.);
#1146=B_SPLINE_CURVE_WITH_KNOTS('',3,(#20374,#20375,#20376,#20377,#20378,
#20379,#20380,#20381,#20382,#20383,#20384,#20385,#20386,#20387,#20388,#20389,
#20390,#20391,#20392,#20393,#20394,#20395,#20396,#20397,#20398,#20399,#20400,
#20401,#20402,#20403,#20404,#20405,#20406,#20407,#20408,#20409,#20410,#20411,
#20412,#20413,#20414,#20415,#20416,#20417,#20418,#20419,#20420,#20421,#20422,
#20423,#20424,#20425,#20426,#20427,#20428,#20429,#20430,#20431,#20432,#20433,
#20434,#20435,#20436,#20437,#20438,#20439,#20440,#20441,#20442,#20443,#20444,
#20445,#20446,#20447,#20448,#20449,#20450,#20451,#20452,#20453,#20454,#20455,
#20456,#20457,#20458,#20459,#20460,#20461,#20462,#20463,#20464,#20465,#20466,
#20467,#20468,#20469,#20470,#20471,#20472,#20473,#20474,#20475,#20476,#20477,
#20478,#20479,#20480,#20481,#20482,#20483,#20484,#20485,#20486,#20487,#20488,
#20489,#20490,#20491,#20492,#20493,#20494,#20495,#20496,#20497,#20498,#20499,
#20500,#20501,#20502,#20503,#20504,#20505,#20506,#20507,#20508,#20509,#20510,
#20511,#20512,#20513,#20514,#20515,#20516,#20517,#20518,#20519,#20520,#20521,
#20522,#20523,#20524,#20525,#20526,#20527,#20528,#20529,#20530,#20531,#20532,
#20533,#20534,#20535,#20536,#20537,#20538,#20539),.UNSPECIFIED.,.F.,.F.,
(4,2,2,2,2,2,2,2,2,2,2,2,2,2,2,2,2,2,2,2,2,2,2,2,2,2,2,2,2,2,2,2,2,2,2,
2,2,2,2,2,2,2,2,2,2,2,2,2,2,2,2,2,2,2,2,2,2,2,2,2,2,2,2,2,2,2,2,2,2,2,2,
2,2,2,2,2,2,2,2,2,2,2,4),(-2.43116705121226,-2.41825989892644,-2.36647369053139,
-2.35025992321336,-2.34562825164978,-2.34273454470215,-2.34005815576854,
-2.33658646075185,-2.32921645052342,-2.28534566527498,-2.26134546291887,
-2.25375569118682,-2.25017789072549,-2.24805388258681,-2.24618226274905,
-2.24472486204046,-2.24301186541103,-2.24007475283859,-2.22836745627527,
-2.19337697260899,-2.15973673741926,-2.15336811601201,-2.15008944227208,
-2.1474220276589,-2.14434108462187,-2.13905971325778,-2.11612030814376,
-2.07729067609646,-2.05778653059882,-2.05451766121803,-2.05274638104333,
-2.05124590055494,-2.04932184647869,-2.04620004885552,-2.02420982710104,
-1.99028567529971,-1.96496510718384,-1.95968227813066,-1.95663415458968,
-1.95396775101269,-1.950654953851,-1.94552035833235,-1.91184399138432,-1.86899400398118,
-1.86267256093303,-1.86037399166691,-1.85881744581162,-1.85741247817496,
-1.85547181027022,-1.85051634624008,-1.81953336583791,-1.78728838944621,
-1.77055887209857,-1.76586406254956,-1.76294628005505,-1.76025770014692,
-1.7567840625937,-1.74918084795132,-1.70851212927825,-1.68626113499655,
-1.67598639338314,-1.66947598569715,-1.66715266223597,-1.6655918973548,
-1.66419090788137,-1.66226812624139,-1.65742240240225,-1.6225527739334,
-1.58006393991122,-1.57380637167895,-1.5705532897928,-1.56789115924466,
-1.56479892619132,-1.55945504565141,-1.53530213154841,-1.49693977941724,
-1.47801749424984,-1.47477535942088,-1.47301270248496,-1.47151445989363,
-1.46958783402063,-1.46645427813501,-1.45799448822835),.UNSPECIFIED.);
#1147=B_SPLINE_CURVE_WITH_KNOTS('',3,(#20544,#20545,#20546,#20547,#20548,
#20549,#20550,#20551,#20552,#20553,#20554,#20555,#20556,#20557,#20558,#20559,
#20560,#20561,#20562,#20563,#20564,#20565,#20566,#20567,#20568,#20569,#20570,
#20571,#20572,#20573,#20574,#20575,#20576,#20577,#20578,#20579,#20580,#20581,
#20582,#20583,#20584,#20585,#20586,#20587,#20588,#20589,#20590,#20591,#20592,
#20593,#20594,#20595,#20596,#20597,#20598,#20599,#20600,#20601,#20602,#20603,
#20604,#20605,#20606,#20607,#20608,#20609,#20610,#20611,#20612,#20613,#20614,
#20615,#20616,#20617,#20618,#20619,#20620,#20621,#20622,#20623,#20624,#20625,
#20626,#20627,#20628,#20629,#20630,#20631,#20632,#20633,#20634,#20635,#20636,
#20637,#20638,#20639,#20640,#20641,#20642,#20643,#20644,#20645,#20646,#20647,
#20648,#20649,#20650,#20651,#20652,#20653,#20654,#20655,#20656,#20657,#20658,
#20659,#20660,#20661,#20662,#20663,#20664,#20665,#20666,#20667,#20668,#20669,
#20670,#20671,#20672,#20673,#20674,#20675,#20676,#20677,#20678,#20679,#20680,
#20681,#20682,#20683,#20684,#20685,#20686,#20687,#20688,#20689,#20690,#20691,
#20692,#20693,#20694,#20695,#20696,#20697,#20698,#20699,#20700,#20701,#20702,
#20703,#20704,#20705,#20706,#20707,#20708,#20709,#20710,#20711,#20712,#20713,
#20714,#20715,#20716,#20717,#20718,#20719,#20720,#20721,#20722,#20723,#20724,
#20725,#20726,#20727,#20728,#20729,#20730,#20731,#20732,#20733,#20734,#20735,
#20736,#20737,#20738,#20739,#20740,#20741,#20742,#20743,#20744,#20745,#20746,
#20747,#20748,#20749,#20750,#20751,#20752,#20753,#20754,#20755),
 .UNSPECIFIED.,.F.,.F.,(4,2,2,2,2,2,2,2,2,2,2,2,2,2,2,2,2,2,2,2,2,2,2,2,
2,2,2,2,2,2,2,2,2,2,2,2,2,2,2,2,2,2,2,2,2,2,2,2,2,2,2,2,2,2,2,2,2,2,2,2,
2,2,2,2,2,2,2,2,2,2,2,2,2,2,2,2,2,2,2,2,2,2,2,2,2,2,2,2,2,2,2,2,2,2,2,2,
2,2,2,2,2,2,2,2,2,4),(-2.18888770495768,-2.17440356240776,-2.15760483198674,
-2.1529013703585,-2.14998009510879,-2.14728951265677,-2.14381493702274,
-2.13621610742933,-2.09547509211733,-2.08172747531193,-2.06051870295789,
-2.05587459133256,-2.05383918232385,-2.05232911905959,-2.05063398069282,
-2.04770158677108,-2.0364564406292,-2.02570297855795,-1.99101537655758,
-1.96553909356269,-1.96024970328795,-1.95720084609208,-1.95453560810125,
-1.95122661499686,-1.94610243463115,-1.91309432495797,-1.86966794363949,
-1.86331604464308,-1.86101313797446,-1.85945555499966,-1.85805021627004,
-1.85611079474346,-1.85116696751013,-1.81977810110936,-1.78894211509328,
-1.77135846820353,-1.76658613284954,-1.76364971124354,-1.76096342398723,
-1.7575197220415,-1.7500913400709,-1.70589220198532,-1.69656608180767,-1.67987754901806,
-1.67079125353471,-1.66816622499803,-1.6665388969697,-1.66501942250558,
-1.6631765141586,-1.65847420477853,-1.61886094922967,-1.58088410189835,
-1.5745581483308,-1.57129132783081,-1.56862868744837,-1.56554790676729,
-1.56025389159061,-1.53702866601674,-1.49803501717298,-1.47872439493125,
-1.47546846403827,-1.4737031323747,-1.47220530171545,-1.47028282855015,
-1.46716349806044,-1.4452196385958,-1.41123484784928,-1.38589295777027,
-1.38060969252384,-1.37756191815101,-1.3748961844373,-1.37158469865851,
-1.36645303480537,-1.33285651672871,-1.28998301756724,-1.28366083261001,
-1.28136189386708,-1.27980499096779,-1.27839870469658,-1.27645596614525,
-1.27149344249406,-1.24188020293477,-1.21605565644257,-1.19280633788884,
-1.18751077798279,-1.18442944257999,-1.18176652851354,-1.17849963399397,
-1.17217440644923,-1.13470962514543,-1.09445035578459,-1.08980226055688,
-1.0879677578334,-1.0864501846656,-1.08481853441266,-1.08217467602329,-1.07289968352053,
-1.05567579519044,-1.01718049724718,-0.998927396005311,-0.993911819765243,
-0.990921987579742,-0.988247505054198,-0.984844934284836,-0.977833746534452,
-0.973925068013576),.UNSPECIFIED.);
#1148=B_SPLINE_CURVE_WITH_KNOTS('',3,(#20756,#20757,#20758,#20759,#20760,
#20761,#20762,#20763,#20764,#20765,#20766,#20767,#20768,#20769,#20770,#20771,
#20772,#20773,#20774,#20775,#20776,#20777,#20778,#20779,#20780,#20781,#20782,
#20783,#20784,#20785,#20786,#20787,#20788,#20789,#20790,#20791,#20792,#20793,
#20794,#20795,#20796,#20797,#20798,#20799,#20800,#20801,#20802,#20803,#20804,
#20805,#20806,#20807,#20808,#20809,#20810,#20811,#20812,#20813,#20814,#20815,
#20816,#20817,#20818,#20819,#20820,#20821,#20822,#20823,#20824,#20825,#20826,
#20827,#20828,#20829,#20830,#20831,#20832,#20833,#20834,#20835,#20836,#20837,
#20838,#20839,#20840,#20841,#20842,#20843,#20844,#20845,#20846,#20847,#20848,
#20849,#20850,#20851,#20852,#20853,#20854,#20855,#20856,#20857,#20858,#20859,
#20860,#20861,#20862,#20863,#20864,#20865,#20866,#20867,#20868,#20869,#20870,
#20871,#20872,#20873,#20874,#20875,#20876,#20877,#20878,#20879,#20880,#20881,
#20882,#20883,#20884,#20885,#20886,#20887,#20888,#20889,#20890,#20891,#20892,
#20893,#20894,#20895,#20896,#20897,#20898,#20899,#20900,#20901,#20902,#20903,
#20904,#20905,#20906,#20907,#20908,#20909,#20910,#20911,#20912,#20913,#20914,
#20915,#20916,#20917,#20918,#20919,#20920,#20921,#20922,#20923,#20924,#20925,
#20926,#20927,#20928,#20929,#20930,#20931,#20932,#20933,#20934,#20935,#20936,
#20937,#20938,#20939,#20940,#20941,#20942,#20943,#20944,#20945,#20946,#20947,
#20948,#20949,#20950,#20951,#20952,#20953,#20954,#20955,#20956,#20957,#20958,
#20959,#20960,#20961),.UNSPECIFIED.,.F.,.F.,(4,2,2,2,2,2,2,2,2,2,2,2,2,
2,2,2,2,2,2,2,2,2,2,2,2,2,2,2,2,2,2,2,2,2,2,2,2,2,2,2,2,2,2,2,2,2,2,2,2,
2,2,2,2,2,2,2,2,2,2,2,2,2,2,2,2,2,2,2,2,2,2,2,2,2,2,2,2,2,2,2,2,2,2,2,2,
2,2,2,2,2,2,2,2,2,2,2,2,2,2,2,2,2,4),(-1.45799448822835,-1.44369859826014,
-1.4103702764355,-1.38519006403529,-1.37991539342407,-1.37686979111578,
-1.37420432427642,-1.3708910545462,-1.36575257505012,-1.33176520332503,
-1.28925062247887,-1.28294848488126,-1.28065265946425,-1.27909664593552,
-1.27769028630853,-1.27574629181798,-1.27077456819685,-1.24130627610694,
-1.21615198256352,-1.19216297183634,-1.18682834779486,-1.18373868908013,
-1.18107715015986,-1.17782276776665,-1.17155637777987,-1.16358575126856,
-1.14486736881379,-1.10345826147743,-1.09115577642696,-1.08816812951347,
-1.08644352677372,-1.08509088844199,-1.08319300473201,-1.07928921225045,
-1.07409112914766,-1.06102008615378,-1.02199955019933,-0.998833693039655,
-0.993542999963677,-0.990462962085075,-0.987800262057036,-0.984532488581164,
-0.978201929049717,-0.939568411565091,-0.900633052680451,-0.895984261951173,
-0.894094773852571,-0.892563380156228,-0.890956019443983,-0.888421611277405,
-0.880200064816503,-0.865852473554847,-0.820750747330644,-0.804551168049324,
-0.799732117706123,-0.796785522238933,-0.794102054317322,-0.790620900147062,
-0.783191943218217,-0.752879198212985,-0.720642340681662,-0.704999505049405,
-0.701804168829464,-0.700032332432719,-0.698535243023055,-0.696621783418443,
-0.692637997230728,-0.68730214706372,-0.673704755880074,-0.633403907149467,
-0.612091287965335,-0.606915906687448,-0.603862129269355,-0.601197261180934,
-0.597894796916618,-0.591391778369867,-0.549596001194279,-0.514371565420689,
-0.509535194772166,-0.507613675795986,-0.506212827380192,-0.50464994023431,
-0.502321648549891,-0.495785540703312,-0.485458474152035,-0.462989283529869,
-0.422705340890909,-0.415090161046028,-0.411612385036776,-0.408921076312092,
-0.406000773055517,-0.401302808986865,-0.384570986613379,-0.352330476805928,
-0.321288902334277,-0.316331596124056,-0.314389778305016,-0.312983762683364,
-0.311426717947963,-0.309126829181139,-0.302797269005275,-0.259790057080148,
-0.242722284356607),.UNSPECIFIED.);
#1149=B_SPLINE_CURVE_WITH_KNOTS('',3,(#20967,#20968,#20969,#20970,#20971,
#20972,#20973,#20974,#20975,#20976,#20977,#20978,#20979,#20980,#20981,#20982,
#20983,#20984,#20985,#20986,#20987,#20988,#20989,#20990,#20991,#20992,#20993,
#20994,#20995,#20996,#20997,#20998,#20999,#21000,#21001,#21002,#21003,#21004,
#21005,#21006,#21007,#21008,#21009,#21010,#21011,#21012,#21013,#21014,#21015,
#21016,#21017,#21018,#21019,#21020,#21021,#21022,#21023,#21024,#21025,#21026,
#21027,#21028,#21029,#21030,#21031,#21032,#21033,#21034,#21035,#21036,#21037,
#21038,#21039,#21040,#21041,#21042,#21043,#21044,#21045,#21046,#21047,#21048,
#21049,#21050,#21051,#21052,#21053,#21054,#21055,#21056,#21057,#21058,#21059,
#21060,#21061,#21062,#21063,#21064,#21065,#21066,#21067,#21068,#21069,#21070,
#21071,#21072,#21073,#21074,#21075,#21076,#21077,#21078,#21079,#21080,#21081,
#21082,#21083,#21084,#21085,#21086,#21087,#21088,#21089,#21090,#21091,#21092,
#21093,#21094,#21095,#21096,#21097,#21098,#21099,#21100,#21101,#21102,#21103,
#21104,#21105,#21106,#21107,#21108,#21109,#21110,#21111,#21112,#21113,#21114,
#21115,#21116,#21117,#21118,#21119,#21120,#21121,#21122,#21123,#21124,#21125,
#21126,#21127,#21128,#21129,#21130,#21131,#21132,#21133,#21134,#21135,#21136,
#21137,#21138,#21139,#21140),.UNSPECIFIED.,.F.,.F.,(4,2,2,2,2,2,2,2,2,2,
2,2,2,2,2,2,2,2,2,2,2,2,2,2,2,2,2,2,2,2,2,2,2,2,2,2,2,2,2,2,2,2,2,2,2,2,
2,2,2,2,2,2,2,2,2,2,2,2,2,2,2,2,2,2,2,2,2,2,2,2,2,2,2,2,2,2,2,2,2,2,2,2,
2,2,2,2,4),(-0.97373548788866,-0.973604728194627,-0.971304204815467,-0.964972036506884,
-0.921921862329116,-0.888535807356521,-0.883406613516542,-0.880095551096803,
-0.877429421992487,-0.874380391823306,-0.869092894546673,-0.843684647440481,
-0.809416338882272,-0.787776625017307,-0.784651797334878,-0.782727512220894,
-0.78122928828612,-0.779464671914078,-0.776213097806986,-0.757031339542577,
-0.718189338689354,-0.707008573991512,-0.69317330880848,-0.688618202861663,
-0.68572859672968,-0.683025537646131,-0.679412424831105,-0.671254008276013,
-0.660051178133697,-0.627218225834422,-0.59696077961473,-0.592014492293333,
-0.590074366644002,-0.588668617756306,-0.587110685802799,-0.58480745382514,
-0.578455726437245,-0.535045578816015,-0.502037618027926,-0.49691265809777,
-0.493602900567647,-0.490936898281507,-0.48788700403431,-0.482595408226687,
-0.457102972014939,-0.422382293104705,-0.411609293767327,-0.400364188362582,
-0.39743114527212,-0.395735550918995,-0.394225006123276,-0.392188881164949,
-0.387542776652187,-0.366323765661868,-0.352429809005365,-0.311874991196785,
-0.304269038113326,-0.300792541335656,-0.298101005782164,-0.295179231159805,
-0.290476160073781,-0.273693586696225,-0.241274892374953,-0.210465338169429,
-0.205519084545317,-0.203578958087331,-0.202173203462676,-0.200646575954329,
-0.198418594633079,-0.195828334265892,-0.191064542594281,-0.142545504539599,
-0.115283373729028,-0.109800370965303,-0.106676548222583,-0.104281696601305,
-0.101175562291424,-0.0956222642232126,-0.0632739055048681,-0.0223188693324635,
-0.0134075072082791,-0.0107024827845414,-0.00905719579829945,-0.0076267449158626,
-0.00611663410577336,-0.00356811798796674,-0.000573380549723848),
 .UNSPECIFIED.);
#1150=B_SPLINE_CURVE_WITH_KNOTS('',3,(#21141,#21142,#21143,#21144,#21145,
#21146,#21147,#21148,#21149,#21150,#21151,#21152,#21153,#21154,#21155,#21156,
#21157,#21158,#21159,#21160,#21161,#21162,#21163,#21164,#21165,#21166,#21167,
#21168,#21169,#21170,#21171,#21172,#21173,#21174,#21175,#21176,#21177,#21178,
#21179,#21180,#21181,#21182),.UNSPECIFIED.,.F.,.F.,(4,2,2,2,2,2,2,2,2,2,
2,2,2,2,2,2,2,2,2,2,4),(-2.4308877319842,-2.40572329914951,-2.38654123381901,
-2.3572219218908,-2.34858689679086,-2.34489311136623,-2.34217776507696,
-2.33931915586052,-2.33490404708301,-2.32218461137482,-2.26758946851478,
-2.25664267001732,-2.25202917463806,-2.24949613063449,-2.24735265802882,
-2.24583264341316,-2.24442746066131,-2.24248841672118,-2.23754619127848,
-2.20688713278786,-2.18888770495768),.UNSPECIFIED.);
#1151=B_SPLINE_CURVE_WITH_KNOTS('',3,(#21184,#21185,#21186,#21187,#21188,
#21189,#21190,#21191,#21192,#21193,#21194,#21195,#21196,#21197,#21198,#21199,
#21200,#21201,#21202,#21203,#21204,#21205,#21206,#21207,#21208,#21209,#21210,
#21211,#21212,#21213,#21214,#21215,#21216,#21217,#21218,#21219,#21220,#21221,
#21222,#21223,#21224,#21225,#21226,#21227,#21228,#21229,#21230,#21231,#21232,
#21233,#21234,#21235,#21236,#21237,#21238,#21239,#21240,#21241,#21242,#21243,
#21244,#21245),.UNSPECIFIED.,.F.,.F.,(4,2,2,2,2,2,2,2,2,2,2,2,2,2,2,2,2,
2,2,2,2,2,2,2,2,2,2,2,2,2,4),(-0.242722284356607,-0.226318259385084,-0.22120460494511,
-0.217898602287688,-0.215233340481677,-0.215182011302106,-0.215143779362832,
-0.215083835499035,-0.215027516824497,-0.211975580060041,-0.208709367535101,
-0.203661761444521,-0.194061184282351,-0.168978162152365,-0.128935362626007,
-0.123295441388878,-0.121032386526694,-0.119498167859693,-0.117894973057576,
-0.115379671990079,-0.107330219378015,-0.0934241922212276,-0.0512612172895995,
-0.0327255814975402,-0.0272962239111053,-0.0241847876084111,-0.0217759015420467,
-0.0192546829051084,-0.0161911752762037,-0.00990648707394315,-0.00057360079793139),
 .UNSPECIFIED.);
#1152=B_SPLINE_CURVE_WITH_KNOTS('',3,(#21246,#21247,#21248,#21249,#21250,
#21251,#21252,#21253,#21254,#21255,#21256,#21257,#21258,#21259,#21260,#21261,
#21262,#21263,#21264,#21265,#21266,#21267,#21268,#21269,#21270,#21271,#21272,
#21273,#21274,#21275,#21276,#21277,#21278,#21279,#21280,#21281,#21282,#21283,
#21284,#21285,#21286,#21287,#21288,#21289,#21290,#21291,#21292,#21293,#21294,
#21295,#21296,#21297,#21298,#21299,#21300,#21301,#21302,#21303,#21304,#21305,
#21306,#21307,#21308,#21309,#21310,#21311,#21312,#21313,#21314,#21315,#21316,
#21317,#21318,#21319,#21320,#21321,#21322,#21323,#21324,#21325,#21326,#21327,
#21328,#21329,#21330,#21331,#21332,#21333,#21334,#21335,#21336,#21337,#21338,
#21339,#21340,#21341,#21342,#21343,#21344,#21345,#21346,#21347,#21348,#21349,
#21350,#21351,#21352,#21353,#21354,#21355,#21356,#21357,#21358,#21359,#21360,
#21361,#21362,#21363,#21364,#21365,#21366,#21367,#21368,#21369,#21370,#21371,
#21372,#21373,#21374,#21375,#21376,#21377,#21378,#21379,#21380,#21381,#21382,
#21383,#21384,#21385,#21386,#21387,#21388,#21389,#21390,#21391,#21392,#21393,
#21394,#21395,#21396,#21397,#21398,#21399,#21400,#21401,#21402,#21403,#21404,
#21405,#21406,#21407,#21408,#21409,#21410,#21411,#21412,#21413,#21414,#21415,
#21416,#21417,#21418,#21419,#21420,#21421,#21422,#21423),.UNSPECIFIED.,
 .F.,.F.,(4,2,2,2,2,2,2,2,2,2,2,2,2,2,2,2,2,2,2,2,2,2,2,2,2,2,2,2,2,2,2,
2,2,2,2,2,2,2,2,2,2,2,2,2,2,2,2,2,2,2,2,2,2,2,2,2,2,2,2,2,2,2,2,2,2,2,2,
2,2,2,2,2,2,2,2,2,2,2,2,2,2,2,2,2,2,2,2,2,4),(-2.43072114342198,-2.38276134734879,
-2.36879770025489,-2.36072718495424,-2.35821004161092,-2.35660680600177,
-2.35507351307365,-2.35317550959972,-2.34847524724012,-2.31077926545563,
-2.28801107601814,-2.27515887765741,-2.2689788211344,-2.26524959406597,
-2.26187752410252,-2.26181526849542,-2.26178716691591,-2.2617563388158,
-2.26172245002302,-2.26168511195143,-2.26164386986024,-2.25908620410354,
-2.25610229025896,-2.25111016739191,-2.23315677617736,-2.18976770432065,
-2.17566124075281,-2.16753467588931,-2.16501116048251,-2.16340645597938,
-2.16187399488937,-2.15997937094444,-2.15529911200416,-2.11708003630143,
-2.08982473700654,-2.07973586822317,-2.07220657030665,-2.06870726012314,
-2.06602180216787,-2.06308493925768,-2.05830887488936,-2.04249631680944,
-2.00169566616791,-1.97596383251657,-1.97253734310369,-1.97073623965491,
-1.96924137849381,-1.9673646643111,-1.96439723563123,-1.94775450060935,
-1.90890171522837,-1.88288479493016,-1.87756958646194,-1.87451533452724,
-1.87185095261923,-1.86855025571772,-1.86345285229067,-1.83277661150112,
-1.78478913746452,-1.78000728641993,-1.77794786395009,-1.7764343884367,
-1.77475134709595,-1.77187389523294,-1.76125209015473,-1.72539049655759,
-1.6913224699871,-1.68501461540306,-1.68175167537826,-1.67908952215944,
-1.6760063166571,-1.67070072643705,-1.64726180099989,-1.60837527431319,
-1.58916777450283,-1.58591577596048,-1.58415139795992,-1.58265366920229,
-1.5807304568846,-1.57760826524219,-1.555500156363,-1.52163916867148,-1.49632195760372,
-1.49104018898702,-1.4879929511025,-1.48532750636872,-1.48201615788284,
-1.4768843119462,-1.45771362438087),.UNSPECIFIED.);
#1153=B_SPLINE_CURVE_WITH_KNOTS('',3,(#21428,#21429,#21430,#21431,#21432,
#21433,#21434,#21435,#21436,#21437,#21438,#21439,#21440,#21441,#21442,#21443,
#21444,#21445,#21446,#21447,#21448,#21449,#21450,#21451,#21452,#21453,#21454,
#21455,#21456,#21457,#21458,#21459,#21460,#21461,#21462,#21463,#21464,#21465,
#21466,#21467,#21468,#21469,#21470,#21471,#21472,#21473,#21474,#21475,#21476,
#21477,#21478,#21479,#21480,#21481,#21482,#21483,#21484,#21485,#21486,#21487,
#21488,#21489,#21490,#21491,#21492,#21493,#21494,#21495,#21496,#21497,#21498,
#21499,#21500,#21501,#21502,#21503,#21504,#21505,#21506,#21507,#21508,#21509,
#21510,#21511,#21512,#21513,#21514,#21515,#21516,#21517,#21518,#21519,#21520,
#21521,#21522,#21523,#21524,#21525,#21526,#21527,#21528,#21529,#21530,#21531,
#21532,#21533,#21534,#21535,#21536,#21537,#21538,#21539,#21540,#21541,#21542,
#21543,#21544,#21545,#21546,#21547,#21548,#21549,#21550,#21551,#21552,#21553,
#21554,#21555,#21556,#21557,#21558,#21559,#21560,#21561,#21562,#21563,#21564,
#21565,#21566,#21567,#21568,#21569,#21570,#21571,#21572,#21573,#21574,#21575,
#21576,#21577,#21578,#21579,#21580,#21581,#21582,#21583,#21584,#21585,#21586,
#21587,#21588,#21589,#21590,#21591,#21592,#21593,#21594,#21595,#21596,#21597,
#21598,#21599,#21600,#21601,#21602,#21603,#21604,#21605,#21606,#21607,#21608,
#21609,#21610,#21611,#21612,#21613,#21614,#21615,#21616,#21617,#21618,#21619,
#21620,#21621,#21622,#21623,#21624,#21625,#21626,#21627,#21628,#21629,#21630,
#21631,#21632,#21633,#21634,#21635,#21636,#21637,#21638,#21639),
 .UNSPECIFIED.,.F.,.F.,(4,2,2,2,2,2,2,2,2,2,2,2,2,2,2,2,2,2,2,2,2,2,2,2,
2,2,2,2,2,2,2,2,2,2,2,2,2,2,2,2,2,2,2,2,2,2,2,2,2,2,2,2,2,2,2,2,2,2,2,2,
2,2,2,2,2,2,2,2,2,2,2,2,2,2,2,2,2,2,2,2,2,2,2,2,2,2,2,2,2,2,2,2,2,2,2,2,
2,2,2,2,2,2,2,2,2,4),(-2.18887902963404,-2.18779188971815,-2.14458953969837,
-2.13824969393521,-2.13594842248798,-2.13439114163079,-2.13298544183683,
-2.13104471703317,-2.12609350142366,-2.09669228265521,-2.06440082352862,
-2.0463670771056,-2.04155693725538,-2.03861220791026,-2.03592809262195,
-2.03250060481311,-2.02516071506774,-1.9798097606552,-1.97156333430698,
-1.94711875847882,-1.94371736288988,-1.94192125821609,-1.94042577121953,
-1.93854220906575,-1.93555284436288,-1.9183831448492,-1.90436129199647,
-1.88057157478502,-1.85570341255035,-1.84946564663623,-1.84621659021721,
-1.84355463634892,-1.84045908688399,-1.83510062419631,-1.81067803282439,
-1.7724906343299,-1.75365097440494,-1.7504122192542,-1.74865045401465,-1.74715209650678,
-1.74522436266864,-1.74208761634755,-1.7191674717933,-1.67918445458263,
-1.66010267785497,-1.65520884403076,-1.65224565862551,-1.64956578452849,
-1.64611563298955,-1.63885393747365,-1.59262975537905,-1.57043742882706,
-1.56317742478124,-1.55813637820146,-1.55603272210668,-1.55451209701436,
-1.55284854193223,-1.55006047043855,-1.54041060039024,-1.49782899287477,
-1.47053882238745,-1.46347976150915,-1.46006810383705,-1.45739272614607,
-1.45440836201934,-1.44941748281705,-1.43164248648742,-1.38269062400031,
-1.37209248498086,-1.36543427394653,-1.36308930374289,-1.3615227641838,
-1.36012441989612,-1.35821359358642,-1.35344143863045,-1.31685842951866,
-1.28852631141926,-1.27298714008495,-1.26840126191458,-1.26550502906752,
-1.26280466704692,-1.25927044523936,-1.25164384538175,-1.21558541551855,
-1.17621304810398,-1.17148743978843,-1.16964060539473,-1.16811992585334,
-1.16649383191799,-1.16387548828637,-1.15485953794626,-1.13837303329464,
-1.12568279567418,-1.08484665284819,-1.07725059933467,-1.07377588084827,
-1.07108459708419,-1.06816197155948,-1.06345503779931,-1.04662967522134,
-1.01405979828696,-0.98346852379255,-0.978510534681342,-0.976568391694447,
-0.975162117925436,-0.97373548788866),.UNSPECIFIED.);
#1154=B_SPLINE_CURVE_WITH_KNOTS('',3,(#21640,#21641,#21642,#21643,#21644,
#21645,#21646,#21647,#21648,#21649,#21650,#21651,#21652,#21653,#21654,#21655,
#21656,#21657,#21658,#21659,#21660,#21661,#21662,#21663,#21664,#21665,#21666,
#21667,#21668,#21669,#21670,#21671,#21672,#21673,#21674,#21675,#21676,#21677,
#21678,#21679,#21680,#21681,#21682,#21683,#21684,#21685,#21686,#21687,#21688,
#21689,#21690,#21691,#21692,#21693,#21694,#21695,#21696,#21697,#21698,#21699,
#21700,#21701,#21702,#21703,#21704,#21705,#21706,#21707,#21708,#21709,#21710,
#21711,#21712,#21713,#21714,#21715,#21716,#21717,#21718,#21719,#21720,#21721,
#21722,#21723,#21724,#21725,#21726,#21727,#21728,#21729,#21730,#21731,#21732,
#21733,#21734,#21735,#21736,#21737,#21738,#21739,#21740,#21741,#21742,#21743,
#21744,#21745,#21746,#21747,#21748,#21749,#21750,#21751,#21752,#21753,#21754,
#21755,#21756,#21757,#21758,#21759,#21760,#21761,#21762,#21763,#21764,#21765,
#21766,#21767,#21768,#21769,#21770,#21771,#21772,#21773,#21774,#21775,#21776,
#21777,#21778,#21779,#21780,#21781,#21782,#21783,#21784,#21785,#21786,#21787,
#21788,#21789,#21790,#21791,#21792,#21793,#21794,#21795,#21796,#21797,#21798,
#21799,#21800,#21801,#21802,#21803,#21804,#21805,#21806,#21807,#21808,#21809,
#21810,#21811,#21812,#21813,#21814,#21815,#21816,#21817,#21818,#21819,#21820,
#21821,#21822,#21823,#21824,#21825,#21826,#21827,#21828,#21829,#21830,#21831,
#21832,#21833,#21834,#21835,#21836,#21837,#21838,#21839,#21840,#21841,#21842,
#21843),.UNSPECIFIED.,.F.,.F.,(4,2,2,2,2,2,2,2,2,2,2,2,2,2,2,2,2,2,2,2,
2,2,2,2,2,2,2,2,2,2,2,2,2,2,2,2,2,2,2,2,2,2,2,2,2,2,2,2,2,2,2,2,2,2,2,2,
2,2,2,2,2,2,2,2,2,2,2,2,2,2,2,2,2,2,2,2,2,2,2,2,2,2,2,2,2,2,2,2,2,2,2,2,
2,2,2,2,2,2,2,2,2,4),(-1.45771362438087,-1.44042256863282,-1.41399613211339,
-1.39586250675788,-1.39265172242565,-1.39089612954797,-1.38939737789245,
-1.38746187054114,-1.38429831392562,-1.35951211632451,-1.35277051501603,
-1.32818523683517,-1.30307746458597,-1.29780601040883,-1.2947609234272,
-1.29209511672579,-1.28878039382736,-1.2836376629233,-1.24835200954516,
-1.21559674475117,-1.20240893850855,-1.19935924627799,-1.19762033398754,
-1.19626970511579,-1.19439158724814,-1.19058812509207,-1.16040482887616,
-1.11287268119788,-1.10574900670334,-1.10232533647546,-1.09964898027898,
-1.09667222563652,-1.0917148101817,-1.07177465942165,-1.02472905344581,
-1.00933686210975,-1.00615464267641,-1.00438570022016,-1.00288824948975,
-1.00097072482877,-0.996966241393652,-0.991594654335988,-0.97785942373292,
-0.936875085724848,-0.916349886461119,-0.911226143515123,-0.908184034343339,
-0.905543163612789,-0.902236222277869,-0.895711341102798,-0.887319638126186,
-0.867067484876713,-0.842139587236554,-0.816595305298695,-0.813424871707151,
-0.81148728411627,-0.809988284158567,-0.808233972044277,-0.805029465425721,
-0.787049734118612,-0.760781535610508,-0.723975493133445,-0.718874583209737,
-0.715572499401652,-0.71290759203684,-0.709853388922403,-0.704539966444257,
-0.678580991744954,-0.640357146823222,-0.623018272463115,-0.620021929988422,
-0.618136314402451,-0.616640801704105,-0.614846618791814,-0.61145419257761,
-0.587408093184771,-0.57413411884912,-0.533845271999984,-0.526230477237613,
-0.522752830216865,-0.520061602518235,-0.517141368687712,-0.512443476116218,
-0.495711471755008,-0.463469771819595,-0.43243120601779,-0.427473836368519,
-0.425532040276686,-0.424126057893796,-0.422569062606413,-0.420269284231241,
-0.413940270099266,-0.370941323991666,-0.337493047809635,-0.332363644730183,
-0.329052902822178,-0.326387339871642,-0.323339304539173,-0.31805446218761,
-0.292685391250116,-0.258662021533076,-0.242408550118657),.UNSPECIFIED.);
#1155=B_SPLINE_CURVE_WITH_KNOTS('',3,(#21849,#21850,#21851,#21852,#21853,
#21854,#21855,#21856,#21857,#21858,#21859,#21860,#21861,#21862,#21863,#21864,
#21865,#21866,#21867,#21868,#21869,#21870,#21871,#21872,#21873,#21874,#21875,
#21876,#21877,#21878,#21879,#21880,#21881,#21882,#21883,#21884,#21885,#21886,
#21887,#21888,#21889,#21890,#21891,#21892,#21893,#21894,#21895,#21896,#21897,
#21898,#21899,#21900,#21901,#21902,#21903,#21904,#21905,#21906,#21907,#21908,
#21909,#21910,#21911,#21912,#21913,#21914,#21915,#21916,#21917,#21918,#21919,
#21920,#21921,#21922,#21923,#21924,#21925,#21926,#21927,#21928,#21929,#21930,
#21931,#21932,#21933,#21934,#21935,#21936,#21937,#21938,#21939,#21940,#21941,
#21942,#21943,#21944,#21945,#21946,#21947,#21948,#21949,#21950,#21951,#21952,
#21953,#21954,#21955,#21956,#21957,#21958,#21959,#21960,#21961,#21962,#21963,
#21964,#21965,#21966,#21967,#21968,#21969,#21970,#21971,#21972,#21973,#21974,
#21975,#21976,#21977,#21978,#21979,#21980,#21981,#21982,#21983,#21984,#21985,
#21986,#21987,#21988,#21989,#21990,#21991,#21992,#21993,#21994,#21995,#21996,
#21997,#21998,#21999,#22000,#22001,#22002,#22003,#22004,#22005,#22006,#22007,
#22008,#22009,#22010,#22011,#22012,#22013,#22014,#22015,#22016,#22017,#22018,
#22019,#22020,#22021,#22022,#22023,#22024,#22025,#22026,#22027,#22028,#22029,
#22030,#22031,#22032,#22033,#22034,#22035,#22036,#22037,#22038),
 .UNSPECIFIED.,.F.,.F.,(4,2,2,2,2,2,2,2,2,2,2,2,2,2,2,2,2,2,2,2,2,2,2,2,
2,2,2,2,2,2,2,2,2,2,2,2,2,2,2,2,2,2,2,2,2,2,2,2,2,2,2,2,2,2,2,2,2,2,2,2,
2,2,2,2,2,2,2,2,2,2,2,2,2,2,2,2,2,2,2,2,2,2,2,2,2,2,2,2,2,2,2,2,2,2,4),
(-0.973910253760765,-0.970007335956458,-0.964667944357671,-0.961576352313021,
-0.958913621710933,-0.955658361597496,-0.949392046898408,-0.91112105632681,
-0.871659387208275,-0.866939882565676,-0.865093908203904,-0.863573345849303,
-0.861946636119496,-0.859325930210996,-0.850287972304353,-0.833740452778761,
-0.82193107628202,-0.780241949326078,-0.772678529725419,-0.769209537951511,
-0.766518907252409,-0.763593202294974,-0.758872884172139,-0.741900740212514,
-0.708807985344714,-0.67889608448649,-0.673943935020186,-0.672002696917308,
-0.670596576677982,-0.669038754928178,-0.666736571655642,-0.660393359338801,
-0.617147114423141,-0.583959659125359,-0.578832377611862,-0.575521746446493,
-0.572855445137152,-0.569805650796398,-0.564515367204381,-0.539057550574652,
-0.504539140678535,-0.493805736823831,-0.482311645400885,-0.479357328303278,
-0.477656965076492,-0.476147471472981,-0.474119931413592,-0.469523055971169,
-0.448768158291233,-0.412539521157562,-0.390043428086862,-0.38478985217901,
-0.38171762119792,-0.379053360498759,-0.375773064954076,-0.369383835400975,
-0.326330713663641,-0.29224060814059,-0.287357532236295,-0.285427782319721,
-0.28402453072648,-0.282463307492475,-0.280144862564058,-0.273684522411905,
-0.263524488281457,-0.234864010360416,-0.197416756382406,-0.191838908032126,
-0.188669621715466,-0.186071841971015,-0.185953164450266,-0.185842802818211,
-0.185739176926683,-0.18564104505233,-0.185547409424046,-0.18545745196806,
-0.185370489254994,-0.185285940113418,-0.185203301766309,-0.185122131959548,
-0.185042035091654,-0.181629860913606,-0.17770542800625,-0.148797542523752,
-0.113508106682466,-0.0963909586767748,-0.0934027590896143,-0.0915192262306326,
-0.0900232638601776,-0.0882259807922269,-0.0848207291040813,-0.0602277111366393,
-0.00936464206830907,-0.00384968017010287,-0.00057394889050387),
 .UNSPECIFIED.);
#1156=B_SPLINE_CURVE_WITH_KNOTS('',3,(#22039,#22040,#22041,#22042,#22043,
#22044,#22045,#22046,#22047,#22048,#22049,#22050,#22051,#22052,#22053,#22054,
#22055,#22056,#22057,#22058,#22059,#22060,#22061,#22062,#22063,#22064,#22065,
#22066,#22067,#22068,#22069,#22070,#22071,#22072,#22073,#22074,#22075,#22076,
#22077,#22078,#22079,#22080,#22081,#22082,#22083,#22084,#22085,#22086),
 .UNSPECIFIED.,.F.,.F.,(4,2,2,2,2,2,2,2,2,2,2,2,2,2,2,2,2,2,2,2,2,2,2,4),
(-2.43085648084854,-2.42887934336279,-2.42647850822906,-2.42393550147241,
-2.42107988776888,-2.41684207527017,-2.40480128623111,-2.35859764609427,
-2.33571224737799,-2.33089544752737,-2.32882995986386,-2.32731553120602,
-2.32563524922959,-2.32277050655347,-2.31228859045544,-2.27633802420747,
-2.25267587834801,-2.2387796649061,-2.23548276615809,-2.23240114174611,
-2.22979458349587,-2.22662945598436,-2.22106611756832,-2.18887902963404),
 .UNSPECIFIED.);
#1157=B_SPLINE_CURVE_WITH_KNOTS('',3,(#22088,#22089,#22090,#22091,#22092,
#22093,#22094,#22095,#22096,#22097,#22098,#22099,#22100,#22101,#22102,#22103,
#22104,#22105,#22106,#22107,#22108,#22109,#22110,#22111,#22112,#22113,#22114,
#22115,#22116,#22117,#22118,#22119,#22120,#22121,#22122,#22123,#22124,#22125,
#22126,#22127,#22128,#22129,#22130,#22131,#22132,#22133,#22134,#22135,#22136,
#22137,#22138,#22139),.UNSPECIFIED.,.F.,.F.,(4,2,2,2,2,2,2,2,2,2,2,2,2,
2,2,2,2,2,2,2,2,2,2,2,2,4),(-0.242408550118657,-0.236717564735722,-0.233597745241758,
-0.231675167927113,-0.230177381040449,-0.228412269050664,-0.225272045602489,
-0.221258788898725,-0.212327099012181,-0.179844890610788,-0.144261837331527,
-0.139122017576931,-0.135808131122734,-0.133142346452952,-0.130096575382254,
-0.124822129015066,-0.101721457752813,-0.0693196227094799,-0.0435634375784882,
-0.0403919137704319,-0.0384540101339557,-0.0369549914634115,-0.0352009208108212,
-0.0333298928224582,-0.0303889327839463,-0.000573497123783065),
 .UNSPECIFIED.);
#1158=B_SPLINE_CURVE_WITH_KNOTS('',3,(#22140,#22141,#22142,#22143,#22144,
#22145,#22146,#22147,#22148,#22149,#22150,#22151,#22152,#22153,#22154,#22155,
#22156,#22157,#22158,#22159,#22160,#22161,#22162,#22163,#22164,#22165,#22166,
#22167,#22168,#22169,#22170,#22171,#22172,#22173,#22174,#22175,#22176,#22177,
#22178,#22179,#22180,#22181,#22182,#22183,#22184,#22185,#22186,#22187,#22188,
#22189,#22190,#22191,#22192,#22193,#22194,#22195,#22196,#22197,#22198,#22199,
#22200,#22201,#22202,#22203,#22204,#22205,#22206,#22207,#22208,#22209,#22210,
#22211,#22212,#22213,#22214,#22215,#22216,#22217,#22218,#22219,#22220,#22221,
#22222,#22223,#22224,#22225,#22226,#22227,#22228,#22229,#22230,#22231,#22232,
#22233,#22234,#22235,#22236,#22237,#22238,#22239,#22240,#22241,#22242,#22243,
#22244,#22245,#22246,#22247,#22248,#22249,#22250,#22251,#22252,#22253,#22254,
#22255,#22256,#22257,#22258,#22259,#22260,#22261,#22262,#22263,#22264,#22265,
#22266,#22267,#22268,#22269,#22270,#22271,#22272,#22273,#22274,#22275,#22276,
#22277,#22278,#22279,#22280,#22281,#22282,#22283,#22284,#22285,#22286,#22287,
#22288,#22289,#22290,#22291,#22292,#22293,#22294,#22295,#22296,#22297,#22298,
#22299,#22300,#22301,#22302,#22303,#22304,#22305,#22306,#22307),
 .UNSPECIFIED.,.F.,.F.,(4,2,2,2,2,2,2,2,2,2,2,2,2,2,2,2,2,2,2,2,2,2,2,2,
2,2,2,2,2,2,2,2,2,2,2,2,2,2,2,2,2,2,2,2,2,2,2,2,2,2,2,2,2,2,2,2,2,2,2,2,
2,2,2,2,2,2,2,2,2,2,2,2,2,2,2,2,2,2,2,2,2,2,2,4),(-2.43118060654611,-2.39196463195278,
-2.3809253323704,-2.37561453331713,-2.37256143721174,-2.36989725642257,
-2.36659576347962,-2.36149512428364,-2.32465356621113,-2.29362904853487,
-2.28451810846221,-2.27862253645854,-2.27642174469659,-2.2748560104628,
-2.2734582909036,-2.27154822780952,-2.26677753380414,-2.2302723028536,-2.20189143935604,
-2.19156205004826,-2.18389507731415,-2.18037068504966,-2.17768191026985,
-2.17475706331223,-2.17003557193757,-2.15471966165479,-2.14713155745807,
-2.1064341139553,-2.08729506461695,-2.08404597051078,-2.08228237933332,
-2.08078483115809,-2.07886122321812,-2.07573717832556,-2.05416041397805,
-2.01987877406766,-1.99447550416318,-1.98919010730847,-1.98614238427989,
-1.98347746232974,-1.98016799574784,-1.9750414445666,-1.9417843913852,-1.89858104190176,
-1.89224129540744,-1.88994027453577,-1.88838323447976,-1.88697782964416,
-1.88503763803769,-1.88008844053518,-1.8501980744753,-1.81712877061964,
-1.8001653238274,-1.79544731112538,-1.79252301168753,-1.78983366583339,
-1.78636633137133,-1.77880668002459,-1.73703102362976,-1.72529624345423,
-1.70873127944794,-1.69968890412828,-1.69706851448798,-1.6954423769428,
-1.69392266450157,-1.69207810075664,-1.6873641910727,-1.64788570824375,
-1.60977856535439,-1.60345220448604,-1.60018561015662,-1.59752338242236,
-1.59444334597592,-1.58915130795254,-1.56595436450651,-1.52693288556181,
-1.50760561576952,-1.50434940332452,-1.50258418239375,-1.50108662753164,
-1.49916478288441,-1.49604701680975,-1.47434180177083,-1.45794268266291),
 .UNSPECIFIED.);
#1159=B_SPLINE_CURVE_WITH_KNOTS('',3,(#22312,#22313,#22314,#22315,#22316,
#22317,#22318,#22319,#22320,#22321,#22322,#22323,#22324,#22325,#22326,#22327,
#22328,#22329,#22330,#22331,#22332,#22333,#22334,#22335,#22336,#22337,#22338,
#22339,#22340,#22341,#22342,#22343,#22344,#22345,#22346,#22347,#22348,#22349,
#22350,#22351,#22352,#22353,#22354,#22355,#22356,#22357,#22358,#22359,#22360,
#22361,#22362,#22363,#22364,#22365,#22366,#22367,#22368,#22369,#22370,#22371,
#22372,#22373,#22374,#22375,#22376,#22377,#22378,#22379,#22380,#22381,#22382,
#22383,#22384,#22385,#22386,#22387,#22388,#22389,#22390,#22391,#22392,#22393,
#22394,#22395,#22396,#22397,#22398,#22399,#22400,#22401,#22402,#22403,#22404,
#22405,#22406,#22407,#22408,#22409,#22410,#22411,#22412,#22413,#22414,#22415,
#22416,#22417,#22418,#22419,#22420,#22421,#22422,#22423,#22424,#22425,#22426,
#22427,#22428,#22429,#22430,#22431,#22432,#22433,#22434,#22435,#22436,#22437,
#22438,#22439,#22440,#22441,#22442,#22443,#22444,#22445,#22446,#22447,#22448,
#22449,#22450,#22451,#22452,#22453,#22454,#22455,#22456,#22457,#22458,#22459,
#22460,#22461,#22462,#22463,#22464,#22465,#22466,#22467,#22468,#22469,#22470,
#22471,#22472,#22473,#22474,#22475,#22476,#22477,#22478,#22479,#22480,#22481,
#22482,#22483,#22484,#22485,#22486,#22487,#22488,#22489,#22490,#22491,#22492,
#22493,#22494,#22495,#22496,#22497,#22498,#22499,#22500,#22501,#22502,#22503,
#22504,#22505,#22506,#22507,#22508,#22509,#22510,#22511,#22512,#22513,#22514,
#22515,#22516,#22517),.UNSPECIFIED.,.F.,.F.,(4,2,2,2,2,2,2,2,2,2,2,2,2,
2,2,2,2,2,2,2,2,2,2,2,2,2,2,2,2,2,2,2,2,2,2,2,2,2,2,2,2,2,2,2,2,2,2,2,2,
2,2,2,2,2,2,2,2,2,2,2,2,2,2,2,2,2,2,2,2,2,2,2,2,2,2,2,2,2,2,2,2,2,2,2,2,
2,2,2,2,2,2,2,2,2,2,2,2,2,2,2,2,2,4),(-2.18915184178403,-2.15490999477389,
-2.12934284439123,-2.12404765414707,-2.12099690624184,-2.11833086968842,
-2.11502199532586,-2.10990013838036,-2.07245149451288,-2.04381121124193,
-2.03361443564529,-2.0271380977853,-2.02481763265576,-2.02325613646213,
-2.02185347927595,-2.0199256280696,-2.01505300186312,-1.98075382772371,
-1.95086985910927,-1.9402303164555,-1.93238640388379,-1.92882890385024,
-1.92613420710193,-1.92322163857381,-1.91856116240269,-1.90382209648975,
-1.86207770094449,-1.83823982733854,-1.8333281168825,-1.83124601000624,
-1.82972864175353,-1.82805520105691,-1.82522306717366,-1.81510238335029,
-1.77887203181308,-1.74477528697373,-1.73834683113047,-1.73505875360406,
-1.73239414653274,-1.72932813196587,-1.72410141056089,-1.70204385928499,
-1.66235668161618,-1.64888273188695,-1.64357872247701,-1.63961342816253,
-1.63770320160982,-1.6363487401082,-1.6346312495718,-1.63167656027281,-1.61981590200441,
-1.61021933546096,-1.57859516134911,-1.5594777374016,-1.55139465839931,
-1.54505788097344,-1.54178826282123,-1.53912471138593,-1.53604440800509,
-1.53075501662727,-1.50763454073341,-1.46857267785558,-1.44919311550179,
-1.44593392733638,-1.44416757799018,-1.44266935110309,-1.44074696870063,
-1.43762893070031,-1.41582932483268,-1.38170779025377,-1.35633135472746,
-1.35104517410425,-1.34799620257989,-1.34532970765976,-1.34201764868971,
-1.33688581603828,-1.30026302319391,-1.27371520508049,-1.25583597384861,
-1.25263466486787,-1.2508806650077,-1.24938100123402,-1.24744132589427,
-1.24426505959426,-1.21611646879554,-1.16847562782958,-1.15992461066259,
-1.15651728394349,-1.15400981362371,-1.15128505896313,-1.14754291434882,
-1.13862344030486,-1.11156221845835,-1.08570731636402,-1.06302336013755,
-1.05988994033273,-1.057963036089,-1.05646451961364,-1.05470160784962,-1.05145835426928,
-1.03250609183763,-0.994058097561331,-0.973910253760765),.UNSPECIFIED.);
#1160=B_SPLINE_CURVE_WITH_KNOTS('',3,(#22518,#22519,#22520,#22521,#22522,
#22523,#22524,#22525,#22526,#22527,#22528,#22529,#22530,#22531,#22532,#22533,
#22534,#22535,#22536,#22537,#22538,#22539,#22540,#22541,#22542,#22543,#22544,
#22545,#22546,#22547,#22548,#22549,#22550,#22551,#22552,#22553,#22554,#22555,
#22556,#22557,#22558,#22559,#22560,#22561,#22562,#22563,#22564,#22565,#22566,
#22567,#22568,#22569,#22570,#22571,#22572,#22573,#22574,#22575,#22576,#22577,
#22578,#22579,#22580,#22581,#22582,#22583,#22584,#22585,#22586,#22587,#22588,
#22589,#22590,#22591,#22592,#22593,#22594,#22595,#22596,#22597,#22598,#22599,
#22600,#22601,#22602,#22603,#22604,#22605,#22606,#22607,#22608,#22609,#22610,
#22611,#22612,#22613,#22614,#22615,#22616,#22617,#22618,#22619,#22620,#22621,
#22622,#22623,#22624,#22625,#22626,#22627,#22628,#22629,#22630,#22631,#22632,
#22633,#22634,#22635,#22636,#22637,#22638,#22639,#22640,#22641,#22642,#22643,
#22644,#22645,#22646,#22647,#22648,#22649,#22650,#22651,#22652,#22653,#22654,
#22655,#22656,#22657,#22658,#22659,#22660,#22661,#22662,#22663,#22664,#22665,
#22666,#22667,#22668,#22669,#22670,#22671,#22672,#22673,#22674,#22675,#22676,
#22677,#22678,#22679,#22680,#22681,#22682,#22683,#22684,#22685,#22686,#22687,
#22688,#22689,#22690,#22691,#22692,#22693,#22694,#22695,#22696,#22697,#22698,
#22699,#22700,#22701,#22702,#22703,#22704,#22705,#22706,#22707,#22708,#22709,
#22710,#22711,#22712,#22713,#22714,#22715,#22716,#22717,#22718,#22719,#22720,
#22721,#22722,#22723,#22724,#22725,#22726,#22727,#22728,#22729),
 .UNSPECIFIED.,.F.,.F.,(4,2,2,2,2,2,2,2,2,2,2,2,2,2,2,2,2,2,2,2,2,2,2,2,
2,2,2,2,2,2,2,2,2,2,2,2,2,2,2,2,2,2,2,2,2,2,2,2,2,2,2,2,2,2,2,2,2,2,2,2,
2,2,2,2,2,2,2,2,2,2,2,2,2,2,2,2,2,2,2,2,2,2,2,2,2,2,2,2,2,2,2,2,2,2,2,2,
2,2,2,2,2,2,2,2,2,4),(-1.45794268266291,-1.44741604209633,-1.41523403763836,
-1.4096870430057,-1.40658285703536,-1.40418878487334,-1.4010649788763,-1.39557942906996,
-1.368235977078,-1.31973183901951,-1.31498320576016,-1.31134506237608,-1.30950018017305,
-1.30815247162596,-1.30638760804386,-1.3032233109807,-1.28815722245847,
-1.24084097654734,-1.22086306844774,-1.21590312159041,-1.21292585344607,
-1.21024966652087,-1.20682708690974,-1.19970896741868,-1.17194602596127,
-1.14588706875495,-1.1215090502018,-1.11835002744888,-1.11641589782808,
-1.11491729963146,-1.11316080137868,-1.10994568863615,-1.0916990789769,
-1.06538139823776,-1.02898729524518,-1.02385073471877,-1.02053797097581,
-1.01787245770853,-1.01482630823605,-1.00954943799119,-0.984333624491158,
-0.95089539424183,-0.928229785922014,-0.925097503499517,-0.923171307247067,
-0.921673356854007,-0.919911167851877,-0.916669426887916,-0.897734553467061,
-0.859316396819779,-0.849172847576924,-0.833933291937676,-0.829219660349825,
-0.826296177641502,-0.823606316291107,-0.820077087298475,-0.812385741515092,
-0.802012983536029,-0.773429723432609,-0.769801592665367,-0.73737707533017,
-0.732451521680624,-0.73051521712097,-0.729110727930674,-0.727552401013611,
-0.72524557892704,-0.718864847481034,-0.674901249235493,-0.642473041565614,
-0.63735448937604,-0.63404722312669,-0.631382174919448,-0.628332232641843,
-0.623037649948009,-0.597461823843092,-0.562234841188767,-0.541711838760622,
-0.538600249233992,-0.536680221536827,-0.535182762950412,-0.533416087002461,
-0.530153227023742,-0.510637425658817,-0.471499603816394,-0.448624523026994,
-0.443350625960008,-0.440274604786087,-0.437611926626121,-0.434339794927307,
-0.427986655175696,-0.419875367136937,-0.400651783053862,-0.365369896465283,
-0.34825509704715,-0.345268039864167,-0.343385344048045,-0.341890137594176,
-0.340093911674002,-0.336691105833041,-0.312151847820454,-0.274447010008433,
-0.254991237744784,-0.249878314528817,-0.246867795098266,-0.244464745431678,
-0.242785158976033),.UNSPECIFIED.);
#1161=B_SPLINE_CURVE_WITH_KNOTS('',3,(#22735,#22736,#22737,#22738,#22739,
#22740,#22741,#22742,#22743,#22744,#22745,#22746,#22747,#22748,#22749,#22750,
#22751,#22752,#22753,#22754,#22755,#22756,#22757,#22758,#22759,#22760,#22761,
#22762,#22763,#22764,#22765,#22766,#22767,#22768,#22769,#22770,#22771,#22772,
#22773,#22774,#22775,#22776,#22777,#22778,#22779,#22780,#22781,#22782,#22783,
#22784,#22785,#22786,#22787,#22788,#22789,#22790,#22791,#22792,#22793,#22794,
#22795,#22796,#22797,#22798,#22799,#22800,#22801,#22802,#22803,#22804,#22805,
#22806,#22807,#22808,#22809,#22810,#22811,#22812,#22813,#22814,#22815,#22816,
#22817,#22818,#22819,#22820,#22821,#22822,#22823,#22824,#22825,#22826,#22827,
#22828,#22829,#22830,#22831,#22832,#22833,#22834,#22835,#22836,#22837,#22838,
#22839,#22840,#22841,#22842,#22843,#22844,#22845,#22846,#22847,#22848,#22849,
#22850,#22851,#22852,#22853,#22854,#22855,#22856,#22857,#22858,#22859,#22860,
#22861,#22862,#22863,#22864,#22865,#22866,#22867,#22868,#22869,#22870,#22871,
#22872,#22873,#22874,#22875,#22876,#22877,#22878,#22879,#22880,#22881,#22882,
#22883,#22884,#22885,#22886,#22887,#22888,#22889,#22890,#22891,#22892,#22893,
#22894,#22895,#22896,#22897,#22898,#22899,#22900,#22901,#22902),
 .UNSPECIFIED.,.F.,.F.,(4,2,2,2,2,2,2,2,2,2,2,2,2,2,2,2,2,2,2,2,2,2,2,2,
2,2,2,2,2,2,2,2,2,2,2,2,2,2,2,2,2,2,2,2,2,2,2,2,2,2,2,2,2,2,2,2,2,2,2,2,
2,2,2,2,2,2,2,2,2,2,2,2,2,2,2,2,2,2,2,2,2,2,2,4),(-0.973989629254837,-0.95370340523295,
-0.949006287027863,-0.947108390963949,-0.945574726407962,-0.943970481800047,
-0.941450662212924,-0.933361580641841,-0.919354220863292,-0.876879867039386,
-0.858036318789459,-0.852975820902075,-0.849976343347942,-0.847571115569945,
-0.84431636718101,-0.838050651751994,-0.830081547811707,-0.811369770786281,
-0.770038718874264,-0.757673886359593,-0.754681189889249,-0.752955156507968,
-0.751602403878788,-0.74970556619611,-0.745807973286562,-0.74062067838746,
-0.727590901734445,-0.688640449053001,-0.665367696956002,-0.660070769465804,
-0.656989085533034,-0.654326136787533,-0.651059537064942,-0.644735961771175,
-0.607644871700186,-0.566942885259483,-0.562339545667482,-0.560332770647229,
-0.558821431547906,-0.557129108857349,-0.554210772635803,-0.541587226277578,
-0.512481966633443,-0.475900708408141,-0.468210944966627,-0.464719486296983,
-0.462025838666575,-0.459111181434841,-0.454440292483736,-0.43800874162127,
-0.384560180050917,-0.371264718516689,-0.368207345636911,-0.366466373572813,
-0.364979287713289,-0.363028789375391,-0.358853087871692,-0.330670806325827,
-0.281389189774354,-0.274471941641788,-0.271087335097601,-0.268414552712803,
-0.26541362182941,-0.260347862576554,-0.23884078735134,-0.211095868981101,
-0.181048084277188,-0.176095616844316,-0.174154413701037,-0.172748376948766,
-0.17122194460444,-0.169094856309564,-0.166569417164278,-0.1619767698802,
-0.151105029433998,-0.0978381037468989,-0.0839777173712444,-0.0794197387270606,
-0.0765296024105952,-0.073826943794206,-0.0702157250734403,-0.062067537268756,
-0.050882973528803,-0.000574376623881859),.UNSPECIFIED.);
#1162=B_SPLINE_CURVE_WITH_KNOTS('',3,(#22903,#22904,#22905,#22906,#22907,
#22908,#22909,#22910,#22911,#22912,#22913,#22914,#22915,#22916,#22917,#22918,
#22919,#22920,#22921,#22922,#22923,#22924,#22925,#22926,#22927,#22928,#22929,
#22930,#22931,#22932,#22933,#22934,#22935,#22936,#22937,#22938,#22939,#22940,
#22941,#22942,#22943,#22944,#22945,#22946,#22947,#22948,#22949,#22950,#22951,
#22952,#22953,#22954,#22955,#22956,#22957,#22958,#22959,#22960,#22961,#22962,
#22963,#22964,#22965,#22966,#22967,#22968,#22969,#22970,#22971,#22972,#22973,
#22974,#22975,#22976,#22977,#22978,#22979,#22980,#22981,#22982,#22983,#22984,
#22985,#22986,#22987,#22988,#22989,#22990,#22991,#22992,#22993,#22994,#22995,
#22996,#22997,#22998,#22999,#23000,#23001,#23002,#23003,#23004,#23005,#23006,
#23007,#23008,#23009,#23010,#23011,#23012,#23013,#23014,#23015,#23016,#23017,
#23018,#23019,#23020,#23021,#23022,#23023,#23024,#23025,#23026,#23027,#23028,
#23029,#23030,#23031,#23032),.UNSPECIFIED.,.F.,.F.,(4,2,2,2,2,2,2,2,2,2,
2,2,2,2,2,2,2,2,2,2,2,2,2,2,2,2,2,2,2,2,2,2,2,2,2,2,2,2,2,2,2,2,2,2,2,2,
2,2,2,2,2,2,2,2,2,2,2,2,2,2,2,2,2,2,4),(-2.43101907711719,-2.4201435497811,
-2.41446115353093,-2.41244095905634,-2.4109370374652,-2.409500923963,-2.40784459936654,
-2.40508954469771,-2.39574741320926,-2.38292146361354,-2.34823399544202,
-2.32258381158638,-2.31728473374966,-2.31423321738437,-2.31156737387828,
-2.30825986190856,-2.30314227594429,-2.26685454718313,-2.240844590539,-2.22820931205344,
-2.22312722866662,-2.21932249573791,-2.21745208274786,-2.21744545958929,
-2.21743877481767,-2.21743202798643,-2.21742521798897,-2.21741834407562,
-2.21741140573566,-2.2174044021135,-2.21739733223398,-2.21739019518902,
-2.21738299025269,-2.21737571665299,-2.21736837358268,-2.2173609600107,
-2.21735347508426,-2.21734591824579,-2.21733828827653,-2.21733058430711,
-2.21732280549441,-2.21731495081584,-2.21730701928989,-2.21729900993269,
-2.21729092185761,-2.21728275405164,-2.21727450538882,-2.21726617507049,
-2.21725776191911,-2.21724926482013,-2.21724068268989,-2.21723201446122,
-2.21722325925826,-2.21721441571959,-2.21720548263654,-2.21719645901663,
-2.21718734360108,-2.21717813541115,-2.21716883304915,-2.21715943530605,
-2.21566153841624,-2.21374197653291,-2.21063311736965,-2.1896358019075,
-2.18915184178403),.UNSPECIFIED.);
#1163=B_SPLINE_CURVE_WITH_KNOTS('',3,(#23034,#23035,#23036,#23037,#23038,
#23039,#23040,#23041,#23042,#23043,#23044,#23045,#23046,#23047,#23048,#23049,
#23050,#23051,#23052,#23053,#23054,#23055,#23056,#23057,#23058,#23059,#23060,
#23061,#23062,#23063,#23064,#23065,#23066,#23067,#23068,#23069,#23070,#23071,
#23072,#23073,#23074,#23075,#23076,#23077),.UNSPECIFIED.,.F.,.F.,(4,2,2,
2,2,2,2,2,2,2,2,2,2,2,2,2,2,2,2,2,2,4),(-0.242785158976033,-0.241227316072973,
-0.235044448781371,-0.227208788780809,-0.208968798338147,-0.164855613220994,
-0.154238467454242,-0.151361302165026,-0.149678282332967,-0.148164701370528,
-0.146105001164423,-0.141515626576424,-0.117068669363286,-0.092648514982216,
-0.0627097051517281,-0.0576267011093042,-0.0543300841093095,-0.0516656013047632,
-0.0486075016806466,-0.0454116381819875,-0.0405346762332557,-0.000573798641427919),
 .UNSPECIFIED.);
#1164=B_SPLINE_CURVE_WITH_KNOTS('',3,(#23078,#23079,#23080,#23081,#23082,
#23083,#23084,#23085,#23086,#23087,#23088,#23089,#23090,#23091,#23092,#23093,
#23094,#23095,#23096,#23097,#23098,#23099,#23100,#23101,#23102,#23103,#23104,
#23105,#23106,#23107,#23108,#23109,#23110,#23111,#23112,#23113,#23114,#23115,
#23116,#23117,#23118,#23119,#23120,#23121,#23122,#23123,#23124,#23125,#23126,
#23127,#23128,#23129,#23130,#23131,#23132,#23133,#23134,#23135,#23136,#23137,
#23138,#23139,#23140,#23141,#23142,#23143,#23144,#23145,#23146,#23147,#23148,
#23149,#23150,#23151,#23152,#23153,#23154,#23155,#23156,#23157,#23158,#23159,
#23160,#23161,#23162,#23163,#23164,#23165,#23166,#23167,#23168,#23169,#23170,
#23171,#23172,#23173,#23174,#23175,#23176,#23177,#23178,#23179,#23180,#23181,
#23182,#23183,#23184,#23185,#23186,#23187,#23188,#23189,#23190,#23191,#23192,
#23193,#23194,#23195,#23196,#23197,#23198,#23199,#23200,#23201,#23202,#23203,
#23204,#23205,#23206,#23207,#23208,#23209,#23210,#23211,#23212,#23213,#23214,
#23215,#23216,#23217,#23218,#23219,#23220,#23221,#23222,#23223,#23224,#23225,
#23226,#23227,#23228),.UNSPECIFIED.,.F.,.F.,(4,3,3,3,3,3,3,3,3,3,3,3,3,
3,3,3,3,3,3,3,3,3,3,3,3,3,3,3,3,3,3,3,3,3,3,3,3,3,3,3,3,3,3,3,3,3,3,3,3,
3,4),(53.4070751110264,53.5488498236995,53.6381223040877,53.7439426673302,
53.8496026361662,53.9551376190527,54.0606061171701,54.1660446288859,54.2714896077376,
54.3770477039605,54.4826696481002,54.5884747927751,54.6373030663835,54.743123429626,
54.8487833984619,54.9543183813483,55.0597868794657,55.1652253911815,55.2706703700334,
55.3762284662562,55.481850410396,55.5876555550709,55.6364838286793,55.7423041919218,
55.8479641607577,55.9534991436442,56.0589676417616,56.1644061534774,56.2698511323292,
56.3754092285521,56.4810311726919,56.5868363173668,56.6356645909751,56.7414849542176,
56.8471449230535,56.95267990594,57.0581484040574,57.1635869157733,57.2690318946251,
57.374589990848,57.4802119349878,57.5860170796627,57.6348453532709,57.7406331779413,
57.8462753337061,57.9518085486852,58.0572694189163,58.1627286964347,58.2681840438519,
58.3737305088498,58.438333049783),.UNSPECIFIED.);
#1165=B_SPLINE_CURVE_WITH_KNOTS('',3,(#23233,#23234,#23235,#23236,#23237,
#23238,#23239,#23240,#23241,#23242,#23243,#23244,#23245,#23246,#23247,#23248,
#23249,#23250,#23251,#23252,#23253,#23254,#23255,#23256,#23257,#23258,#23259,
#23260,#23261,#23262,#23263,#23264,#23265,#23266,#23267,#23268,#23269,#23270,
#23271,#23272,#23273,#23274,#23275,#23276,#23277,#23278,#23279,#23280,#23281,
#23282,#23283,#23284,#23285,#23286,#23287,#23288,#23289,#23290,#23291,#23292,
#23293,#23294,#23295,#23296,#23297,#23298,#23299,#23300,#23301,#23302,#23303,
#23304,#23305,#23306,#23307,#23308,#23309,#23310,#23311,#23312,#23313,#23314,
#23315,#23316,#23317,#23318,#23319,#23320,#23321,#23322,#23323,#23324,#23325,
#23326,#23327,#23328,#23329,#23330,#23331,#23332,#23333,#23334,#23335,#23336,
#23337,#23338,#23339,#23340,#23341,#23342,#23343,#23344,#23345,#23346,#23347,
#23348,#23349,#23350,#23351,#23352,#23353,#23354,#23355,#23356,#23357,#23358,
#23359,#23360,#23361,#23362,#23363,#23364,#23365,#23366,#23367,#23368,#23369,
#23370,#23371,#23372,#23373,#23374,#23375,#23376,#23377,#23378,#23379,#23380,
#23381,#23382,#23383,#23384,#23385,#23386,#23387,#23388,#23389,#23390,#23391,
#23392,#23393,#23394,#23395,#23396,#23397,#23398,#23399,#23400,#23401,#23402,
#23403,#23404,#23405,#23406,#23407,#23408,#23409,#23410,#23411,#23412,#23413,
#23414,#23415,#23416,#23417,#23418,#23419,#23420,#23421,#23422,#23423,#23424,
#23425,#23426,#23427,#23428,#23429,#23430,#23431,#23432,#23433,#23434,#23435,
#23436,#23437,#23438),.UNSPECIFIED.,.F.,.F.,(4,2,2,2,2,2,2,2,2,2,2,2,2,
2,2,2,2,2,2,2,2,2,2,2,2,2,2,2,2,2,2,2,2,2,2,2,2,2,2,2,2,2,2,2,2,2,2,2,2,
2,2,2,2,2,2,2,2,2,2,2,2,2,2,2,2,2,2,2,2,2,2,2,2,2,2,2,2,2,2,2,2,2,2,2,2,
2,2,2,2,2,2,2,2,2,2,2,2,2,2,2,2,2,4),(-2.189001750981,-2.14225794250904,
-2.11149306444298,-2.10767380722915,-2.10579262300464,-2.10444175848357,
-2.10270521951084,-2.09966569351592,-2.08662571360936,-2.08131111737203,
-2.07758280351107,-2.04317976059327,-2.01775494815292,-2.01246798904254,
-2.00941961035485,-2.00675424740815,-2.00344439262422,-1.99831751517754,
-1.96506045065472,-1.92186946920969,-1.91553026636808,-1.91322909264721,
-1.9116718380376,-1.9102661305893,-1.90832535526835,-1.90337380772395,-1.8725717084742,
-1.84020013229762,-1.82343242970201,-1.81873147053482,-1.81581056814682,
-1.8131195384669,-1.80964327519445,-1.80203615956091,-1.76150922799894,
-1.73919681621692,-1.72890645338217,-1.72238784261669,-1.72006195559318,
-1.71849959533238,-1.71709832776201,-1.71517512064348,-1.71032859246593,
-1.67550056100348,-1.63295953315827,-1.62672164201925,-1.62347278327525,
-1.62081112223071,-1.61771606136226,-1.6123588178702,-1.58798198472502,
-1.54976824761276,-1.53091804545937,-1.52767917739744,-1.5259175089066,
-1.52441933182097,-1.52249195669889,-1.51935603948711,-1.49646617107584,
-1.46899890230181,-1.4411879861954,-1.43406339052084,-1.43063938873421,
-1.4279628061315,-1.42498582254446,-1.42002804972072,-1.40262899828603,
-1.36290024948229,-1.34584224522774,-1.33662599841886,-1.33398803534395,
-1.33235780167674,-1.33083974129108,-1.32900280833424,-1.32433863369126,
-1.28428918802367,-1.27846229687321,-1.25063430291216,-1.24170277689903,
-1.23795922699513,-1.23523472839415,-1.2323911005675,-1.22804851800325,
-1.21589747069481,-1.19601363549382,-1.15347748098336,-1.14371425460895,
-1.1409151249908,-1.13924915491815,-1.13772948436155,-1.13563157467613,
-1.13062475074033,-1.1234308251802,-1.10157858815624,-1.05486202190455,
-1.04765304364835,-1.0442129006471,-1.04153428988957,-1.03856586990926,
-1.03364785696611,-1.01424781010532,-0.991532890587958,-0.973989629254837),
 .UNSPECIFIED.);
#1166=B_SPLINE_CURVE_WITH_KNOTS('',3,(#23440,#23441,#23442,#23443,#23444,
#23445,#23446,#23447,#23448,#23449,#23450,#23451,#23452,#23453,#23454,#23455,
#23456,#23457,#23458,#23459,#23460,#23461,#23462,#23463,#23464,#23465,#23466,
#23467,#23468,#23469,#23470,#23471,#23472,#23473,#23474,#23475,#23476,#23477,
#23478,#23479),.UNSPECIFIED.,.F.,.F.,(4,3,3,3,3,3,3,3,3,3,3,3,3,4),(58.438333049783,
58.5441224300846,58.6340261155667,58.7398464788092,58.8455064476451,58.9510414305316,
59.0565099286489,59.1619484403647,59.2673934192164,59.3729515154392,59.478573459579,
59.5843786042538,59.6332068778625,59.6902604182061),.UNSPECIFIED.);
#1167=B_SPLINE_CURVE_WITH_KNOTS('',3,(#23480,#23481,#23482,#23483,#23484,
#23485,#23486,#23487,#23488),.UNSPECIFIED.,.F.,.F.,(4,1,1,1,1,1,4),(59.6902673029908,
60.6323876401583,61.6315684024541,62.6307491647499,63.6299299270457,64.6291106893415,
64.7226639182745),.UNSPECIFIED.);
#1168=B_SPLINE_CURVE_WITH_KNOTS('',3,(#23494,#23495,#23496,#23497,#23498,
#23499,#23500,#23501,#23502),.UNSPECIFIED.,.F.,.F.,(4,1,1,1,1,1,4),(65.9734520027693,
66.2860804764019,67.2852612386977,68.2844420009935,69.2836227632893,70.2828035255851,
71.0044067958708),.UNSPECIFIED.);
#1169=B_SPLINE_CURVE_WITH_KNOTS('',3,(#23503,#23504,#23505,#23506,#23507,
#23508,#23509,#23510,#23511,#23512,#23513,#23514,#23515,#23516,#23517,#23518,
#23519,#23520,#23521,#23522,#23523,#23524,#23525,#23526,#23527,#23528,#23529,
#23530,#23531,#23532,#23533,#23534,#23535,#23536,#23537,#23538,#23539,#23540,
#23541,#23542,#23543,#23544,#23545,#23546,#23547,#23548,#23549,#23550,#23551,
#23552,#23553,#23554,#23555,#23556,#23557,#23558,#23559,#23560,#23561,#23562,
#23563,#23564,#23565,#23566,#23567,#23568,#23569,#23570,#23571,#23572,#23573,
#23574,#23575,#23576,#23577,#23578,#23579,#23580,#23581,#23582,#23583,#23584,
#23585,#23586,#23587,#23588,#23589,#23590,#23591,#23592,#23593,#23594,#23595,
#23596,#23597,#23598,#23599,#23600,#23601,#23602,#23603,#23604,#23605,#23606,
#23607,#23608,#23609,#23610),.UNSPECIFIED.,.F.,.F.,(4,2,2,2,2,2,2,2,2,2,
2,2,2,2,2,2,2,2,2,2,2,2,2,2,2,2,2,2,2,2,2,2,2,2,2,2,2,2,2,2,2,2,2,2,2,2,
2,2,2,2,2,2,2,4),(-2.43103019217924,-2.41217091518336,-2.40266616406287,
-2.39929537754217,-2.39668852902964,-2.39400774005481,-2.39105235808666,
-2.3861918764179,-2.3695930752094,-2.35000957128429,-2.30999805620414,-2.3048060717791,
-2.30090625589495,-2.29900927956527,-2.2976568206229,-2.29593167669591,
-2.29294169404183,-2.28060525376839,-2.27405386106923,-2.2428478186499,
-2.22185086546765,-2.21326197753705,-2.20666897445879,-2.2034488225326,
-2.20343115831572,-2.20341246364597,-2.20339267491428,-2.20337172420637,
-2.20334953900008,-2.20332604187673,-2.20330114998533,-2.20327477463628,
-2.20324682097543,-2.20321718749107,-2.20318576532779,-2.20315243785984,
-2.20311707992428,-2.20307955727866,-2.20303972585846,-2.20299743086428,
-2.2029525060551,-2.20290477272776,-2.20285403884808,-2.20280009795184,
-2.20274272813671,-2.20268169089799,-2.20263697406887,-2.20257699048357,
-2.20249652378171,-2.202388585695,-2.19971090533018,-2.19627453084266,-2.18908317483088,
-2.189001750981),.UNSPECIFIED.);
#1170=B_SPLINE_CURVE_WITH_KNOTS('',3,(#23612,#23613,#23614,#23615,#23616),
 .UNSPECIFIED.,.F.,.F.,(4,1,4),(64.7226639182745,65.6282914516373,65.9734383180058),
 .UNSPECIFIED.);
#1171=B_SPLINE_CURVE_WITH_KNOTS('',3,(#23617,#23618,#23619,#23620,#23621,
#23622,#23623,#23624,#23625,#23626,#23627,#23628,#23629,#23630,#23631,#23632,
#23633,#23634,#23635,#23636,#23637,#23638,#23639,#23640,#23641,#23642,#23643,
#23644,#23645,#23646,#23647,#23648,#23649,#23650,#23651,#23652,#23653,#23654,
#23655,#23656,#23657,#23658,#23659,#23660,#23661,#23662,#23663,#23664,#23665,
#23666,#23667,#23668,#23669,#23670,#23671,#23672,#23673,#23674,#23675,#23676,
#23677,#23678,#23679,#23680,#23681,#23682,#23683,#23684,#23685,#23686,#23687,
#23688,#23689,#23690,#23691,#23692,#23693,#23694,#23695,#23696,#23697,#23698,
#23699,#23700,#23701,#23702,#23703,#23704,#23705,#23706,#23707,#23708,#23709,
#23710,#23711,#23712,#23713,#23714,#23715,#23716,#23717,#23718,#23719,#23720,
#23721,#23722,#23723,#23724,#23725,#23726,#23727,#23728,#23729,#23730,#23731,
#23732,#23733,#23734,#23735,#23736,#23737,#23738,#23739,#23740,#23741,#23742,
#23743,#23744,#23745,#23746,#23747,#23748,#23749,#23750,#23751,#23752,#23753,
#23754,#23755,#23756,#23757,#23758,#23759,#23760,#23761,#23762,#23763,#23764,
#23765,#23766,#23767,#23768,#23769,#23770,#23771,#23772,#23773,#23774,#23775,
#23776,#23777,#23778,#23779,#23780,#23781,#23782,#23783,#23784,#23785,#23786,
#23787,#23788,#23789,#23790,#23791,#23792),.UNSPECIFIED.,.F.,.F.,(4,2,2,
2,2,2,2,2,2,2,2,2,2,2,2,2,2,2,2,2,2,2,2,2,2,2,2,2,2,2,2,2,2,2,2,2,2,2,2,
2,2,2,2,2,2,2,2,2,2,2,2,2,2,2,2,2,2,2,2,2,2,2,2,2,2,2,2,2,2,2,2,2,2,2,2,
2,2,2,2,2,2,2,2,2,2,2,2,4),(-2.43122156991905,-2.41740188853736,-2.4093327733779,
-2.40590964227835,-2.4032856118482,-2.40072669449692,-2.39783687629169,
-2.39327630227369,-2.37938394661034,-2.35744382917557,-2.31469050536173,
-2.30837579829069,-2.30607838843393,-2.30452217671395,-2.30311624872971,
-2.30117371357907,-2.29621020343292,-2.26662662311645,-2.24085266165562,
-2.2252094959536,-2.21813981860739,-2.21405477499885,-2.21042245807682,
-2.20774918356246,-2.20524828129091,-2.20121608808074,-2.19118114876341,
-2.14506180475598,-2.1409661220333,-2.11722528897416,-2.11384007303311,
-2.11204760675826,-2.11055229022504,-2.10866537196592,-2.10566413752689,
-2.08818712863389,-2.07437502791,-2.04036593179245,-2.02314655945143,-2.01840598438993,
-2.01547675198109,-2.01278887666726,-2.00933181003124,-2.00182875647805,
-1.95885090316993,-1.94832763199638,-1.92402418771038,-1.92062621899117,
-1.91883102801624,-1.9173357913925,-1.91545194236067,-1.91246104236256,
-1.89524555958718,-1.88160975532147,-1.84724874496579,-1.82993540816725,
-1.82518651326017,-1.82225538142978,-1.81956790872277,-1.81611434207564,
-1.80863100464044,-1.76528520350111,-1.73176870790186,-1.72775452305202,
-1.72583522224988,-1.72433776182905,-1.7225704142123,-1.71939490784715,
-1.70412150133219,-1.65262819098408,-1.64188440756512,-1.63398231757764,
-1.63041523817908,-1.62771998166277,-1.62481325919949,-1.6201762290837,
-1.60563418704462,-1.55868324364107,-1.5441942441099,-1.53863120870868,
-1.53451720653437,-1.53257881871942,-1.53109340826038,-1.5293454572945,
-1.52625567310631,-1.51247154949388,-1.47891218751976,-1.45794880066605),
 .UNSPECIFIED.);
#1172=B_SPLINE_CURVE_WITH_KNOTS('',3,(#23798,#23799,#23800,#23801,#23802,
#23803,#23804,#23805,#23806,#23807,#23808,#23809,#23810,#23811,#23812,#23813,
#23814,#23815,#23816,#23817,#23818,#23819,#23820,#23821,#23822,#23823,#23824,
#23825,#23826,#23827,#23828,#23829,#23830,#23831,#23832,#23833,#23834,#23835,
#23836,#23837,#23838,#23839,#23840,#23841,#23842,#23843,#23844,#23845,#23846,
#23847,#23848,#23849,#23850,#23851,#23852,#23853,#23854,#23855,#23856,#23857,
#23858,#23859,#23860,#23861,#23862,#23863,#23864,#23865,#23866,#23867,#23868,
#23869,#23870,#23871,#23872,#23873,#23874,#23875,#23876,#23877,#23878,#23879,
#23880,#23881,#23882,#23883,#23884,#23885,#23886,#23887,#23888,#23889,#23890,
#23891,#23892,#23893,#23894,#23895,#23896,#23897,#23898,#23899,#23900,#23901,
#23902,#23903,#23904,#23905,#23906,#23907,#23908,#23909,#23910,#23911,#23912,
#23913,#23914,#23915,#23916,#23917,#23918,#23919,#23920,#23921,#23922,#23923,
#23924,#23925,#23926,#23927,#23928,#23929,#23930,#23931,#23932,#23933,#23934,
#23935,#23936,#23937,#23938,#23939,#23940,#23941,#23942,#23943,#23944,#23945,
#23946,#23947,#23948,#23949,#23950,#23951,#23952,#23953,#23954),
 .UNSPECIFIED.,.F.,.F.,(4,3,3,3,3,3,3,3,3,3,3,3,3,3,3,3,3,3,3,3,3,3,3,3,
3,3,3,3,3,3,3,3,3,3,3,3,3,3,3,3,3,3,3,3,3,3,3,3,3,3,3,3,4),(72.2566310325652,
72.2811650501767,72.3869854134193,72.4926453822552,72.5981803651418,72.7036488632592,
72.809087374975,72.9145323538269,73.0200904500499,73.1257123941897,73.2315175388647,
73.2803458124725,73.386166175715,73.4918261445509,73.5973611274374,73.7028296255547,
73.8082681372705,73.9137131161223,74.0192712123451,74.1248931564849,74.2306983011597,
74.2795265747683,74.3853469380109,74.4910069068467,74.5965418897333,74.7020103878507,
74.8074488995665,74.9128938784183,75.0184519746412,75.124073918781,75.2298790634559,
75.2787073370641,75.3845277003066,75.4901876691425,75.595722652029,75.7011911501463,
75.8066296618621,75.9120746407139,76.0176327369367,76.1232546810765,76.2290598257514,
76.2778880993599,76.3837084626024,76.4893684314383,76.5949034143247,76.7003719124421,
76.8058104241579,76.9112554030097,77.0168134992326,77.1224354433723,77.2282405880472,
77.2770688616556,77.2885547891013),.UNSPECIFIED.);
#1173=B_SPLINE_CURVE_WITH_KNOTS('',3,(#23955,#23956,#23957,#23958,#23959),
 .UNSPECIFIED.,.F.,.F.,(4,1,4),(71.0044067958708,71.2819842878809,72.256627539715),
 .UNSPECIFIED.);
#1174=B_SPLINE_CURVE_WITH_KNOTS('',3,(#23960,#23961,#23962,#23963,#23964,
#23965,#23966,#23967,#23968,#23969,#23970,#23971,#23972,#23973,#23974,#23975,
#23976,#23977,#23978,#23979,#23980,#23981,#23982,#23983,#23984,#23985,#23986,
#23987,#23988,#23989,#23990,#23991,#23992,#23993,#23994,#23995,#23996,#23997,
#23998,#23999,#24000,#24001,#24002,#24003,#24004,#24005,#24006,#24007,#24008,
#24009,#24010,#24011,#24012,#24013,#24014,#24015,#24016,#24017,#24018,#24019,
#24020,#24021,#24022,#24023,#24024,#24025,#24026,#24027,#24028,#24029,#24030,
#24031,#24032,#24033,#24034,#24035,#24036,#24037,#24038,#24039,#24040,#24041,
#24042,#24043,#24044,#24045,#24046,#24047,#24048,#24049,#24050,#24051,#24052,
#24053,#24054,#24055,#24056,#24057,#24058,#24059,#24060,#24061,#24062,#24063,
#24064,#24065,#24066,#24067,#24068,#24069,#24070,#24071,#24072,#24073,#24074,
#24075,#24076,#24077,#24078,#24079,#24080,#24081,#24082,#24083,#24084,#24085,
#24086,#24087,#24088,#24089,#24090,#24091,#24092,#24093,#24094,#24095,#24096,
#24097,#24098,#24099,#24100,#24101,#24102,#24103,#24104,#24105,#24106,#24107,
#24108,#24109,#24110,#24111,#24112,#24113,#24114,#24115,#24116,#24117,#24118,
#24119,#24120,#24121,#24122,#24123,#24124,#24125,#24126,#24127,#24128,#24129,
#24130,#24131,#24132,#24133,#24134,#24135,#24136,#24137,#24138,#24139,#24140,
#24141,#24142,#24143,#24144,#24145,#24146,#24147,#24148,#24149,#24150,#24151,
#24152,#24153,#24154,#24155,#24156,#24157,#24158,#24159,#24160,#24161,#24162,
#24163,#24164,#24165,#24166,#24167,#24168,#24169,#24170,#24171,#24172,#24173,
#24174,#24175,#24176,#24177,#24178,#24179,#24180,#24181),.UNSPECIFIED.,
 .F.,.F.,(4,2,2,2,2,2,2,2,2,2,2,2,2,2,2,2,2,2,2,2,2,2,2,2,2,2,2,2,2,2,2,
2,2,2,2,2,2,2,2,2,2,2,2,2,2,2,2,2,2,2,2,2,2,2,2,2,2,2,2,2,2,2,2,2,2,2,2,
2,2,2,2,2,2,2,2,2,2,2,2,2,2,2,2,2,2,2,2,2,2,2,2,2,2,2,2,2,2,2,2,2,2,2,2,
2,2,2,2,2,2,2,4),(-1.45794880066605,-1.44624583571765,-1.43988442584939,
-1.43661057713039,-1.43394773679398,-1.43087290480914,-1.42560445174949,
-1.40283074358948,-1.36365295036055,-1.35037177699628,-1.3451186259298,
-1.34118311006444,-1.33927907839669,-1.33792574755609,-1.33620524424236,
-1.33323582115914,-1.32117645524588,-1.31414670900283,-1.28263613648096,
-1.25432591061907,-1.24713909071555,-1.24370345531477,-1.24102573820999,
-1.23805564787756,-1.23312863735979,-1.21583347700753,-1.18497150596766,
-1.15355369204604,-1.14860798580015,-1.14666826839542,-1.1452628842504,
-1.14370546287263,-1.14140320700633,-1.13505565425296,-1.09171147953475,
-1.05863054385238,-1.05350572852608,-1.05019650976018,-1.04753124311002,
-1.04448253104394,-1.03919389959753,-1.01374196838361,-0.979244378436831,
-0.968515689473857,-0.956998261618626,-0.954042680044054,-0.952342440646011,
-0.950833670468636,-0.948807974718877,-0.944218910033777,-0.923529693423371,
-0.887367842065201,-0.864747161548468,-0.859487633063125,-0.856414765503111,
-0.853751675864774,-0.850475033727133,-0.844100159448475,-0.835953623514413,
-0.816602813065972,-0.781181109754996,-0.77816482347728,-0.76410347150806,
-0.760998252123578,-0.759246768097607,-0.757747476756573,-0.755806015301985,
-0.751676037795849,-0.746085610191573,-0.731488182406631,-0.682244381522221,
-0.669687503721353,-0.665292923386707,-0.662438501485609,-0.659720558330306,
-0.656012876785706,-0.647296464341834,-0.618761573177164,-0.586297399801915,
-0.570972098293276,-0.567793724762032,-0.566025764400172,-0.564528403530472,
-0.562610041717839,-0.55860056303628,-0.553220146140338,-0.539449872453238,
-0.498283151384905,-0.477975133994351,-0.47280529456626,-0.469782366597916,
-0.46738088870423,-0.464160365097725,-0.458059881052783,-0.418238394251748,
-0.38016866975499,-0.375480296488304,-0.37358407013704,-0.372051004934755,
-0.370446495475348,-0.367924749888287,-0.359816415676196,-0.345759603294467,
-0.302983491661031,-0.284454747495694,-0.279418354307256,-0.276424414403936,
-0.274018760713709,-0.270757045763547,-0.264455664153103,-0.242747535804741),
 .UNSPECIFIED.);
#1175=B_SPLINE_CURVE_WITH_KNOTS('',3,(#24187,#24188,#24189,#24190,#24191,
#24192,#24193,#24194,#24195,#24196,#24197,#24198,#24199,#24200,#24201,#24202,
#24203,#24204,#24205,#24206,#24207,#24208,#24209,#24210,#24211,#24212,#24213,
#24214,#24215,#24216,#24217,#24218,#24219,#24220,#24221,#24222,#24223,#24224,
#24225,#24226,#24227,#24228,#24229,#24230,#24231,#24232,#24233,#24234,#24235,
#24236,#24237,#24238,#24239,#24240,#24241,#24242,#24243,#24244,#24245,#24246,
#24247,#24248,#24249,#24250,#24251,#24252,#24253,#24254,#24255,#24256,#24257,
#24258,#24259,#24260,#24261,#24262,#24263,#24264,#24265,#24266,#24267,#24268,
#24269,#24270,#24271,#24272,#24273,#24274,#24275,#24276,#24277,#24278,#24279,
#24280,#24281,#24282,#24283,#24284,#24285,#24286,#24287,#24288,#24289,#24290,
#24291,#24292,#24293,#24294,#24295,#24296,#24297,#24298,#24299,#24300,#24301,
#24302,#24303,#24304,#24305,#24306,#24307,#24308,#24309,#24310,#24311,#24312,
#24313,#24314,#24315,#24316,#24317,#24318,#24319,#24320,#24321,#24322,#24323,
#24324,#24325,#24326,#24327,#24328,#24329,#24330,#24331,#24332,#24333,#24334,
#24335,#24336,#24337,#24338,#24339,#24340,#24341,#24342,#24343,#24344,#24345,
#24346,#24347,#24348,#24349,#24350,#24351,#24352,#24353,#24354,#24355,#24356,
#24357,#24358,#24359,#24360),.UNSPECIFIED.,.F.,.F.,(4,2,2,2,2,2,2,2,2,2,
2,2,2,2,2,2,2,2,2,2,2,2,2,2,2,2,2,2,2,2,2,2,2,2,2,2,2,2,2,2,2,2,2,2,2,2,
2,2,2,2,2,2,2,2,2,2,2,2,2,2,2,2,2,2,2,2,2,2,2,2,2,2,2,2,2,2,2,2,2,2,2,2,
2,2,2,2,4),(-0.973882930196809,-0.944219937250399,-0.921904536119179,-0.918777710195008,
-0.91685282360926,-0.915354543274545,-0.913590344154815,-0.91034076376922,
-0.891213882423294,-0.852451212595539,-0.844176821288675,-0.827850967344199,
-0.823016528795024,-0.820066095282667,-0.81738273765496,-0.813906840357539,
-0.806508943917871,-0.776464141743833,-0.76839603253496,-0.730722904709127,
-0.726018052964024,-0.724118672175214,-0.722584467970821,-0.72098046981968,
-0.718462445648489,-0.71039140922058,-0.696431000629615,-0.654238625258667,
-0.635090389733211,-0.629998336572393,-0.626991719434676,-0.624587153286583,
-0.621341639154425,-0.615122516984872,-0.60722902830931,-0.588787258900323,
-0.562682126076683,-0.535520250092716,-0.532346444750821,-0.530407652113421,
-0.5289082615078,-0.527154085472223,-0.52395125884013,-0.50602312727782,
-0.479496203386512,-0.442948143474137,-0.437823682432759,-0.434514084214073,
-0.431848104869673,-0.42879812173562,-0.423506074937283,-0.398004075686,
-0.363228067327037,-0.352443867188458,-0.341265491734738,-0.338338188761974,
-0.33664385964487,-0.33513298368972,-0.333094430513295,-0.32843449508106,
-0.307084319225128,-0.276704102858013,-0.249475516282498,-0.243993774060742,
-0.240870156261451,-0.238234585146884,-0.235028725449389,-0.229158204643075,
-0.221721078250796,-0.204858344090895,-0.164049181648068,-0.148561766286696,
-0.145373992918243,-0.143603540342072,-0.142105807475087,-0.14018915712708,
-0.136376403077181,-0.105253522109437,-0.0818081601489447,-0.056113797427619,
-0.050699364712091,-0.0475907848367115,-0.0449544151876206,-0.0417309778911177,
-0.038301942588913,-0.0328593950830175,-0.000573591561804652),
 .UNSPECIFIED.);
#1176=B_SPLINE_CURVE_WITH_KNOTS('',3,(#24361,#24362,#24363,#24364,#24365,
#24366,#24367,#24368,#24369,#24370,#24371,#24372,#24373,#24374,#24375,#24376,
#24377,#24378,#24379,#24380,#24381,#24382,#24383,#24384,#24385,#24386,#24387,
#24388,#24389,#24390,#24391,#24392,#24393,#24394,#24395,#24396,#24397),
 .UNSPECIFIED.,.F.,.F.,(4,3,3,3,3,3,3,3,3,3,3,3,4),(77.2885547891013,77.3943557879778,
77.5045925174745,77.6101150423719,77.7155766333603,77.8210137795483,77.9264629309739,
78.0320286129095,78.1376631195039,78.2434760803445,78.2762496239514,78.4105186845177,
78.5398163394612),.UNSPECIFIED.);
#1177=B_SPLINE_CURVE_WITH_KNOTS('',3,(#24399,#24400,#24401,#24402,#24403,
#24404,#24405,#24406,#24407,#24408,#24409,#24410,#24411,#24412,#24413,#24414,
#24415,#24416,#24417,#24418,#24419,#24420,#24421,#24422,#24423,#24424,#24425,
#24426,#24427,#24428,#24429,#24430,#24431,#24432,#24433,#24434,#24435,#24436),
 .UNSPECIFIED.,.F.,.F.,(4,2,2,2,2,2,2,2,2,2,2,2,2,2,2,2,2,2,4),(-0.242747535804741,
-0.223836868626812,-0.186992156459622,-0.18223779622474,-0.180330219392406,
-0.178932872265027,-0.177397228214326,-0.175215061136868,-0.172619024178979,
-0.167839411107292,-0.119303502477546,-0.0920807826407651,-0.0866003096148791,
-0.0834775358710877,-0.0808427586427267,-0.0776379762208395,-0.0716139334229604,
-0.0340705181892316,-0.000574328313784234),.UNSPECIFIED.);
#1178=B_SPLINE_CURVE_WITH_KNOTS('',3,(#24437,#24438,#24439,#24440,#24441,
#24442,#24443,#24444,#24445,#24446,#24447,#24448,#24449,#24450,#24451,#24452,
#24453,#24454,#24455,#24456,#24457,#24458,#24459,#24460,#24461,#24462,#24463,
#24464,#24465,#24466,#24467,#24468,#24469,#24470,#24471,#24472,#24473,#24474,
#24475,#24476,#24477,#24478,#24479,#24480,#24481,#24482,#24483,#24484,#24485,
#24486,#24487,#24488,#24489,#24490,#24491,#24492,#24493,#24494,#24495,#24496,
#24497,#24498,#24499,#24500,#24501,#24502,#24503,#24504,#24505,#24506,#24507,
#24508,#24509,#24510,#24511,#24512,#24513,#24514,#24515,#24516,#24517,#24518,
#24519,#24520,#24521,#24522,#24523,#24524,#24525,#24526,#24527,#24528,#24529,
#24530,#24531,#24532,#24533,#24534,#24535,#24536,#24537,#24538,#24539,#24540,
#24541,#24542,#24543,#24544,#24545,#24546,#24547,#24548,#24549,#24550,#24551,
#24552,#24553,#24554,#24555,#24556,#24557,#24558,#24559,#24560,#24561,#24562,
#24563,#24564,#24565,#24566,#24567,#24568,#24569,#24570,#24571,#24572,#24573,
#24574,#24575,#24576,#24577,#24578,#24579,#24580,#24581,#24582,#24583,#24584,
#24585,#24586,#24587,#24588,#24589,#24590,#24591,#24592,#24593,#24594,#24595,
#24596,#24597,#24598,#24599,#24600,#24601,#24602,#24603,#24604,#24605,#24606),
 .UNSPECIFIED.,.F.,.F.,(4,2,2,2,2,2,2,2,2,2,2,2,2,2,2,2,2,2,2,2,2,2,2,2,
2,2,2,2,2,2,2,2,2,2,2,2,2,2,2,2,2,2,2,2,2,2,2,2,2,2,2,2,2,2,2,2,2,2,2,2,
2,2,2,2,2,2,2,2,2,2,2,2,2,2,2,2,2,2,2,2,2,2,2,2,4),(-2.43107777278142,-2.4216364324254,
-2.41932244202859,-2.41770638159793,-2.41630998116545,-2.41479108515786,
-2.41294963960475,-2.40825520827373,-2.39630263645416,-2.36157565826851,
-2.32934693264584,-2.32379892703653,-2.32069466021498,-2.31830074764382,
-2.31517746502707,-2.30969365184746,-2.28238376064854,-2.23386733437854,
-2.22910969561732,-2.22652207082348,-2.22429890510821,-2.22277261991302,
-2.22136752681913,-2.21942880521082,-2.21448858493093,-2.18328521629785,
-2.15118763940105,-2.13449740174692,-2.12980367821092,-2.12688453840775,
-2.12419331191462,-2.12071424852467,-2.11309053295057,-2.07304840388646,
-2.05038849796661,-2.0400160823175,-2.03346018588833,-2.03112937133336,
-2.02956609366946,-2.02816588101134,-2.02624651462117,-2.02142215583497,
-1.9859760447991,-1.94399983033855,-1.93776351499308,-1.93451516597527,
-1.93185378161207,-1.92875889438622,-1.92340161419112,-1.89913200765131,
-1.8608297152583,-1.84194398007218,-1.83870393329097,-1.83694211661892,
-1.83544413256886,-1.83351745958127,-1.83038358874895,-1.80760884713865,
-1.77428789038115,-1.74910774785104,-1.74383285866949,-1.74078712610847,
-1.73812154444079,-1.73480813158663,-1.72966942538366,-1.6956762828095,
-1.65316954903024,-1.64686762612116,-1.64457168082692,-1.64301551906721,
-1.64160889423659,-1.63966444876635,-1.63469108009369,-1.60523632508808,
-1.57299071051188,-1.56105717805104,-1.55249767501423,-1.54881615395698,
-1.54610247230968,-1.5435818490515,-1.54012025179612,-1.53123501631135,
-1.48392839280664,-1.46447905982084,-1.45793772452377),.UNSPECIFIED.);
#1179=B_SPLINE_CURVE_WITH_KNOTS('',3,(#24611,#24612,#24613,#24614,#24615,
#24616,#24617,#24618,#24619,#24620,#24621,#24622,#24623,#24624,#24625,#24626,
#24627,#24628,#24629,#24630,#24631,#24632,#24633,#24634,#24635,#24636,#24637,
#24638,#24639,#24640,#24641,#24642,#24643,#24644,#24645,#24646,#24647,#24648,
#24649,#24650,#24651,#24652,#24653,#24654,#24655,#24656,#24657,#24658,#24659,
#24660,#24661,#24662,#24663,#24664,#24665,#24666,#24667,#24668,#24669,#24670,
#24671,#24672,#24673,#24674,#24675,#24676,#24677,#24678,#24679,#24680,#24681,
#24682,#24683,#24684,#24685,#24686,#24687,#24688,#24689,#24690,#24691,#24692,
#24693,#24694,#24695,#24696,#24697,#24698,#24699,#24700,#24701,#24702,#24703,
#24704,#24705,#24706,#24707,#24708,#24709,#24710,#24711,#24712,#24713,#24714,
#24715,#24716,#24717,#24718,#24719,#24720,#24721,#24722,#24723,#24724,#24725,
#24726,#24727,#24728,#24729,#24730,#24731,#24732,#24733,#24734,#24735,#24736,
#24737,#24738,#24739,#24740,#24741,#24742,#24743,#24744,#24745,#24746,#24747,
#24748,#24749,#24750,#24751,#24752,#24753,#24754,#24755,#24756,#24757,#24758,
#24759,#24760,#24761,#24762,#24763,#24764,#24765,#24766,#24767,#24768,#24769,
#24770,#24771,#24772,#24773,#24774,#24775,#24776,#24777,#24778,#24779,#24780,
#24781,#24782,#24783,#24784,#24785,#24786,#24787,#24788,#24789,#24790,#24791,
#24792,#24793,#24794,#24795,#24796,#24797,#24798,#24799,#24800,#24801,#24802,
#24803,#24804,#24805,#24806,#24807,#24808,#24809,#24810,#24811,#24812,#24813,
#24814,#24815,#24816,#24817,#24818,#24819,#24820,#24821,#24822,#24823,#24824),
 .UNSPECIFIED.,.F.,.F.,(4,2,2,2,2,2,2,2,2,2,2,2,2,2,2,2,2,2,2,2,2,2,2,2,
2,2,2,2,2,2,2,2,2,2,2,2,2,2,2,2,2,2,2,2,2,2,2,2,2,2,2,2,2,2,2,2,2,2,2,2,
2,2,2,2,2,2,2,2,2,2,2,2,2,2,2,2,2,2,2,2,2,2,2,2,2,2,2,2,2,2,2,2,2,2,2,2,
2,2,2,2,2,2,2,2,2,2,4),(-2.18919381409884,-2.18542769624879,-2.1777550237912,
-2.17422858908373,-2.17153847469439,-2.16861237384775,-2.16388928441978,
-2.14857128267781,-2.10261070908038,-2.08809248688705,-2.08252165729276,
-2.07840294323425,-2.07646327995554,-2.07497731303468,-2.0732291679483,
-2.07014005085251,-2.05637759821995,-2.00342625063843,-1.98705445192856,
-1.98238917352435,-1.97947574326804,-1.976781691186,-1.97328752886651,-1.96586912773494,
-1.92308683471171,-1.89858077769942,-1.89089199082272,-1.88562898840809,
-1.88348891756278,-1.88196214043551,-1.88051843314864,-1.87800479452204,
-1.8706858724857,-1.82469417385007,-1.79784198361439,-1.79083888670194,
-1.78743792333612,-1.78476366425887,-1.78177299964344,-1.77675342853374,
-1.75845083450918,-1.71544045981571,-1.70134356018655,-1.69321996452482,
-1.690696145298,-1.68909095117362,-1.6875577429757,-1.68566187193951,-1.68097691931811,
-1.64285247617887,-1.6203412173297,-1.60103565878672,-1.59612451272635,
-1.5931573941776,-1.59047814195304,-1.58703463879686,-1.57980908547012,
-1.53320777337025,-1.51124999396228,-1.50403509618806,-1.49901756117681,
-1.49691771975033,-1.49539761352437,-1.49373219991273,-1.49093611821525,
-1.48120699232189,-1.43867198146836,-1.41141562442926,-1.40436056946333,
-1.40094950720844,-1.39827400401815,-1.39528888692692,-1.39029528082016,
-1.37249159492932,-1.32356413018792,-1.31296712999778,-1.30630927328946,
-1.30396422927291,-1.30239758477807,-1.30099910392051,-1.2990880372357,
-1.29431500741867,-1.25773782524663,-1.21592120741526,-1.21077910597509,
-1.20746409577167,-1.2047976176147,-1.2017512723742,-1.19647635650801,-1.1713220702832,
-1.13810540300183,-1.1151603057416,-1.11202252287472,-1.11009437201323,
-1.10859582331981,-1.10683397245524,-1.10359544058248,-1.08476539751549,
-1.04659329765605,-1.02217500090176,-1.01681715453497,-1.01372148048733,
-1.01105913531796,-1.00780924510266,-1.00156877734155,-0.977939243506538,
-0.973882930196809),.UNSPECIFIED.);
#1180=B_SPLINE_CURVE_WITH_KNOTS('',3,(#24825,#24826,#24827,#24828,#24829,
#24830,#24831,#24832,#24833,#24834,#24835,#24836,#24837,#24838,#24839,#24840,
#24841,#24842,#24843,#24844,#24845,#24846,#24847,#24848,#24849,#24850,#24851,
#24852,#24853,#24854,#24855,#24856,#24857,#24858,#24859,#24860,#24861,#24862,
#24863,#24864,#24865,#24866,#24867,#24868,#24869,#24870,#24871,#24872,#24873,
#24874,#24875,#24876,#24877,#24878,#24879,#24880,#24881,#24882,#24883,#24884,
#24885,#24886,#24887,#24888,#24889,#24890,#24891,#24892,#24893,#24894,#24895,
#24896,#24897,#24898,#24899,#24900,#24901,#24902,#24903,#24904,#24905,#24906,
#24907,#24908,#24909,#24910,#24911,#24912,#24913,#24914,#24915,#24916,#24917,
#24918,#24919,#24920,#24921,#24922,#24923,#24924,#24925,#24926,#24927,#24928,
#24929,#24930,#24931,#24932,#24933,#24934,#24935,#24936,#24937,#24938,#24939,
#24940,#24941,#24942,#24943,#24944,#24945,#24946,#24947,#24948,#24949,#24950,
#24951,#24952,#24953,#24954,#24955,#24956,#24957,#24958,#24959,#24960,#24961,
#24962,#24963,#24964,#24965,#24966,#24967,#24968,#24969,#24970,#24971,#24972,
#24973,#24974,#24975,#24976,#24977,#24978,#24979,#24980,#24981,#24982,#24983,
#24984,#24985,#24986,#24987,#24988,#24989,#24990,#24991,#24992,#24993,#24994,
#24995,#24996,#24997,#24998,#24999,#25000,#25001,#25002,#25003,#25004,#25005,
#25006,#25007,#25008,#25009,#25010,#25011,#25012,#25013,#25014,#25015,#25016,
#25017,#25018,#25019,#25020,#25021,#25022,#25023,#25024,#25025,#25026,#25027,
#25028,#25029,#25030,#25031,#25032,#25033,#25034,#25035,#25036,#25037,#25038,
#25039,#25040,#25041,#25042),.UNSPECIFIED.,.F.,.F.,(4,2,2,2,2,2,2,2,2,2,
2,2,2,2,2,2,2,2,2,2,2,2,2,2,2,2,2,2,2,2,2,2,2,2,2,2,2,2,2,2,2,2,2,2,2,2,
2,2,2,2,2,2,2,2,2,2,2,2,2,2,2,2,2,2,2,2,2,2,2,2,2,2,2,2,2,2,2,2,2,2,2,2,
2,2,2,2,2,2,2,2,2,2,2,2,2,2,2,2,2,2,2,2,2,2,2,2,2,2,4),(-1.45793772452377,
-1.45777260193418,-1.45302510647799,-1.45097148119764,-1.44945870609026,
-1.44777250859995,-1.44488130714998,-1.43410949080527,-1.42326776027908,
-1.38816492231145,-1.36261109191867,-1.35731728178986,-1.35426725838252,
-1.35160182549809,-1.34829367472127,-1.34317292084646,-1.31064906147403,
-1.26672852869036,-1.2603490701703,-1.25804216883641,-1.25648364598898,
-1.25507886058817,-1.25314201465082,-1.24821429570316,-1.21607450283724,
-1.17290643617366,-1.16541401843643,-1.16195846157678,-1.15927034153411,
-1.15633941416287,-1.15159290171079,-1.13431420204943,-1.10008974803179,
-1.08603721795572,-1.0689892503762,-1.06600454508107,-1.06412240731802,
-1.06262700769033,-1.0608297859991,-1.05742302373645,-1.03271633723126,
-1.03018026579809,-0.985573901999544,-0.974000860973215,-0.969739201323046,
-0.967195311141253,-0.964495470080255,-0.960900192787971,-0.952840943924294,
-0.941815908503195,-0.909944670525386,-0.878387172933484,-0.87344512441187,
-0.871505950686854,-0.8701006318668,-0.868542888226062,-0.866239485521736,
-0.85988450826816,-0.816409187166543,-0.783459588513825,-0.778335694898967,
-0.775026615041645,-0.77236116509105,-0.769311920914844,-0.764021535459174,
-0.738540521405353,-0.70389236572519,-0.693133871966376,-0.681793968046884,
-0.678853204095014,-0.677156130011352,-0.675646392456661,-0.673614280273694,
-0.668989536000823,-0.647968709999461,-0.637911410746544,-0.592909663164301,
-0.585541557029416,-0.582108903140882,-0.579424125852703,-0.576482132769866,
-0.571684385101919,-0.553801624567775,-0.52201272084882,-0.491855394997577,
-0.48690870579373,-0.484968752166898,-0.483563251706732,-0.482005767265275,
-0.47970352997016,-0.473356738445829,-0.430031118061,-0.396925879821879,
-0.391800519269523,-0.388491027004843,-0.385825590895464,-0.382776740491327,
-0.37748801206359,-0.352039160988258,-0.317564269844856,-0.306839703351112,
-0.295291557202058,-0.29233325901375,-0.290632359355875,-0.289123635477083,
-0.287098856002939,-0.282515369392134,-0.261879296234975,-0.242598015109206),
 .UNSPECIFIED.);
#1181=B_SPLINE_CURVE_WITH_KNOTS('',3,(#25048,#25049,#25050,#25051,#25052,
#25053,#25054,#25055,#25056,#25057,#25058,#25059,#25060,#25061,#25062,#25063,
#25064,#25065,#25066,#25067,#25068,#25069,#25070,#25071,#25072,#25073,#25074,
#25075,#25076,#25077,#25078,#25079,#25080,#25081,#25082,#25083,#25084,#25085,
#25086,#25087,#25088,#25089,#25090,#25091,#25092,#25093,#25094,#25095,#25096,
#25097,#25098,#25099,#25100,#25101,#25102,#25103,#25104,#25105,#25106,#25107,
#25108,#25109,#25110,#25111,#25112,#25113,#25114,#25115,#25116,#25117,#25118,
#25119,#25120,#25121,#25122,#25123,#25124,#25125,#25126,#25127,#25128,#25129,
#25130,#25131,#25132,#25133,#25134,#25135,#25136,#25137,#25138,#25139,#25140,
#25141,#25142,#25143,#25144,#25145,#25146,#25147,#25148,#25149,#25150,#25151,
#25152,#25153,#25154,#25155,#25156,#25157,#25158,#25159,#25160,#25161,#25162,
#25163,#25164,#25165,#25166,#25167,#25168,#25169,#25170,#25171,#25172,#25173,
#25174,#25175,#25176,#25177,#25178,#25179,#25180,#25181,#25182,#25183,#25184,
#25185,#25186,#25187,#25188,#25189,#25190,#25191,#25192,#25193,#25194,#25195,
#25196,#25197,#25198,#25199,#25200,#25201,#25202,#25203,#25204,#25205,#25206,
#25207,#25208,#25209,#25210,#25211,#25212,#25213,#25214,#25215,#25216,#25217,
#25218,#25219,#25220,#25221,#25222,#25223),.UNSPECIFIED.,.F.,.F.,(4,2,2,
2,2,2,2,2,2,2,2,2,2,2,2,2,2,2,2,2,2,2,2,2,2,2,2,2,2,2,2,2,2,2,2,2,2,2,2,
2,2,2,2,2,2,2,2,2,2,2,2,2,2,2,2,2,2,2,2,2,2,2,2,2,2,2,2,2,2,2,2,2,2,2,2,
2,2,2,2,2,2,2,2,2,2,2,2,4),(-0.973675603579949,-0.971516545702564,-0.930207628100764,
-0.910055662766931,-0.904894525557746,-0.901872638858196,-0.899469778060034,
-0.896244545073618,-0.890125455208344,-0.882393248108257,-0.864518822685786,
-0.822516491085122,-0.809555093950112,-0.806519786723747,-0.80478373302264,
-0.803432056024337,-0.801548231090491,-0.797718261896276,-0.766595679976655,
-0.720227631034037,-0.712980580123312,-0.709532686935743,-0.70685253418381,
-0.703886974766604,-0.698984401662838,-0.679800807313866,-0.639366388857412,
-0.616934035005804,-0.613804741691513,-0.611878969585161,-0.610380414445586,
-0.608616378284783,-0.605368329087662,-0.58629352483316,-0.547613866466647,
-0.523885721762268,-0.518563001989904,-0.515475006691077,-0.512811776446246,
-0.509551367970992,-0.50326068605035,-0.495251781037841,-0.476400612464549,
-0.453745058672016,-0.443404562924578,-0.423606817613433,-0.420522643710844,
-0.418610360662707,-0.417112853054904,-0.415338884977469,-0.412043920266098,
-0.391611772752849,-0.350030570565927,-0.330191463439554,-0.325051095962264,
-0.322033793843072,-0.31963044514499,-0.316399220770562,-0.310250665249883,
-0.302471048839356,-0.284430818090247,-0.261065134729581,-0.232835747709177,
-0.227898432150552,-0.225959748821636,-0.224554301354016,-0.222995809771584,
-0.22077740087351,-0.214805222085212,-0.205623932127911,-0.171239789863074,
-0.137946773011612,-0.13281829323107,-0.129507294688439,-0.126840960263971,
-0.123791414958773,-0.118502302402707,-0.093068436308353,-0.075759600010088,
-0.0561909817124832,-0.0370787145087763,-0.0340184316652335,-0.032113354409625,
-0.0306164029671963,-0.0291941361075527,-0.0274304870625983,-0.0247525085311,
-0.00057331623553469),.UNSPECIFIED.);
#1182=B_SPLINE_CURVE_WITH_KNOTS('',3,(#25224,#25225,#25226,#25227,#25228,
#25229,#25230,#25231,#25232,#25233,#25234,#25235,#25236,#25237,#25238,#25239,
#25240,#25241,#25242,#25243,#25244,#25245,#25246,#25247,#25248,#25249,#25250,
#25251,#25252,#25253,#25254,#25255,#25256,#25257,#25258,#25259,#25260,#25261,
#25262,#25263),.UNSPECIFIED.,.F.,.F.,(4,2,2,2,2,2,2,2,2,2,2,2,2,2,2,2,2,
2,2,4),(-2.43135763693152,-2.39010762561609,-2.3736094853284,-2.3689324498023,
-2.36601639977979,-2.36332310713148,-2.35983442650161,-2.35216055904289,
-2.31704743805613,-2.28764413026702,-2.27844799834302,-2.27249722781729,
-2.2702960836424,-2.26872965301005,-2.26733120275681,-2.26541997702744,
-2.26064552361995,-2.2241812751241,-2.19576577617892,-2.18919381409884),
 .UNSPECIFIED.);
#1183=B_SPLINE_CURVE_WITH_KNOTS('',3,(#25265,#25266,#25267,#25268,#25269,
#25270,#25271,#25272,#25273,#25274,#25275,#25276,#25277,#25278,#25279,#25280,
#25281,#25282,#25283,#25284,#25285,#25286,#25287,#25288,#25289,#25290,#25291,
#25292,#25293,#25294,#25295,#25296,#25297,#25298,#25299,#25300,#25301,#25302,
#25303,#25304,#25305,#25306,#25307,#25308),.UNSPECIFIED.,.F.,.F.,(4,2,2,
2,2,2,2,2,2,2,2,2,2,2,2,2,2,2,2,2,2,4),(-0.242598015109206,-0.227163281818878,
-0.203228039698266,-0.197905029555936,-0.194857094765726,-0.192436765906469,
-0.189919151777873,-0.18506649448357,-0.166510004901814,-0.12697888806249,
-0.102972664901064,-0.0998183661447284,-0.0978855205166566,-0.0963868748126413,
-0.0946291020277296,-0.0914086123451188,-0.0730339436113313,-0.0468214669586457,
-0.0105994822371148,-0.0049216022030536,-0.00224184904898379,-0.000573763776605669),
 .UNSPECIFIED.);
#1184=B_SPLINE_CURVE_WITH_KNOTS('',3,(#25309,#25310,#25311,#25312,#25313,
#25314,#25315,#25316,#25317,#25318,#25319,#25320,#25321,#25322,#25323,#25324,
#25325,#25326,#25327,#25328,#25329,#25330,#25331,#25332,#25333,#25334,#25335,
#25336,#25337,#25338,#25339,#25340,#25341,#25342,#25343,#25344,#25345,#25346,
#25347,#25348,#25349,#25350,#25351,#25352,#25353,#25354,#25355,#25356,#25357,
#25358,#25359,#25360,#25361,#25362,#25363,#25364,#25365,#25366,#25367,#25368,
#25369,#25370,#25371,#25372,#25373,#25374,#25375,#25376,#25377,#25378,#25379,
#25380,#25381,#25382,#25383,#25384,#25385,#25386,#25387,#25388,#25389,#25390,
#25391,#25392,#25393,#25394,#25395,#25396,#25397,#25398,#25399,#25400,#25401,
#25402,#25403,#25404,#25405,#25406,#25407,#25408,#25409,#25410,#25411,#25412,
#25413,#25414,#25415,#25416,#25417,#25418,#25419,#25420,#25421,#25422,#25423,
#25424,#25425,#25426,#25427,#25428,#25429,#25430,#25431,#25432,#25433,#25434,
#25435,#25436,#25437,#25438,#25439,#25440,#25441,#25442,#25443,#25444,#25445,
#25446,#25447,#25448,#25449,#25450,#25451,#25452,#25453,#25454,#25455,#25456,
#25457,#25458,#25459,#25460,#25461,#25462,#25463,#25464,#25465,#25466,#25467,
#25468,#25469,#25470,#25471,#25472,#25473,#25474,#25475,#25476,#25477,#25478,
#25479,#25480),.UNSPECIFIED.,.F.,.F.,(4,2,2,2,2,2,2,2,2,2,2,2,2,2,2,2,2,
2,2,2,2,2,2,2,2,2,2,2,2,2,2,2,2,2,2,2,2,2,2,2,2,2,2,2,2,2,2,2,2,2,2,2,2,
2,2,2,2,2,2,2,2,2,2,2,2,2,2,2,2,2,2,2,2,2,2,2,2,2,2,2,2,2,2,2,2,4),(-2.43064787994583,
-2.4289190210585,-2.42590811732101,-2.42030236014,-2.38685906955935,-2.34389011788488,
-2.33756419720643,-2.33526545999383,-2.33370916013169,-2.33230379034719,
-2.33036283993118,-2.32540758614958,-2.29569892686985,-2.26251447774013,
-2.24552119086148,-2.24080133843114,-2.23829282289489,-2.23584217532018,
-2.23273719918661,-2.22715894983949,-2.19068040242632,-2.16422719106788,
-2.14615275733102,-2.14294522181671,-2.14119069149659,-2.13969239880238,
-2.13775690350697,-2.13459222877797,-2.10959332943499,-2.10307293607284,
-2.07848455943645,-2.05340159386969,-2.04813276729518,-2.04508890314991,
-2.04242399270497,-2.03911015689396,-2.03396836240495,-1.9988459325157,
-1.96627775410301,-1.95711350629871,-1.95112099402074,-1.94886973898967,
-1.94732291346048,-1.94590794469718,-1.9439301998852,-1.93984041333757,
-1.89855366435952,-1.86609895593524,-1.85705972856345,-1.85329963442785,
-1.85057314229474,-1.84807189670572,-1.8446850018454,-1.83624862938741,
-1.78259217885247,-1.76191112988104,-1.75732366100261,-1.75529851846876,
-1.75379011226426,-1.7520902015077,-1.74913505322763,-1.73761679237468,
-1.72690675488464,-1.69243946737807,-1.66700178032922,-1.66171495221982,
-1.65866704501352,-1.65600233945449,-1.65269363251008,-1.64756920491083,
-1.61448414016948,-1.57112173838723,-1.56477359990295,-1.56247150322932,
-1.56091431370218,-1.55950922833424,-1.55757005656073,-1.55262638160502,
-1.52231856401055,-1.4906834685268,-1.47887261063741,-1.47038015652668,
-1.46671046107402,-1.46399919321191,-1.46113238353101,-1.45771014066774),
 .UNSPECIFIED.);
#1185=B_SPLINE_CURVE_WITH_KNOTS('',3,(#25485,#25486,#25487,#25488,#25489,
#25490,#25491,#25492,#25493,#25494,#25495,#25496,#25497,#25498,#25499,#25500,
#25501,#25502,#25503,#25504,#25505,#25506,#25507,#25508,#25509,#25510,#25511,
#25512,#25513,#25514,#25515,#25516,#25517,#25518,#25519,#25520,#25521,#25522,
#25523,#25524,#25525,#25526,#25527,#25528,#25529,#25530,#25531,#25532,#25533,
#25534,#25535,#25536,#25537,#25538,#25539,#25540,#25541,#25542,#25543,#25544,
#25545,#25546,#25547,#25548,#25549,#25550,#25551,#25552,#25553,#25554,#25555,
#25556,#25557,#25558,#25559,#25560,#25561,#25562,#25563,#25564,#25565,#25566,
#25567,#25568,#25569,#25570,#25571,#25572,#25573,#25574,#25575,#25576,#25577,
#25578,#25579,#25580,#25581,#25582,#25583,#25584,#25585,#25586,#25587,#25588,
#25589,#25590,#25591,#25592,#25593,#25594,#25595,#25596,#25597,#25598,#25599,
#25600,#25601,#25602,#25603,#25604,#25605,#25606,#25607,#25608,#25609,#25610,
#25611,#25612,#25613,#25614,#25615,#25616,#25617,#25618,#25619,#25620,#25621,
#25622,#25623,#25624,#25625,#25626,#25627,#25628,#25629,#25630,#25631,#25632,
#25633,#25634,#25635,#25636,#25637,#25638,#25639,#25640,#25641,#25642,#25643,
#25644,#25645,#25646,#25647,#25648,#25649,#25650,#25651,#25652,#25653,#25654,
#25655,#25656,#25657,#25658,#25659,#25660,#25661,#25662,#25663,#25664,#25665,
#25666,#25667,#25668,#25669,#25670,#25671,#25672,#25673,#25674,#25675,#25676,
#25677,#25678,#25679,#25680,#25681,#25682,#25683,#25684,#25685,#25686,#25687,
#25688,#25689,#25690,#25691,#25692,#25693,#25694,#25695,#25696,#25697,#25698,
#25699,#25700,#25701,#25702,#25703,#25704,#25705,#25706),.UNSPECIFIED.,
 .F.,.F.,(4,2,2,2,2,2,2,2,2,2,2,2,2,2,2,2,2,2,2,2,2,2,2,2,2,2,2,2,2,2,2,
2,2,2,2,2,2,2,2,2,2,2,2,2,2,2,2,2,2,2,2,2,2,2,2,2,2,2,2,2,2,2,2,2,2,2,2,
2,2,2,2,2,2,2,2,2,2,2,2,2,2,2,2,2,2,2,2,2,2,2,2,2,2,2,2,2,2,2,2,2,2,2,2,
2,2,2,2,2,2,2,4),(-2.18893440373178,-2.18602305786878,-2.16487091400591,
-2.16023231457417,-2.15819763181326,-2.1566874213041,-2.15499135353963,
-2.15205568663814,-2.14077685919479,-2.13002647373089,-2.09535795113231,
-2.06988112048211,-2.064590891489,-2.06154147031496,-2.05887569195832,-2.05556596644588,
-2.05044053335471,-2.01740304575757,-1.97398955760533,-1.96763755204927,
-1.9653343451133,-1.9637764821387,-1.96237082841933,-1.96043089521855,-1.95548537618928,
-1.92535396810428,-1.89358592516691,-1.88174720020594,-1.87323888998993,
-1.86956560541463,-1.86685287536765,-1.86432949074828,-1.86085835727804,
-1.85191396969911,-1.79887899223932,-1.77827687901786,-1.7736967184568,
-1.77167218648568,-1.7701631495298,-1.76846127573765,-1.76549991484857,
-1.75392099002902,-1.74321722797438,-1.70879026024711,-1.68335451852561,
-1.67806565603243,-1.67501622121556,-1.67234995917235,-1.66903901954368,
-1.66391052276692,-1.6306526074751,-1.5874370888434,-1.58109519990408,-1.57879317217166,
-1.57723537522772,-1.57582920619691,-1.57388782924634,-1.5689349279576,
-1.53808269105599,-1.5057295628002,-1.48896453399656,-1.48426273646838,
-1.4813410096129,-1.47864901713721,-1.47517122472504,-1.46755958068519,
-1.42707670052492,-1.40471700609384,-1.39441375747966,-1.38788865915149,
-1.38556140289252,-1.38399839314225,-1.38259675313312,-1.38067329990869,
-1.37582753832456,-1.3409293869156,-1.31144764697642,-1.30088876153053,
-1.29309029771994,-1.28954076003256,-1.28684701406824,-1.28393055504674,
-1.27925305117643,-1.26435976829608,-1.25438270843973,-1.21556411502999,
-1.20696664149327,-1.19582403134391,-1.1928994913769,-1.19120559517347,
-1.18969427530323,-1.18765399453005,-1.18298537480698,-1.16155642862552,
-1.14618853845349,-1.10741217210891,-1.0997575243565,-1.09627189659431,
-1.09357863695319,-1.09066031336706,-1.08597455117074,-1.06938876259283,
-1.03766007233324,-1.02329890733008,-1.00343974320704,-1.00035324565996,
-0.998440232838664,-0.99694262591694,-0.995169098041974,-0.991876390883277,
-0.973675603579949),.UNSPECIFIED.);
#1186=B_SPLINE_CURVE_WITH_KNOTS('',3,(#25707,#25708,#25709,#25710,#25711,
#25712,#25713,#25714,#25715,#25716,#25717,#25718,#25719,#25720,#25721,#25722,
#25723,#25724,#25725,#25726,#25727,#25728,#25729,#25730,#25731,#25732,#25733,
#25734,#25735,#25736,#25737,#25738,#25739,#25740,#25741,#25742,#25743,#25744,
#25745,#25746,#25747,#25748,#25749,#25750,#25751,#25752,#25753,#25754,#25755,
#25756,#25757,#25758,#25759,#25760,#25761,#25762,#25763,#25764,#25765,#25766,
#25767,#25768,#25769,#25770,#25771,#25772,#25773,#25774,#25775,#25776,#25777,
#25778,#25779,#25780,#25781,#25782,#25783,#25784,#25785,#25786,#25787,#25788,
#25789,#25790,#25791,#25792,#25793,#25794,#25795,#25796,#25797,#25798,#25799,
#25800,#25801,#25802,#25803,#25804,#25805,#25806,#25807,#25808,#25809,#25810,
#25811,#25812,#25813,#25814,#25815,#25816,#25817,#25818,#25819,#25820,#25821,
#25822,#25823,#25824,#25825,#25826,#25827,#25828,#25829,#25830,#25831,#25832,
#25833,#25834,#25835,#25836,#25837,#25838,#25839,#25840,#25841,#25842,#25843,
#25844,#25845,#25846,#25847,#25848,#25849,#25850,#25851,#25852,#25853,#25854,
#25855,#25856,#25857,#25858,#25859,#25860,#25861,#25862,#25863,#25864,#25865,
#25866,#25867,#25868,#25869,#25870,#25871,#25872,#25873,#25874,#25875,#25876,
#25877,#25878,#25879,#25880,#25881,#25882,#25883,#25884,#25885,#25886,#25887,
#25888,#25889,#25890,#25891,#25892,#25893,#25894,#25895,#25896,#25897,#25898,
#25899,#25900,#25901,#25902,#25903,#25904,#25905,#25906,#25907,#25908),
 .UNSPECIFIED.,.F.,.F.,(4,2,2,2,2,2,2,2,2,2,2,2,2,2,2,2,2,2,2,2,2,2,2,2,
2,2,2,2,2,2,2,2,2,2,2,2,2,2,2,2,2,2,2,2,2,2,2,2,2,2,2,2,2,2,2,2,2,2,2,2,
2,2,2,2,2,2,2,2,2,2,2,2,2,2,2,2,2,2,2,2,2,2,2,2,2,2,2,2,2,2,2,2,2,2,2,2,
2,2,2,2,4),(-1.45771014066774,-1.45667896209667,-1.4436589147369,-1.3949449356228,
-1.38036652437068,-1.37478123034979,-1.37065459855406,-1.36871390249068,
-1.36721483707466,-1.36546317299772,-1.36235665252896,-1.34826800834459,
-1.29563748950007,-1.27930531203896,-1.2746449174408,-1.27173332242007,
-1.26904015774483,-1.26554601325508,-1.25812343967897,-1.21546100192093,
-1.18283601992191,-1.17791177013262,-1.17597580612725,-1.1745715048641,
-1.17301331536511,-1.17070657569251,-1.16432529795637,-1.12034299655681,
-1.08794315292719,-1.08282539651323,-1.07951856671759,-1.07685381988491,
-1.07380416748319,-1.06850994601822,-1.04293230290773,-1.00767946574459,
-0.987191059266374,-0.984081164631363,-0.982161751905746,-0.980664489394589,
-0.978897711057709,-0.975633811286164,-0.956080509205561,-0.916934485389681,
-0.894111378017313,-0.888840883348332,-0.885765842745586,-0.883103411165743,
-0.879830815892662,-0.873474297335921,-0.830878874654645,-0.796266644605056,
-0.791407783296881,-0.789482695654562,-0.788081124010819,-0.786519723641954,
-0.784197549563012,-0.777704262364909,-0.767470357860424,-0.74538974999726,
-0.70455457474415,-0.696960129142908,-0.693486529616642,-0.690796286215908,
-0.687874974636894,-0.683170592283469,-0.666360274833386,-0.633837989435531,
-0.603209809923447,-0.598237640064125,-0.596293539579796,-0.594887128982579,
-0.593331145199573,-0.591035377371374,-0.584733268469614,-0.542208660200637,
-0.508282019138443,-0.503145329396524,-0.499832687773274,-0.497167405390114,
-0.49412166431872,-0.488845872908267,-0.463644235162826,-0.430252348335858,
-0.407534388992947,-0.404401451037019,-0.402475151664517,-0.400977316991683,
-0.399215493912936,-0.395975005937027,-0.377067344638283,-0.338707948943681,
-0.314576396216332,-0.309214885121022,-0.306119167061324,-0.303458019368198,
-0.300211151864504,-0.293981470332704,-0.286070135113773,-0.267562130815639,
-0.242523000470694),.UNSPECIFIED.);
#1187=B_SPLINE_CURVE_WITH_KNOTS('',3,(#25914,#25915,#25916,#25917,#25918,
#25919,#25920,#25921,#25922,#25923,#25924,#25925,#25926,#25927,#25928,#25929,
#25930,#25931,#25932,#25933,#25934,#25935,#25936,#25937,#25938,#25939,#25940,
#25941,#25942,#25943,#25944,#25945,#25946,#25947,#25948,#25949,#25950,#25951,
#25952,#25953,#25954,#25955,#25956,#25957,#25958,#25959,#25960,#25961,#25962,
#25963,#25964,#25965,#25966,#25967,#25968,#25969,#25970,#25971,#25972,#25973,
#25974,#25975,#25976,#25977,#25978,#25979,#25980,#25981,#25982,#25983,#25984,
#25985,#25986,#25987,#25988,#25989,#25990,#25991,#25992,#25993,#25994,#25995,
#25996,#25997,#25998,#25999,#26000,#26001,#26002,#26003,#26004,#26005,#26006,
#26007,#26008,#26009,#26010,#26011,#26012,#26013,#26014,#26015,#26016,#26017,
#26018,#26019,#26020,#26021,#26022,#26023,#26024,#26025,#26026,#26027,#26028,
#26029,#26030,#26031,#26032,#26033,#26034,#26035,#26036,#26037,#26038,#26039,
#26040,#26041,#26042,#26043,#26044,#26045,#26046,#26047,#26048,#26049,#26050,
#26051,#26052,#26053,#26054,#26055,#26056,#26057,#26058,#26059,#26060,#26061,
#26062,#26063,#26064,#26065,#26066,#26067,#26068,#26069,#26070,#26071,#26072,
#26073,#26074,#26075,#26076,#26077,#26078,#26079,#26080,#26081,#26082,#26083,
#26084,#26085,#26086,#26087),.UNSPECIFIED.,.F.,.F.,(4,2,2,2,2,2,2,2,2,2,
2,2,2,2,2,2,2,2,2,2,2,2,2,2,2,2,2,2,2,2,2,2,2,2,2,2,2,2,2,2,2,2,2,2,2,2,
2,2,2,2,2,2,2,2,2,2,2,2,2,2,2,2,2,2,2,2,2,2,2,2,2,2,2,2,2,2,2,2,2,2,2,2,
2,2,2,2,4),(-0.973953791624347,-0.967465283548968,-0.93257382470948,-0.894350184248222,
-0.889667267830394,-0.887771673941779,-0.886238480733053,-0.884633020449155,
-0.882108315310275,-0.873977447167938,-0.859864109875752,-0.816722088528658,
-0.798592648572637,-0.793583341054268,-0.790594766678859,-0.787919862796101,
-0.784514637423928,-0.777490251075113,-0.750471891894025,-0.706204541135851,
-0.697629614907016,-0.69495920454513,-0.693321547969722,-0.691789277177381,
-0.689618848966036,-0.684165984301634,-0.676104448185037,-0.649427519433313,
-0.609666667085141,-0.602035471931189,-0.598554287537814,-0.595861918601123,
-0.592942027209865,-0.58824815409868,-0.571569594685118,-0.539517057923146,
-0.508214878954685,-0.503267252809573,-0.501326820288319,-0.49992092930726,
-0.498362936215472,-0.496059777511753,-0.489709292117109,-0.446327241972436,
-0.413284282842176,-0.408158636613833,-0.40484854774077,-0.402182350935323,
-0.399132313220868,-0.393840672264474,-0.368353088603507,-0.333667606726196,
-0.32290141055539,-0.311610242154255,-0.308673126592816,-0.306976564446801,
-0.305466139022737,-0.303431506604102,-0.298794354924746,-0.277661467989196,
-0.267257679463108,-0.222792088207318,-0.215387494571896,-0.211947562297166,
-0.209338104763373,-0.209118628772211,-0.206205006617162,-0.203140246674459,
-0.19858310458366,-0.19029767399017,-0.170441064598559,-0.127939719980367,
-0.118095997031503,-0.11528904690412,-0.113621126960683,-0.112101720114293,
-0.110007019702433,-0.105020942601532,-0.0804123930246865,-0.0394781845988557,
-0.0248226972464058,-0.020173041506687,-0.0172627057060512,-0.0146929297418167,
-0.0120771358670828,-0.00710051591487547,-0.000573354566209522),
 .UNSPECIFIED.);
#1188=B_SPLINE_CURVE_WITH_KNOTS('',3,(#26088,#26089,#26090,#26091,#26092,
#26093,#26094,#26095,#26096,#26097,#26098,#26099,#26100,#26101,#26102,#26103,
#26104,#26105,#26106,#26107,#26108,#26109,#26110,#26111,#26112,#26113,#26114,
#26115,#26116,#26117,#26118,#26119,#26120,#26121,#26122,#26123,#26124,#26125,
#26126,#26127,#26128,#26129),.UNSPECIFIED.,.F.,.F.,(4,2,2,2,2,2,2,2,2,2,
2,2,2,2,2,2,2,2,2,2,4),(-2.43089244675199,-2.40677745000843,-2.35827798625117,
-2.35352462500566,-2.35146986841046,-2.34995680866057,-2.34827086484605,
-2.34538127194777,-2.33462896991367,-2.32694146459418,-2.28202576276737,
-2.26906222322403,-2.26284470438802,-2.25909990257145,-2.25575924492405,
-2.25317421810439,-2.25062377863152,-2.24632839655743,-2.23451447360949,
-2.19012167723457,-2.18893440373178),.UNSPECIFIED.);
#1189=B_SPLINE_CURVE_WITH_KNOTS('',3,(#26131,#26132,#26133,#26134,#26135,
#26136,#26137,#26138,#26139,#26140,#26141,#26142,#26143,#26144,#26145,#26146,
#26147,#26148,#26149,#26150,#26151,#26152,#26153,#26154,#26155,#26156,#26157,
#26158,#26159,#26160,#26161,#26162,#26163,#26164,#26165,#26166,#26167,#26168,
#26169,#26170,#26171,#26172,#26173,#26174,#26175,#26176,#26177,#26178,#26179,
#26180,#26181,#26182,#26183,#26184),.UNSPECIFIED.,.F.,.F.,(4,2,2,2,2,2,
2,2,2,2,2,2,2,2,2,2,2,2,2,2,2,2,2,2,2,2,4),(-0.242523000470694,-0.225437215451584,
-0.213483329943007,-0.21052208750719,-0.208803534643909,-0.207328355820071,
-0.205402718327066,-0.203242716653735,-0.199587124904956,-0.191779697504846,
-0.166594550645333,-0.124805976705311,-0.117249000866896,-0.113782134205105,
-0.111092826629847,-0.108168244987422,-0.103449063901853,-0.0864739067951593,
-0.0342141991625467,-0.0222927842798497,-0.0184345143076221,-0.0165127155936031,
-0.0151118482286253,-0.0137081037350018,-0.0121594087514008,-0.0100183340058566,
-0.000573215276035292),.UNSPECIFIED.);
#1190=B_SPLINE_CURVE_WITH_KNOTS('',3,(#26185,#26186,#26187,#26188,#26189,
#26190,#26191,#26192,#26193,#26194,#26195,#26196,#26197,#26198,#26199,#26200,
#26201,#26202,#26203,#26204,#26205,#26206,#26207,#26208,#26209,#26210,#26211,
#26212,#26213,#26214,#26215,#26216,#26217,#26218,#26219,#26220,#26221,#26222,
#26223,#26224,#26225,#26226,#26227,#26228,#26229,#26230,#26231,#26232,#26233,
#26234,#26235,#26236,#26237,#26238,#26239,#26240,#26241,#26242,#26243,#26244,
#26245,#26246,#26247,#26248,#26249,#26250,#26251,#26252,#26253,#26254,#26255,
#26256,#26257,#26258,#26259,#26260,#26261,#26262,#26263,#26264,#26265,#26266,
#26267,#26268,#26269,#26270,#26271,#26272,#26273,#26274,#26275,#26276,#26277,
#26278,#26279,#26280,#26281,#26282,#26283,#26284,#26285,#26286,#26287,#26288,
#26289,#26290,#26291,#26292,#26293,#26294,#26295,#26296,#26297,#26298,#26299,
#26300,#26301,#26302,#26303,#26304,#26305,#26306,#26307,#26308,#26309,#26310,
#26311,#26312,#26313,#26314,#26315,#26316,#26317,#26318,#26319,#26320,#26321,
#26322,#26323,#26324,#26325,#26326,#26327,#26328,#26329,#26330,#26331,#26332,
#26333,#26334,#26335,#26336,#26337,#26338,#26339,#26340,#26341,#26342,#26343,
#26344,#26345,#26346,#26347,#26348,#26349,#26350),.UNSPECIFIED.,.F.,.F.,
(4,2,2,2,2,2,2,2,2,2,2,2,2,2,2,2,2,2,2,2,2,2,2,2,2,2,2,2,2,2,2,2,2,2,2,
2,2,2,2,2,2,2,2,2,2,2,2,2,2,2,2,2,2,2,2,2,2,2,2,2,2,2,2,2,2,2,2,2,2,2,2,
2,2,2,2,2,2,2,2,2,2,2,4),(-2.43140146279566,-2.38370979736051,-2.35858650028034,
-2.35331485990005,-2.35027001609835,-2.34760462941594,-2.3442906989176,
-2.33914971997813,-2.30371362431687,-2.27108906035359,-2.26213777882005,
-2.25811879143242,-2.25581520230946,-2.2538368257165,-2.2523519783445,-2.25070353057344,
-2.24798224076958,-2.2389479479071,-2.20195248740586,-2.17119534139135,
-2.1621984943043,-2.15844482225991,-2.1557190505994,-2.15321574617055,-2.14982190611309,
-2.14134635258128,-2.08772673698565,-2.06704764588328,-2.06245990744073,
-2.06043447086318,-2.05892577366725,-2.05722545440735,-2.05426941865898,
-2.04274542382737,-2.03203374958153,-1.99756225872869,-1.97211992349234,
-1.96683204606896,-1.96378352461148,-1.96111827654726,-1.95780888885823,
-1.95268339319331,-1.91958902034189,-1.87622025808154,-1.86987096202069,
-1.86756841575638,-1.86601091336605,-1.86460553882285,-1.86266595920262,
-1.85772120050715,-1.82743146116468,-1.79464970466104,-1.77776521256565,
-1.77305379162657,-1.77013066613508,-1.76744045664711,-1.76396928754582,
-1.75639006957688,-1.71506016713977,-1.68950523112516,-1.68163302011892,
-1.67627664297594,-1.67412185138993,-1.67259272297262,-1.6709500866416,
-1.66825578780362,-1.65946702755077,-1.62221375103456,-1.58735157548973,
-1.58103957103891,-1.57777563667933,-1.57511323924908,-1.57203038677833,
-1.56672698860878,-1.54333370761027,-1.5044156167401,-1.48518439795463,
-1.48193133968392,-1.48016665390761,-1.47866882862526,-1.47674570447627,
-1.47362406522875,-1.45805210159456),.UNSPECIFIED.);
#1191=B_SPLINE_CURVE_WITH_KNOTS('',3,(#26355,#26356,#26357,#26358,#26359,
#26360,#26361,#26362,#26363,#26364,#26365,#26366,#26367,#26368,#26369,#26370,
#26371,#26372,#26373,#26374,#26375,#26376,#26377,#26378,#26379,#26380,#26381,
#26382,#26383,#26384,#26385,#26386,#26387,#26388,#26389,#26390,#26391,#26392,
#26393,#26394,#26395,#26396,#26397,#26398,#26399,#26400,#26401,#26402,#26403,
#26404,#26405,#26406,#26407,#26408,#26409,#26410,#26411,#26412,#26413,#26414,
#26415,#26416,#26417,#26418,#26419,#26420,#26421,#26422,#26423,#26424,#26425,
#26426,#26427,#26428,#26429,#26430,#26431,#26432,#26433,#26434,#26435,#26436,
#26437,#26438,#26439,#26440,#26441,#26442,#26443,#26444,#26445,#26446,#26447,
#26448,#26449,#26450,#26451,#26452,#26453,#26454,#26455,#26456,#26457,#26458,
#26459,#26460,#26461,#26462,#26463,#26464,#26465,#26466,#26467,#26468,#26469,
#26470,#26471,#26472,#26473,#26474,#26475,#26476,#26477,#26478,#26479,#26480,
#26481,#26482,#26483,#26484,#26485,#26486,#26487,#26488,#26489,#26490,#26491,
#26492,#26493,#26494,#26495,#26496,#26497,#26498,#26499,#26500,#26501,#26502,
#26503,#26504,#26505,#26506,#26507,#26508,#26509,#26510,#26511,#26512,#26513,
#26514,#26515,#26516,#26517,#26518,#26519,#26520,#26521,#26522,#26523,#26524,
#26525,#26526,#26527,#26528,#26529,#26530,#26531,#26532,#26533,#26534,#26535,
#26536,#26537,#26538,#26539,#26540,#26541,#26542,#26543,#26544,#26545,#26546,
#26547,#26548,#26549,#26550,#26551,#26552,#26553,#26554,#26555,#26556,#26557,
#26558,#26559,#26560,#26561,#26562,#26563,#26564,#26565,#26566,#26567,#26568,
#26569,#26570),.UNSPECIFIED.,.F.,.F.,(4,2,2,2,2,2,2,2,2,2,2,2,2,2,2,2,2,
2,2,2,2,2,2,2,2,2,2,2,2,2,2,2,2,2,2,2,2,2,2,2,2,2,2,2,2,2,2,2,2,2,2,2,2,
2,2,2,2,2,2,2,2,2,2,2,2,2,2,2,2,2,2,2,2,2,2,2,2,2,2,2,2,2,2,2,2,2,2,2,2,
2,2,2,2,2,2,2,2,2,2,2,2,2,2,2,2,2,2,4),(-2.18908437233165,-2.18018897530132,
-2.16147584202253,-2.1535059286629,-2.14723917490848,-2.14398413157484,
-2.14157877424435,-2.13857926260685,-2.13351900829028,-2.11468332877233,
-2.07646810778413,-2.05169001029865,-2.04828132401378,-2.04648358683509,
-2.04498802921325,-2.04310600217505,-2.04012204858244,-2.02309177048872,
-1.98461402729307,-1.95863660825575,-1.95332209409581,-1.95026735957319,
-1.94760202824388,-1.94429945837683,-1.93919779280146,-1.90236137329814,
-1.87607577873784,-1.85811309456896,-1.85490881003816,-1.85315437472235,
-1.8516550916492,-1.84971688455819,-1.8465449384384,-1.82061848294505,-1.79609686870761,
-1.76840600251381,-1.76129593804436,-1.75787438079302,-1.75519771874331,
-1.75221859884262,-1.74725240130115,-1.7297647183804,-1.68599126390407,
-1.67178639394292,-1.66362059419485,-1.66109199454717,-1.6594856939297,
-1.65795309219008,-1.6560597201182,-1.65138956113164,-1.61289579102747,
-1.57393927536086,-1.56758160551049,-1.56430792359671,-1.56164434582861,
-1.55856767741368,-1.55329360686779,-1.5304384447075,-1.49128283574657,
-1.4717223947889,-1.46845698503998,-1.46668940168618,-1.46519144171741,
-1.46327109001382,-1.46015959070346,-1.43965840171215,-1.40444384221564,
-1.3788735253873,-1.37357817129341,-1.37052738355103,-1.36786134426156,
-1.36455250817576,-1.35943079075152,-1.32201509685289,-1.29311230136627,
-1.28305869310448,-1.27664802728967,-1.27433658392991,-1.27277694721012,
-1.27137266659989,-1.26943840522657,-1.26452736074527,-1.23136005854359,
-1.21611666486218,-1.18625101294632,-1.18116878531827,-1.17787190342583,
-1.1752066923533,-1.17214717987868,-1.16681158537516,-1.1403977464359,-1.11656711192485,
-1.1025136908001,-1.08534256231142,-1.08235254472572,-1.08046861774952,
-1.07897285931959,-1.07717644124281,-1.07377450652148,-1.04931653877236,
-1.04148220225156,-0.995695977725987,-0.989120603118532,-0.985762090778382,
-0.983266831226487,-0.980532244715124,-0.976733915400356,-0.973953791624347),
 .UNSPECIFIED.);
#1192=B_SPLINE_CURVE_WITH_KNOTS('',3,(#26571,#26572,#26573,#26574,#26575,
#26576,#26577,#26578,#26579,#26580,#26581,#26582,#26583,#26584,#26585,#26586,
#26587,#26588,#26589,#26590,#26591,#26592,#26593,#26594,#26595,#26596,#26597,
#26598,#26599,#26600,#26601,#26602,#26603,#26604,#26605,#26606,#26607,#26608,
#26609,#26610,#26611,#26612,#26613,#26614,#26615,#26616,#26617,#26618,#26619,
#26620,#26621,#26622,#26623,#26624,#26625,#26626,#26627,#26628,#26629,#26630,
#26631,#26632,#26633,#26634,#26635,#26636,#26637,#26638,#26639,#26640,#26641,
#26642,#26643,#26644,#26645,#26646,#26647,#26648,#26649,#26650,#26651,#26652,
#26653,#26654,#26655,#26656,#26657,#26658,#26659,#26660,#26661,#26662,#26663,
#26664,#26665,#26666,#26667,#26668,#26669,#26670,#26671,#26672,#26673,#26674,
#26675,#26676,#26677,#26678,#26679,#26680,#26681,#26682,#26683,#26684,#26685,
#26686,#26687,#26688,#26689,#26690,#26691,#26692,#26693,#26694,#26695,#26696,
#26697,#26698,#26699,#26700,#26701,#26702,#26703,#26704,#26705,#26706,#26707,
#26708,#26709,#26710,#26711,#26712,#26713,#26714,#26715,#26716,#26717,#26718,
#26719,#26720,#26721,#26722,#26723,#26724,#26725,#26726,#26727,#26728,#26729,
#26730,#26731,#26732,#26733,#26734,#26735,#26736,#26737,#26738,#26739,#26740,
#26741,#26742,#26743,#26744,#26745,#26746,#26747,#26748,#26749,#26750,#26751,
#26752,#26753,#26754,#26755,#26756,#26757,#26758,#26759,#26760,#26761,#26762,
#26763,#26764,#26765,#26766,#26767,#26768,#26769,#26770,#26771,#26772,#26773,
#26774,#26775,#26776,#26777,#26778,#26779,#26780,#26781,#26782),
 .UNSPECIFIED.,.F.,.F.,(4,2,2,2,2,2,2,2,2,2,2,2,2,2,2,2,2,2,2,2,2,2,2,2,
2,2,2,2,2,2,2,2,2,2,2,2,2,2,2,2,2,2,2,2,2,2,2,2,2,2,2,2,2,2,2,2,2,2,2,2,
2,2,2,2,2,2,2,2,2,2,2,2,2,2,2,2,2,2,2,2,2,2,2,2,2,2,2,2,2,2,2,2,2,2,2,2,
2,2,2,2,2,2,2,2,2,4),(-1.45805210159456,-1.45155832824827,-1.41765818253014,
-1.39233078637762,-1.38704820423083,-1.38400064475323,-1.38133500580256,
-1.37802352940773,-1.37289170412753,-1.33930255891899,-1.29639934286917,
-1.2900751176326,-1.28777593157304,-1.28621901397535,-1.28481283948997,
-1.28287046280774,-1.27790994558091,-1.24824005346882,-1.21613472700597,
-1.19848888329236,-1.19350923827962,-1.19052739993062,-1.18785166355357,
-1.18443594985395,-1.17735535784278,-1.14989380355426,-1.13973334595397,
-1.10100471792365,-1.09634369476463,-1.09445204800143,-1.09292005251862,
-1.09131341960513,-1.08878266943041,-1.08059533491553,-1.06633662164289,
-1.02209861898637,-1.00505955494107,-1.00015690592514,-0.997191891165642,
-0.994512615658126,-0.991066404841612,-0.983825110958358,-0.95507452038955,
-0.923972351031826,-0.917250699546878,-0.904971523359243,-0.901985201712351,
-0.900260689400688,-0.8989077994464,-0.897009080966061,-0.893101552106182,
-0.887897196921466,-0.874803028849946,-0.835751626717067,-0.812637959816677,
-0.807349899771707,-0.804270337130832,-0.80160741738904,-0.798338576229525,
-0.792003391534514,-0.783921681803954,-0.764806748120944,-0.729639509155669,
-0.712247545169637,-0.709248964360094,-0.707362622897675,-0.705867002370958,
-0.704073250379847,-0.700683148148376,-0.676746967370331,-0.662588265387774,
-0.623102640789911,-0.615464304194692,-0.611982296638298,-0.609290300048909,
-0.606371828086698,-0.601682506472688,-0.585046985829955,-0.553142881480964,
-0.521627852765654,-0.516684149974468,-0.514744636695253,-0.513339186199238,
-0.511781433824716,-0.509478251580026,-0.503125366750244,-0.459692398241449,
-0.426694449356944,-0.421569845191526,-0.41826046255989,-0.415594869710006,
-0.412545572364426,-0.40725537892338,-0.38178235461823,-0.347183712815403,
-0.336434810682388,-0.325032544647356,-0.322086412055251,-0.320388107912964,
-0.318878592942747,-0.316848563458607,-0.312235938004416,-0.291329855913279,
-0.287488014356654,-0.244499584275477,-0.242711045913264),.UNSPECIFIED.);
#1193=B_SPLINE_CURVE_WITH_KNOTS('',3,(#26788,#26789,#26790,#26791,#26792,
#26793,#26794,#26795,#26796,#26797,#26798,#26799,#26800,#26801,#26802,#26803,
#26804,#26805,#26806,#26807,#26808,#26809,#26810,#26811,#26812,#26813,#26814,
#26815,#26816,#26817,#26818,#26819,#26820,#26821,#26822,#26823,#26824,#26825,
#26826,#26827,#26828,#26829,#26830,#26831,#26832,#26833,#26834,#26835,#26836,
#26837,#26838,#26839,#26840,#26841,#26842,#26843,#26844,#26845,#26846,#26847,
#26848,#26849,#26850,#26851,#26852,#26853,#26854,#26855,#26856,#26857,#26858,
#26859,#26860,#26861,#26862,#26863,#26864,#26865,#26866,#26867,#26868,#26869,
#26870,#26871,#26872,#26873,#26874,#26875,#26876,#26877,#26878,#26879,#26880,
#26881,#26882,#26883,#26884,#26885,#26886,#26887,#26888,#26889,#26890,#26891,
#26892,#26893,#26894,#26895,#26896,#26897,#26898,#26899,#26900,#26901,#26902,
#26903,#26904,#26905,#26906,#26907,#26908,#26909,#26910,#26911,#26912,#26913,
#26914,#26915,#26916,#26917,#26918,#26919,#26920,#26921,#26922,#26923,#26924,
#26925,#26926,#26927,#26928,#26929,#26930,#26931,#26932,#26933,#26934,#26935,
#26936,#26937,#26938,#26939,#26940,#26941,#26942,#26943,#26944,#26945,#26946,
#26947,#26948,#26949,#26950,#26951,#26952,#26953,#26954,#26955,#26956,#26957,
#26958,#26959,#26960,#26961,#26962,#26963,#26964,#26965),.UNSPECIFIED.,
 .F.,.F.,(4,2,2,2,2,2,2,2,2,2,2,2,2,2,2,2,2,2,2,2,2,2,2,2,2,2,2,2,2,2,2,
2,2,2,2,2,2,2,2,2,2,2,2,2,2,2,2,2,2,2,2,2,2,2,2,2,2,2,2,2,2,2,2,2,2,2,2,
2,2,2,2,2,2,2,2,2,2,2,2,2,2,2,2,2,2,2,2,2,4),(-0.973680670967328,-0.973307112572624,
-0.970220541363192,-0.968473310280311,-0.966987818653059,-0.965048391252937,
-0.960928624075663,-0.95535589718811,-0.940828043205159,-0.893006977768661,
-0.879263898633052,-0.874720999707776,-0.871834782675239,-0.869131868753156,
-0.865514359003847,-0.857325865642324,-0.846067488257675,-0.812917873193628,
-0.783111919959633,-0.778158141897692,-0.77621714532033,-0.774811531052763,
-0.773254517483143,-0.770954214231317,-0.76462061636457,-0.721522501514497,
-0.688210222796253,-0.683083250219667,-0.679773334948916,-0.677107942420935,
-0.674059548236232,-0.668772614842662,-0.643352814329744,-0.608991222007037,
-0.594277944636392,-0.586000149579008,-0.583365199668248,-0.5817357104235,
-0.580199965929129,-0.578008413965618,-0.572416758313034,-0.564076622368752,
-0.535656242335143,-0.498199762596961,-0.490532534490196,-0.487045628025484,
-0.484353187475155,-0.481437547404829,-0.476760049399391,-0.460248456596532,
-0.406066518825857,-0.393522706038287,-0.390517210355603,-0.388788323940043,
-0.387436142727619,-0.385543740037546,-0.381668302843481,-0.376518843685185,
-0.363631187904509,-0.324961652495334,-0.301243430819132,-0.295922541049584,
-0.292835567998951,-0.290173196477519,-0.286913810897248,-0.280625014431996,
-0.243988883928487,-0.202645276554972,-0.198234021075032,-0.196223672501802,
-0.194763546437064,-0.193364279321359,-0.191718970663122,-0.186607333298091,
-0.179212623817119,-0.156310733632371,-0.111229925958632,-0.103869968369257,
-0.100438647868069,-0.0977538578003124,-0.0948107634063591,-0.0900087154509661,
-0.0720766169546895,-0.0143120872675185,-0.0061825986812647,-0.00361975116399399,
-0.00201508611533718,-0.00101558929569232,-0.0005762572455496),
 .UNSPECIFIED.);
#1194=B_SPLINE_CURVE_WITH_KNOTS('',3,(#26966,#26967,#26968,#26969,#26970,
#26971,#26972,#26973,#26974,#26975,#26976,#26977,#26978,#26979,#26980,#26981,
#26982,#26983,#26984,#26985,#26986,#26987,#26988,#26989,#26990,#26991,#26992,
#26993,#26994,#26995,#26996,#26997,#26998,#26999,#27000,#27001,#27002,#27003,
#27004,#27005,#27006,#27007),.UNSPECIFIED.,.F.,.F.,(4,2,2,2,2,2,2,2,2,2,
2,2,2,2,2,2,2,2,2,2,4),(-2.43110192767283,-2.43046386845514,-2.4286601279836,
-2.42395621479106,-2.38392888016529,-2.34632532223177,-2.34029961040404,
-2.33709440964267,-2.3344595056279,-2.3313368283343,-2.32585712279234,-2.29865413240242,
-2.25008607935706,-2.24301003239931,-2.24061086161376,-2.23921421723126,
-2.23770922238876,-2.23560160568965,-2.23067339359046,-2.20291808918862,
-2.18908437233165),.UNSPECIFIED.);
#1195=B_SPLINE_CURVE_WITH_KNOTS('',3,(#27009,#27010,#27011,#27012,#27013,
#27014,#27015,#27016,#27017,#27018,#27019,#27020,#27021,#27022,#27023,#27024,
#27025,#27026,#27027,#27028,#27029,#27030,#27031,#27032,#27033,#27034,#27035,
#27036,#27037,#27038,#27039,#27040,#27041,#27042,#27043,#27044,#27045,#27046,
#27047,#27048,#27049,#27050,#27051,#27052,#27053,#27054,#27055,#27056,#27057,
#27058,#27059,#27060,#27061,#27062,#27063,#27064),.UNSPECIFIED.,.F.,.F.,
(4,2,2,2,2,2,2,2,2,2,2,2,2,2,2,2,2,2,2,2,2,2,2,2,2,2,2,4),(-0.242711045913264,
-0.231176709974483,-0.226684594073206,-0.22380892673107,-0.221154531929772,
-0.217633423655963,-0.213704703696832,-0.207029271880388,-0.192651858150418,
-0.164304706903861,-0.157250992792754,-0.132746176728411,-0.12958524641712,
-0.127650438261172,-0.126151631030437,-0.124395257839107,-0.121181296267978,
-0.102970487894109,-0.0656064654841873,-0.047230945741886,-0.0370128089892073,
-0.0329512545508428,-0.0304445845184497,-0.0279065401753038,-0.0252520144840107,
-0.0217418394651842,-0.0138411091822967,-0.000573273520096065),
 .UNSPECIFIED.);
#1196=B_SPLINE_CURVE_WITH_KNOTS('',3,(#27065,#27066,#27067,#27068,#27069,
#27070,#27071,#27072,#27073,#27074,#27075,#27076,#27077,#27078,#27079,#27080,
#27081,#27082,#27083,#27084,#27085,#27086,#27087,#27088,#27089,#27090,#27091,
#27092,#27093,#27094,#27095,#27096,#27097,#27098,#27099,#27100,#27101,#27102,
#27103,#27104,#27105,#27106,#27107,#27108,#27109,#27110,#27111,#27112,#27113,
#27114,#27115,#27116,#27117,#27118,#27119,#27120,#27121,#27122,#27123,#27124,
#27125,#27126,#27127,#27128,#27129,#27130,#27131,#27132,#27133,#27134,#27135,
#27136,#27137,#27138,#27139,#27140,#27141,#27142,#27143,#27144,#27145,#27146,
#27147,#27148,#27149,#27150,#27151,#27152,#27153,#27154,#27155,#27156,#27157,
#27158,#27159,#27160,#27161,#27162,#27163,#27164,#27165,#27166,#27167,#27168,
#27169,#27170,#27171,#27172,#27173,#27174,#27175,#27176,#27177,#27178,#27179,
#27180,#27181,#27182,#27183,#27184,#27185,#27186,#27187,#27188,#27189,#27190,
#27191,#27192,#27193,#27194,#27195,#27196,#27197,#27198,#27199,#27200,#27201,
#27202,#27203,#27204,#27205,#27206,#27207,#27208,#27209,#27210,#27211,#27212,
#27213,#27214,#27215,#27216,#27217,#27218,#27219,#27220,#27221,#27222,#27223,
#27224,#27225,#27226,#27227,#27228,#27229,#27230,#27231,#27232,#27233,#27234,
#27235,#27236,#27237,#27238,#27239,#27240,#27241,#27242,#27243,#27244,#27245,
#27246,#27247,#27248),.UNSPECIFIED.,.F.,.F.,(4,2,2,2,2,2,2,2,2,2,2,2,2,
2,2,2,2,2,2,2,2,2,2,2,2,2,2,2,2,2,2,2,2,2,2,2,2,2,2,2,2,2,2,2,2,2,2,2,2,
2,2,2,2,2,2,2,2,2,2,2,2,2,2,2,2,2,2,2,2,2,2,2,2,2,2,2,2,2,2,2,2,2,2,2,2,
2,2,2,2,2,2,4),(-2.43059120140729,-2.40176411519585,-2.37924065705335,-2.37191823912807,
-2.36684510743679,-2.36473671149885,-2.36321586566685,-2.3615555629141,
-2.35877998558255,-2.34924819275323,-2.31258978755237,-2.28864380702338,
-2.27931354962663,-2.2722873728991,-2.26891256605437,-2.26885041105801,
-2.26882259043734,-2.26879192438638,-2.26875805672232,-2.26872057308606,
-2.26867898886497,-2.268632733327,-2.26600523940527,-2.26298236445286,-2.25781076479936,
-2.23771651997203,-2.19527932024513,-2.1759384101753,-2.17268207697178,
-2.17091698551516,-2.16941966203352,-2.1674982700754,-2.16438153606426,
-2.1425609685007,-2.10847038795447,-2.08310668312617,-2.07782340813856,
-2.07477622294913,-2.0721113674349,-2.06880145790918,-2.06367320676321,
-2.03025474691899,-1.98720856692464,-1.98087757698263,-1.97857783629604,
-1.97702110400056,-1.97561553824432,-1.97367456521103,-1.96872052565076,
-1.9377000258246,-1.90548737825386,-1.88876505130444,-1.88406877644971,
-1.88114929104664,-1.87845857759594,-1.87498134652716,-1.86736649729363,
-1.82707107844286,-1.80459233392749,-1.7942629259308,-1.7877267676132,-1.78539878519538,
-1.7838362138004,-1.78243569868484,-1.78051474842912,-1.7756803150939,-1.74047688857932,
-1.71121863782505,-1.70070704339347,-1.69293626210463,-1.68939286501308,
-1.68670119331296,-1.68378448128163,-1.67910109205838,-1.66413884314958,
-1.65424683554806,-1.61543674897209,-1.59628315833094,-1.5930333385922,
-1.59126951169962,-1.58977187376964,-1.58784828772541,-1.58472452416869,
-1.56320591087893,-1.52887149709664,-1.50345648675929,-1.49817025296574,
-1.49512223096155,-1.49245715624619,-1.48914764185125,-1.48402129172557,
-1.45774156469356),.UNSPECIFIED.);
#1197=B_SPLINE_CURVE_WITH_KNOTS('',3,(#27253,#27254,#27255,#27256,#27257,
#27258,#27259,#27260,#27261,#27262,#27263,#27264,#27265,#27266,#27267,#27268,
#27269,#27270,#27271,#27272,#27273,#27274,#27275,#27276,#27277,#27278,#27279,
#27280,#27281,#27282,#27283,#27284,#27285,#27286,#27287,#27288,#27289,#27290,
#27291,#27292,#27293,#27294,#27295,#27296,#27297,#27298,#27299,#27300,#27301,
#27302,#27303,#27304,#27305,#27306,#27307,#27308,#27309,#27310,#27311,#27312,
#27313,#27314,#27315,#27316,#27317,#27318,#27319,#27320,#27321,#27322,#27323,
#27324,#27325,#27326,#27327,#27328,#27329,#27330,#27331,#27332,#27333,#27334,
#27335,#27336,#27337,#27338,#27339,#27340,#27341,#27342,#27343,#27344,#27345,
#27346,#27347,#27348,#27349,#27350,#27351,#27352,#27353,#27354,#27355,#27356,
#27357,#27358,#27359,#27360,#27361,#27362,#27363,#27364,#27365,#27366,#27367,
#27368,#27369,#27370,#27371,#27372,#27373,#27374,#27375,#27376,#27377,#27378,
#27379,#27380,#27381,#27382,#27383,#27384,#27385,#27386,#27387,#27388,#27389,
#27390,#27391,#27392,#27393,#27394,#27395,#27396,#27397,#27398,#27399,#27400,
#27401,#27402,#27403,#27404,#27405,#27406,#27407,#27408,#27409,#27410,#27411,
#27412,#27413,#27414,#27415,#27416,#27417,#27418,#27419,#27420,#27421,#27422,
#27423,#27424,#27425,#27426,#27427,#27428,#27429,#27430,#27431,#27432,#27433,
#27434,#27435,#27436,#27437,#27438,#27439,#27440,#27441,#27442,#27443,#27444,
#27445,#27446,#27447,#27448,#27449,#27450,#27451,#27452,#27453,#27454,#27455,
#27456),.UNSPECIFIED.,.F.,.F.,(4,2,2,2,2,2,2,2,2,2,2,2,2,2,2,2,2,2,2,2,
2,2,2,2,2,2,2,2,2,2,2,2,2,2,2,2,2,2,2,2,2,2,2,2,2,2,2,2,2,2,2,2,2,2,2,2,
2,2,2,2,2,2,2,2,2,2,2,2,2,2,2,2,2,2,2,2,2,2,2,2,2,2,2,2,2,2,2,2,2,2,2,2,
2,2,2,2,2,2,2,2,2,4),(-2.18849108915717,-2.15266013468229,-2.13281934407809,
-2.12953807643128,-2.12776459071803,-2.1262696251205,-2.12436212834478,
-2.12127664626578,-2.10117972039313,-2.06558767109897,-2.04160339281333,
-2.03538884025472,-2.03215696032724,-2.02976736911702,-2.02678602079028,
-2.0217536328847,-2.00304045513004,-1.95472191134549,-1.94416894088238,
-1.93753929223462,-1.93520875496794,-1.93365257342325,-1.93225578835142,
-1.93034928785462,-1.92559383454869,-1.8886671237466,-1.84844494068774,
-1.84195091334751,-1.83864673129327,-1.83600188812104,-1.83294821141922,
-1.82778782534966,-1.80675962260305,-1.76643055187204,-1.74633971953345,
-1.74305035011965,-1.7412745648043,-1.73977427310048,-1.73785560607621,
-1.73475232613582,-1.71448898236866,-1.67909908352295,-1.65352095508538,
-1.64822512625401,-1.64517395417711,-1.64250749105697,-1.63919799698376,
-1.63407499966821,-1.59659594405102,-1.5679143463654,-1.55774813459632,
-1.55128604804088,-1.54896793492492,-1.54740728361188,-1.54600572536922,
-1.5440787692502,-1.53920555437016,-1.50500423318681,-1.48755700157245,
-1.46953798830174,-1.46176657325522,-1.45562407869187,-1.45239637310504,
-1.44999580223646,-1.44698224204046,-1.44184898309285,-1.42206268676701,
-1.38039460898463,-1.35994186780902,-1.35664890488591,-1.35487669537028,
-1.35338027033035,-1.35146931769891,-1.34838859788563,-1.32866247366433,
-1.29274268820445,-1.26707154246869,-1.2617714319881,-1.25871962402025,
-1.25605368973657,-1.25274626062083,-1.2476291187028,-1.21544667268272,
-1.19159390250438,-1.16714204705005,-1.16398156093356,-1.16204651928411,
-1.16054735685897,-1.15879040479579,-1.1555739960999,-1.13730219780434,
-1.111015762905,-1.0746174170429,-1.06949637276067,-1.06618819079095,-1.06352283731794,
-1.06047300664893,-1.05517977129378,-1.02963633647775,-0.994598971063149,
-0.987054886639988,-0.973680670967328),.UNSPECIFIED.);
#1198=B_SPLINE_CURVE_WITH_KNOTS('',3,(#27457,#27458,#27459,#27460,#27461,
#27462,#27463,#27464,#27465,#27466,#27467,#27468,#27469,#27470,#27471,#27472,
#27473,#27474,#27475,#27476,#27477,#27478,#27479,#27480,#27481,#27482,#27483,
#27484,#27485,#27486,#27487,#27488,#27489,#27490,#27491,#27492,#27493,#27494,
#27495,#27496,#27497,#27498,#27499,#27500,#27501,#27502,#27503,#27504,#27505,
#27506,#27507,#27508,#27509,#27510,#27511,#27512,#27513,#27514,#27515,#27516,
#27517,#27518,#27519,#27520,#27521,#27522,#27523,#27524,#27525,#27526,#27527,
#27528,#27529,#27530,#27531,#27532,#27533,#27534,#27535,#27536,#27537,#27538,
#27539,#27540,#27541,#27542,#27543,#27544,#27545,#27546,#27547,#27548,#27549,
#27550,#27551,#27552,#27553,#27554,#27555,#27556,#27557,#27558,#27559,#27560,
#27561,#27562,#27563,#27564,#27565,#27566,#27567,#27568,#27569,#27570,#27571,
#27572,#27573,#27574,#27575,#27576,#27577,#27578,#27579,#27580,#27581,#27582,
#27583,#27584,#27585,#27586,#27587,#27588,#27589,#27590,#27591,#27592,#27593,
#27594,#27595,#27596,#27597,#27598,#27599,#27600,#27601,#27602,#27603,#27604,
#27605,#27606,#27607,#27608,#27609,#27610,#27611,#27612,#27613,#27614,#27615,
#27616,#27617,#27618,#27619,#27620,#27621,#27622,#27623,#27624,#27625,#27626,
#27627,#27628,#27629,#27630,#27631,#27632,#27633,#27634,#27635,#27636,#27637,
#27638,#27639,#27640,#27641,#27642,#27643,#27644,#27645,#27646,#27647,#27648,
#27649,#27650,#27651,#27652,#27653,#27654,#27655,#27656,#27657,#27658,#27659,
#27660,#27661,#27662,#27663,#27664,#27665,#27666),.UNSPECIFIED.,.F.,.F.,
(4,2,2,2,2,2,2,2,2,2,2,2,2,2,2,2,2,2,2,2,2,2,2,2,2,2,2,2,2,2,2,2,2,2,2,
2,2,2,2,2,2,2,2,2,2,2,2,2,2,2,2,2,2,2,2,2,2,2,2,2,2,2,2,2,2,2,2,2,2,2,2,
2,2,2,2,2,2,2,2,2,2,2,2,2,2,2,2,2,2,2,2,2,2,2,2,2,2,2,2,2,2,2,2,2,4),(-1.45774156469356,
-1.44739981159367,-1.42086196857323,-1.40297846348158,-1.39977814107482,
-1.39802489162989,-1.3965260130748,-1.39458758625038,-1.39141385330027,
-1.36359096878459,-1.35983368817261,-1.33512240877691,-1.31019738194206,
-1.30493554098366,-1.30189269784308,-1.29922689825234,-1.29590962827869,
-1.29075799384052,-1.25434783568208,-1.22794769439444,-1.21569342014878,
-1.2084541263403,-1.20595162122452,-1.2045103706597,-1.20298269617185,-1.20083591818395,
-1.19552938897309,-1.18775587556551,-1.16276588515745,-1.12070722810191,
-1.11391086713143,-1.11049812197198,-1.10798992813832,-1.10526752472965,
-1.10153432047915,-1.09266411867427,-1.04164484768245,-1.01700046353567,
-1.01383803011727,-1.01190282475087,-1.01040411329617,-1.00864838145331,
-1.00543660980835,-0.98727117919836,-0.960889904626584,-0.924453566308083,
-0.919322527633418,-0.916011508584598,-0.913346231091153,-0.910299081276575,
-0.905017225778567,-0.879699325078244,-0.845854186821235,-0.823684998781276,
-0.820561437869342,-0.818637867130274,-0.817140134727259,-0.815376050876469,
-0.812125556132187,-0.792956890817172,-0.754118616731859,-0.743488300243655,
-0.729182413309358,-0.724572265490336,-0.721671134195013,-0.718973363557861,
-0.715391464363775,-0.707407736370249,-0.696517620997121,-0.643187740116664,
-0.629767640441604,-0.626702273475596,-0.624959562333876,-0.62347255218525,
-0.621524341348986,-0.61736225612228,-0.611716185186961,-0.596898061999179,
-0.546733502324264,-0.535158172327656,-0.530895471465228,-0.528350851481221,
-0.525650144588506,-0.522053536958216,-0.513990430579724,-0.50295954172223,
-0.47106306676251,-0.439533622379584,-0.434589937295616,-0.432650548447213,
-0.43124514422834,-0.429688700694187,-0.427387590571668,-0.421040792031044,
-0.377695071781274,-0.344568260414681,-0.339444298874924,-0.3361364709531,
-0.333472915158102,-0.330426840172926,-0.325144641405455,-0.299778962680421,
-0.26546578814229,-0.243803969752984,-0.242412075418231),.UNSPECIFIED.);
#1199=B_SPLINE_CURVE_WITH_KNOTS('',3,(#27670,#27671,#27672,#27673,#27674,
#27675,#27676,#27677,#27678,#27679,#27680,#27681,#27682,#27683,#27684,#27685,
#27686,#27687,#27688,#27689,#27690,#27691,#27692,#27693,#27694,#27695,#27696,
#27697,#27698,#27699,#27700,#27701,#27702,#27703,#27704,#27705,#27706,#27707,
#27708,#27709,#27710,#27711,#27712,#27713,#27714,#27715,#27716,#27717,#27718,
#27719,#27720,#27721,#27722,#27723,#27724,#27725,#27726,#27727,#27728,#27729,
#27730,#27731,#27732,#27733,#27734,#27735,#27736),.UNSPECIFIED.,.F.,.F.,
(4,3,3,3,3,3,3,3,3,3,3,3,3,3,3,3,3,3,3,3,3,3,4),(-4.03543298028448,-3.99672304918318,
-3.89595759133389,-3.79533840330999,-3.69483804394509,-3.59440285562119,
-3.49400173130791,-3.39360360625489,-3.29310883660255,-3.19256758969348,
-3.09184776189799,-2.99754228688738,-2.89689019062382,-2.79638182227688,
-2.69598798286087,-2.59565665698743,-2.49535661742761,-2.39505667661869,
-2.29465488736954,-2.1942039278363,-2.09356879289011,-1.99836152459159,
-1.98502202421796),.UNSPECIFIED.);
#1200=B_SPLINE_CURVE_WITH_KNOTS('',3,(#27740,#27741,#27742,#27743,#27744),
 .UNSPECIFIED.,.F.,.F.,(4,1,4),(0.,0.99918076229579,1.09118169752329),
 .UNSPECIFIED.);
#1201=B_SPLINE_CURVE_WITH_KNOTS('',3,(#27746,#27747,#27748,#27749,#27750,
#27751,#27752,#27753,#27754,#27755,#27756,#27757,#27758,#27759,#27760,#27761,
#27762,#27763,#27764,#27765,#27766,#27767,#27768,#27769,#27770,#27771,#27772,
#27773,#27774,#27775,#27776,#27777,#27778,#27779,#27780,#27781,#27782,#27783,
#27784,#27785,#27786,#27787,#27788,#27789,#27790,#27791,#27792,#27793,#27794,
#27795,#27796,#27797,#27798,#27799,#27800,#27801,#27802,#27803,#27804,#27805,
#27806,#27807,#27808,#27809,#27810,#27811,#27812,#27813,#27814,#27815,#27816,
#27817,#27818,#27819,#27820,#27821,#27822,#27823,#27824,#27825,#27826,#27827,
#27828,#27829,#27830,#27831,#27832,#27833,#27834,#27835,#27836,#27837,#27838,
#27839,#27840,#27841,#27842,#27843,#27844,#27845,#27846,#27847,#27848,#27849,
#27850,#27851,#27852,#27853,#27854,#27855,#27856,#27857,#27858,#27859,#27860,
#27861,#27862,#27863,#27864,#27865,#27866,#27867,#27868,#27869,#27870,#27871,
#27872,#27873,#27874,#27875,#27876,#27877,#27878,#27879,#27880,#27881,#27882,
#27883,#27884,#27885,#27886,#27887,#27888,#27889,#27890,#27891,#27892,#27893,
#27894,#27895,#27896,#27897,#27898,#27899,#27900,#27901,#27902,#27903,#27904,
#27905,#27906,#27907,#27908,#27909,#27910,#27911,#27912,#27913,#27914,#27915,
#27916,#27917,#27918,#27919,#27920,#27921,#27922,#27923,#27924,#27925,#27926,
#27927,#27928,#27929,#27930,#27931,#27932,#27933,#27934,#27935,#27936,#27937,
#27938),.UNSPECIFIED.,.F.,.F.,(4,3,3,3,3,3,3,3,3,3,3,3,3,3,3,3,3,3,3,3,
3,3,3,3,3,3,3,3,3,3,3,3,3,3,3,3,3,3,3,3,3,3,3,3,3,3,3,3,3,3,3,3,3,3,3,3,
3,3,3,3,3,3,3,3,4),(1.09118169752329,1.1896959556779,1.29077915179211,1.38904433454204,
1.48725511535204,1.58544488685155,1.68867404628656,1.78698419332035,1.88536024163621,
1.98389249908034,1.99836152459159,2.09902676471727,2.19954548948454,2.29994544373208,
2.40028030446876,2.50058130287116,2.60087962797148,2.70127576315601,2.801718856171,
2.90234245763168,2.99754228688738,3.09829032006072,3.1988958757297,3.29938836910179,
3.39981920029758,3.50021947039764,3.60062024155676,3.7011231397562,3.80167552218592,
3.9024114541881,3.99672304918318,4.09719725455871,4.19752413466765,4.29773195500147,
4.39787459266619,4.49798354981372,4.59809028643905,4.6982969173245,4.798551330636,
4.89898993011201,4.99590381147897,5.09650340045884,5.19695718532926,5.29729360980329,
5.39756583082475,5.49780517353264,5.5980429218164,5.69838063612143,5.79876638986576,
5.89933520417227,5.99508457377477,6.09568510891062,6.196140215738,6.29647852714504,
6.39675297823251,6.49699489176417,6.59723554958376,6.69757669172742,6.79796616153923,
6.8985391436799,6.99426533607056,7.10763214834903,7.22058123652918,7.33282228707307,
7.37436700447423),.UNSPECIFIED.);
#1202=B_SPLINE_CURVE_WITH_KNOTS('',3,(#27940,#27941,#27942,#27943,#27944,
#27945,#27946,#27947,#27948,#27949,#27950,#27951,#27952,#27953,#27954,#27955,
#27956,#27957,#27958,#27959,#27960,#27961,#27962,#27963,#27964,#27965,#27966,
#27967,#27968,#27969,#27970,#27971,#27972,#27973,#27974,#27975,#27976,#27977,
#27978,#27979,#27980,#27981,#27982,#27983,#27984,#27985,#27986,#27987,#27988,
#27989,#27990,#27991,#27992,#27993,#27994,#27995,#27996,#27997,#27998,#27999,
#28000,#28001,#28002,#28003,#28004,#28005,#28006,#28007,#28008,#28009,#28010,
#28011,#28012,#28013,#28014,#28015,#28016,#28017,#28018,#28019,#28020,#28021,
#28022,#28023,#28024,#28025,#28026,#28027,#28028,#28029,#28030,#28031,#28032,
#28033,#28034,#28035,#28036,#28037,#28038,#28039,#28040,#28041,#28042,#28043,
#28044,#28045,#28046,#28047,#28048,#28049,#28050,#28051,#28052,#28053,#28054,
#28055,#28056,#28057,#28058,#28059,#28060,#28061,#28062,#28063,#28064,#28065,
#28066,#28067,#28068,#28069,#28070,#28071,#28072,#28073,#28074,#28075,#28076,
#28077,#28078,#28079,#28080,#28081,#28082,#28083,#28084,#28085,#28086,#28087,
#28088,#28089,#28090,#28091,#28092,#28093,#28094,#28095,#28096,#28097,#28098,
#28099,#28100,#28101,#28102,#28103,#28104,#28105,#28106,#28107,#28108,#28109,
#28110,#28111,#28112,#28113,#28114,#28115,#28116,#28117,#28118,#28119,#28120,
#28121,#28122,#28123,#28124,#28125,#28126,#28127,#28128,#28129),
 .UNSPECIFIED.,.F.,.F.,(4,3,3,3,3,3,3,3,3,3,3,3,3,3,3,3,3,3,3,3,3,3,3,3,
3,3,3,3,3,3,3,3,3,3,3,3,3,3,3,3,3,3,3,3,3,3,3,3,3,3,3,3,3,3,3,3,3,3,3,3,
3,3,3,4),(7.37436700470286,7.47544920574276,7.5765487283242,7.68077307083474,
7.78206527225033,7.88775568530835,7.99344609836636,8.09403166845495,8.19447144366285,
8.29479394118139,8.39505229193151,8.49527784072248,8.59550189117569,8.69582615791945,
8.79619857851924,8.89675441596759,8.99262686066215,9.09321116618092,9.19364970284286,
9.29397100745409,9.39422819361974,9.49445260784943,9.59467555549259,9.69499877779154,
9.7953701840505,9.89592507111648,9.99180762295794,10.0923882266938,10.1928229895668,
10.2931404293427,10.393393696979,10.4936141443668,10.5938330821875,10.6941522547303,
10.7945195828049,10.8950703914646,10.9909883852537,11.0915713241027,11.1920084546912,
11.2923283001836,11.392583995592,11.4928068894489,11.5930282890972,11.6933499304325,
11.793719735156,11.8942730043996,11.9901691475495,12.0907517522298,12.191188549124,
12.2915080632764,12.3917634289269,12.4919859950748,12.5922070695311,12.6925283919897,
12.7928978807551,12.893450842842,12.9893499098453,13.0898277925669,13.190163629574,
13.2903890484297,13.390540824841,13.4906480029083,13.590772326802,13.6575523118825),
 .UNSPECIFIED.);
#1203=B_SPLINE_CURVE_WITH_KNOTS('',3,(#28131,#28132,#28133,#28134,#28135,
#28136,#28137,#28138,#28139,#28140,#28141,#28142,#28143,#28144,#28145,#28146,
#28147,#28148,#28149,#28150,#28151,#28152,#28153,#28154,#28155,#28156,#28157,
#28158,#28159,#28160,#28161,#28162,#28163,#28164,#28165,#28166,#28167,#28168,
#28169,#28170,#28171,#28172,#28173,#28174,#28175,#28176,#28177,#28178,#28179,
#28180,#28181,#28182,#28183,#28184,#28185,#28186,#28187,#28188,#28189,#28190,
#28191,#28192,#28193,#28194,#28195,#28196,#28197,#28198,#28199,#28200,#28201,
#28202,#28203,#28204,#28205,#28206,#28207,#28208,#28209,#28210,#28211,#28212,
#28213,#28214,#28215,#28216,#28217,#28218,#28219,#28220,#28221,#28222,#28223,
#28224,#28225,#28226,#28227,#28228,#28229,#28230,#28231,#28232,#28233,#28234,
#28235,#28236,#28237,#28238,#28239,#28240,#28241,#28242,#28243,#28244,#28245,
#28246,#28247,#28248,#28249,#28250,#28251,#28252,#28253,#28254,#28255,#28256,
#28257,#28258,#28259,#28260,#28261,#28262,#28263,#28264,#28265,#28266,#28267,
#28268,#28269,#28270,#28271,#28272,#28273,#28274,#28275,#28276,#28277,#28278,
#28279,#28280,#28281,#28282,#28283,#28284,#28285,#28286,#28287,#28288,#28289,
#28290,#28291,#28292,#28293,#28294,#28295,#28296,#28297,#28298,#28299,#28300,
#28301,#28302,#28303,#28304,#28305,#28306,#28307,#28308,#28309,#28310,#28311,
#28312,#28313,#28314,#28315,#28316,#28317,#28318,#28319,#28320),
 .UNSPECIFIED.,.F.,.F.,(4,3,3,3,3,3,3,3,3,3,3,3,3,3,3,3,3,3,3,3,3,3,3,3,
3,3,3,3,3,3,3,3,3,3,3,3,3,3,3,3,3,3,3,3,3,3,3,3,3,3,3,3,3,3,3,3,3,3,3,3,
3,3,3,4),(13.6575523120968,13.774561329179,13.8928200570759,13.9885306721411,
14.089113174966,14.1895498660058,14.2898692687403,14.3901245196356,14.4903469678447,
14.590567921329,14.6908891188475,14.791258480304,14.8918113125242,14.9877114344369,
15.0882938735373,15.1887305005501,15.289049839111,15.3893050257722,15.4895274097768,
15.5897482991763,15.6900694332554,15.7904387315201,15.89099150173,15.9868921967327,
16.0874745927285,16.1879111756588,16.2882304688656,16.3884856094189,16.4887079466247,
16.5889287885971,16.6892498745856,16.7896191243191,16.8901718458187,16.9860729590285,
17.0866553946192,17.1870920177533,17.2874113518932,17.3876665338053,17.4878889127384,
17.5881097967499,17.6884309249752,17.7888002171228,17.8893529808349,17.9852537213243,
18.0858361462718,18.186272758679,18.2865920820166,18.3868472530856,18.4870696211499,
18.5872904942819,18.687611611688,18.7879808930314,18.8885336460944,18.9844344836201,
19.0843400792264,19.1841005133511,19.2837456873425,19.383328985701,19.4828826102244,
19.5824387231545,19.6820933266986,19.7818013921032,19.8816760023566,19.9407376187629),
 .UNSPECIFIED.);
#1204=B_SPLINE_CURVE_WITH_KNOTS('',3,(#28322,#28323,#28324,#28325,#28326,
#28327,#28328,#28329,#28330,#28331,#28332,#28333,#28334,#28335,#28336,#28337,
#28338,#28339,#28340,#28341,#28342,#28343,#28344,#28345,#28346,#28347,#28348,
#28349,#28350,#28351,#28352,#28353,#28354,#28355,#28356,#28357,#28358,#28359,
#28360,#28361,#28362,#28363,#28364,#28365,#28366,#28367,#28368,#28369,#28370,
#28371,#28372,#28373,#28374,#28375,#28376,#28377,#28378,#28379,#28380,#28381,
#28382,#28383,#28384,#28385,#28386,#28387,#28388,#28389,#28390,#28391,#28392,
#28393,#28394,#28395,#28396,#28397,#28398,#28399,#28400,#28401,#28402,#28403,
#28404,#28405,#28406,#28407,#28408,#28409,#28410,#28411,#28412,#28413,#28414,
#28415,#28416,#28417,#28418,#28419,#28420,#28421,#28422,#28423,#28424,#28425,
#28426,#28427,#28428,#28429,#28430,#28431,#28432,#28433,#28434,#28435,#28436,
#28437,#28438,#28439,#28440,#28441,#28442,#28443,#28444,#28445,#28446,#28447,
#28448,#28449,#28450,#28451,#28452,#28453,#28454,#28455,#28456,#28457,#28458,
#28459,#28460,#28461,#28462,#28463,#28464,#28465,#28466,#28467,#28468,#28469,
#28470,#28471,#28472,#28473,#28474,#28475,#28476,#28477,#28478,#28479,#28480,
#28481,#28482,#28483,#28484,#28485,#28486,#28487,#28488,#28489,#28490,#28491,
#28492,#28493,#28494,#28495,#28496,#28497,#28498,#28499,#28500,#28501,#28502,
#28503,#28504,#28505,#28506,#28507,#28508,#28509,#28510,#28511),
 .UNSPECIFIED.,.F.,.F.,(4,3,3,3,3,3,3,3,3,3,3,3,3,3,3,3,3,3,3,3,3,3,3,3,
3,3,3,3,3,3,3,3,3,3,3,3,3,3,3,3,3,3,3,3,3,3,3,3,3,3,3,3,3,3,3,3,3,3,3,3,
3,3,3,4),(19.9407376190621,19.9836152459159,20.0841976716306,20.1846342847766,
20.2849536088068,20.3852087805397,20.4854311492384,20.585652022974,20.6859731409308,
20.7863424227969,20.8868951763282,20.9827960082117,21.0833784322771,21.1838150437577,
21.2841343661058,21.3843895361473,21.4846119031475,21.5848327751802,21.6851538914387,
21.7855231716063,21.886075923459,21.9819767705075,22.0825591942063,22.1829958053088,
22.2833151272632,22.3835702969016,22.4837926634901,22.5840135351027,22.6843346509311,
22.7847039306623,22.8852566820731,22.9811575328033,23.0817399571192,23.1821765688491,
23.2824958914437,23.3827510617297,23.4829734289723,23.5831943012447,23.6835154177372,
23.783884698136,23.8844374502123,23.9803382950991,24.0809207191718,24.1813573306558,
24.2816766530015,24.381931823037,24.4821541900276,24.5823750620472,24.682696178287,
24.7830654584328,24.8836182102586,24.9795190573948,25.0801014814436,25.1805380929028,
25.2808574152219,25.3811125852299,25.4813349521921,25.5815558241822,25.6818769403915,
25.7822462205059,25.8827989722996,25.9786998196906,26.1100759682844,26.2239229259801),
 .UNSPECIFIED.);
#1205=B_SPLINE_CURVE_WITH_KNOTS('',3,(#28513,#28514,#28515,#28516,#28517,
#28518,#28519,#28520,#28521,#28522,#28523,#28524,#28525,#28526,#28527,#28528,
#28529,#28530,#28531,#28532,#28533,#28534,#28535,#28536,#28537,#28538,#28539,
#28540,#28541,#28542,#28543,#28544,#28545,#28546,#28547,#28548,#28549,#28550,
#28551,#28552,#28553,#28554,#28555,#28556,#28557,#28558,#28559,#28560,#28561,
#28562,#28563,#28564,#28565,#28566,#28567,#28568,#28569,#28570,#28571,#28572,
#28573,#28574,#28575,#28576,#28577,#28578,#28579,#28580,#28581,#28582,#28583,
#28584,#28585,#28586,#28587,#28588,#28589,#28590,#28591,#28592,#28593,#28594,
#28595,#28596,#28597,#28598,#28599,#28600,#28601,#28602,#28603,#28604,#28605,
#28606,#28607,#28608,#28609,#28610,#28611,#28612,#28613,#28614,#28615,#28616,
#28617,#28618,#28619,#28620,#28621,#28622,#28623,#28624,#28625,#28626,#28627,
#28628,#28629,#28630,#28631,#28632,#28633,#28634,#28635,#28636,#28637,#28638,
#28639,#28640,#28641,#28642,#28643,#28644,#28645,#28646,#28647,#28648,#28649,
#28650,#28651,#28652,#28653,#28654,#28655,#28656,#28657,#28658,#28659,#28660,
#28661,#28662,#28663,#28664,#28665,#28666,#28667,#28668,#28669,#28670,#28671,
#28672,#28673,#28674,#28675,#28676,#28677,#28678,#28679,#28680,#28681,#28682,
#28683,#28684,#28685,#28686,#28687,#28688,#28689,#28690,#28691,#28692,#28693,
#28694,#28695,#28696,#28697,#28698,#28699,#28700,#28701,#28702),
 .UNSPECIFIED.,.F.,.F.,(4,3,3,3,3,3,3,3,3,3,3,3,3,3,3,3,3,3,3,3,3,3,3,3,
3,3,3,3,3,3,3,3,3,3,3,3,3,3,3,3,3,3,3,3,3,3,3,3,3,3,3,3,3,3,3,3,3,3,3,3,
3,3,3,4),(26.2239229262416,26.3230559083015,26.4221251848231,26.5211634966858,
26.6202035420719,26.7193428737506,26.8185358680633,26.9178980737154,26.9778805819864,
27.0784630060752,27.1788996175751,27.2792189399362,27.3794741099869,27.4796964769925,
27.5799173490265,27.6802384652802,27.7806077454396,27.8811604972783,27.9770613442822,
28.077643768371,28.1780803798707,28.2783997022315,28.3786548722818,28.4788772392868,
28.5790981113202,28.6794192275731,28.7797885077316,28.8803412595694,28.976242106578,
29.0768245306755,29.1772611421844,29.2775804645544,29.3778356346138,29.4780580016284,
29.5782788736713,29.6785999899338,29.778969270102,29.8795220219494,29.9754228688738,
30.0760052929666,30.1764419044703,30.2767612268354,30.3770163968898,30.4772387638994,
30.5774596359376,30.6777807521952,30.7781500323582,30.8787027842006,30.9746036311696,
31.0751860552629,31.1756226667668,31.2759419891322,31.3761971591871,31.4764195261968,
31.5766403982353,31.676961514493,31.7773307946564,31.8778835464991,31.9737843934654,
32.0780783946679,32.1853358543562,32.2892156838711,32.3981619586461,32.5071082334212),
 .UNSPECIFIED.);
#1206=B_SPLINE_CURVE_WITH_KNOTS('',3,(#28704,#28705,#28706,#28707,#28708,
#28709,#28710,#28711,#28712,#28713,#28714,#28715,#28716,#28717,#28718,#28719,
#28720,#28721,#28722,#28723,#28724,#28725,#28726,#28727,#28728,#28729,#28730,
#28731,#28732,#28733,#28734,#28735,#28736,#28737,#28738,#28739,#28740,#28741,
#28742,#28743,#28744,#28745,#28746,#28747,#28748,#28749,#28750,#28751,#28752,
#28753,#28754,#28755,#28756,#28757,#28758,#28759,#28760,#28761,#28762,#28763,
#28764,#28765,#28766,#28767,#28768,#28769,#28770,#28771,#28772,#28773,#28774,
#28775,#28776,#28777,#28778,#28779,#28780,#28781,#28782,#28783,#28784,#28785,
#28786,#28787,#28788,#28789,#28790,#28791,#28792,#28793,#28794,#28795,#28796,
#28797,#28798,#28799,#28800,#28801,#28802,#28803,#28804,#28805,#28806,#28807,
#28808,#28809,#28810,#28811,#28812,#28813,#28814,#28815,#28816,#28817,#28818,
#28819,#28820,#28821,#28822,#28823,#28824,#28825,#28826,#28827,#28828,#28829,
#28830,#28831,#28832,#28833,#28834,#28835,#28836,#28837,#28838,#28839,#28840,
#28841,#28842,#28843,#28844,#28845,#28846,#28847,#28848,#28849,#28850,#28851,
#28852,#28853,#28854,#28855,#28856,#28857,#28858,#28859,#28860,#28861,#28862,
#28863,#28864,#28865,#28866,#28867,#28868,#28869,#28870,#28871,#28872,#28873,
#28874,#28875,#28876,#28877,#28878,#28879,#28880,#28881,#28882,#28883,#28884,
#28885,#28886,#28887,#28888,#28889,#28890,#28891,#28892,#28893,#28894,#28895,
#28896),.UNSPECIFIED.,.F.,.F.,(4,3,3,3,3,3,3,3,3,3,3,3,3,3,3,3,3,3,3,3,
3,3,3,3,3,3,3,3,3,3,3,3,3,3,3,3,3,3,3,3,3,3,3,3,3,3,3,3,3,3,3,3,3,3,3,3,
3,3,3,3,3,3,3,3,4),(32.5071082337745,32.6136854124345,32.7206393044122,
32.8277947974754,32.935264742081,32.9729651557612,33.0735475798547,33.1739841913593,
33.274303513725,33.3745586837803,33.4747810507904,33.575001922829,33.6753230390872,
33.775692319251,33.8762450710941,33.972145918057,34.0727283421507,34.1731649536554,
34.2734842760213,34.3737394460767,34.473961813087,34.5741826851257,34.6745038013841,
34.7748730815481,34.8754258333912,34.9713266803528,35.0719091044466,35.1723457159514,
35.2726650383175,35.372920208373,35.4731425753834,35.5733634474223,35.6736845636808,
35.7740538438449,35.8746065956882,35.9705074426486,36.0710898667423,36.1715264782471,
36.271845800613,36.3721009706685,36.4723233376788,36.5725442097176,36.672865325976,
36.77323460614,36.8737873579833,36.9696882049444,37.0702706290381,37.1707072405429,
37.2710265629088,37.3712817329643,37.4715040999747,37.5717249720135,37.6720460882719,
37.772415368436,37.8729681202792,37.9688689672402,38.0715470388752,38.1704609817843,
38.2692818278376,38.3680426710374,38.4667765229307,38.5655590052605,38.6643713321975,
38.7632960917447,38.7902935403205),.UNSPECIFIED.);
#1207=B_SPLINE_CURVE_WITH_KNOTS('',3,(#28898,#28899,#28900,#28901,#28902,
#28903,#28904,#28905,#28906,#28907,#28908,#28909,#28910,#28911,#28912,#28913,
#28914,#28915,#28916,#28917,#28918,#28919,#28920,#28921,#28922,#28923,#28924,
#28925,#28926,#28927,#28928,#28929,#28930,#28931,#28932,#28933,#28934,#28935,
#28936,#28937,#28938,#28939,#28940,#28941,#28942,#28943,#28944,#28945,#28946,
#28947,#28948,#28949,#28950,#28951,#28952,#28953,#28954,#28955,#28956,#28957,
#28958,#28959,#28960,#28961,#28962,#28963,#28964,#28965,#28966,#28967,#28968,
#28969,#28970,#28971,#28972,#28973,#28974,#28975,#28976,#28977,#28978,#28979,
#28980,#28981,#28982,#28983,#28984,#28985,#28986,#28987,#28988,#28989,#28990,
#28991,#28992,#28993,#28994,#28995,#28996,#28997,#28998,#28999,#29000,#29001,
#29002,#29003,#29004,#29005,#29006,#29007,#29008,#29009,#29010,#29011,#29012,
#29013,#29014,#29015,#29016,#29017,#29018,#29019,#29020,#29021,#29022,#29023,
#29024,#29025,#29026,#29027,#29028,#29029,#29030,#29031,#29032,#29033,#29034,
#29035,#29036,#29037,#29038,#29039,#29040,#29041,#29042,#29043,#29044,#29045,
#29046,#29047,#29048,#29049,#29050,#29051,#29052,#29053,#29054,#29055,#29056,
#29057,#29058,#29059,#29060,#29061,#29062,#29063,#29064,#29065,#29066,#29067,
#29068,#29069,#29070,#29071,#29072,#29073,#29074,#29075,#29076,#29077,#29078,
#29079,#29080,#29081,#29082,#29083,#29084,#29085,#29086,#29087),
 .UNSPECIFIED.,.F.,.F.,(4,3,3,3,3,3,3,3,3,3,3,3,3,3,3,3,3,3,3,3,3,3,3,3,
3,3,3,3,3,3,3,3,3,3,3,3,3,3,3,3,3,3,3,3,3,3,3,3,3,3,3,3,3,3,3,3,3,3,3,3,
3,3,3,4),(38.7902935406008,38.9439982042354,38.968049729536,39.0686321536296,
39.1690687651342,39.2693880875,39.3696432575553,39.4698656245654,39.5700864966042,
39.6704076128624,39.7707768930262,39.8713296448693,39.9672304918318,40.0678129159255,
40.1682495274303,40.2685688497962,40.3688240198517,40.469046386862,40.5692672589008,
40.6695883751592,40.7699576553232,40.8705104071664,40.9664112541276,41.0669936782214,
41.1674302897262,41.2677496120922,41.3680047821478,41.4682271491582,41.5684480211971,
41.6687691374555,41.7691384176196,41.8696911694629,41.9655920164233,42.0661744405169,
42.1666110520216,42.2669303743875,42.3671855444429,42.4674079114532,42.567628783492,
42.6679498997503,42.7683191799143,42.8688719317574,42.9647727787191,43.0653552028129,
43.1657918143178,43.2661111366838,43.3663663067393,43.4665886737497,43.5668095457887,
43.6671306620471,43.7674999422112,43.8680526940545,43.9639535410149,44.0645359651086,
44.1649725766133,44.2652918989792,44.3655470690347,44.465769436045,44.5659903080837,
44.6663114243421,44.7666807045061,44.8672334563492,44.9631343033107,45.0734788477804),
 .UNSPECIFIED.);
#1208=B_SPLINE_CURVE_WITH_KNOTS('',3,(#29089,#29090,#29091,#29092,#29093,
#29094,#29095,#29096,#29097,#29098,#29099,#29100,#29101,#29102,#29103,#29104,
#29105,#29106,#29107,#29108,#29109,#29110,#29111,#29112,#29113,#29114,#29115,
#29116,#29117,#29118,#29119,#29120,#29121,#29122,#29123,#29124,#29125,#29126,
#29127,#29128,#29129,#29130,#29131,#29132,#29133,#29134,#29135,#29136,#29137,
#29138,#29139,#29140,#29141,#29142,#29143,#29144,#29145,#29146,#29147,#29148,
#29149,#29150,#29151,#29152,#29153,#29154,#29155,#29156,#29157,#29158,#29159,
#29160,#29161,#29162,#29163,#29164,#29165,#29166,#29167,#29168,#29169,#29170,
#29171,#29172,#29173,#29174,#29175,#29176,#29177,#29178,#29179,#29180,#29181,
#29182,#29183,#29184,#29185,#29186,#29187,#29188,#29189,#29190,#29191,#29192,
#29193,#29194,#29195,#29196,#29197,#29198,#29199,#29200,#29201,#29202,#29203,
#29204,#29205,#29206,#29207,#29208,#29209,#29210,#29211,#29212,#29213,#29214,
#29215,#29216,#29217,#29218,#29219,#29220,#29221,#29222,#29223,#29224,#29225,
#29226,#29227,#29228,#29229,#29230,#29231,#29232,#29233,#29234,#29235,#29236,
#29237,#29238,#29239,#29240,#29241,#29242,#29243,#29244,#29245,#29246,#29247,
#29248,#29249,#29250,#29251,#29252,#29253,#29254,#29255,#29256,#29257,#29258,
#29259,#29260,#29261,#29262,#29263,#29264,#29265,#29266,#29267,#29268,#29269,
#29270,#29271,#29272,#29273,#29274,#29275,#29276,#29277,#29278),
 .UNSPECIFIED.,.F.,.F.,(4,3,3,3,3,3,3,3,3,3,3,3,3,3,3,3,3,3,3,3,3,3,3,3,
3,3,3,3,3,3,3,3,3,3,3,3,3,3,3,3,3,3,3,3,3,3,3,3,3,3,3,3,3,3,3,3,3,3,3,3,
3,3,3,4),(45.0734788480091,45.1726643676828,45.2717096259563,45.3706772508578,
45.4696001387515,45.5685111265611,45.6675114574198,45.7665534619267,45.8657746186064,
45.9623150656065,46.0628974897002,46.1633341012049,46.2636534235708,46.3639085936263,
46.4641309606367,46.5643518326753,46.6646729489337,46.7650422290977,46.8655949809409,
46.9614958279023,47.062078251996,47.1625148635009,47.2628341858669,47.3630893559225,
47.4633117229327,47.5635325949716,47.6638537112301,47.764222991394,47.8647757432373,
47.9606765901981,48.0612590142918,48.1616956257966,48.2620149481625,48.3622701182179,
48.4624924852283,48.562713357267,48.6630344735255,48.7634037536895,48.8639565055327,
48.9598573524939,49.0604397765875,49.1608763880926,49.2611957104586,49.3614508805141,
49.4616732475243,49.5618941195634,49.6622152358218,49.7625845159858,49.863137267829,
49.9590381147897,50.0596205388833,50.1600571503878,50.2603764727537,50.3606316428091,
50.4608540098193,50.5610748818582,50.6613959981166,50.7617652782805,50.8623180301237,
50.9582188770855,51.070080858906,51.181585042824,51.2924809446677,51.3566641547469),
 .UNSPECIFIED.);
#1209=B_SPLINE_CURVE_WITH_KNOTS('',3,(#29280,#29281,#29282,#29283,#29284,
#29285,#29286,#29287,#29288,#29289,#29290,#29291,#29292,#29293,#29294,#29295,
#29296,#29297,#29298,#29299,#29300,#29301,#29302,#29303,#29304,#29305,#29306,
#29307,#29308,#29309,#29310,#29311,#29312,#29313,#29314,#29315,#29316,#29317,
#29318,#29319,#29320,#29321,#29322,#29323,#29324,#29325,#29326,#29327,#29328,
#29329,#29330,#29331,#29332,#29333,#29334,#29335,#29336,#29337,#29338,#29339,
#29340,#29341,#29342,#29343,#29344,#29345,#29346,#29347,#29348,#29349,#29350,
#29351,#29352,#29353,#29354,#29355,#29356,#29357,#29358,#29359,#29360,#29361,
#29362,#29363,#29364,#29365,#29366,#29367,#29368,#29369,#29370,#29371,#29372,
#29373,#29374,#29375,#29376,#29377,#29378,#29379,#29380,#29381,#29382,#29383,
#29384,#29385,#29386,#29387,#29388,#29389,#29390,#29391,#29392,#29393,#29394,
#29395,#29396,#29397,#29398,#29399,#29400,#29401,#29402,#29403,#29404,#29405,
#29406,#29407,#29408,#29409,#29410,#29411,#29412,#29413,#29414,#29415,#29416,
#29417,#29418,#29419,#29420,#29421,#29422,#29423,#29424,#29425,#29426,#29427,
#29428,#29429,#29430,#29431,#29432,#29433,#29434,#29435,#29436,#29437,#29438,
#29439,#29440,#29441,#29442,#29443,#29444,#29445,#29446,#29447,#29448,#29449,
#29450,#29451,#29452,#29453,#29454,#29455,#29456,#29457,#29458,#29459,#29460,
#29461,#29462,#29463,#29464,#29465,#29466,#29467,#29468,#29469),
 .UNSPECIFIED.,.F.,.F.,(4,3,3,3,3,3,3,3,3,3,3,3,3,3,3,3,3,3,3,3,3,3,3,3,
3,3,3,3,3,3,3,3,3,3,3,3,3,3,3,3,3,3,3,3,3,3,3,3,3,3,3,3,3,3,3,3,3,3,3,3,
3,3,3,4),(51.35666415496,51.4582046051034,51.5597783328067,51.6614969549953,
51.7632886368995,51.8652929421708,51.9573996393813,52.057982063475,52.1584186749796,
52.2587379973455,52.3589931674009,52.4592155344113,52.5594364064501,52.6597575227085,
52.7601268028724,52.8606795547156,52.9565804016771,53.0571628257708,53.1575994372756,
53.2579187596415,53.358173929697,53.4583962967073,53.5586171687462,53.6589382850046,
53.7593075651686,53.8598603170118,53.9557611639729,54.0563435880666,54.1567801995714,
54.2570995219374,54.3573546919928,54.4575770590032,54.5577979310419,54.6581190473004,
54.7584883274645,54.8590410793077,54.9549419262687,55.0555243503623,55.1559609618672,
55.2562802842331,55.3565354542886,55.456757821299,55.556978693338,55.6572998095964,
55.7576690897604,55.8582218416037,55.9541226885645,56.0547051126583,56.1551417241628,
56.2554610465287,56.3557162165841,56.4559385835944,56.556159455633,56.6564805718914,
56.7568498520554,56.8574026038986,56.9533034508602,57.053466577448,57.1534907762757,
57.2534080991903,57.3532611161024,57.4530730259249,57.5529179342892,57.6398494621396),
 .UNSPECIFIED.);
#1210=B_SPLINE_CURVE_WITH_KNOTS('',3,(#29471,#29472,#29473,#29474,#29475,
#29476,#29477,#29478,#29479,#29480,#29481,#29482,#29483,#29484,#29485,#29486,
#29487,#29488,#29489,#29490,#29491,#29492,#29493,#29494,#29495,#29496,#29497,
#29498,#29499,#29500,#29501,#29502,#29503,#29504,#29505,#29506,#29507,#29508,
#29509,#29510,#29511,#29512,#29513,#29514,#29515,#29516,#29517,#29518,#29519,
#29520,#29521,#29522,#29523,#29524,#29525,#29526,#29527,#29528,#29529,#29530,
#29531,#29532,#29533,#29534,#29535,#29536,#29537,#29538,#29539,#29540,#29541,
#29542,#29543,#29544,#29545,#29546,#29547,#29548,#29549,#29550,#29551,#29552,
#29553,#29554,#29555,#29556,#29557,#29558,#29559,#29560,#29561,#29562,#29563,
#29564,#29565,#29566,#29567,#29568,#29569,#29570,#29571,#29572,#29573,#29574,
#29575,#29576,#29577,#29578,#29579,#29580,#29581,#29582,#29583,#29584,#29585,
#29586,#29587,#29588,#29589,#29590,#29591,#29592,#29593,#29594,#29595,#29596,
#29597,#29598,#29599,#29600,#29601,#29602,#29603,#29604,#29605,#29606,#29607,
#29608,#29609,#29610,#29611,#29612,#29613,#29614,#29615,#29616,#29617,#29618,
#29619,#29620,#29621,#29622,#29623,#29624,#29625,#29626,#29627,#29628,#29629,
#29630,#29631,#29632,#29633,#29634,#29635,#29636,#29637,#29638,#29639,#29640,
#29641,#29642,#29643,#29644,#29645,#29646,#29647,#29648,#29649,#29650,#29651,
#29652,#29653,#29654,#29655,#29656,#29657,#29658,#29659,#29660),
 .UNSPECIFIED.,.F.,.F.,(4,3,3,3,3,3,3,3,3,3,3,3,3,3,3,3,3,3,3,3,3,3,3,3,
3,3,3,3,3,3,3,3,3,3,3,3,3,3,3,3,3,3,3,3,3,3,3,3,3,3,3,3,3,3,3,3,3,3,3,3,
3,3,3,4),(57.6398494625214,57.7589701131946,57.8795801756191,57.9524842131561,
58.0530666372499,58.1535032487546,58.2538225711206,58.354077741176,58.4543001081864,
58.5545209802252,58.6548420964837,58.7552113766477,58.855764128491,58.9516649754518,
59.0522473995455,59.1526840110503,59.2530033334162,59.3532585034717,59.4534808704821,
59.553701742521,59.6540228587794,59.7543921389434,59.8549448907867,59.9508457377476,
60.0514281618413,60.1518647733461,60.252184095712,60.3524392657675,60.4526616327778,
60.5528825048166,60.653203621075,60.753572901239,60.8541256530822,60.9500265000434,
61.0506089241371,61.1510455356419,61.2513648580079,61.3516200280634,61.4518423950738,
61.5520632671126,61.652384383371,61.752753663535,61.8533064153783,61.9492072623392,
62.0497896864329,62.1502262979376,62.2505456203036,62.3508007903591,62.4510231573694,
62.5512440294082,62.6515651456666,62.7519344258307,62.8524871776739,62.948388024635,
63.0485570779958,63.1485806798993,63.2484883191134,63.3483332353989,63.4481473208821,
63.5479624276795,63.6478773952426,63.7478438550818,63.8479848096707,63.9230347689432),
 .UNSPECIFIED.);
#1211=B_SPLINE_CURVE_WITH_KNOTS('',3,(#29662,#29663,#29664,#29665,#29666,
#29667,#29668,#29669,#29670,#29671,#29672,#29673,#29674,#29675,#29676,#29677,
#29678,#29679,#29680,#29681,#29682,#29683,#29684,#29685,#29686,#29687,#29688,
#29689,#29690,#29691,#29692,#29693,#29694,#29695,#29696,#29697,#29698,#29699,
#29700,#29701,#29702,#29703,#29704,#29705,#29706,#29707,#29708,#29709,#29710,
#29711,#29712,#29713,#29714,#29715,#29716,#29717,#29718,#29719,#29720,#29721,
#29722,#29723,#29724,#29725,#29726,#29727,#29728,#29729,#29730,#29731,#29732,
#29733,#29734,#29735,#29736,#29737,#29738,#29739,#29740,#29741,#29742,#29743,
#29744,#29745,#29746,#29747,#29748,#29749,#29750,#29751,#29752,#29753,#29754,
#29755,#29756,#29757,#29758,#29759,#29760,#29761,#29762,#29763,#29764,#29765,
#29766,#29767,#29768,#29769,#29770,#29771,#29772,#29773,#29774,#29775,#29776,
#29777,#29778,#29779,#29780,#29781,#29782,#29783,#29784,#29785,#29786,#29787,
#29788,#29789,#29790,#29791,#29792,#29793,#29794,#29795,#29796,#29797,#29798,
#29799,#29800,#29801,#29802,#29803,#29804,#29805,#29806,#29807,#29808,#29809,
#29810,#29811,#29812,#29813,#29814,#29815,#29816,#29817,#29818,#29819,#29820,
#29821,#29822,#29823,#29824,#29825,#29826,#29827,#29828,#29829,#29830,#29831,
#29832,#29833,#29834,#29835,#29836,#29837,#29838,#29839,#29840,#29841,#29842,
#29843,#29844,#29845,#29846,#29847,#29848,#29849,#29850,#29851),
 .UNSPECIFIED.,.F.,.F.,(4,3,3,3,3,3,3,3,3,3,3,3,3,3,3,3,3,3,3,3,3,3,3,3,
3,3,3,3,3,3,3,3,3,3,3,3,3,3,3,3,3,3,3,3,3,3,3,3,3,3,3,3,3,3,3,3,3,3,3,3,
3,3,3,4),(63.9230347693192,63.9475687869308,64.0481512110245,64.1485878225294,
64.2489071448954,64.3491623149509,64.4493846819612,64.5496055540001,64.6499266702586,
64.7502959504226,64.8508487022659,64.9467495492266,65.0473319733203,65.1477685848251,
65.248087907191,65.3483430772466,65.448565444257,65.5487863162958,65.6491074325543,
65.7494767127183,65.8500294645616,65.9459303115224,66.0465127356161,66.1469493471208,
66.2472686694868,66.3475238395422,66.4477462065526,66.5479670785914,66.6482881948498,
66.7486574750138,66.849210226857,66.9451110738182,67.0456934979119,67.1461301094167,
67.2464494317826,67.3467046018381,67.4469269688484,67.5471478408872,67.6474689571456,
67.7478382373096,67.8483909891528,67.944291836114,68.0448742602077,68.1453108717125,
68.2456301940785,68.345885364134,68.4461077311443,68.5463286031831,68.6466497194415,
68.7470189996055,68.8475717514488,68.9434725984098,69.0440550225035,69.1444916340084,
69.2448109563743,69.3450661264298,69.4452884934402,69.5455093654791,69.6458304817376,
69.7461997619017,69.8467525137449,69.9426533607056,70.0744367184332,70.2062200761607),
 .UNSPECIFIED.);
#1212=B_SPLINE_CURVE_WITH_KNOTS('',3,(#29853,#29854,#29855,#29856,#29857,
#29858,#29859,#29860,#29861,#29862,#29863,#29864,#29865,#29866,#29867,#29868,
#29869,#29870,#29871,#29872,#29873,#29874,#29875,#29876,#29877,#29878,#29879,
#29880,#29881,#29882,#29883,#29884,#29885,#29886,#29887,#29888,#29889,#29890,
#29891,#29892,#29893,#29894,#29895,#29896,#29897,#29898,#29899,#29900,#29901,
#29902,#29903,#29904,#29905,#29906,#29907,#29908,#29909,#29910,#29911,#29912,
#29913,#29914,#29915,#29916,#29917,#29918,#29919,#29920,#29921,#29922,#29923,
#29924,#29925,#29926,#29927,#29928,#29929,#29930,#29931,#29932,#29933,#29934,
#29935,#29936,#29937,#29938,#29939,#29940,#29941,#29942,#29943,#29944,#29945,
#29946,#29947,#29948,#29949,#29950,#29951,#29952,#29953,#29954,#29955,#29956,
#29957,#29958,#29959,#29960,#29961,#29962,#29963,#29964,#29965,#29966,#29967,
#29968,#29969,#29970,#29971,#29972,#29973,#29974,#29975,#29976,#29977,#29978,
#29979,#29980,#29981,#29982,#29983,#29984,#29985,#29986,#29987,#29988,#29989,
#29990,#29991,#29992,#29993,#29994,#29995,#29996,#29997,#29998,#29999,#30000,
#30001,#30002,#30003,#30004,#30005,#30006,#30007,#30008,#30009,#30010,#30011,
#30012,#30013,#30014,#30015,#30016,#30017,#30018,#30019,#30020,#30021,#30022,
#30023,#30024,#30025,#30026,#30027,#30028,#30029,#30030,#30031,#30032,#30033,
#30034,#30035,#30036,#30037,#30038,#30039,#30040,#30041,#30042,#30043,#30044,
#30045),.UNSPECIFIED.,.F.,.F.,(4,3,3,3,3,3,3,3,3,3,3,3,3,3,3,3,3,3,3,3,
3,3,3,3,3,3,3,3,3,3,3,3,3,3,3,3,3,3,3,3,3,3,3,3,3,3,3,3,3,3,3,3,3,3,3,3,
3,3,3,3,3,3,3,3,4),(70.2062200764988,70.305495551724,70.4047158033365,70.503913389098,
70.6031208337801,70.7024336389929,70.8018070712722,70.9013453472432,70.9418341230014,
71.0424165470951,71.1428531586,71.243172480966,71.3434276510215,71.4436500180318,
71.5438708900706,71.644192006329,71.744561286493,71.8451140383363,71.9410148852972,
72.0415973093909,72.1420339208956,72.2423532432615,72.3426084133169,72.4428307803273,
72.5430516523662,72.6433727686245,72.7437420487885,72.8442948006317,72.9401956475929,
73.0407780716866,73.1412146831914,73.2415340055574,73.3417891756129,73.4420115426231,
73.5422324146621,73.6425535309205,73.7429228110844,73.8434755629275,73.9393764098887,
74.0399588339824,74.1403954454876,74.2407147678536,74.340969937909,74.4411923049193,
74.5414131769583,74.6417342932166,74.7421035733806,74.8426563252239,74.9385571721845,
75.0391395962781,75.139576207783,75.239895530149,75.3401507002046,75.440373067215,
75.5405939392537,75.6409150555122,75.7412843356761,75.8418370875194,75.9377379344803,
76.0413335477396,76.1447484660192,76.247965445848,76.3510651505503,76.4540511721591,
76.4894053836784),.UNSPECIFIED.);
#1213=B_SPLINE_CURVE_WITH_KNOTS('',3,(#30047,#30048,#30049,#30050,#30051,
#30052,#30053,#30054,#30055,#30056,#30057,#30058,#30059,#30060,#30061,#30062,
#30063,#30064,#30065,#30066,#30067,#30068,#30069,#30070,#30071,#30072,#30073,
#30074,#30075,#30076,#30077,#30078,#30079,#30080,#30081,#30082,#30083,#30084,
#30085,#30086,#30087,#30088,#30089,#30090,#30091,#30092,#30093,#30094,#30095,
#30096,#30097,#30098,#30099,#30100,#30101,#30102,#30103,#30104,#30105,#30106,
#30107,#30108,#30109,#30110,#30111,#30112,#30113,#30114,#30115,#30116,#30117,
#30118,#30119,#30120,#30121,#30122,#30123,#30124,#30125,#30126,#30127,#30128,
#30129,#30130,#30131,#30132,#30133,#30134,#30135,#30136,#30137,#30138,#30139,
#30140,#30141,#30142,#30143,#30144,#30145,#30146,#30147,#30148,#30149,#30150,
#30151,#30152,#30153,#30154,#30155,#30156,#30157,#30158,#30159,#30160,#30161,
#30162,#30163,#30164,#30165,#30166,#30167,#30168,#30169,#30170,#30171,#30172,
#30173,#30174,#30175,#30176,#30177,#30178,#30179,#30180,#30181,#30182,#30183,
#30184,#30185,#30186,#30187,#30188,#30189,#30190,#30191,#30192,#30193,#30194,
#30195,#30196,#30197,#30198,#30199,#30200,#30201,#30202,#30203,#30204,#30205,
#30206,#30207,#30208,#30209,#30210,#30211,#30212,#30213,#30214,#30215,#30216,
#30217,#30218,#30219,#30220,#30221,#30222,#30223,#30224,#30225,#30226,#30227,
#30228,#30229,#30230,#30231,#30232,#30233,#30234,#30235,#30236),
 .UNSPECIFIED.,.F.,.F.,(4,3,3,3,3,3,3,3,3,3,3,3,3,3,3,3,3,3,3,3,3,3,3,3,
3,3,3,3,3,3,3,3,3,3,3,3,3,3,3,3,3,3,3,3,3,3,3,3,3,3,3,3,3,3,3,3,3,3,3,3,
3,3,3,4),(76.4894053839406,76.6012837121495,76.7092937118267,76.8231062043014,
76.9369186967761,77.0375011208698,77.1379377323746,77.2382570547405,77.338512224796,
77.4387345918064,77.5389554638453,77.6392765801037,77.7396458602678,77.840198612111,
77.9360994590719,78.0366818831656,78.1371184946705,78.2374378170365,78.337692987092,
78.4379153541024,78.5381362261413,78.6384573423997,78.7388266225638,78.8393793744071,
78.9352802213677,79.0358626454614,79.1362992569661,79.2366185793321,79.3368737493875,
79.4370961163978,79.5373169884366,79.637638104695,79.7380073848589,79.8385601367021,
79.9344609836635,80.0350434077572,80.135480019262,80.235799341628,80.3360545116835,
80.4362768786938,80.5364977507326,80.636818866991,80.737188147155,80.8377408989983,
80.9336417459593,81.0342241700531,81.1346607815578,81.2349801039237,81.3352352739792,
81.4354576409896,81.5356785130284,81.6359996292869,81.7363689094508,81.8369216612941,
81.9328225082551,82.0319079799504,82.130826023152,82.229650296528,82.3284138954426,
82.427149832368,82.5259386101351,82.6247563736218,82.723698889131,82.7725906905032),
 .UNSPECIFIED.);
#1214=B_SPLINE_CURVE_WITH_KNOTS('',3,(#30238,#30239,#30240,#30241,#30242,
#30243,#30244,#30245,#30246,#30247,#30248,#30249,#30250,#30251,#30252,#30253,
#30254,#30255,#30256,#30257,#30258,#30259,#30260,#30261,#30262,#30263,#30264,
#30265,#30266,#30267,#30268,#30269,#30270,#30271,#30272,#30273,#30274,#30275,
#30276,#30277,#30278,#30279,#30280,#30281,#30282,#30283,#30284,#30285,#30286,
#30287,#30288,#30289,#30290,#30291,#30292,#30293,#30294,#30295,#30296,#30297,
#30298,#30299,#30300,#30301,#30302,#30303,#30304,#30305,#30306,#30307,#30308,
#30309,#30310,#30311,#30312,#30313,#30314,#30315,#30316,#30317,#30318,#30319,
#30320,#30321,#30322,#30323,#30324,#30325,#30326,#30327,#30328,#30329,#30330,
#30331,#30332,#30333,#30334,#30335,#30336,#30337,#30338,#30339,#30340,#30341,
#30342,#30343,#30344,#30345,#30346,#30347,#30348,#30349,#30350,#30351,#30352,
#30353,#30354,#30355,#30356,#30357,#30358,#30359,#30360,#30361,#30362,#30363,
#30364,#30365,#30366,#30367,#30368,#30369,#30370,#30371,#30372,#30373,#30374,
#30375,#30376,#30377,#30378,#30379,#30380,#30381,#30382,#30383,#30384,#30385,
#30386,#30387,#30388,#30389,#30390,#30391,#30392,#30393,#30394,#30395,#30396,
#30397,#30398,#30399,#30400,#30401,#30402,#30403,#30404,#30405,#30406,#30407,
#30408,#30409,#30410,#30411,#30412,#30413,#30414,#30415,#30416,#30417,#30418,
#30419,#30420,#30421,#30422,#30423,#30424),.UNSPECIFIED.,.F.,.F.,(4,3,3,
3,3,3,3,3,3,3,3,3,3,3,3,3,3,3,3,3,3,3,3,3,3,3,3,3,3,3,3,3,3,3,3,3,3,3,3,
3,3,3,3,3,3,3,3,3,3,3,3,3,3,3,3,3,3,3,3,3,3,3,4),(82.772590690858,82.9320032705509,
83.0325856946445,83.1330223061491,83.2333416285149,83.3335967985702,83.4338191655803,
83.5340400376191,83.6343611538773,83.7347304340412,83.8352831858843,83.9311840328467,
84.0317664569405,84.1322030684453,84.2325223908113,84.3327775608669,84.4329999278774,
84.5332207999163,84.6335419161747,84.7339111963388,84.8344639481822,84.9303647951425,
85.0309472192362,85.131383830741,85.231703153107,85.3319583231625,85.4321806901728,
85.5324015622116,85.63272267847,85.733091958634,85.8336447104773,85.9295455574383,
86.0301279815319,86.1305645930366,86.2308839154025,86.3311390854579,86.4313614524681,
86.5315823245069,86.6319034407652,86.7322727209291,86.8328254727723,86.9287263197341,
87.0293087438279,87.1297453553328,87.2300646776988,87.3303198477544,87.4305422147649,
87.5307630868038,87.6310842030623,87.7314534832264,87.8320062350697,87.9279070820299,
88.0284895061235,88.1289261176283,88.2292454399941,88.3295006100496,88.4297229770599,
88.5299438490986,88.6302649653569,88.7306342455209,88.8311869973641,88.9270878443257,
89.0557759980376),.UNSPECIFIED.);
#1215=B_SPLINE_CURVE_WITH_KNOTS('',3,(#30426,#30427,#30428,#30429,#30430,
#30431,#30432,#30433,#30434,#30435,#30436,#30437,#30438,#30439,#30440,#30441,
#30442,#30443,#30444,#30445,#30446,#30447,#30448,#30449,#30450,#30451,#30452,
#30453,#30454,#30455,#30456,#30457,#30458,#30459,#30460,#30461,#30462,#30463,
#30464,#30465,#30466,#30467,#30468,#30469,#30470,#30471,#30472,#30473,#30474,
#30475,#30476,#30477,#30478,#30479,#30480,#30481,#30482,#30483,#30484,#30485,
#30486,#30487,#30488,#30489,#30490,#30491,#30492,#30493,#30494,#30495,#30496,
#30497,#30498,#30499,#30500,#30501,#30502,#30503,#30504,#30505,#30506,#30507,
#30508,#30509,#30510,#30511,#30512,#30513,#30514,#30515,#30516,#30517,#30518,
#30519,#30520,#30521,#30522,#30523,#30524,#30525,#30526,#30527,#30528,#30529,
#30530,#30531,#30532,#30533,#30534,#30535,#30536,#30537,#30538,#30539,#30540,
#30541,#30542,#30543,#30544,#30545,#30546,#30547,#30548,#30549,#30550,#30551,
#30552,#30553,#30554,#30555,#30556,#30557,#30558,#30559,#30560,#30561,#30562,
#30563,#30564,#30565,#30566,#30567,#30568,#30569,#30570,#30571,#30572,#30573,
#30574,#30575,#30576,#30577,#30578,#30579,#30580,#30581,#30582,#30583,#30584,
#30585,#30586,#30587,#30588,#30589,#30590,#30591,#30592,#30593,#30594,#30595,
#30596,#30597,#30598,#30599,#30600,#30601,#30602,#30603,#30604,#30605,#30606,
#30607,#30608,#30609,#30610,#30611,#30612,#30613,#30614,#30615),
 .UNSPECIFIED.,.F.,.F.,(4,3,3,3,3,3,3,3,3,3,3,3,3,3,3,3,3,3,3,3,3,3,3,3,
3,3,3,3,3,3,3,3,3,3,3,3,3,3,3,3,3,3,3,3,3,3,3,3,3,3,3,3,3,3,3,3,3,3,3,3,
3,3,3,4),(89.0557759982561,89.1548478356137,89.2537870669335,89.3526536190256,
89.4514804608427,89.550300507013,89.6492130022719,89.7481719107378,89.8473039942485,
89.9262686066214,90.0268510307156,90.1272876422209,90.2276069645874,90.3278621346434,
90.4280845016543,90.5283053736936,90.6286264899526,90.7289957701171,90.8295485219609,
90.9254493689172,91.0260317930103,91.1264684045144,91.2267877268798,91.3270428969347,
91.4272652639444,91.5274861359828,91.6278072522406,91.728176532404,91.8287292842468,
91.924630131213,92.0252125553059,92.1256491668097,92.2259684891748,92.3262236592295,
92.426446026239,92.5266668982769,92.6269880145345,92.7273572946976,92.82791004654,
92.9238108935088,93.0243933176066,93.1248299291159,93.2251492514859,93.3254044215455,
93.42562678856,93.525847660603,93.6261687768654,93.7265380570335,93.8270908088807,
93.9229916558046,94.0235740798929,94.1240106913923,94.2243300137529,94.324585183803,
94.4248075508081,94.5250284228413,94.6253495390945,94.7257188192534,94.8262715710917,
94.9221724181004,95.0326493234279,95.1428149119553,95.2524554430212,95.3389613048398),
 .UNSPECIFIED.);
#1216=B_SPLINE_CURVE_WITH_KNOTS('',3,(#30617,#30618,#30619,#30620,#30621,
#30622,#30623,#30624,#30625,#30626,#30627,#30628,#30629,#30630,#30631,#30632,
#30633,#30634,#30635,#30636,#30637,#30638,#30639,#30640,#30641,#30642,#30643,
#30644,#30645,#30646,#30647,#30648,#30649,#30650,#30651,#30652,#30653,#30654,
#30655,#30656,#30657,#30658,#30659,#30660,#30661,#30662,#30663,#30664,#30665,
#30666,#30667,#30668,#30669,#30670,#30671,#30672,#30673,#30674,#30675,#30676,
#30677,#30678,#30679,#30680,#30681,#30682,#30683,#30684,#30685,#30686,#30687,
#30688,#30689,#30690,#30691,#30692,#30693,#30694,#30695,#30696,#30697,#30698,
#30699,#30700,#30701,#30702,#30703,#30704,#30705,#30706,#30707,#30708,#30709,
#30710,#30711,#30712,#30713,#30714,#30715,#30716,#30717,#30718,#30719,#30720,
#30721,#30722,#30723,#30724,#30725,#30726,#30727,#30728,#30729,#30730,#30731,
#30732,#30733,#30734,#30735,#30736,#30737,#30738,#30739,#30740,#30741,#30742,
#30743,#30744,#30745,#30746,#30747,#30748,#30749,#30750,#30751,#30752,#30753,
#30754,#30755,#30756,#30757,#30758,#30759,#30760,#30761,#30762,#30763,#30764,
#30765,#30766,#30767,#30768,#30769,#30770,#30771,#30772,#30773,#30774,#30775,
#30776,#30777,#30778,#30779,#30780,#30781,#30782,#30783,#30784,#30785,#30786,
#30787,#30788,#30789,#30790,#30791,#30792,#30793,#30794,#30795,#30796,#30797,
#30798,#30799,#30800,#30801,#30802,#30803,#30804,#30805,#30806),
 .UNSPECIFIED.,.F.,.F.,(4,3,3,3,3,3,3,3,3,3,3,3,3,3,3,3,3,3,3,3,3,3,3,3,
3,3,3,3,3,3,3,3,3,3,3,3,3,3,3,3,3,3,3,3,3,3,3,3,3,3,3,3,3,3,3,3,3,3,3,3,
3,3,3,4),(95.3389613052171,95.4409974933841,95.5430847052396,95.6453339618529,
95.7476693299862,95.8502180918647,95.9213531803962,96.0219356045212,96.1223722160572,
96.2226915384546,96.3229467085413,96.4231690755829,96.5233899476529,96.6237110639422,
96.7240803441367,96.8246330960099,96.920533942692,97.0211163667362,97.1215529781915,
97.2218723005085,97.3221274705153,97.4223498374773,97.5225707094681,97.6228918256795,
97.723261105797,97.823813857595,97.9197147049878,98.0202971290644,98.1207337405514,
98.2210530628988,98.3213082329353,98.4215305999262,98.521751471945,98.6220725881831,
98.7224418683265,98.8229946201489,98.9188954672836,99.0194778916097,99.1199145033476,
99.2202338259468,99.3204889962355,99.4207113634785,99.5209322357496,99.6212533522374,
99.7216226326296,99.8221753846965,99.9180762295794,100.018658653241,100.119095264314,
100.219414586251,100.31966975588,100.419892122466,100.520112994084,100.62043410993,
100.720803389684,100.821356141129,100.917256991875,101.017146774421,101.116900249328,
101.216549802348,101.31794900486,101.417504245207,101.519825428802,101.622146612397),
 .UNSPECIFIED.);
#1217=B_SPLINE_CURVE_WITH_KNOTS('',3,(#30808,#30809,#30810,#30811,#30812,
#30813,#30814,#30815,#30816,#30817,#30818,#30819,#30820,#30821,#30822,#30823,
#30824,#30825,#30826,#30827,#30828,#30829,#30830,#30831,#30832,#30833,#30834,
#30835,#30836,#30837,#30838,#30839,#30840,#30841,#30842,#30843,#30844,#30845,
#30846,#30847,#30848,#30849,#30850,#30851,#30852,#30853,#30854,#30855,#30856,
#30857,#30858,#30859,#30860,#30861,#30862,#30863,#30864,#30865,#30866,#30867,
#30868,#30869,#30870,#30871,#30872,#30873,#30874,#30875,#30876,#30877,#30878,
#30879,#30880,#30881,#30882,#30883,#30884,#30885,#30886,#30887,#30888,#30889,
#30890,#30891,#30892,#30893,#30894,#30895,#30896,#30897,#30898,#30899,#30900,
#30901,#30902,#30903,#30904,#30905,#30906,#30907,#30908,#30909,#30910,#30911,
#30912,#30913,#30914,#30915,#30916,#30917,#30918,#30919,#30920,#30921,#30922,
#30923,#30924,#30925,#30926,#30927,#30928,#30929,#30930,#30931,#30932,#30933,
#30934,#30935,#30936,#30937,#30938,#30939,#30940,#30941,#30942,#30943,#30944,
#30945,#30946,#30947,#30948,#30949,#30950,#30951,#30952,#30953,#30954,#30955,
#30956,#30957,#30958,#30959,#30960,#30961,#30962,#30963,#30964,#30965,#30966,
#30967,#30968,#30969,#30970,#30971,#30972,#30973,#30974,#30975,#30976,#30977,
#30978,#30979,#30980,#30981,#30982,#30983,#30984,#30985,#30986,#30987,#30988,
#30989,#30990,#30991,#30992,#30993,#30994,#30995,#30996,#30997),
 .UNSPECIFIED.,.F.,.F.,(4,3,3,3,3,3,3,3,3,3,3,3,3,3,3,3,3,3,3,3,3,3,3,3,
3,3,3,3,3,3,3,3,3,3,3,3,3,3,3,3,3,3,3,3,3,3,3,3,3,3,3,3,3,3,3,3,3,3,3,3,
3,3,3,4),(101.622146612713,101.743648563498,101.866952969244,101.916437754171,
102.017020179948,102.117456793143,102.217776117202,102.318031288951,102.418253657653,
102.51847453138,102.618795649309,102.719164931136,102.819717684611,102.915618516467,
103.016200936897,103.11663754474,103.216956863466,103.317212029896,103.417434393299,
103.517655261755,103.617976374493,103.718345651164,103.818898399605,103.914799278763,
104.015381704087,104.115818316789,104.216137640298,104.316392811462,104.416615179546,
104.516836052622,104.617157169854,104.717526450959,104.818079203675,104.913980041058,
105.01456247698,105.114999100375,105.215318434665,105.315573616661,105.415795995612,
105.516016879574,105.616338007647,105.716707299584,105.817260062992,105.913160803354,
106.013743197147,106.114179778353,106.214499070561,106.314754210557,106.414976547646,
106.515197389943,106.615518476947,106.715887728074,106.816440451595,106.91234156565,
107.012812979089,107.113138663605,107.213347435279,107.313492448411,107.413605205227,
107.51371716713,107.61392945356,107.714190827401,107.81463362687,107.905331919362),
 .UNSPECIFIED.);
#1218=B_SPLINE_CURVE_WITH_KNOTS('',3,(#30999,#31000,#31001,#31002,#31003,
#31004,#31005,#31006,#31007,#31008,#31009,#31010,#31011,#31012,#31013,#31014,
#31015,#31016,#31017,#31018,#31019,#31020,#31021,#31022,#31023,#31024,#31025,
#31026,#31027,#31028,#31029,#31030,#31031,#31032,#31033,#31034,#31035,#31036,
#31037,#31038,#31039,#31040,#31041,#31042,#31043,#31044,#31045,#31046,#31047,
#31048,#31049,#31050,#31051,#31052,#31053,#31054,#31055,#31056,#31057,#31058,
#31059,#31060,#31061,#31062,#31063,#31064,#31065,#31066,#31067,#31068,#31069,
#31070,#31071,#31072,#31073,#31074,#31075,#31076,#31077,#31078,#31079,#31080,
#31081,#31082,#31083,#31084,#31085,#31086,#31087,#31088,#31089,#31090,#31091,
#31092,#31093,#31094,#31095,#31096,#31097,#31098,#31099,#31100,#31101,#31102,
#31103,#31104,#31105,#31106,#31107,#31108,#31109,#31110,#31111,#31112,#31113,
#31114,#31115,#31116,#31117,#31118,#31119,#31120,#31121,#31122,#31123,#31124,
#31125,#31126,#31127,#31128,#31129,#31130,#31131,#31132,#31133,#31134,#31135,
#31136,#31137,#31138,#31139,#31140,#31141,#31142,#31143,#31144,#31145,#31146,
#31147,#31148,#31149,#31150,#31151,#31152,#31153,#31154,#31155,#31156,#31157,
#31158,#31159,#31160,#31161,#31162,#31163,#31164,#31165,#31166,#31167,#31168,
#31169,#31170,#31171,#31172,#31173,#31174,#31175,#31176,#31177,#31178,#31179,
#31180,#31181,#31182,#31183,#31184,#31185,#31186,#31187,#31188,#31189,#31190,
#31191),.UNSPECIFIED.,.F.,.F.,(4,3,3,3,3,3,3,3,3,3,3,3,3,3,3,3,3,3,3,3,
3,3,3,3,3,3,3,3,3,3,3,3,3,3,3,3,3,3,3,3,3,3,3,3,3,3,3,3,3,3,3,3,3,3,3,3,
3,3,3,3,3,3,3,3,4),(107.905331919576,107.911522327946,108.012104832105,
108.11254152419,108.212860927529,108.313116178762,108.413338627042,108.51355958033,
108.613880777234,108.714250137846,108.814802968842,108.910703090242,109.011285269332,
109.111721635678,109.212040713789,109.312295640242,109.412517764625,109.51273839534,
109.613059274002,109.713428318213,109.813980839695,109.909883852537,110.010466487225,
110.110903307623,110.211222835385,110.311478208629,110.411700776365,110.511921846407,
110.612243155036,110.712612624817,110.813165559368,110.909064614833,111.009647553955,
111.110084684757,111.210404530373,111.310660225851,111.410883119722,111.51110451933,
111.61142616054,111.711795965091,111.812349234085,111.908245377129,112.008825861756,
112.109260531332,112.209577917086,112.309831154579,112.410051595662,112.510270551,
112.610589778432,112.710957181861,112.811508099817,112.907426139425,113.008010700115,
113.10844943665,113.20877085699,113.309028107726,113.409252535454,113.509475445561,
113.609798550258,113.71016979507,113.810724447976,113.906606901721,114.032061637831,
114.155474775546,114.188517226495),.UNSPECIFIED.);
#1219=B_SPLINE_CURVE_WITH_KNOTS('',3,(#31193,#31194,#31195,#31196,#31197,
#31198,#31199,#31200,#31201,#31202,#31203,#31204,#31205,#31206,#31207,#31208,
#31209,#31210,#31211,#31212,#31213,#31214,#31215,#31216,#31217,#31218,#31219,
#31220,#31221,#31222,#31223,#31224,#31225,#31226,#31227,#31228,#31229,#31230,
#31231,#31232,#31233,#31234,#31235,#31236,#31237,#31238,#31239,#31240,#31241,
#31242,#31243,#31244,#31245,#31246,#31247,#31248,#31249,#31250,#31251,#31252,
#31253,#31254,#31255,#31256,#31257,#31258,#31259,#31260,#31261,#31262,#31263,
#31264,#31265,#31266,#31267,#31268,#31269,#31270,#31271,#31272,#31273,#31274,
#31275,#31276,#31277,#31278,#31279,#31280,#31281,#31282,#31283,#31284,#31285,
#31286,#31287,#31288,#31289,#31290,#31291,#31292,#31293,#31294,#31295,#31296,
#31297,#31298,#31299,#31300,#31301,#31302,#31303,#31304,#31305,#31306,#31307,
#31308,#31309,#31310,#31311,#31312,#31313,#31314,#31315,#31316,#31317,#31318,
#31319,#31320,#31321,#31322,#31323,#31324,#31325,#31326,#31327,#31328,#31329,
#31330,#31331,#31332,#31333,#31334,#31335,#31336,#31337,#31338,#31339,#31340,
#31341,#31342,#31343,#31344,#31345,#31346,#31347,#31348,#31349,#31350,#31351,
#31352,#31353,#31354,#31355,#31356,#31357,#31358,#31359,#31360,#31361,#31362,
#31363,#31364,#31365,#31366,#31367,#31368,#31369,#31370,#31371,#31372,#31373,
#31374,#31375,#31376,#31377,#31378,#31379,#31380,#31381,#31382,#31383,#31384,
#31385),.UNSPECIFIED.,.F.,.F.,(4,3,3,3,3,3,3,3,3,3,3,3,3,3,3,3,3,3,3,3,
3,3,3,3,3,3,3,3,3,3,3,3,3,3,3,3,3,3,3,3,3,3,3,3,3,3,3,3,3,3,3,3,3,3,3,3,
3,3,3,3,3,3,3,3,4),(114.188517226756,114.287978532167,114.387393774356,
114.486795269358,114.586215309855,114.685747211439,114.785347086434,114.885107888347,
114.905787664016,115.006355055542,115.106776605851,115.207080893984,115.307321052522,
115.407528450849,115.507734417188,115.60804083083,115.708395494866,115.808933951395,
115.904968426312,116.005571080338,116.10602784679,116.20636711905,116.306642106101,
116.406884131427,116.507124477183,116.607464642396,116.707852771135,116.80842380852,
116.904149188608,117.004747547077,117.105200368142,117.205536234604,117.305808144354,
117.406047422113,117.506285351591,117.606623633199,117.70701016571,117.807580109372,
117.903329950904,118.003798493702,118.104120937105,118.204326186812,118.30446738779,
118.404576040251,118.504683603356,118.604892837216,118.705150825343,118.805594615079,
118.902510713199,119.003276219575,119.103895455646,119.204395862128,119.304831096984,
119.405232267188,119.505630437432,119.606125250882,119.706666540895,119.807386410131,
119.901691475495,120.004328434329,120.106799487655,120.209100979967,120.311302855602,
120.413424519418,120.471702533936),.UNSPECIFIED.);
#1220=B_SPLINE_CURVE_WITH_KNOTS('',3,(#31387,#31388,#31389,#31390,#31391,
#31392,#31393,#31394,#31395,#31396,#31397,#31398,#31399,#31400,#31401,#31402),
 .UNSPECIFIED.,.F.,.F.,(4,3,3,3,3,4),(120.471702534265,120.581378567869,
120.691378633643,120.801880018795,120.900872237791,120.914211738165),
 .UNSPECIFIED.);
#1221=B_SPLINE_CURVE_WITH_KNOTS('',3,(#31408,#31409,#31410,#31411,#31412,
#31413,#31414,#31415,#31416),.UNSPECIFIED.,.F.,.F.,(4,1,1,1,1,1,4),(-122.899233762383,
-121.900053000087,-120.900872237791,-119.901691475495,-118.9025107132,-117.903329950904,
-117.132769022939),.UNSPECIFIED.);
#1222=B_SPLINE_CURVE_WITH_KNOTS('',3,(#31418,#31419,#31420,#31421,#31422,
#31423,#31424,#31425,#31426,#31427,#31428,#31429,#31430,#31431,#31432,#31433,
#31434,#31435,#31436,#31437,#31438,#31439,#31440,#31441,#31442,#31443,#31444,
#31445,#31446,#31447,#31448,#31449,#31450,#31451,#31452,#31453,#31454,#31455,
#31456,#31457,#31458,#31459,#31460,#31461,#31462,#31463,#31464,#31465,#31466,
#31467,#31468,#31469,#31470,#31471,#31472,#31473,#31474,#31475,#31476,#31477,
#31478,#31479,#31480,#31481,#31482,#31483,#31484,#31485,#31486,#31487,#31488,
#31489,#31490,#31491,#31492,#31493,#31494,#31495,#31496,#31497,#31498,#31499,
#31500,#31501,#31502,#31503,#31504,#31505,#31506,#31507,#31508,#31509,#31510,
#31511,#31512,#31513,#31514,#31515,#31516,#31517,#31518,#31519,#31520,#31521,
#31522,#31523,#31524,#31525,#31526,#31527,#31528,#31529,#31530,#31531,#31532,
#31533,#31534,#31535,#31536,#31537,#31538,#31539,#31540,#31541,#31542,#31543,
#31544,#31545,#31546,#31547,#31548,#31549,#31550,#31551,#31552,#31553,#31554,
#31555,#31556,#31557,#31558,#31559,#31560,#31561,#31562,#31563,#31564,#31565,
#31566,#31567,#31568,#31569,#31570,#31571,#31572,#31573,#31574,#31575,#31576,
#31577,#31578,#31579,#31580,#31581,#31582,#31583,#31584,#31585,#31586,#31587,
#31588,#31589,#31590,#31591,#31592,#31593,#31594,#31595,#31596,#31597,#31598,
#31599,#31600,#31601,#31602,#31603,#31604,#31605,#31606,#31607),
 .UNSPECIFIED.,.F.,.F.,(4,3,3,3,3,3,3,3,3,3,3,3,3,3,3,3,3,3,3,3,3,3,3,3,
3,3,3,3,3,3,3,3,3,3,3,3,3,3,3,3,3,3,3,3,3,3,3,3,3,3,3,3,3,3,3,3,3,3,3,3,
3,3,3,4),(-117.132768509517,-116.99762221968,-116.904149188608,-116.803548664545,
-116.70309356908,-116.602755269422,-116.502480830314,-116.402238928977,
-116.30199828355,-116.20165715403,-116.101267696988,-116.000694727717,-115.904968426312,
-115.804400176277,-115.703977948936,-115.603673260019,-115.50343286865,
-115.403225405187,-115.303019541313,-115.20271349326,-115.102359338845,
-115.001821631126,-114.905787664016,-114.805202101569,-114.704762334078,
-114.604439844353,-114.504181501441,-114.40395596052,-114.303731917959,
-114.203407659086,-114.103035246359,-114.002479416692,-113.906606901721,
-113.806022597919,-113.705584063024,-113.605262760248,-113.505005575957,
-113.404781163642,-113.304558217948,-113.204234997641,-113.103863593401,
-113.003308708377,-112.907426139425,-112.806845532387,-112.70641076616,
-112.606093322967,-112.505840051877,-112.405619601004,-112.305400659671,
-112.205081483597,-112.104714151975,-112.004163339784,-111.908245377129,
-111.807662439649,-111.707225310445,-111.606905466351,-111.50664977235,
-111.406426879908,-111.306205481679,-111.20588384176,-111.105514038454,
-111.004960770612,-110.909064614833,-110.849583202338),.UNSPECIFIED.);
#1223=B_SPLINE_CURVE_WITH_KNOTS('',3,(#31609,#31610,#31611,#31612,#31613,
#31614,#31615,#31616,#31617,#31618,#31619,#31620,#31621,#31622,#31623,#31624,
#31625,#31626,#31627,#31628,#31629,#31630,#31631,#31632,#31633,#31634,#31635,
#31636,#31637,#31638,#31639,#31640,#31641,#31642,#31643,#31644,#31645,#31646,
#31647,#31648,#31649,#31650,#31651,#31652,#31653,#31654,#31655,#31656,#31657,
#31658,#31659,#31660,#31661,#31662,#31663,#31664,#31665,#31666,#31667,#31668,
#31669,#31670,#31671,#31672,#31673,#31674,#31675,#31676,#31677,#31678,#31679,
#31680,#31681,#31682,#31683,#31684,#31685,#31686,#31687,#31688,#31689,#31690,
#31691,#31692,#31693,#31694,#31695,#31696,#31697,#31698,#31699,#31700,#31701,
#31702,#31703,#31704,#31705,#31706,#31707,#31708,#31709,#31710,#31711,#31712,
#31713,#31714,#31715,#31716,#31717,#31718,#31719,#31720,#31721,#31722,#31723,
#31724,#31725,#31726,#31727,#31728,#31729,#31730,#31731,#31732,#31733,#31734,
#31735,#31736,#31737,#31738,#31739,#31740,#31741,#31742,#31743,#31744,#31745,
#31746,#31747,#31748,#31749,#31750,#31751,#31752,#31753,#31754,#31755,#31756,
#31757,#31758,#31759,#31760,#31761,#31762,#31763,#31764,#31765,#31766,#31767,
#31768,#31769,#31770,#31771,#31772,#31773,#31774,#31775,#31776,#31777,#31778,
#31779,#31780,#31781,#31782,#31783,#31784,#31785,#31786,#31787,#31788,#31789,
#31790,#31791,#31792,#31793,#31794,#31795,#31796,#31797,#31798),
 .UNSPECIFIED.,.F.,.F.,(4,3,3,3,3,3,3,3,3,3,3,3,3,3,3,3,3,3,3,3,3,3,3,3,
3,3,3,3,3,3,3,3,3,3,3,3,3,3,3,3,3,3,3,3,3,3,3,3,3,3,3,3,3,3,3,3,3,3,3,3,
3,3,3,4),(-110.849583201969,-110.749906777761,-110.65036988621,-110.550939824221,
-110.451566049954,-110.352216145972,-110.252857728841,-110.153395285142,
-110.053873649823,-109.954186934386,-109.909883852537,-109.80930165653,
-109.708865276814,-109.608546190731,-109.50829125959,-109.408069133795,
-109.307848504946,-109.207527633292,-109.107158598905,-109.006606091923,
-108.910703090242,-108.810120587652,-108.709683896851,-108.609364494357,
-108.509109243704,-108.408886795739,-108.308665842499,-108.208344645225,
-108.107975284014,-108.007422452036,-107.911522327946,-107.81093988886,
-107.710503261861,-107.610183923317,-107.509928736672,-107.409706352685,
-107.309485463304,-107.209164329244,-107.108795031,-107.008242260811,-106.91234156565,
-106.811759169579,-106.711322586572,-106.611003293288,-106.510748152655,
-106.41052581537,-106.310304973317,-106.209983887248,-106.109614637433,
-106.009061915852,-105.913160803354,-105.812578367802,-105.712141744707,
-105.611822410606,-105.511567228734,-105.411344849841,-105.31112396587,
-105.210802837685,-105.110433545577,-105.009880781905,-104.913980041058,
-104.797419643664,-104.681890702285,-104.566397895385),.UNSPECIFIED.);
#1224=B_SPLINE_CURVE_WITH_KNOTS('',3,(#31800,#31801,#31802,#31803,#31804,
#31805,#31806,#31807,#31808,#31809,#31810,#31811,#31812,#31813,#31814,#31815,
#31816,#31817,#31818,#31819,#31820,#31821,#31822,#31823,#31824,#31825,#31826,
#31827,#31828,#31829,#31830,#31831,#31832,#31833,#31834,#31835,#31836,#31837,
#31838,#31839,#31840,#31841,#31842,#31843,#31844,#31845,#31846,#31847,#31848,
#31849,#31850,#31851,#31852,#31853,#31854,#31855,#31856,#31857,#31858,#31859,
#31860,#31861,#31862,#31863,#31864,#31865,#31866,#31867,#31868,#31869,#31870,
#31871,#31872,#31873,#31874,#31875,#31876,#31877,#31878,#31879,#31880,#31881,
#31882,#31883,#31884,#31885,#31886,#31887,#31888,#31889,#31890,#31891,#31892,
#31893,#31894,#31895,#31896,#31897,#31898,#31899,#31900,#31901,#31902,#31903,
#31904,#31905,#31906,#31907,#31908,#31909,#31910,#31911,#31912,#31913,#31914,
#31915,#31916,#31917,#31918,#31919,#31920,#31921,#31922,#31923,#31924,#31925,
#31926,#31927,#31928,#31929,#31930,#31931,#31932,#31933,#31934,#31935,#31936,
#31937,#31938,#31939,#31940,#31941,#31942,#31943,#31944,#31945,#31946,#31947,
#31948,#31949,#31950,#31951,#31952,#31953,#31954,#31955,#31956,#31957,#31958,
#31959,#31960,#31961,#31962,#31963,#31964,#31965,#31966,#31967,#31968,#31969,
#31970,#31971,#31972,#31973,#31974,#31975,#31976,#31977,#31978,#31979,#31980,
#31981,#31982,#31983,#31984,#31985,#31986,#31987,#31988,#31989,#31990,#31991,
#31992),.UNSPECIFIED.,.F.,.F.,(4,3,3,3,3,3,3,3,3,3,3,3,3,3,3,3,3,3,3,3,
3,3,3,3,3,3,3,3,3,3,3,3,3,3,3,3,3,3,3,3,3,3,3,3,3,3,3,3,3,3,3,3,3,3,3,3,
3,3,3,3,3,3,3,3,4),(-104.566397895158,-104.465980669188,-104.365570501461,
-104.265136550864,-104.164578820184,-104.063951390142,-103.9631441112,-103.914799278763,
-103.814216858034,-103.713780249953,-103.613460931085,-103.513205764572,
-103.412983401142,-103.312762532717,-103.212441420101,-103.112072143601,
-103.011519395415,-102.915618516467,-102.815036090758,-102.714599477618,
-102.614280153594,-102.514024981867,-102.413802613174,-102.313581739445,
-102.213260621494,-102.112891339635,-102.01233858611,-101.916437754171,
-101.815855330105,-101.715418718623,-101.615099396275,-101.514844226233,
-101.414621859232,-101.314400987198,-101.214079870939,-101.113710590771,
-101.013157838918,-100.917256991875,-100.816674568175,-100.716237957071,
-100.615918635115,-100.515663465475,-100.415441098886,-100.315220227272,
-100.214899111442,-100.114529831709,-100.013977080297,-99.9180762295794,
-99.8174938052647,-99.7170571935358,-99.6167378709423,-99.5164827006572,
-99.4162603334156,-99.316039461144,-99.2157183446526,-99.1153490642547,
-99.0147963121794,-98.9188954672836,-98.8177509139559,-98.7167554082157,
-98.6158783757221,-98.5150934552823,-98.414361403763,-98.3136395349575,
-98.2832125879784),.UNSPECIFIED.);
#1225=B_SPLINE_CURVE_WITH_KNOTS('',3,(#31994,#31995,#31996,#31997,#31998,
#31999,#32000,#32001,#32002,#32003,#32004,#32005,#32006,#32007,#32008,#32009,
#32010,#32011,#32012,#32013,#32014,#32015,#32016,#32017,#32018,#32019,#32020,
#32021,#32022,#32023,#32024,#32025,#32026,#32027,#32028,#32029,#32030,#32031,
#32032,#32033,#32034,#32035,#32036,#32037,#32038,#32039,#32040,#32041,#32042,
#32043,#32044,#32045,#32046,#32047,#32048,#32049,#32050,#32051,#32052,#32053,
#32054,#32055,#32056,#32057,#32058,#32059,#32060,#32061,#32062,#32063,#32064,
#32065,#32066,#32067,#32068,#32069,#32070,#32071,#32072,#32073,#32074,#32075,
#32076,#32077,#32078,#32079,#32080,#32081,#32082,#32083,#32084,#32085,#32086,
#32087,#32088,#32089,#32090,#32091,#32092,#32093,#32094,#32095,#32096,#32097,
#32098,#32099,#32100,#32101,#32102,#32103,#32104,#32105,#32106,#32107,#32108,
#32109,#32110,#32111,#32112,#32113,#32114,#32115,#32116,#32117,#32118,#32119,
#32120,#32121,#32122,#32123,#32124,#32125,#32126,#32127,#32128,#32129,#32130,
#32131,#32132,#32133,#32134,#32135,#32136,#32137,#32138,#32139,#32140,#32141,
#32142,#32143,#32144,#32145,#32146,#32147,#32148,#32149,#32150,#32151,#32152,
#32153,#32154,#32155,#32156,#32157,#32158,#32159,#32160,#32161,#32162,#32163,
#32164,#32165,#32166,#32167,#32168,#32169,#32170,#32171,#32172,#32173,#32174,
#32175,#32176,#32177,#32178,#32179,#32180,#32181,#32182,#32183,#32184,#32185,
#32186),.UNSPECIFIED.,.F.,.F.,(4,3,3,3,3,3,3,3,3,3,3,3,3,3,3,3,3,3,3,3,
3,3,3,3,3,3,3,3,3,3,3,3,3,3,3,3,3,3,3,3,3,3,3,3,3,3,3,3,3,3,3,3,3,3,3,3,
3,3,3,3,3,3,3,3,4),(-98.2832125877455,-98.1694097971249,-98.0550264144753,
-97.9399742888503,-97.9197147049878,-97.8191322809388,-97.7186956694796,
-97.6183763471603,-97.5181211771522,-97.4178988101899,-97.3176779381995,
-97.2173568219901,-97.1169875418754,-97.0164347900815,-96.920533942692,
-96.8199515185687,-96.719514907034,-96.6191955846376,-96.5189404145513,
-96.4187180475099,-96.3184971754399,-96.2181760591502,-96.1178067789548,
-96.0172540270803,-95.9213531803962,-95.8207707563073,-95.7203341448072,
-95.620014822446,-95.5197596523953,-95.4195372853897,-95.3193164133555,
-95.2189952971017,-95.1186260169423,-95.0180732651035,-94.9221724181004,
-94.8215899940116,-94.7211533825118,-94.620834060151,-94.5205788901007,
-94.4203565230957,-94.3201356510622,-94.2198145348092,-94.1194452546507,
-94.0188925028129,-93.9229916558047,-93.8224092317071,-93.7219726201984,
-93.6216532978285,-93.5213981277689,-93.4211757607546,-93.3209548887116,
-93.2206337724491,-93.1202644922809,-93.0197117404336,-92.9238108935089,
-92.8242800268147,-92.7212484335895,-92.6219796999193,-92.5227705795473,
-92.4235884764662,-92.3244008328193,-92.2251181263679,-92.1257782787119,
-92.0262884834329,-92.0000272810126),.UNSPECIFIED.);
#1226=B_SPLINE_CURVE_WITH_KNOTS('',3,(#32188,#32189,#32190,#32191,#32192,
#32193,#32194,#32195,#32196,#32197,#32198,#32199,#32200,#32201,#32202,#32203,
#32204,#32205,#32206,#32207,#32208,#32209,#32210,#32211,#32212,#32213,#32214,
#32215,#32216,#32217,#32218,#32219,#32220,#32221,#32222,#32223,#32224,#32225,
#32226,#32227,#32228,#32229,#32230,#32231,#32232,#32233,#32234,#32235,#32236,
#32237,#32238,#32239,#32240,#32241,#32242,#32243,#32244,#32245,#32246,#32247,
#32248,#32249,#32250,#32251,#32252,#32253,#32254,#32255,#32256,#32257,#32258,
#32259,#32260,#32261,#32262,#32263,#32264,#32265,#32266,#32267,#32268,#32269,
#32270,#32271,#32272,#32273,#32274,#32275,#32276,#32277,#32278,#32279,#32280,
#32281,#32282,#32283,#32284,#32285,#32286,#32287,#32288,#32289,#32290,#32291,
#32292,#32293,#32294,#32295,#32296,#32297,#32298,#32299,#32300,#32301,#32302,
#32303,#32304,#32305,#32306,#32307,#32308,#32309,#32310,#32311,#32312,#32313,
#32314,#32315,#32316,#32317,#32318,#32319,#32320,#32321,#32322,#32323,#32324,
#32325,#32326,#32327,#32328,#32329,#32330,#32331,#32332,#32333,#32334,#32335,
#32336,#32337,#32338,#32339,#32340,#32341,#32342,#32343,#32344,#32345,#32346,
#32347,#32348,#32349,#32350,#32351,#32352,#32353,#32354,#32355,#32356,#32357,
#32358,#32359,#32360,#32361,#32362,#32363,#32364,#32365,#32366,#32367,#32368,
#32369,#32370,#32371,#32372,#32373,#32374,#32375,#32376,#32377),
 .UNSPECIFIED.,.F.,.F.,(4,3,3,3,3,3,3,3,3,3,3,3,3,3,3,3,3,3,3,3,3,3,3,3,
3,3,3,3,3,3,3,3,3,3,3,3,3,3,3,3,3,3,3,3,3,3,3,3,3,3,3,3,3,3,3,3,3,3,3,3,
3,3,3,4),(-92.0000272807988,-91.9246301312131,-91.82404770712,-91.7236110956159,
-91.6232917732506,-91.5230366031958,-91.4228142361862,-91.3225933641481,
-91.2222722478904,-91.1219029677271,-91.0213502158846,-90.9254493689173,
-90.824866944823,-90.7244303333177,-90.6241110109511,-90.523855840895,-90.4236334738841,
-90.3234126018446,-90.2230914855856,-90.122722205421,-90.0221694535771,
-89.9262686066215,-89.825686182528,-89.7252495710234,-89.6249302486576,
-89.5246750786023,-89.4244527115922,-89.3242318395535,-89.2239107232953,
-89.1235414431315,-89.0229886912884,-88.9270878443257,-88.826505420232,
-88.7260688087273,-88.6257494863614,-88.5254943163059,-88.4252719492956,
-88.3250510772568,-88.2247299609984,-88.1243606808344,-88.0238079289912,
-87.9279070820299,-87.8273246579361,-87.7268880464313,-87.6265687240653,
-87.5263135540097,-87.4260911869993,-87.3258703149604,-87.2255491987019,
-87.1251799185378,-87.0246271666945,-86.9287263197341,-86.8281438956404,
-86.7277072841356,-86.6273879617697,-86.5271327917142,-86.426910424704,
-86.3266895526652,-86.2263684364068,-86.1259991562429,-86.0254464043996,
-85.9295455574383,-85.7895984276924,-85.7168419736192),.UNSPECIFIED.);
#1227=B_SPLINE_CURVE_WITH_KNOTS('',3,(#32379,#32380,#32381,#32382,#32383,
#32384,#32385,#32386,#32387,#32388,#32389,#32390,#32391,#32392,#32393,#32394,
#32395,#32396,#32397,#32398,#32399,#32400,#32401,#32402,#32403,#32404,#32405,
#32406,#32407,#32408,#32409,#32410,#32411,#32412,#32413,#32414,#32415,#32416,
#32417,#32418,#32419,#32420,#32421,#32422,#32423,#32424,#32425,#32426,#32427,
#32428,#32429,#32430,#32431,#32432,#32433,#32434,#32435,#32436,#32437,#32438,
#32439,#32440,#32441,#32442,#32443,#32444,#32445,#32446,#32447,#32448,#32449,
#32450,#32451,#32452,#32453,#32454,#32455,#32456,#32457,#32458,#32459,#32460,
#32461,#32462,#32463,#32464,#32465,#32466,#32467,#32468,#32469,#32470,#32471,
#32472,#32473,#32474,#32475,#32476,#32477,#32478,#32479,#32480,#32481,#32482,
#32483,#32484,#32485,#32486,#32487,#32488,#32489,#32490,#32491,#32492,#32493,
#32494,#32495,#32496,#32497,#32498,#32499,#32500,#32501,#32502,#32503,#32504,
#32505,#32506,#32507,#32508,#32509,#32510,#32511,#32512,#32513,#32514,#32515,
#32516,#32517,#32518,#32519,#32520,#32521,#32522,#32523,#32524,#32525,#32526,
#32527,#32528,#32529,#32530,#32531,#32532,#32533,#32534,#32535,#32536,#32537,
#32538,#32539,#32540,#32541,#32542,#32543,#32544,#32545,#32546,#32547,#32548,
#32549,#32550,#32551,#32552,#32553,#32554,#32555,#32556,#32557,#32558,#32559,
#32560,#32561,#32562,#32563,#32564,#32565,#32566,#32567,#32568),
 .UNSPECIFIED.,.F.,.F.,(4,3,3,3,3,3,3,3,3,3,3,3,3,3,3,3,3,3,3,3,3,3,3,3,
3,3,3,3,3,3,3,3,3,3,3,3,3,3,3,3,3,3,3,3,3,3,3,3,3,3,3,3,3,3,3,3,3,3,3,3,
3,3,3,4),(-85.7168419733983,-85.6178735192426,-85.5189824534746,-85.4201358121954,
-85.3213006913025,-85.2223761543513,-85.1234094807557,-85.0242647323262,
-84.9303647951425,-84.8297823710488,-84.7293457595441,-84.6290264371782,
-84.5287712671227,-84.4285489001124,-84.3283280280738,-84.2280069118154,
-84.1276376316514,-84.0270848798082,-83.9311840328467,-83.8306016087529,
-83.7301649972482,-83.6298456748821,-83.5295905048266,-83.4293681378162,
-83.3291472657775,-83.228826149519,-83.1284568693549,-83.0279041175116,
-82.9320032705509,-82.8314208464572,-82.7309842349524,-82.6306649125865,
-82.5304097425309,-82.4301873755207,-82.3299665034819,-82.2296453872236,
-82.1292761070595,-82.0287233552163,-81.9328225082551,-81.8322400841614,
-81.7318034726565,-81.6314841502906,-81.5312289802351,-81.4310066132246,
-81.3307857411861,-81.2304646249277,-81.1300953447638,-81.0295425929205,
-80.9336417459593,-80.8330593218657,-80.7326227103606,-80.6323033879947,
-80.5320482179393,-80.4318258509289,-80.3316049788899,-80.2312838626314,
-80.1309145824676,-80.0303618306243,-79.9344609836635,-79.8287563918983,
-79.7233516333537,-79.6181260623224,-79.5131294138356,-79.4336566664396),
 .UNSPECIFIED.);
#1228=B_SPLINE_CURVE_WITH_KNOTS('',3,(#32570,#32571,#32572,#32573,#32574,
#32575,#32576,#32577,#32578,#32579,#32580,#32581,#32582,#32583,#32584,#32585,
#32586,#32587,#32588,#32589,#32590,#32591,#32592,#32593,#32594,#32595,#32596,
#32597,#32598,#32599,#32600,#32601,#32602,#32603,#32604,#32605,#32606,#32607,
#32608,#32609,#32610,#32611,#32612,#32613,#32614,#32615,#32616,#32617,#32618,
#32619,#32620,#32621,#32622,#32623,#32624,#32625,#32626,#32627,#32628,#32629,
#32630,#32631,#32632,#32633,#32634,#32635,#32636,#32637,#32638,#32639,#32640,
#32641,#32642,#32643,#32644,#32645,#32646,#32647,#32648,#32649,#32650,#32651,
#32652,#32653,#32654,#32655,#32656,#32657,#32658,#32659,#32660,#32661,#32662,
#32663,#32664,#32665,#32666,#32667,#32668,#32669,#32670,#32671,#32672,#32673,
#32674,#32675,#32676,#32677,#32678,#32679,#32680,#32681,#32682,#32683,#32684,
#32685,#32686,#32687,#32688,#32689,#32690,#32691,#32692,#32693,#32694,#32695,
#32696,#32697,#32698,#32699,#32700,#32701,#32702,#32703,#32704,#32705,#32706,
#32707,#32708,#32709,#32710,#32711,#32712,#32713,#32714,#32715,#32716,#32717,
#32718,#32719,#32720,#32721,#32722,#32723,#32724,#32725,#32726,#32727,#32728,
#32729,#32730,#32731,#32732,#32733,#32734,#32735,#32736,#32737,#32738,#32739,
#32740,#32741,#32742,#32743,#32744,#32745,#32746,#32747,#32748,#32749,#32750,
#32751,#32752,#32753,#32754,#32755,#32756,#32757,#32758,#32759),
 .UNSPECIFIED.,.F.,.F.,(4,3,3,3,3,3,3,3,3,3,3,3,3,3,3,3,3,3,3,3,3,3,3,3,
3,3,3,3,3,3,3,3,3,3,3,3,3,3,3,3,3,3,3,3,3,3,3,3,3,3,3,3,3,3,3,3,3,3,3,3,
3,3,3,4),(-79.4336566660391,-79.32862297329,-79.223297972688,-79.1178224512306,
-79.0120566743491,-78.9352802213677,-78.834697797274,-78.7342611857693,
-78.6339418634034,-78.5336866933479,-78.4334643263377,-78.3332434542988,
-78.2329223380405,-78.1325530578765,-78.0320003060333,-77.936099459072,
-77.8355170349783,-77.7350804234736,-77.6347611011076,-77.5345059310521,
-77.4342835640418,-77.334062692003,-77.2337415757446,-77.1333722955806,
-77.0328195437373,-76.9369186967762,-76.8363362726825,-76.7358996611777,
-76.6355803388117,-76.5353251687562,-76.4351028017458,-76.334881929707,
-76.2345608134485,-76.1341915332845,-76.0336387814412,-75.9377379344804,
-75.8371555103867,-75.7367188988819,-75.636399576516,-75.5361444064605,
-75.4359220394502,-75.3357011674114,-75.235380051153,-75.1350107709891,
-75.0344580191458,-74.9385571721846,-74.8379747480909,-74.737538136586,
-74.6372188142201,-74.5369636441646,-74.4367412771542,-74.3365204051153,
-74.2361992888569,-74.1358300086929,-74.0352772568497,-73.9393764098888,
-73.8402435573838,-73.7412396430733,-73.6423315119675,-73.5434861373362,
-73.4446309224566,-73.3457775064429,-73.246816995228,-73.1504713595064),
 .UNSPECIFIED.);
#1229=B_SPLINE_CURVE_WITH_KNOTS('',3,(#32761,#32762,#32763,#32764,#32765,
#32766,#32767,#32768,#32769,#32770,#32771,#32772,#32773,#32774,#32775,#32776,
#32777,#32778,#32779,#32780,#32781,#32782,#32783,#32784,#32785,#32786,#32787,
#32788,#32789,#32790,#32791,#32792,#32793,#32794,#32795,#32796,#32797,#32798,
#32799,#32800,#32801,#32802,#32803,#32804,#32805,#32806,#32807,#32808,#32809,
#32810,#32811,#32812,#32813,#32814,#32815,#32816,#32817,#32818,#32819,#32820,
#32821,#32822,#32823,#32824,#32825,#32826,#32827,#32828,#32829,#32830,#32831,
#32832,#32833,#32834,#32835,#32836,#32837,#32838,#32839,#32840,#32841,#32842,
#32843,#32844,#32845,#32846,#32847,#32848,#32849,#32850,#32851,#32852,#32853,
#32854,#32855,#32856,#32857,#32858,#32859,#32860,#32861,#32862,#32863,#32864,
#32865,#32866,#32867,#32868,#32869,#32870,#32871,#32872,#32873,#32874,#32875,
#32876,#32877,#32878,#32879,#32880,#32881,#32882,#32883,#32884,#32885,#32886,
#32887,#32888,#32889,#32890,#32891,#32892,#32893,#32894,#32895,#32896,#32897,
#32898,#32899,#32900,#32901,#32902,#32903,#32904,#32905,#32906,#32907,#32908,
#32909,#32910,#32911,#32912,#32913,#32914,#32915,#32916,#32917,#32918,#32919,
#32920,#32921,#32922,#32923,#32924,#32925,#32926,#32927,#32928,#32929,#32930,
#32931,#32932,#32933,#32934,#32935,#32936,#32937,#32938,#32939,#32940,#32941,
#32942,#32943,#32944,#32945,#32946,#32947,#32948,#32949,#32950),
 .UNSPECIFIED.,.F.,.F.,(4,3,3,3,3,3,3,3,3,3,3,3,3,3,3,3,3,3,3,3,3,3,3,3,
3,3,3,3,3,3,3,3,3,3,3,3,3,3,3,3,3,3,3,3,3,3,3,3,3,3,3,3,3,3,3,3,3,3,3,3,
3,3,3,4),(-73.15047135926,-73.0097533718863,-72.940195647593,-72.8396132234992,
-72.7391766119943,-72.6388572896282,-72.5386021195726,-72.4383797525622,
-72.3381588805232,-72.2378377642647,-72.1374684841005,-72.0369157322571,
-71.9410148852972,-71.8404324612035,-71.7399958496988,-71.6396765273329,
-71.5394213572774,-71.4391989902671,-71.3389781182283,-71.2386570019699,
-71.138287721806,-71.0377349699627,-70.9418341230014,-70.8412516989077,
-70.7408150874029,-70.6404957650369,-70.5402405949815,-70.4400182279711,
-70.3397973559323,-70.2394762396739,-70.1391069595099,-70.0385542076666,
-69.9426533607056,-69.8420709366119,-69.7416343251071,-69.6413150027412,
-69.5410598326856,-69.4408374656753,-69.3406165936365,-69.2402954773781,
-69.1399261972141,-69.0393734453708,-68.9434725984098,-68.8428901743161,
-68.7424535628113,-68.6421342404454,-68.5418790703899,-68.4416567033796,
-68.3414358313408,-68.2411147150824,-68.1407454349183,-68.0401926830751,
-67.944291836114,-67.8437094120203,-67.7432728005156,-67.6429534781497,
-67.5426983080942,-67.4424759410838,-67.3422550690451,-67.2419339527867,
-67.1415646726227,-67.0410119207795,-66.9451110738182,-66.8672860520804),
 .UNSPECIFIED.);
#1230=B_SPLINE_CURVE_WITH_KNOTS('',3,(#32952,#32953,#32954,#32955,#32956,
#32957,#32958,#32959,#32960,#32961,#32962,#32963,#32964,#32965,#32966,#32967,
#32968,#32969,#32970,#32971,#32972,#32973,#32974,#32975,#32976,#32977,#32978,
#32979,#32980,#32981,#32982,#32983,#32984,#32985,#32986,#32987,#32988,#32989,
#32990,#32991,#32992,#32993,#32994,#32995,#32996,#32997,#32998,#32999,#33000,
#33001,#33002,#33003,#33004,#33005,#33006,#33007,#33008,#33009,#33010,#33011,
#33012,#33013,#33014,#33015,#33016,#33017,#33018,#33019,#33020,#33021,#33022,
#33023,#33024,#33025,#33026,#33027,#33028,#33029,#33030,#33031,#33032,#33033,
#33034,#33035,#33036,#33037,#33038,#33039,#33040,#33041,#33042,#33043,#33044,
#33045,#33046,#33047,#33048,#33049,#33050,#33051,#33052,#33053,#33054,#33055,
#33056,#33057,#33058,#33059,#33060,#33061,#33062,#33063,#33064,#33065,#33066,
#33067,#33068,#33069,#33070,#33071,#33072,#33073,#33074,#33075,#33076,#33077,
#33078,#33079,#33080,#33081,#33082,#33083,#33084,#33085,#33086,#33087,#33088,
#33089,#33090,#33091,#33092,#33093,#33094,#33095,#33096,#33097,#33098,#33099,
#33100,#33101,#33102,#33103,#33104,#33105,#33106,#33107,#33108,#33109,#33110,
#33111,#33112,#33113,#33114,#33115,#33116,#33117,#33118,#33119,#33120,#33121,
#33122,#33123,#33124,#33125,#33126,#33127,#33128,#33129,#33130,#33131,#33132,
#33133,#33134,#33135,#33136,#33137,#33138,#33139,#33140,#33141,#33142,#33143,
#33144),.UNSPECIFIED.,.F.,.F.,(4,3,3,3,3,3,3,3,3,3,3,3,3,3,3,3,3,3,3,3,
3,3,3,3,3,3,3,3,3,3,3,3,3,3,3,3,3,3,3,3,3,3,3,3,3,3,3,3,3,3,3,3,3,3,3,3,
3,3,3,3,3,3,3,3,4),(-66.8672860518669,-66.7678166672169,-66.6650808727551,
-66.5658511493962,-66.4666728636925,-66.3675134088591,-66.2683402071068,
-66.1690603763527,-66.0697162817546,-65.9702133876511,-65.9459303115224,
-65.8453478874287,-65.7449112759237,-65.6445919535578,-65.5443367835023,
-65.4441144164919,-65.3438935444529,-65.2435724281946,-65.1432031480306,
-65.0426503961873,-64.9467495492266,-64.8461671251329,-64.7457305136282,
-64.6454111912623,-64.5451560212068,-64.4449336541966,-64.3447127821579,
-64.2443916658995,-64.1440223857354,-64.0434696338922,-63.9475687869308,
-63.8469863628371,-63.7465497513326,-63.6462304289666,-63.5459752589111,
-63.4457528919008,-63.3455320198621,-63.2452109036037,-63.1448416234397,
-63.0442888715964,-62.948388024635,-62.8478056005413,-62.7473689890367,
-62.6470496666707,-62.5467944966153,-62.4465721296051,-62.3463512575662,
-62.2460301413079,-62.1456608611438,-62.0451081093007,-61.9492072623393,
-61.8486248382457,-61.7481882267407,-61.6478689043748,-61.5476137343193,
-61.4473913673091,-61.34717049527,-61.2468493790115,-61.1464800988477,-61.0459273470045,
-60.9500265000435,-60.8353267768354,-60.7211028297473,-60.607680245254,
-60.5841007451335),.UNSPECIFIED.);
#1231=B_SPLINE_CURVE_WITH_KNOTS('',3,(#33146,#33147,#33148,#33149,#33150,
#33151,#33152,#33153,#33154,#33155,#33156,#33157,#33158,#33159,#33160,#33161,
#33162,#33163,#33164,#33165,#33166,#33167,#33168,#33169,#33170,#33171,#33172,
#33173,#33174,#33175,#33176,#33177,#33178,#33179,#33180,#33181,#33182,#33183,
#33184,#33185,#33186,#33187,#33188,#33189,#33190,#33191,#33192,#33193,#33194,
#33195,#33196,#33197,#33198,#33199,#33200,#33201,#33202,#33203,#33204,#33205,
#33206,#33207,#33208,#33209,#33210,#33211,#33212,#33213,#33214,#33215,#33216,
#33217,#33218,#33219,#33220,#33221,#33222,#33223,#33224,#33225,#33226,#33227,
#33228,#33229,#33230,#33231,#33232,#33233,#33234,#33235,#33236,#33237,#33238,
#33239,#33240,#33241,#33242,#33243,#33244,#33245,#33246,#33247,#33248,#33249,
#33250,#33251,#33252,#33253,#33254,#33255,#33256,#33257,#33258,#33259,#33260,
#33261,#33262,#33263,#33264,#33265,#33266,#33267,#33268,#33269,#33270,#33271,
#33272,#33273,#33274,#33275,#33276,#33277,#33278,#33279,#33280,#33281,#33282,
#33283,#33284,#33285,#33286,#33287,#33288,#33289,#33290,#33291,#33292,#33293,
#33294,#33295,#33296,#33297,#33298,#33299,#33300,#33301,#33302,#33303,#33304,
#33305,#33306,#33307,#33308,#33309,#33310,#33311,#33312,#33313,#33314,#33315,
#33316,#33317,#33318,#33319,#33320,#33321,#33322,#33323,#33324,#33325,#33326,
#33327,#33328,#33329,#33330,#33331,#33332,#33333,#33334,#33335,#33336,#33337,
#33338),.UNSPECIFIED.,.F.,.F.,(4,3,3,3,3,3,3,3,3,3,3,3,3,3,3,3,3,3,3,3,
3,3,3,3,3,3,3,3,3,3,3,3,3,3,3,3,3,3,3,3,3,3,3,3,3,3,3,3,3,3,3,3,3,3,3,3,
3,3,3,3,3,3,3,3,4),(-60.5841007449008,-60.4833190396952,-60.3825311205423,
-60.2817068382764,-60.1807479736463,-60.0797095309897,-59.978493193977,
-59.9508457377477,-59.850263313654,-59.749826702149,-59.649507379783,-59.5492522097275,
-59.4490298427171,-59.3488089706783,-59.2484878544198,-59.1481185742557,
-59.0475658224124,-58.9516649754519,-58.8510825513582,-58.7506459398535,
-58.6503266174876,-58.5500714474321,-58.4498490804218,-58.3496282083831,
-58.2493070921247,-58.1489378119608,-58.0483850601176,-57.9524842131561,
-57.8519017890623,-57.7514651775573,-57.6511458551914,-57.5508906851359,
-57.4506683181256,-57.3504474460868,-57.2501263298283,-57.1497570496644,
-57.0492042978211,-56.9533034508603,-56.8527210267666,-56.7522844152619,
-56.651965092896,-56.5517099228405,-56.4514875558302,-56.3512666837915,
-56.2509455675331,-56.1505762873691,-56.0500235355259,-55.9541226885645,
-55.8535402644708,-55.7531036529662,-55.6527843306003,-55.5525291605447,
-55.4523067935341,-55.3520859214954,-55.251764805237,-55.1513955250728,
-55.0508427732296,-54.9549419262687,-54.8541907418917,-54.7535843979548,
-54.6530916721567,-54.5526803013764,-54.4523167667248,-54.3519481085295,
-54.3009154377212),.UNSPECIFIED.);
#1232=B_SPLINE_CURVE_WITH_KNOTS('',3,(#33340,#33341,#33342,#33343,#33344,
#33345,#33346,#33347,#33348,#33349,#33350,#33351,#33352,#33353,#33354,#33355,
#33356,#33357,#33358,#33359,#33360,#33361,#33362,#33363,#33364,#33365,#33366,
#33367,#33368,#33369,#33370,#33371,#33372,#33373,#33374,#33375,#33376,#33377,
#33378,#33379,#33380,#33381,#33382,#33383,#33384,#33385,#33386,#33387,#33388,
#33389,#33390,#33391,#33392,#33393,#33394,#33395,#33396,#33397,#33398,#33399,
#33400,#33401,#33402,#33403,#33404,#33405,#33406,#33407,#33408,#33409,#33410,
#33411,#33412,#33413,#33414,#33415,#33416,#33417,#33418,#33419,#33420,#33421,
#33422,#33423,#33424,#33425,#33426,#33427,#33428,#33429,#33430,#33431,#33432,
#33433,#33434,#33435,#33436,#33437,#33438,#33439,#33440,#33441,#33442,#33443,
#33444,#33445,#33446,#33447,#33448,#33449,#33450,#33451,#33452,#33453,#33454,
#33455,#33456,#33457,#33458,#33459,#33460,#33461,#33462,#33463,#33464,#33465,
#33466,#33467,#33468,#33469,#33470,#33471,#33472,#33473,#33474,#33475,#33476,
#33477,#33478,#33479,#33480,#33481,#33482,#33483,#33484,#33485,#33486,#33487,
#33488,#33489,#33490,#33491,#33492,#33493,#33494,#33495,#33496,#33497,#33498,
#33499,#33500,#33501,#33502,#33503,#33504,#33505,#33506,#33507,#33508,#33509,
#33510,#33511,#33512,#33513,#33514,#33515,#33516,#33517,#33518,#33519,#33520,
#33521,#33522,#33523,#33524,#33525,#33526,#33527,#33528,#33529),
 .UNSPECIFIED.,.F.,.F.,(4,3,3,3,3,3,3,3,3,3,3,3,3,3,3,3,3,3,3,3,3,3,3,3,
3,3,3,3,3,3,3,3,3,3,3,3,3,3,3,3,3,3,3,3,3,3,3,3,3,3,3,3,3,3,3,3,3,3,3,3,
3,3,3,4),(-54.3009154374959,-54.185380291694,-54.0687436090842,-53.9557611639729,
-53.855178739879,-53.754742128374,-53.654422806008,-53.5541676359524,-53.4539452689419,
-53.353724396903,-53.2534032806445,-53.1530340004804,-53.052481248637,-52.9565804016771,
-52.8559979775834,-52.7555613660786,-52.6552420437127,-52.5549868736572,
-52.454764506647,-52.3545436346082,-52.2542225183498,-52.1538532381859,
-52.0533004863427,-51.9573996393813,-51.8568172152876,-51.7563806037828,
-51.6560612814169,-51.5558061113614,-51.455583744351,-51.3553628723122,
-51.2550417560538,-51.1546724758898,-51.0541197240466,-50.9582188770855,
-50.8576364529918,-50.757199841487,-50.656880519121,-50.5566253490656,-50.4564029820552,
-50.3561821100164,-50.255860993758,-50.155491713594,-50.0549389617507,-49.9590381147897,
-49.858455690696,-49.7580190791912,-49.6576997568252,-49.5574445867697,
-49.4572222197594,-49.3570013477206,-49.2566802314622,-49.1563109512982,
-49.0557581994549,-48.9598573524939,-48.8601294116964,-48.7605464198726,
-48.6610783124346,-48.5616715488526,-48.4622937332782,-48.3629125092727,
-48.2634343733349,-48.1639015109284,-48.064208747103,-48.0177301309082),
 .UNSPECIFIED.);
#1233=B_SPLINE_CURVE_WITH_KNOTS('',3,(#33531,#33532,#33533,#33534,#33535,
#33536,#33537,#33538,#33539,#33540,#33541,#33542,#33543,#33544,#33545,#33546,
#33547,#33548,#33549,#33550,#33551,#33552,#33553,#33554,#33555,#33556,#33557,
#33558,#33559,#33560,#33561,#33562,#33563,#33564,#33565,#33566,#33567,#33568,
#33569,#33570,#33571,#33572,#33573,#33574,#33575,#33576,#33577,#33578,#33579,
#33580,#33581,#33582,#33583,#33584,#33585,#33586,#33587,#33588,#33589,#33590,
#33591,#33592,#33593,#33594,#33595,#33596,#33597,#33598,#33599,#33600,#33601,
#33602,#33603,#33604,#33605,#33606,#33607,#33608,#33609,#33610,#33611,#33612,
#33613,#33614,#33615,#33616,#33617,#33618,#33619,#33620,#33621,#33622,#33623,
#33624,#33625,#33626,#33627,#33628,#33629,#33630,#33631,#33632,#33633,#33634,
#33635,#33636,#33637,#33638,#33639,#33640,#33641,#33642,#33643,#33644,#33645,
#33646,#33647,#33648,#33649,#33650,#33651,#33652,#33653,#33654,#33655,#33656,
#33657,#33658,#33659,#33660,#33661,#33662,#33663,#33664,#33665,#33666,#33667,
#33668,#33669,#33670,#33671,#33672,#33673,#33674,#33675,#33676,#33677,#33678,
#33679,#33680,#33681,#33682,#33683,#33684,#33685,#33686,#33687,#33688,#33689,
#33690,#33691,#33692,#33693,#33694,#33695,#33696,#33697,#33698,#33699,#33700,
#33701,#33702,#33703,#33704,#33705,#33706,#33707,#33708,#33709,#33710,#33711,
#33712,#33713,#33714,#33715,#33716,#33717,#33718,#33719,#33720),
 .UNSPECIFIED.,.F.,.F.,(4,3,3,3,3,3,3,3,3,3,3,3,3,3,3,3,3,3,3,3,3,3,3,3,
3,3,3,3,3,3,3,3,3,3,3,3,3,3,3,3,3,3,3,3,3,3,3,3,3,3,3,3,3,3,3,3,3,3,3,3,
3,3,3,4),(-48.0177301305417,-47.9606765901981,-47.8600941661048,-47.7596575546004,
-47.6593382322349,-47.5590830621798,-47.45886069517,-47.3586398231315,-47.2583187068736,
-47.1579494267101,-47.0573966748673,-46.9614958279023,-46.8609134038085,
-46.7604767923035,-46.6601574699374,-46.5599022998818,-46.4596799328713,
-46.3594590608323,-46.2591379445738,-46.1587686644096,-46.0582159125662,
-45.9623150656065,-45.8617326415128,-45.761296030008,-45.660976707642,-45.5607215375865,
-45.4604991705762,-45.3602782985374,-45.2599571822789,-45.1595879021149,
-45.0590351502717,-44.9631343033107,-44.862551879217,-44.7621152677123,
-44.6617959453463,-44.5615407752909,-44.4613184082806,-44.3610975362418,
-44.2607764199834,-44.1604071398194,-44.0598543879762,-43.9639535410149,
-43.8633711169212,-43.7629345054164,-43.6626151830505,-43.562360012995,
-43.4621376459846,-43.3619167739458,-43.2615956576874,-43.1612263775234,
-43.0606736256801,-42.9647727787192,-42.8641903546255,-42.7637537431207,
-42.6634344207548,-42.5631792506994,-42.4629568836891,-42.3627360116502,
-42.2624148953918,-42.1620456152278,-42.0614928633846,-41.9655920164234,
-41.830834925829,-41.734544823362),.UNSPECIFIED.);
#1234=B_SPLINE_CURVE_WITH_KNOTS('',3,(#33722,#33723,#33724,#33725,#33726,
#33727,#33728,#33729,#33730,#33731,#33732,#33733,#33734,#33735,#33736,#33737,
#33738,#33739,#33740,#33741,#33742,#33743,#33744,#33745,#33746,#33747,#33748,
#33749,#33750,#33751,#33752,#33753,#33754,#33755,#33756,#33757,#33758,#33759,
#33760,#33761,#33762,#33763,#33764,#33765,#33766,#33767,#33768,#33769,#33770,
#33771,#33772,#33773,#33774,#33775,#33776,#33777,#33778,#33779,#33780,#33781,
#33782,#33783,#33784,#33785,#33786,#33787,#33788,#33789,#33790,#33791,#33792,
#33793,#33794,#33795,#33796,#33797,#33798,#33799,#33800,#33801,#33802,#33803,
#33804,#33805,#33806,#33807,#33808,#33809,#33810,#33811,#33812,#33813,#33814,
#33815,#33816,#33817,#33818,#33819,#33820,#33821,#33822,#33823,#33824,#33825,
#33826,#33827,#33828,#33829,#33830,#33831,#33832,#33833,#33834,#33835,#33836,
#33837,#33838,#33839,#33840,#33841,#33842,#33843,#33844,#33845,#33846,#33847,
#33848,#33849,#33850,#33851,#33852,#33853,#33854,#33855,#33856,#33857,#33858,
#33859,#33860,#33861,#33862,#33863,#33864,#33865,#33866,#33867,#33868,#33869,
#33870,#33871,#33872,#33873,#33874,#33875,#33876,#33877,#33878,#33879,#33880,
#33881,#33882,#33883,#33884,#33885,#33886,#33887,#33888,#33889,#33890,#33891,
#33892,#33893,#33894,#33895,#33896,#33897,#33898,#33899,#33900,#33901,#33902,
#33903,#33904,#33905,#33906,#33907,#33908,#33909,#33910,#33911),
 .UNSPECIFIED.,.F.,.F.,(4,3,3,3,3,3,3,3,3,3,3,3,3,3,3,3,3,3,3,3,3,3,3,3,
3,3,3,3,3,3,3,3,3,3,3,3,3,3,3,3,3,3,3,3,3,3,3,3,3,3,3,3,3,3,3,3,3,3,3,3,
3,3,3,4),(-41.7345448230988,-41.6354972405392,-41.536519530477,-41.4375788402514,
-41.3386423674142,-41.2396110473611,-41.1405312145927,-41.0412784805418,
-40.9664112541276,-40.8658288300339,-40.7653922185292,-40.6650728961633,
-40.5648177261078,-40.4645953590974,-40.3643744870585,-40.2640533708001,
-40.1636840906361,-40.0631313387928,-39.9672304918318,-39.8666480677381,
-39.7662114562332,-39.6658921338672,-39.5656369638116,-39.4654145968013,
-39.3651937247626,-39.2648726085041,-39.1645033283401,-39.0639505764968,
-38.968049729536,-38.8674673054423,-38.7670306939372,-38.6667113715712,
-38.5664562015157,-38.4662338345054,-38.3660129624668,-38.2656918462084,
-38.1653225660444,-38.0647698142011,-37.9688689672402,-37.8682865431464,
-37.7678499316415,-37.6675306092756,-37.56727543922,-37.4670530722098,-37.3668322001707,
-37.2665110839123,-37.1661418037483,-37.0655890519051,-36.9696882049444,
-36.8691057808506,-36.7686691693456,-36.6683498469797,-36.5680946769243,
-36.4678723099141,-36.3676514378752,-36.2673303216168,-36.1669610414528,
-36.0664082896095,-35.9705074426486,-35.8656270199032,-35.7610219707335,
-35.6565790613792,-35.5523314356879,-35.4513595161825),.UNSPECIFIED.);
#1235=B_SPLINE_CURVE_WITH_KNOTS('',3,(#33913,#33914,#33915,#33916,#33917,
#33918,#33919,#33920,#33921,#33922,#33923,#33924,#33925,#33926,#33927,#33928,
#33929,#33930,#33931,#33932,#33933,#33934,#33935,#33936,#33937,#33938,#33939,
#33940,#33941,#33942,#33943,#33944,#33945,#33946,#33947,#33948,#33949,#33950,
#33951,#33952,#33953,#33954,#33955,#33956,#33957,#33958,#33959,#33960,#33961,
#33962,#33963,#33964,#33965,#33966,#33967,#33968,#33969,#33970,#33971,#33972,
#33973,#33974,#33975,#33976,#33977,#33978,#33979,#33980,#33981,#33982,#33983,
#33984,#33985,#33986,#33987,#33988,#33989,#33990,#33991,#33992,#33993,#33994,
#33995,#33996,#33997,#33998,#33999,#34000,#34001,#34002,#34003,#34004,#34005,
#34006,#34007,#34008,#34009,#34010,#34011,#34012,#34013,#34014,#34015,#34016,
#34017,#34018,#34019,#34020,#34021,#34022,#34023,#34024,#34025,#34026,#34027,
#34028,#34029,#34030,#34031,#34032,#34033,#34034,#34035,#34036,#34037,#34038,
#34039,#34040,#34041,#34042,#34043,#34044,#34045,#34046,#34047,#34048,#34049,
#34050,#34051,#34052,#34053,#34054,#34055,#34056,#34057,#34058,#34059,#34060,
#34061,#34062,#34063,#34064,#34065,#34066,#34067,#34068,#34069,#34070,#34071,
#34072,#34073,#34074,#34075,#34076,#34077,#34078,#34079,#34080,#34081,#34082,
#34083,#34084,#34085,#34086,#34087,#34088,#34089,#34090,#34091,#34092,#34093,
#34094,#34095,#34096,#34097,#34098,#34099,#34100,#34101,#34102,#34103,#34104,
#34105),.UNSPECIFIED.,.F.,.F.,(4,3,3,3,3,3,3,3,3,3,3,3,3,3,3,3,3,3,3,3,
3,3,3,3,3,3,3,3,3,3,3,3,3,3,3,3,3,3,3,3,3,3,3,3,3,3,3,3,3,3,3,3,3,3,3,3,
3,3,3,3,3,3,3,3,4),(-35.4513595157648,-35.345485624045,-35.2392752592576,
-35.1328871370317,-35.0261959781545,-34.9713266803528,-34.8707442562593,
-34.7703076447547,-34.6699883223889,-34.5697331523335,-34.4695107853233,
-34.3692899132845,-34.2689687970262,-34.1685995168624,-34.0680467650193,
-33.972145918057,-33.8715634939634,-33.7711268824587,-33.6708075600929,
-33.5705523900376,-33.4703300230273,-33.3701091509886,-33.2697880347303,
-33.1694187545665,-33.0688660027233,-32.9729651557612,-32.8723827316669,
-32.7719461201616,-32.6716267977951,-32.5713716277391,-32.4711492607282,
-32.3709283886889,-32.2706072724299,-32.1702379922654,-32.0696852404216,
-31.9737843934654,-31.8732019693723,-31.7727653578681,-31.6724460355027,
-31.5721908654478,-31.471968498438,-31.3717476263997,-31.2714265101418,
-31.1710572299784,-31.0705044781357,-30.9746036311696,-30.8740212070767,
-30.7735845955729,-30.6732652732078,-30.5730101031532,-30.4727877361437,
-30.3725668641058,-30.2722457478483,-30.1718764676851,-30.0713237158428,
-29.9754228688738,-29.8745167864168,-29.7755770001772,-29.6767314645433,
-29.577947102431,-29.4755038791276,-29.3767031531877,-29.2778723689772,
-29.1789381542911,-29.1681742092176),.UNSPECIFIED.);
#1236=B_SPLINE_CURVE_WITH_KNOTS('',3,(#34107,#34108,#34109,#34110,#34111,
#34112,#34113,#34114,#34115,#34116,#34117,#34118,#34119,#34120,#34121,#34122,
#34123,#34124,#34125,#34126,#34127,#34128,#34129,#34130,#34131,#34132,#34133,
#34134,#34135,#34136,#34137,#34138,#34139,#34140,#34141,#34142,#34143,#34144,
#34145,#34146,#34147,#34148,#34149,#34150,#34151,#34152,#34153,#34154,#34155,
#34156,#34157,#34158,#34159,#34160,#34161,#34162,#34163,#34164,#34165,#34166,
#34167,#34168,#34169,#34170,#34171,#34172,#34173,#34174,#34175,#34176,#34177,
#34178,#34179,#34180,#34181,#34182,#34183,#34184,#34185,#34186,#34187,#34188,
#34189,#34190,#34191,#34192,#34193,#34194,#34195,#34196,#34197,#34198,#34199,
#34200,#34201,#34202,#34203,#34204,#34205,#34206,#34207,#34208,#34209,#34210,
#34211,#34212,#34213,#34214,#34215,#34216,#34217,#34218,#34219,#34220,#34221,
#34222,#34223,#34224,#34225,#34226,#34227,#34228,#34229,#34230,#34231,#34232,
#34233,#34234,#34235,#34236,#34237,#34238,#34239,#34240,#34241,#34242,#34243,
#34244,#34245,#34246,#34247,#34248,#34249,#34250,#34251,#34252,#34253,#34254,
#34255,#34256,#34257,#34258,#34259,#34260,#34261,#34262,#34263,#34264,#34265,
#34266,#34267,#34268,#34269,#34270,#34271,#34272,#34273,#34274,#34275,#34276,
#34277,#34278,#34279,#34280,#34281,#34282,#34283,#34284,#34285,#34286,#34287,
#34288,#34289,#34290,#34291,#34292,#34293,#34294,#34295,#34296),
 .UNSPECIFIED.,.F.,.F.,(4,3,3,3,3,3,3,3,3,3,3,3,3,3,3,3,3,3,3,3,3,3,3,3,
3,3,3,3,3,3,3,3,3,3,3,3,3,3,3,3,3,3,3,3,3,3,3,3,3,3,3,3,3,3,3,3,3,3,3,3,
3,3,3,4),(-29.1681742090029,-29.0208248230063,-28.976242106578,-28.8756596824898,
-28.7752230709906,-28.6749037486302,-28.5746485785802,-28.4744262115752,
-28.3742053395417,-28.2738842232886,-28.1735149431298,-28.0729621912916,
-27.9770613442822,-27.876478920193,-27.7760423086927,-27.6757229863314,
-27.5754678162805,-27.4752454492749,-27.3750245772408,-27.2747034609872,
-27.174334180828,-27.0737814289895,-26.9778805819864,-26.8772981578615,
-26.7768615463255,-26.6765422239283,-26.5762870538417,-26.4760646868002,
-26.3758438147304,-26.2755226984413,-26.1751534182469,-26.0746006663738,
-25.9786998196906,-25.8781173956462,-25.7776807841907,-25.6773614618735,
-25.5771062918666,-25.4768839249044,-25.3766630529134,-25.2763419367019,
-25.1759726565842,-25.0754199047861,-24.9795190573949,-24.8789366333182,
-24.778500021831,-24.6781806994834,-24.5779255294467,-24.4777031624557,
-24.3774822904366,-24.2771611741983,-24.1767918940548,-24.0762391422323,
-23.9803382950991,-23.8797558707739,-23.7793192590369,-23.6789999364387,
-23.578744766151,-23.4785223989088,-23.3783015266388,-23.277980410152,-23.1776111297607,
-23.0770583776947,-22.9811575328033,-22.8849889018233),.UNSPECIFIED.);
#1237=B_SPLINE_CURVE_WITH_KNOTS('',3,(#34298,#34299,#34300,#34301,#34302,
#34303,#34304,#34305,#34306,#34307,#34308,#34309,#34310,#34311,#34312,#34313,
#34314,#34315,#34316,#34317,#34318,#34319,#34320,#34321,#34322,#34323,#34324,
#34325,#34326,#34327,#34328,#34329,#34330,#34331,#34332,#34333,#34334,#34335,
#34336,#34337,#34338,#34339,#34340,#34341,#34342,#34343,#34344,#34345,#34346,
#34347,#34348,#34349,#34350,#34351,#34352,#34353,#34354,#34355,#34356,#34357,
#34358,#34359,#34360,#34361,#34362,#34363,#34364,#34365,#34366,#34367,#34368,
#34369,#34370,#34371,#34372,#34373,#34374,#34375,#34376,#34377,#34378,#34379,
#34380,#34381,#34382,#34383,#34384,#34385,#34386,#34387,#34388,#34389,#34390,
#34391,#34392,#34393,#34394,#34395,#34396,#34397,#34398,#34399,#34400,#34401,
#34402,#34403,#34404,#34405,#34406,#34407,#34408,#34409,#34410,#34411,#34412,
#34413,#34414,#34415,#34416,#34417,#34418,#34419,#34420,#34421,#34422,#34423,
#34424,#34425,#34426,#34427,#34428,#34429,#34430,#34431,#34432,#34433,#34434,
#34435,#34436,#34437,#34438,#34439,#34440,#34441,#34442,#34443,#34444,#34445,
#34446,#34447,#34448,#34449,#34450,#34451,#34452,#34453,#34454,#34455,#34456,
#34457,#34458,#34459,#34460,#34461,#34462,#34463,#34464,#34465,#34466,#34467,
#34468,#34469,#34470,#34471,#34472,#34473,#34474,#34475,#34476,#34477,#34478,
#34479,#34480,#34481,#34482,#34483,#34484,#34485,#34486,#34487),
 .UNSPECIFIED.,.F.,.F.,(4,3,3,3,3,3,3,3,3,3,3,3,3,3,3,3,3,3,3,3,3,3,3,3,
3,3,3,3,3,3,3,3,3,3,3,3,3,3,3,3,3,3,3,3,3,3,3,3,3,3,3,3,3,3,3,3,3,3,3,3,
3,3,3,4),(-22.8849889015957,-22.785692606535,-22.6852281270316,-22.5861595338316,
-22.4871388318715,-22.3881332689759,-22.2865941443588,-22.1874612031866,
-22.0847189868471,-21.9819767705075,-21.8813943464021,-21.7809577348901,
-21.6806384125236,-21.5803832424715,-21.4801608754687,-21.3799400034411,
-21.2796188872001,-21.1792496070569,-21.0786968552397,-20.9827960082117,
-20.8822135824413,-20.7817769692529,-20.6814576452008,-20.5812024734585,
-20.4809801047627,-20.3807592310424,-20.2804381131202,-20.1800688312996,
-20.0795160778312,-19.9836152459159,-19.883032825475,-19.7825962176206,
-19.6822768988838,-19.5820217324432,-19.4817993690288,-19.3815785005619,
-19.2812573878133,-19.1808881111309,-19.0803353626801,-18.9844344836201,
-18.8838520582959,-18.7834154455939,-18.6830961220852,-18.5828409509208,
-18.4826185828361,-18.3823977097594,-18.2820765925266,-18.1817073114211,
-18.0811545587033,-17.9852537213243,-17.8846712854417,-17.7842346620878,
-17.6839153278377,-17.5836601458819,-17.4834377669715,-17.3832168830492,
-17.2828957550165,-17.1825264631186,-17.0819736997497,-16.9860729590285,
-16.8730392479783,-16.7604081100515,-16.6484609984442,-16.6018035948693),
 .UNSPECIFIED.);
#1238=B_SPLINE_CURVE_WITH_KNOTS('',3,(#34489,#34490,#34491,#34492,#34493,
#34494,#34495,#34496,#34497,#34498,#34499,#34500,#34501,#34502,#34503,#34504,
#34505,#34506,#34507,#34508,#34509,#34510,#34511,#34512,#34513,#34514,#34515,
#34516,#34517,#34518,#34519,#34520,#34521,#34522,#34523,#34524,#34525,#34526,
#34527,#34528,#34529,#34530,#34531,#34532,#34533,#34534,#34535,#34536,#34537,
#34538,#34539,#34540,#34541,#34542,#34543,#34544,#34545,#34546,#34547,#34548,
#34549,#34550,#34551,#34552,#34553,#34554,#34555,#34556,#34557,#34558,#34559,
#34560,#34561,#34562,#34563,#34564,#34565,#34566,#34567,#34568,#34569,#34570,
#34571,#34572,#34573,#34574,#34575,#34576,#34577,#34578,#34579,#34580,#34581,
#34582,#34583,#34584,#34585,#34586,#34587,#34588,#34589,#34590,#34591,#34592,
#34593,#34594,#34595,#34596,#34597,#34598,#34599,#34600,#34601,#34602,#34603,
#34604,#34605,#34606,#34607,#34608,#34609,#34610,#34611,#34612,#34613,#34614,
#34615,#34616,#34617,#34618,#34619,#34620,#34621,#34622,#34623,#34624,#34625,
#34626,#34627,#34628,#34629,#34630,#34631,#34632,#34633,#34634,#34635,#34636,
#34637,#34638,#34639,#34640,#34641,#34642,#34643,#34644,#34645,#34646,#34647,
#34648,#34649,#34650,#34651,#34652,#34653,#34654,#34655,#34656,#34657,#34658,
#34659,#34660,#34661,#34662,#34663,#34664,#34665,#34666,#34667,#34668,#34669,
#34670,#34671,#34672,#34673,#34674,#34675,#34676,#34677,#34678),
 .UNSPECIFIED.,.F.,.F.,(4,3,3,3,3,3,3,3,3,3,3,3,3,3,3,3,3,3,3,3,3,3,3,3,
3,3,3,3,3,3,3,3,3,3,3,3,3,3,3,3,3,3,3,3,3,3,3,3,3,3,3,3,3,3,3,3,3,3,3,3,
3,3,3,4),(-16.6018035946437,-16.5006122134358,-16.3993999728341,-16.2962730288087,
-16.1948628929016,-16.0908775448171,-15.9868921967327,-15.8863097542278,
-15.785873124552,-15.6855537844569,-15.5852985969477,-15.4850762127801,
-15.384855323902,-15.2845341914182,-15.1841648953368,-15.0836121282851,
-14.9877114344369,-14.8871289305195,-14.7866922386777,-14.6863728355818,
-14.5861175845928,-14.4858951365572,-14.3856741835129,-14.2853529868507,
-14.184983626479,-14.0844307957194,-13.9885306721411,-13.8879484924996,
-13.7875121256017,-13.6871930469416,-13.5869381199415,-13.4867159950122,
-13.3864953637554,-13.2861744845588,-13.1858054398181,-13.0852529178185,
-12.9893499098453,-12.8887672754061,-12.7883304552521,-12.6880109277277,
-12.587755554717,-12.4875329872103,-12.387311917392,-12.2869906089774,-12.1866211394074,
-12.0860682050563,-11.9901691475495,-11.8895862098247,-11.7891490804281,
-11.6888292362236,-11.5885735421607,-11.4883506497053,-11.388129251512,
-11.287807611706,-11.187437808555,-11.0868845409385,-10.9909883852537,-10.8905873154232,
-10.790327535112,-10.6901773093172,-10.5900985337102,-10.4900634929034,
-10.3900077170264,-10.3186182874641),.UNSPECIFIED.);
#1239=B_SPLINE_CURVE_WITH_KNOTS('',3,(#34679,#34680,#34681,#34682,#34683,
#34684,#34685,#34686,#34687,#34688,#34689,#34690,#34691,#34692,#34693,#34694,
#34695,#34696,#34697,#34698,#34699,#34700,#34701,#34702,#34703,#34704,#34705,
#34706,#34707,#34708,#34709,#34710,#34711,#34712,#34713,#34714,#34715,#34716,
#34717,#34718,#34719,#34720,#34721,#34722,#34723,#34724,#34725,#34726,#34727,
#34728,#34729,#34730,#34731,#34732,#34733,#34734,#34735,#34736,#34737,#34738,
#34739,#34740,#34741,#34742,#34743,#34744,#34745,#34746,#34747,#34748,#34749,
#34750,#34751,#34752,#34753,#34754,#34755,#34756,#34757,#34758,#34759,#34760,
#34761,#34762,#34763,#34764,#34765,#34766,#34767,#34768,#34769,#34770,#34771,
#34772,#34773,#34774,#34775,#34776,#34777,#34778,#34779,#34780,#34781,#34782,
#34783,#34784,#34785,#34786,#34787,#34788,#34789,#34790,#34791,#34792,#34793,
#34794,#34795,#34796,#34797,#34798,#34799,#34800,#34801,#34802,#34803,#34804,
#34805,#34806,#34807,#34808,#34809,#34810,#34811,#34812,#34813,#34814,#34815,
#34816,#34817,#34818,#34819,#34820,#34821,#34822,#34823,#34824,#34825,#34826,
#34827,#34828,#34829,#34830,#34831,#34832,#34833,#34834,#34835,#34836,#34837,
#34838,#34839,#34840,#34841,#34842,#34843,#34844,#34845,#34846,#34847,#34848,
#34849,#34850,#34851,#34852,#34853,#34854,#34855,#34856,#34857,#34858,#34859,
#34860,#34861,#34862,#34863,#34864,#34865,#34866,#34867,#34868),
 .UNSPECIFIED.,.F.,.F.,(4,3,3,3,3,3,3,3,3,3,3,3,3,3,3,3,3,3,3,3,3,3,3,3,
3,3,3,3,3,3,3,3,3,3,3,3,3,3,3,3,3,3,3,3,3,3,3,3,3,3,3,3,3,3,3,3,3,3,3,3,
3,3,3,4),(-10.3186182870443,-10.2011545560181,-10.0823918979535,-9.99180762295794,
-9.89122306431455,-9.79078432980569,-9.6904629114498,-9.59020566267282,
-9.48998123687609,-9.38975832867021,-9.28943522581426,-9.18906398281329,
-9.08850933164576,-8.99262686066215,-8.8920413763641,-8.79160167008605,
-8.6912792158045,-8.59102089266657,-8.49079535587881,-8.39057130182047,
-8.29024700692928,-8.18987454475535,-8.08931864337274,-7.99344609836635,
-7.89287868600335,-7.79245711482735,-7.69215280587807,-7.59191262656223,
-7.49170520752304,-7.39149922056677,-7.29119278659681,-7.19083810235733,
-7.09029962607513,-6.99426533607056,-6.89366269493674,-6.79320594127186,
-6.69286668158642,-6.59259170697504,-6.49234969393895,-6.39210936030836,
-6.29176920688027,-6.19138108976055,-6.09081006357693,-5.99508457377476,
-5.89448625755712,-5.79403347902593,-5.69369765531915,-5.59342578844064,
-5.49318655361032,-5.3929486670598,-5.29261042807389,-5.19222393808779,
-5.0916540362804,-4.99590381147897,-4.896050224785,-4.79634212419318,-4.69674938914012,
-4.59721866292036,-4.49771769171307,-4.39821426140152,-4.29861090058313,
-4.19895407607732,-4.09912709998999,-4.0354329805645),.UNSPECIFIED.);
#1240=B_SPLINE_CURVE_WITH_KNOTS('',3,(#34871,#34872,#34873,#34874,#34875,
#34876,#34877,#34878,#34879,#34880,#34881,#34882,#34883,#34884,#34885,#34886,
#34887,#34888,#34889,#34890,#34891,#34892,#34893,#34894,#34895,#34896,#34897,
#34898,#34899,#34900,#34901,#34902,#34903,#34904,#34905,#34906,#34907,#34908,
#34909,#34910,#34911,#34912,#34913,#34914,#34915,#34916,#34917,#34918,#34919,
#34920),.UNSPECIFIED.,.F.,.F.,(4,2,2,2,2,2,2,2,2,2,2,2,2,2,2,2,2,2,2,2,
2,2,2,2,4),(-0.242412075418231,-0.24068258493173,-0.23876015295065,-0.23726279880318,
-0.235498379397621,-0.232535044312713,-0.217554658625273,-0.175019001490325,
-0.150773707812734,-0.145414945615575,-0.142318515927924,-0.139655388881361,
-0.136404372732187,-0.130628635693296,-0.10322634121326,-0.0796420139484518,
-0.0505808179684192,-0.0474274175871481,-0.0454937459518301,-0.0439922154119611,
-0.0422271644585061,-0.0403423932910817,-0.0373729963661339,-0.0315833569543321,
-0.000576332490211338),.UNSPECIFIED.);
#1241=B_SPLINE_CURVE_WITH_KNOTS('',3,(#34922,#34923,#34924,#34925,#34926,
#34927,#34928,#34929,#34930,#34931,#34932,#34933,#34934,#34935,#34936,#34937,
#34938,#34939,#34940,#34941,#34942,#34943,#34944,#34945,#34946,#34947,#34948,
#34949,#34950,#34951,#34952,#34953,#34954,#34955,#34956,#34957,#34958,#34959,
#34960,#34961,#34962,#34963,#34964,#34965,#34966,#34967,#34968,#34969,#34970,
#34971,#34972,#34973,#34974,#34975,#34976,#34977,#34978,#34979,#34980,#34981,
#34982,#34983,#34984,#34985,#34986,#34987,#34988,#34989,#34990,#34991,#34992,
#34993,#34994,#34995,#34996,#34997,#34998,#34999,#35000,#35001,#35002,#35003,
#35004,#35005,#35006,#35007,#35008,#35009,#35010,#35011,#35012,#35013,#35014,
#35015,#35016,#35017,#35018,#35019,#35020,#35021,#35022,#35023,#35024,#35025,
#35026,#35027,#35028,#35029,#35030,#35031,#35032,#35033,#35034,#35035,#35036,
#35037,#35038,#35039),.UNSPECIFIED.,.F.,.F.,(4,3,3,3,3,3,3,3,3,3,3,3,3,
3,3,3,3,3,3,3,3,3,3,3,3,3,3,3,3,3,3,3,3,3,3,3,3,3,3,4),(128.805298797457,
128.909530301967,129.013684715498,129.117800270842,129.221915141085,129.326134956294,
129.430415400967,129.534872675319,129.575860238568,129.681560904871,129.787100864418,
129.892515952901,129.997864692822,130.103183758175,130.208509778359,130.313950456587,
130.419455685508,130.525146421068,130.575041000864,130.681053929543,130.78690594986,
130.892631297518,130.998288997924,131.103915267213,131.20954627527,131.315286538609,
131.421088702291,131.527069210927,131.57422176316,131.680115426827,131.785850999542,
131.891464565972,131.997013443811,132.102533989557,132.208062516701,132.313705829073,
132.419414064884,132.525306211834,132.573402525455,132.586742025829),
 .UNSPECIFIED.);
#1242=B_SPLINE_CURVE_WITH_KNOTS('',3,(#35043,#35044,#35045,#35046,#35047,
#35048,#35049,#35050,#35051,#35052,#35053,#35054,#35055,#35056,#35057,#35058,
#35059,#35060,#35061,#35062,#35063,#35064,#35065,#35066,#35067,#35068,#35069,
#35070,#35071,#35072,#35073,#35074,#35075,#35076,#35077,#35078,#35079,#35080,
#35081,#35082,#35083,#35084,#35085,#35086,#35087,#35088,#35089,#35090,#35091,
#35092,#35093,#35094,#35095,#35096,#35097,#35098,#35099,#35100,#35101,#35102,
#35103,#35104,#35105,#35106,#35107,#35108,#35109,#35110,#35111,#35112,#35113,
#35114,#35115),.UNSPECIFIED.,.F.,.F.,(4,3,3,3,3,3,3,3,3,3,3,3,3,3,3,3,3,
3,3,3,3,3,3,3,4),(128.805298797453,128.920686329815,129.036431940841,129.152706586493,
129.234468501037,129.339286844061,129.443944512182,129.54848134576,129.652954615654,
129.757402129115,129.861861652104,129.966449229204,130.071107485331,130.175969886253,
130.233649263333,130.342332107421,130.453644347197,130.561962326317,130.670177107086,
130.778318699004,130.89194653066,131.000061984321,131.108188597098,131.216390672611,
131.232830025629),.UNSPECIFIED.);
#1243=B_SPLINE_CURVE_WITH_KNOTS('',3,(#35116,#35117,#35118,#35119,#35120,
#35121,#35122,#35123,#35124,#35125,#35126,#35127,#35128,#35129,#35130,#35131,
#35132,#35133,#35134,#35135,#35136,#35137,#35138,#35139,#35140,#35141,#35142,
#35143,#35144,#35145,#35146,#35147,#35148,#35149,#35150,#35151,#35152,#35153,
#35154,#35155,#35156,#35157,#35158,#35159,#35160,#35161,#35162,#35163,#35164,
#35165,#35166,#35167,#35168,#35169),.UNSPECIFIED.,.F.,.F.,(4,2,2,2,2,2,
2,2,2,2,2,2,2,2,2,2,2,2,2,2,2,2,2,2,2,2,4),(-2.43052060028278,-2.42452327733995,
-2.41980014231107,-2.41714485996155,-2.41455047789507,-2.4116171269049,
-2.40697072271808,-2.39259337102949,-2.34514218860885,-2.33228857955003,
-2.32712859312713,-2.3232333540881,-2.32131082001195,-2.31993325557163,
-2.31817269023445,-2.31507196203576,-2.30138252764729,-2.24861046291519,
-2.23777801862789,-2.2322815284433,-2.22882458265371,-2.22563133019317,
-2.22300679682425,-2.21991811223185,-2.21463391519929,-2.19212759162886,
-2.18849108915717),.UNSPECIFIED.);
#1244=B_SPLINE_CURVE_WITH_KNOTS('',3,(#35173,#35174,#35175,#35176,#35177,
#35178,#35179,#35180,#35181,#35182,#35183,#35184,#35185,#35186,#35187,#35188,
#35189,#35190,#35191,#35192,#35193,#35194,#35195,#35196,#35197,#35198,#35199,
#35200,#35201,#35202,#35203,#35204,#35205,#35206,#35207,#35208,#35209,#35210,
#35211,#35212,#35213,#35214,#35215,#35216,#35217,#35218,#35219,#35220,#35221,
#35222,#35223,#35224,#35225,#35226,#35227,#35228,#35229,#35230,#35231,#35232,
#35233,#35234,#35235,#35236,#35237,#35238,#35239,#35240,#35241,#35242,#35243,
#35244,#35245,#35246,#35247,#35248,#35249,#35250,#35251),.UNSPECIFIED.,
 .F.,.F.,(4,3,3,3,3,3,3,3,3,3,3,3,3,3,3,3,3,3,3,3,3,3,3,3,3,3,4),(-0.423931964449299,
-0.398828895834902,-0.377505476130339,-0.372498818727613,-0.347705174956756,
-0.32990042178538,-0.325542832515127,-0.321200290882412,-0.297020641771167,
-0.273379185129757,-0.250225980523141,-0.239676135708419,-0.235939475515521,
-0.213014612686521,-0.205267149585748,-0.181769288410816,-0.159132288662692,
-0.153558814986012,-0.130782794694077,-0.108108185525988,-0.0856259844313709,
-0.0774184937638966,-0.0738810096236942,-0.0519894683140413,-0.030460990690467,
-0.00962200678755835,-1.16575970560916E-14),.UNSPECIFIED.);
#1245=B_SPLINE_CURVE_WITH_KNOTS('',3,(#35252,#35253,#35254,#35255,#35256,
#35257,#35258,#35259,#35260,#35261,#35262,#35263,#35264,#35265,#35266,#35267,
#35268,#35269,#35270,#35271,#35272,#35273,#35274,#35275,#35276,#35277,#35278,
#35279,#35280,#35281,#35282,#35283,#35284,#35285,#35286,#35287,#35288,#35289,
#35290,#35291,#35292,#35293,#35294,#35295,#35296,#35297,#35298,#35299,#35300,
#35301,#35302,#35303,#35304,#35305,#35306,#35307,#35308,#35309,#35310,#35311,
#35312,#35313,#35314,#35315,#35316,#35317,#35318,#35319,#35320,#35321,#35322,
#35323,#35324,#35325,#35326,#35327,#35328,#35329,#35330),.UNSPECIFIED.,
 .F.,.F.,(4,3,3,3,3,3,3,3,3,3,3,3,3,3,3,3,3,3,3,3,3,3,3,3,3,3,4),(-0.43028912773393,
-0.409095039634617,-0.389617234398967,-0.383301851779856,-0.361178803936431,
-0.343501455552783,-0.339161608446753,-0.316328762903765,-0.293495917360776,
-0.27693657759957,-0.264333174521167,-0.258637327723869,-0.234922334847588,
-0.227258558315955,-0.204133994215651,-0.181009430115347,-0.177044799294305,
-0.153366378725593,-0.129080143187624,-0.104793907649655,-0.0968425625095517,
-0.0919203420448217,-0.0878017623663734,-0.0627749710934861,-0.0377028824416867,
-0.0131606293708096,0.),.UNSPECIFIED.);
#1246=B_SPLINE_CURVE_WITH_KNOTS('',3,(#35835,#35836,#35837,#35838),
 .UNSPECIFIED.,.F.,.F.,(4,4),(-0.0446554005265974,0.),.UNSPECIFIED.);
#1247=B_SPLINE_CURVE_WITH_KNOTS('',3,(#35839,#35840,#35841,#35842,#35843,
#35844,#35845,#35846,#35847,#35848,#35849,#35850,#35851,#35852,#35853,#35854,
#35855,#35856,#35857,#35858,#35859,#35860,#35861,#35862,#35863,#35864,#35865,
#35866,#35867,#35868,#35869,#35870,#35871,#35872,#35873,#35874,#35875,#35876,
#35877,#35878,#35879,#35880,#35881,#35882,#35883,#35884,#35885,#35886,#35887,
#35888,#35889,#35890,#35891,#35892,#35893,#35894,#35895,#35896,#35897,#35898,
#35899,#35900,#35901,#35902,#35903,#35904,#35905,#35906,#35907,#35908,#35909,
#35910,#35911,#35912,#35913,#35914,#35915,#35916,#35917),.UNSPECIFIED.,
 .F.,.F.,(4,3,3,3,3,3,3,3,3,3,3,3,3,3,3,3,3,3,3,3,3,3,3,3,3,3,4),(-0.430284631122155,
-0.409090485009149,-0.389617069570191,-0.38330183976251,-0.361188616218542,
-0.343501442591732,-0.339161607595677,-0.316328764317089,-0.293495921038502,
-0.276936580357852,-0.26433317834727,-0.258637326590171,-0.234922332869949,
-0.227258558315902,-0.204375919054567,-0.181009440361364,-0.177044805514887,
-0.153366390422607,-0.129080158372962,-0.104793926323317,-0.0968425970791397,
-0.0919205100039578,-0.0878017655959253,-0.0628154480136494,-0.0378426001661505,
-0.0131606168603668,0.),.UNSPECIFIED.);
#1248=B_SPLINE_CURVE_WITH_KNOTS('',3,(#35922,#35923,#35924,#35925,#35926,
#35927,#35928,#35929,#35930,#35931,#35932,#35933,#35934,#35935,#35936,#35937,
#35938,#35939,#35940,#35941,#35942,#35943,#35944,#35945,#35946,#35947,#35948,
#35949,#35950,#35951,#35952,#35953,#35954,#35955,#35956,#35957,#35958,#35959,
#35960,#35961,#35962,#35963,#35964,#35965,#35966,#35967,#35968,#35969,#35970,
#35971,#35972,#35973,#35974,#35975,#35976,#35977,#35978,#35979,#35980,#35981,
#35982,#35983,#35984,#35985,#35986,#35987,#35988,#35989,#35990,#35991,#35992,
#35993,#35994,#35995,#35996,#35997,#35998,#35999,#36000),.UNSPECIFIED.,
 .F.,.F.,(4,3,3,3,3,3,3,3,3,3,3,3,3,3,3,3,3,3,3,3,3,3,3,3,3,3,4),(-0.423931917983707,
-0.398828849205038,-0.377505459037515,-0.372498795999555,-0.347705151353274,
-0.329900401132338,-0.325542781731763,-0.321200279025117,-0.297020628104016,
-0.273379162081259,-0.250225943592493,-0.239676120732133,-0.235939452644732,
-0.213014579934855,-0.205267149585788,-0.181769286159282,-0.159132282983792,
-0.153558817716272,-0.130782793604138,-0.108108193702964,-0.0856260055726251,
-0.0774185049266986,-0.0738810206053447,-0.0519894904181288,-0.0306843036419977,
-0.00962206573183614,-7.03132749747345E-15),.UNSPECIFIED.);
#1249=B_SPLINE_CURVE_WITH_KNOTS('',3,(#36506,#36507,#36508,#36509),
 .UNSPECIFIED.,.F.,.F.,(4,4),(-0.0447834994719192,0.),.UNSPECIFIED.);
#1250=B_SPLINE_CURVE_WITH_KNOTS('',3,(#37380,#37381,#37382,#37383,#37384,
#37385,#37386,#37387,#37388,#37389,#37390,#37391,#37392,#37393,#37394,#37395,
#37396,#37397,#37398,#37399,#37400,#37401,#37402,#37403,#37404,#37405,#37406,
#37407,#37408,#37409,#37410,#37411,#37412,#37413,#37414,#37415,#37416,#37417,
#37418,#37419,#37420,#37421,#37422,#37423,#37424,#37425,#37426,#37427,#37428,
#37429,#37430,#37431,#37432,#37433,#37434,#37435,#37436,#37437,#37438,#37439,
#37440,#37441,#37442,#37443,#37444,#37445,#37446,#37447,#37448,#37449,#37450,
#37451,#37452,#37453,#37454,#37455,#37456,#37457,#37458,#37459,#37460,#37461,
#37462,#37463,#37464,#37465,#37466,#37467,#37468,#37469,#37470,#37471,#37472,
#37473,#37474,#37475,#37476,#37477,#37478,#37479,#37480,#37481,#37482,#37483,
#37484,#37485,#37486,#37487,#37488,#37489,#37490,#37491,#37492,#37493,#37494,
#37495,#37496,#37497,#37498,#37499,#37500,#37501,#37502,#37503,#37504,#37505,
#37506,#37507,#37508,#37509),.UNSPECIFIED.,.F.,.F.,(4,3,3,3,3,3,3,3,3,3,
3,3,3,3,3,3,3,3,3,3,3,3,3,3,3,3,3,3,3,3,3,3,3,3,3,3,3,3,3,3,3,3,3,4),(10.3186182874641,
10.3239953002556,10.4300038943101,10.5411527598664,10.6468733851658,10.7525295886974,
10.8581575555237,10.9637934277648,11.0695404627179,11.1753522010957,11.2813394755448,
11.3191948187603,11.4252459288507,11.5363894799025,11.6421623944753,11.74787433385,
11.8535614052088,11.9592596763638,12.065073665625,12.1709550724332,12.2770154594751,
12.314394337265,12.4201373345448,12.5257192007202,12.6311751710519,12.7365642163835,
12.8419229525085,12.9472879499407,13.0527650948566,13.1583061525316,13.2640283089846,
13.3095938557697,13.4154942679295,13.5266566562226,13.6322701065976,13.7378198081219,
13.8433421239847,13.9488733752784,14.0545180315408,14.1602285717525,14.2661173730005,
14.3047933742744,14.4106730427761,14.457190242259),.UNSPECIFIED.);
#1251=B_SPLINE_CURVE_WITH_KNOTS('',3,(#37512,#37513,#37514,#37515,#37516,
#37517,#37518,#37519,#37520,#37521,#37522,#37523,#37524,#37525,#37526,#37527,
#37528,#37529,#37530,#37531,#37532,#37533,#37534,#37535,#37536,#37537,#37538,
#37539,#37540,#37541,#37542,#37543,#37544,#37545,#37546,#37547,#37548,#37549,
#37550,#37551,#37552,#37553,#37554,#37555,#37556,#37557,#37558,#37559,#37560,
#37561,#37562,#37563,#37564,#37565,#37566,#37567,#37568,#37569,#37570,#37571,
#37572,#37573,#37574,#37575,#37576,#37577,#37578,#37579,#37580,#37581,#37582,
#37583,#37584,#37585,#37586,#37587,#37588,#37589,#37590,#37591,#37592,#37593,
#37594,#37595,#37596),.UNSPECIFIED.,.F.,.F.,(4,3,3,3,3,3,3,3,3,3,3,3,3,
3,3,3,3,3,3,3,3,3,3,3,3,3,3,3,4),(11.6725302876646,11.7808330913471,11.8916951806998,
11.9999183950615,12.1081436308134,12.2164003956853,12.3292327483063,12.4377217360197,
12.5463108432516,12.6550959203905,12.6677298061693,12.7725797148627,12.8772543949575,
12.9817864245415,13.0862414773316,13.1906574122375,13.295072030404,13.3995935079154,
13.5041742946929,13.6089390469749,13.662929324674,13.768906453379,13.8747386674348,
13.9804623817128,14.0861138807601,14.1917607912468,14.297403516148,14.4031294877355,
14.4560348278906),.UNSPECIFIED.);
#1252=B_SPLINE_CURVE_WITH_KNOTS('',3,(#37602,#37603,#37604,#37605,#37606,
#37607,#37608,#37609,#37610,#37611,#37612,#37613,#37614,#37615,#37616,#37617,
#37618,#37619,#37620,#37621,#37622,#37623,#37624,#37625,#37626,#37627,#37628,
#37629,#37630,#37631,#37632,#37633,#37634,#37635,#37636,#37637,#37638,#37639,
#37640,#37641,#37642,#37643,#37644,#37645,#37646,#37647,#37648,#37649,#37650,
#37651,#37652,#37653,#37654,#37655,#37656,#37657,#37658,#37659,#37660,#37661,
#37662,#37663,#37664,#37665,#37666,#37667,#37668,#37669,#37670,#37671,#37672,
#37673,#37674,#37675,#37676,#37677,#37678,#37679,#37680,#37681,#37682,#37683,
#37684,#37685,#37686,#37687,#37688,#37689,#37690,#37691,#37692,#37693,#37694,
#37695,#37696,#37697,#37698,#37699,#37700,#37701,#37702,#37703,#37704,#37705,
#37706,#37707,#37708,#37709,#37710,#37711,#37712,#37713,#37714,#37715,#37716,
#37717,#37718,#37719,#37720,#37721,#37722,#37723,#37724,#37725,#37726,#37727,
#37728,#37729,#37730,#37731,#37732,#37733,#37734,#37735,#37736,#37737,#37738,
#37739,#37740,#37741,#37742,#37743,#37744,#37745,#37746,#37747,#37748,#37749,
#37750,#37751,#37752,#37753,#37754,#37755),.UNSPECIFIED.,.F.,.F.,(4,3,3,
3,3,3,3,3,3,3,3,3,3,3,3,3,3,3,3,3,3,3,3,3,3,3,3,3,3,3,3,3,3,3,3,3,3,3,3,
3,3,3,3,3,3,3,3,3,3,3,3,4),(15.707963267949,15.8151330995317,15.9223517262571,
16.0297361942916,16.1372132458269,16.2449080240999,16.2951924112838,16.4010712431056,
16.5122363289409,16.6178281121499,16.7233561737618,16.8288569113081,16.9343666802768,
17.0399901377781,17.1456796180955,17.2515477643943,17.2903919297885,17.3962679028274,
17.5074333460106,17.6130223227781,17.7185476047815,17.8240455940151,17.9295526504612,
18.0351734668675,18.1408603442465,18.2467259693383,18.2855914482932,18.3914628384719,
18.5026288545127,18.6082130240858,18.7137334296441,18.8192264806583,18.924728544519,
19.0303443187165,19.1360261191755,19.241886662104,19.2807909667979,19.3866656920306,
19.4978312911896,19.6034189078599,19.7089427922628,19.814439348484,19.9199449385594,
20.0255642478333,20.1312495927124,20.2371136612566,20.2759904853026,20.3818694039373,
20.4875658530965,20.5931570867173,20.698678083258,20.7399394645196),
 .UNSPECIFIED.);
#1253=B_SPLINE_CURVE_WITH_KNOTS('',3,(#37756,#37757,#37758,#37759,#37760,
#37761,#37762,#37763,#37764,#37765,#37766,#37767,#37768,#37769,#37770,#37771,
#37772,#37773,#37774,#37775,#37776,#37777,#37778,#37779,#37780,#37781,#37782,
#37783,#37784,#37785,#37786,#37787,#37788,#37789,#37790,#37791,#37792),
 .UNSPECIFIED.,.F.,.F.,(4,3,3,3,3,3,3,3,3,3,3,3,4),(14.457190242259,14.562854862703,
14.6684337986202,14.7739634667209,14.8794802188877,14.9850965746116,15.0907591877488,
15.1966208740822,15.2999928927791,15.4167046733531,15.5330578786748,15.6488271475791,
15.7079632676211),.UNSPECIFIED.);
#1254=B_SPLINE_CURVE_WITH_KNOTS('',3,(#37794,#37795,#37796,#37797,#37798,
#37799,#37800,#37801,#37802,#37803,#37804,#37805,#37806,#37807,#37808,#37809,
#37810,#37811,#37812,#37813,#37814,#37815,#37816,#37817,#37818,#37819,#37820,
#37821,#37822,#37823,#37824,#37825,#37826,#37827,#37828,#37829,#37830,#37831,
#37832,#37833),.UNSPECIFIED.,.F.,.F.,(4,3,3,3,3,3,3,3,3,3,3,3,3,4),(14.4560348278906,
14.562000547318,14.6581288431788,14.7641800030469,14.8753235478765,14.9810965159128,
15.0868085099609,15.1924956371218,15.2981939651273,15.4040080124557,15.509889478102,
15.6159499246049,15.6533283616835,15.707963267949),.UNSPECIFIED.);
#1255=B_SPLINE_CURVE_WITH_KNOTS('',3,(#37834,#37835,#37836,#37837,#37838,
#37839,#37840,#37841,#37842,#37843,#37844,#37845,#37846,#37847,#37848,#37849,
#37850,#37851,#37852,#37853,#37854,#37855,#37856,#37857,#37858,#37859,#37860,
#37861,#37862,#37863,#37864,#37865,#37866,#37867,#37868,#37869,#37870,#37871,
#37872,#37873,#37874,#37875,#37876,#37877,#37878,#37879,#37880,#37881,#37882,
#37883,#37884,#37885,#37886,#37887,#37888,#37889,#37890,#37891,#37892,#37893,
#37894,#37895,#37896,#37897,#37898,#37899,#37900,#37901,#37902,#37903,#37904,
#37905,#37906,#37907,#37908,#37909,#37910,#37911,#37912,#37913,#37914,#37915,
#37916,#37917,#37918,#37919,#37920,#37921,#37922,#37923,#37924,#37925,#37926,
#37927,#37928,#37929,#37930,#37931,#37932,#37933,#37934,#37935,#37936,#37937,
#37938,#37939,#37940,#37941,#37942,#37943,#37944,#37945,#37946,#37947,#37948,
#37949,#37950,#37951,#37952,#37953,#37954,#37955,#37956,#37957,#37958,#37959,
#37960,#37961,#37962,#37963,#37964,#37965,#37966,#37967,#37968,#37969,#37970,
#37971,#37972,#37973,#37974,#37975,#37976,#37977,#37978,#37979,#37980,#37981,
#37982,#37983,#37984,#37985,#37986,#37987,#37988,#37989,#37990,#37991,#37992,
#37993,#37994,#37995,#37996,#37997,#37998,#37999,#38000,#38001,#38002,#38003,
#38004,#38005,#38006,#38007,#38008,#38009,#38010,#38011),.UNSPECIFIED.,
 .F.,.F.,(4,2,2,2,2,2,2,2,2,2,2,2,2,2,2,2,2,2,2,2,2,2,2,2,2,2,2,2,2,2,2,
2,2,2,2,2,2,2,2,2,2,2,2,2,2,2,2,2,2,2,2,2,2,2,2,2,2,2,2,2,2,2,2,2,2,2,2,
2,2,2,2,2,2,2,2,2,2,2,2,2,2,2,2,2,2,2,2,2,4),(-2.43133029467023,-2.38045001641935,
-2.35582585487554,-2.34996458315354,-2.34737231509244,-2.34544514087839,
-2.34364787513912,-2.34117544414635,-2.33486585233081,-2.28574937995146,
-2.26320221662845,-2.25641259847009,-2.25337582158693,-2.25165987492902,
-2.25015458445799,-2.24908376645736,-2.24807298134615,-2.24639599349135,
-2.2420617591264,-2.20459396018532,-2.20325870874998,-2.16114216120753,
-2.15647733790003,-2.15409971006157,-2.15220279008586,-2.15002604328546,
-2.14630497841577,-2.1327292995895,-2.12305786403638,-2.0723386663915,-2.06093177442003,
-2.05865927109117,-2.05740262436177,-2.0563309285897,-2.05497533199509,
-2.05221788883994,-2.03150830505557,-1.99827162636792,-1.97841989445824,
-1.96681044873025,-1.96343346403003,-1.96133520783537,-1.95940855322915,
-1.95693657970761,-1.95286438517933,-1.92477504883846,-1.87686021439252,
-1.86815836690016,-1.86606893828926,-1.86485555255859,-1.86378135222052,
-1.86239428053879,-1.86008446922467,-1.84548994150369,-1.84188271978142,
-1.83737314524978,-1.78735171086278,-1.77449287947572,-1.77099907195111,
-1.76887677773858,-1.76695963469935,-1.76450247220002,-1.76056358161632,
-1.73709776247759,-1.68729728933206,-1.67596246878737,-1.67370142540451,
-1.67245099739686,-1.67138219433715,-1.67002849029079,-1.66727639878152,
-1.63428435466996,-1.60904546014541,-1.58569358874201,-1.57997665320094,
-1.57739888543641,-1.57546262700068,-1.5736423375891,-1.57111494340174,
-1.56453208978344,-1.51953315279275,-1.49439804095941,-1.48351717476073,
-1.48127975245331,-1.48003320198764,-1.47896300189892,-1.47760087849872,
-1.47480684896619,-1.45825318070351),.UNSPECIFIED.);
#1256=B_SPLINE_CURVE_WITH_KNOTS('',3,(#38017,#38018,#38019,#38020,#38021,
#38022,#38023,#38024,#38025,#38026,#38027,#38028,#38029,#38030,#38031,#38032,
#38033,#38034,#38035,#38036,#38037,#38038,#38039,#38040,#38041,#38042,#38043,
#38044,#38045,#38046,#38047,#38048,#38049,#38050,#38051,#38052,#38053,#38054,
#38055,#38056,#38057,#38058,#38059,#38060,#38061,#38062,#38063,#38064,#38065,
#38066,#38067,#38068,#38069,#38070,#38071,#38072,#38073,#38074,#38075,#38076,
#38077,#38078,#38079,#38080,#38081,#38082,#38083,#38084,#38085,#38086,#38087,
#38088,#38089,#38090,#38091,#38092,#38093,#38094,#38095,#38096,#38097,#38098,
#38099,#38100,#38101,#38102,#38103,#38104,#38105,#38106,#38107,#38108,#38109,
#38110,#38111,#38112,#38113,#38114,#38115,#38116,#38117,#38118,#38119,#38120,
#38121,#38122,#38123,#38124,#38125,#38126,#38127,#38128,#38129,#38130,#38131,
#38132,#38133,#38134,#38135,#38136,#38137,#38138,#38139,#38140,#38141,#38142,
#38143,#38144,#38145,#38146,#38147,#38148,#38149,#38150,#38151,#38152,#38153,
#38154,#38155,#38156,#38157,#38158,#38159,#38160,#38161,#38162,#38163,#38164,
#38165,#38166,#38167,#38168,#38169,#38170,#38171,#38172,#38173,#38174,#38175,
#38176,#38177,#38178,#38179,#38180,#38181,#38182,#38183,#38184,#38185,#38186,
#38187,#38188,#38189,#38190,#38191,#38192,#38193,#38194,#38195,#38196,#38197,
#38198,#38199,#38200),.UNSPECIFIED.,.F.,.F.,(4,2,2,2,2,2,2,2,2,2,2,2,2,
2,2,2,2,2,2,2,2,2,2,2,2,2,2,2,2,2,2,2,2,2,2,2,2,2,2,2,2,2,2,2,2,2,2,2,2,
2,2,2,2,2,2,2,2,2,2,2,2,2,2,2,2,2,2,2,2,2,2,2,2,2,2,2,2,2,2,2,2,2,2,2,2,
2,2,2,2,2,2,4),(-0.973731012778231,-0.955750958635197,-0.927909947755372,
-0.923844024993355,-0.921373817980455,-0.919447326652216,-0.917348026432846,
-0.913966681351581,-0.902316084334358,-0.882364141007552,-0.846990293236625,
-0.842697461103928,-0.828114535608816,-0.825803131074563,-0.824414718568904,
-0.82333944937632,-0.822125063138687,-0.820033087835368,-0.811307980630995,
-0.763285194946165,-0.735403154309707,-0.731336423695054,-0.728866047581838,
-0.726939616766068,-0.724840576847746,-0.721460080022725,-0.709816718998952,
-0.689882362547447,-0.670522457648294,-0.63846656759735,-0.634012125360898,
-0.632315970877924,-0.631301323134629,-0.630204156020763,-0.628653925132381,
-0.624810025087573,-0.605890794874009,-0.580447336426393,-0.569174825301193,
-0.542898176919398,-0.538863974553914,-0.536403146008452,-0.534478019893663,
-0.53237416812308,-0.528972086168774,-0.517113257272782,-0.467748584387895,
-0.443502234065478,-0.440697060970407,-0.439332560367093,-0.438262155148899,
-0.437017434643968,-0.434787607278837,-0.424028574732282,-0.39939235477578,
-0.353670719479631,-0.347123507531396,-0.344601732751843,-0.342782934594833,
-0.34084590276073,-0.338263073718374,-0.332518166164782,-0.324799974382857,
-0.304815429683866,-0.260585220866742,-0.250183900526884,-0.248090563291109,
-0.246752913181188,-0.245684319785793,-0.244419147477469,-0.242095000800413,
-0.229725171460215,-0.197764680691731,-0.160971399894507,-0.154554730935017,
-0.152053934683415,-0.150240545456253,-0.148300202652094,-0.146394599564277,
-0.142044179569303,-0.118569620754311,-0.0985583869616866,-0.0813296821625467,
-0.0793844099193463,-0.0584312395777052,-0.0556646330183186,-0.0543077968269223,
-0.0532380215325895,-0.051987825727483,-0.0497327075339078,-0.0469305815507994,
-0.000564225491686792),.UNSPECIFIED.);
#1257=B_SPLINE_CURVE_WITH_KNOTS('',3,(#38201,#38202,#38203,#38204,#38205,
#38206,#38207,#38208,#38209,#38210,#38211,#38212,#38213,#38214,#38215,#38216,
#38217,#38218,#38219,#38220,#38221,#38222,#38223,#38224,#38225,#38226,#38227,
#38228,#38229,#38230,#38231,#38232,#38233,#38234,#38235,#38236,#38237),
 .UNSPECIFIED.,.F.,.F.,(4,3,3,3,3,3,3,3,3,3,3,3,4),(20.7399394645196,20.8454343576969,
20.9518732692245,21.0575111976985,21.1643506007529,21.2711900038073,21.3761014635548,
21.480866411635,21.5855227766783,21.6901309418475,21.7947058019396,21.8993450709265,
21.9911485751286),.UNSPECIFIED.);
#1258=B_SPLINE_CURVE_WITH_KNOTS('',3,(#38238,#38239,#38240,#38241,#38242,
#38243,#38244,#38245,#38246,#38247,#38248,#38249,#38250,#38251,#38252,#38253,
#38254,#38255,#38256,#38257,#38258,#38259,#38260,#38261,#38262,#38263,#38264,
#38265,#38266,#38267,#38268,#38269,#38270,#38271,#38272,#38273,#38274,#38275,
#38276,#38277,#38278,#38279,#38280,#38281,#38282,#38283,#38284,#38285,#38286,
#38287,#38288,#38289,#38290,#38291,#38292,#38293,#38294,#38295,#38296,#38297,
#38298,#38299,#38300,#38301,#38302,#38303,#38304,#38305,#38306,#38307,#38308,
#38309,#38310,#38311,#38312,#38313,#38314,#38315,#38316,#38317,#38318,#38319,
#38320,#38321,#38322,#38323,#38324,#38325,#38326,#38327,#38328,#38329,#38330,
#38331,#38332,#38333,#38334,#38335,#38336,#38337,#38338,#38339,#38340,#38341,
#38342,#38343,#38344,#38345,#38346,#38347,#38348,#38349,#38350,#38351,#38352,
#38353,#38354,#38355,#38356,#38357,#38358,#38359,#38360,#38361,#38362,#38363,
#38364,#38365,#38366,#38367,#38368,#38369,#38370,#38371,#38372,#38373,#38374,
#38375,#38376,#38377,#38378,#38379,#38380,#38381,#38382,#38383,#38384,#38385,
#38386,#38387,#38388,#38389,#38390,#38391,#38392,#38393,#38394,#38395,#38396,
#38397,#38398,#38399,#38400,#38401,#38402,#38403,#38404,#38405,#38406,#38407,
#38408,#38409,#38410,#38411,#38412,#38413,#38414,#38415,#38416,#38417,#38418,
#38419,#38420,#38421,#38422,#38423,#38424,#38425,#38426,#38427,#38428,#38429,
#38430,#38431,#38432,#38433,#38434,#38435,#38436,#38437,#38438,#38439,#38440,
#38441,#38442,#38443,#38444,#38445,#38446,#38447),.UNSPECIFIED.,.F.,.F.,
(4,2,2,2,2,2,2,2,2,2,2,2,2,2,2,2,2,2,2,2,2,2,2,2,2,2,2,2,2,2,2,2,2,2,2,
2,2,2,2,2,2,2,2,2,2,2,2,2,2,2,2,2,2,2,2,2,2,2,2,2,2,2,2,2,2,2,2,2,2,2,2,
2,2,2,2,2,2,2,2,2,2,2,2,2,2,2,2,2,2,2,2,2,2,2,2,2,2,2,2,2,2,2,2,2,4),(-1.45825318070351,
-1.45156178778247,-1.42090792497479,-1.40102276261981,-1.38939887848518,
-1.38602083639596,-1.38392262513754,-1.38199648791495,-1.37952584138216,
-1.37545724963582,-1.34748120068021,-1.29950333832415,-1.29079437424628,
-1.28870398222319,-1.28749014757655,-1.28641514699885,-1.28502680057963,
-1.28271489394581,-1.2681049786494,-1.26053267416157,-1.21637831561782,
-1.19820627391089,-1.19452940480568,-1.19215069055576,-1.19023982714425,
-1.18806589020858,-1.18434464466145,-1.16872170824729,-1.10977602424721,
-1.09873956671539,-1.0966071259162,-1.09525768936263,-1.09418855470572,
-1.0929330402689,-1.09065330185538,-1.07901753526725,-1.02564218440679,
-1.00579633564512,-1.00202362975111,-0.999615218290805,-0.997701221088182,
-0.995545782674325,-0.991910100888293,-0.977418749284369,-0.949515751727793,
-0.909099786448388,-0.904865961813497,-0.903205015183827,-0.902197083093176,
-0.901094145324588,-0.899513702299606,-0.895479460004572,-0.874680517282409,
-0.832977281385335,-0.813300926898741,-0.809536708368696,-0.807130920758082,
-0.805217220821617,-0.803060222208958,-0.799417318693306,-0.784834337890712,
-0.73530540501547,-0.714355716199509,-0.711589300202888,-0.710232547595368,
-0.709162826002879,-0.7079126754028,-0.705657631261806,-0.694465257317898,
-0.646214321686994,-0.621179007803346,-0.617190326586427,-0.614716520525246,
-0.612795209862247,-0.610677226762678,-0.607210898824432,-0.594682526475048,
-0.54429322378361,-0.541775326839909,-0.534962483064637,-0.521403817291864,
-0.519138492929374,-0.517763632053185,-0.516690000901088,-0.515467352430039,
-0.513338033538654,-0.504109563266951,-0.455558614375983,-0.428725696984432,
-0.424685281485952,-0.422222638518982,-0.420297280843739,-0.418194382487543,
-0.41479652381461,-0.402979963969508,-0.353683036759244,-0.329323022126649,
-0.326516834600987,-0.325152143085468,-0.324081736938291,-0.32283718818749,
-0.320608075622083,-0.309860402849404,-0.285269174135166,-0.242759173181297),
 .UNSPECIFIED.);
#1259=B_SPLINE_CURVE_WITH_KNOTS('',3,(#38452,#38453,#38454,#38455,#38456,
#38457,#38458,#38459,#38460,#38461,#38462,#38463,#38464,#38465,#38466,#38467,
#38468,#38469,#38470,#38471,#38472,#38473,#38474,#38475,#38476,#38477,#38478,
#38479,#38480,#38481,#38482,#38483,#38484,#38485,#38486,#38487,#38488,#38489,
#38490,#38491,#38492,#38493,#38494,#38495,#38496,#38497,#38498,#38499,#38500,
#38501,#38502,#38503,#38504,#38505,#38506,#38507,#38508,#38509,#38510,#38511,
#38512,#38513,#38514,#38515,#38516,#38517,#38518,#38519,#38520,#38521,#38522,
#38523,#38524,#38525,#38526,#38527,#38528,#38529,#38530,#38531,#38532,#38533,
#38534,#38535,#38536,#38537,#38538,#38539,#38540,#38541,#38542,#38543,#38544,
#38545,#38546,#38547,#38548,#38549,#38550,#38551,#38552,#38553,#38554,#38555,
#38556,#38557,#38558,#38559,#38560,#38561,#38562,#38563,#38564,#38565,#38566,
#38567,#38568,#38569,#38570,#38571,#38572,#38573,#38574,#38575,#38576,#38577,
#38578,#38579,#38580,#38581,#38582,#38583,#38584,#38585,#38586,#38587,#38588,
#38589,#38590,#38591,#38592,#38593,#38594,#38595,#38596,#38597,#38598,#38599,
#38600,#38601,#38602,#38603,#38604,#38605,#38606,#38607,#38608,#38609,#38610,
#38611,#38612,#38613,#38614,#38615,#38616,#38617,#38618,#38619,#38620,#38621,
#38622,#38623,#38624,#38625,#38626,#38627,#38628,#38629,#38630,#38631,#38632,
#38633,#38634,#38635,#38636,#38637,#38638,#38639,#38640,#38641,#38642,#38643,
#38644,#38645,#38646,#38647,#38648,#38649,#38650,#38651,#38652,#38653,#38654,
#38655,#38656,#38657,#38658,#38659,#38660,#38661,#38662,#38663,#38664,#38665,
#38666,#38667,#38668,#38669,#38670,#38671,#38672,#38673,#38674,#38675,#38676,
#38677,#38678,#38679),.UNSPECIFIED.,.F.,.F.,(4,2,2,2,2,2,2,2,2,2,2,2,2,
2,2,2,2,2,2,2,2,2,2,2,2,2,2,2,2,2,2,2,2,2,2,2,2,2,2,2,2,2,2,2,2,2,2,2,2,
2,2,2,2,2,2,2,2,2,2,2,2,2,2,2,2,2,2,2,2,2,2,2,2,2,2,2,2,2,2,2,2,2,2,2,2,
2,2,2,2,2,2,2,2,2,2,2,2,2,2,2,2,2,2,2,2,2,2,2,2,2,2,2,2,4),(-2.18907843185636,
-2.1839306013294,-2.17485020575198,-2.17273199547205,-2.17151200523755,
-2.17043821167424,-2.1690599687162,-2.16678258086056,-2.15298325962618,
-2.14407336322025,-2.09404474057858,-2.08113083700294,-2.07762964538173,
-2.07550427092731,-2.07358523571058,-2.07112686624626,-2.06718845219888,
-2.04352277838749,-1.99392469203216,-1.98260702366587,-1.9803451476513,
-1.97909365696134,-1.97802428852795,-1.97666991122767,-1.97391466295616,
-1.94102259251772,-1.91596288141848,-1.8923771341101,-1.88663055052084,
-1.88404773803523,-1.88211102295667,-1.88029273909076,-1.87777202276496,
-1.87122963832237,-1.82541566561039,-1.80082765372363,-1.79008210236407,
-1.7878533619564,-1.78660902981171,-1.78553881750097,-1.78417438900382,
-1.78136876502146,-1.75699340207282,-1.70774602364499,-1.69594469696769,
-1.69254873306982,-1.69044647398244,-1.68852134558622,-1.68605850477318,
-1.68201668517563,-1.65511711555205,-1.60638806299799,-1.59735403843273,
-1.59523899949626,-1.5940195897443,-1.59294547489239,-1.59156575312678,
-1.5892837254437,-1.57538620389586,-1.53753193309329,-1.5052955359033,-1.50087091112575,
-1.49854547458503,-1.49663774468201,-1.49442304134062,-1.49061937817887,
-1.47559385812967,-1.46762063018482,-1.4297860559281,-1.41322955288997,
-1.40479868284896,-1.40272975314678,-1.40152054116425,-1.40044422584235,
-1.39904717505007,-1.39670603320875,-1.38135480916071,-1.34231200871113,
-1.31548288268737,-1.30933359090502,-1.30667934594091,-1.3047306205867,
-1.30293049425767,-1.30048066331338,-1.29436616552681,-1.24352118243223,
-1.22232034260141,-1.21576905562745,-1.21148236839234,-1.20981285835396,
-1.20880331644811,-1.20770183331242,-1.20612900255011,-1.20214357010386,
-1.18183778006478,-1.14511941468412,-1.12031081678326,-1.11632887885858,
-1.11385702466666,-1.11193586457025,-1.10981666469395,-1.10634518918034,
-1.09376300387386,-1.04341552098978,-1.03992207094416,-1.03518427337638,
-1.02062666848119,-1.01831619305407,-1.0169280136395,-1.01585272486253,
-1.01463809124073,-1.01254517944843,-1.00380882148382,-0.973731012778231),
 .UNSPECIFIED.);
#1260=B_SPLINE_CURVE_WITH_KNOTS('',3,(#38681,#38682,#38683,#38684,#38685,
#38686,#38687,#38688,#38689,#38690,#38691,#38692,#38693,#38694,#38695,#38696,
#38697,#38698,#38699,#38700,#38701,#38702,#38703,#38704,#38705,#38706,#38707,
#38708,#38709,#38710,#38711,#38712,#38713,#38714,#38715,#38716,#38717,#38718,
#38719,#38720,#38721,#38722,#38723,#38724,#38725,#38726,#38727,#38728,#38729,
#38730,#38731,#38732,#38733,#38734,#38735,#38736),.UNSPECIFIED.,.F.,.F.,
(4,2,2,2,2,2,2,2,2,2,2,2,2,2,2,2,2,2,2,2,2,2,2,2,2,2,2,4),(-0.242759173181297,
-0.239484908413729,-0.232942998134359,-0.230422100898547,-0.228603562991515,
-0.226666463115397,-0.224134462219529,-0.218612162294353,-0.211204854271706,
-0.192410102059554,-0.15099184128989,-0.136420870478374,-0.134109912752697,
-0.132721617013,-0.131646344922579,-0.130431850700236,-0.128339453177511,
-0.119609190654219,-0.0749861339708847,-0.0622325535010866,-0.0431063276215727,
-0.0393705230611759,-0.036973320299747,-0.0350602865874416,-0.0332660364412645,
-0.0311437737735425,-0.0280691132243875,-0.000562207713922817),
 .UNSPECIFIED.);
#1261=B_SPLINE_CURVE_WITH_KNOTS('',3,(#38737,#38738,#38739,#38740,#38741,
#38742,#38743,#38744,#38745,#38746,#38747,#38748,#38749,#38750,#38751,#38752,
#38753,#38754,#38755,#38756,#38757,#38758,#38759,#38760,#38761,#38762,#38763,
#38764,#38765,#38766,#38767,#38768,#38769,#38770,#38771,#38772,#38773,#38774,
#38775,#38776,#38777,#38778,#38779,#38780,#38781,#38782,#38783,#38784,#38785,
#38786,#38787,#38788,#38789,#38790,#38791,#38792,#38793,#38794,#38795,#38796,
#38797,#38798,#38799,#38800,#38801,#38802,#38803,#38804,#38805,#38806,#38807,
#38808,#38809,#38810,#38811,#38812,#38813,#38814,#38815,#38816,#38817,#38818,
#38819,#38820,#38821,#38822,#38823,#38824,#38825,#38826,#38827,#38828,#38829,
#38830,#38831,#38832,#38833,#38834,#38835,#38836,#38837,#38838,#38839,#38840,
#38841,#38842,#38843,#38844,#38845,#38846,#38847,#38848,#38849,#38850,#38851,
#38852,#38853,#38854,#38855,#38856,#38857,#38858,#38859,#38860,#38861,#38862,
#38863,#38864,#38865,#38866,#38867,#38868,#38869,#38870,#38871,#38872,#38873,
#38874,#38875,#38876,#38877,#38878,#38879,#38880,#38881,#38882,#38883,#38884,
#38885,#38886,#38887,#38888,#38889,#38890,#38891,#38892,#38893,#38894,#38895,
#38896,#38897,#38898,#38899,#38900,#38901,#38902,#38903,#38904,#38905,#38906,
#38907,#38908),.UNSPECIFIED.,.F.,.F.,(4,2,2,2,2,2,2,2,2,2,2,2,2,2,2,2,2,
2,2,2,2,2,2,2,2,2,2,2,2,2,2,2,2,2,2,2,2,2,2,2,2,2,2,2,2,2,2,2,2,2,2,2,2,
2,2,2,2,2,2,2,2,2,2,2,2,2,2,2,2,2,2,2,2,2,2,2,2,2,2,2,2,2,2,2,2,4),(-2.43106450421894,
-2.39856083670546,-2.37674236244877,-2.37260994751277,-2.37101451032931,
-2.36990877942184,-2.36890423794777,-2.36726031490655,-2.36312756464469,
-2.32129209831977,-2.29974641558412,-2.28724398588586,-2.27896222066677,
-2.27605490535705,-2.27426731044241,-2.27234199218159,-2.26987731557179,
-2.2658290795459,-2.23915429692451,-2.19091947104382,-2.18126430669329,
-2.17910533358957,-2.17787627917333,-2.17680395021957,-2.17541678511089,
-2.17315947718651,-2.15975564875051,-2.11477183353478,-2.09118845382734,
-2.08544213871858,-2.08285935469182,-2.0809226242386,-2.07910429922532,
-2.07658348332363,-2.07004059226666,-2.02422976751882,-1.9996387147458,
-1.98889233519711,-1.98666352473376,-1.9854191676788,-1.98434894271607,
-1.98298450976323,-1.9801789165061,-1.95581080779381,-1.90655821994549,
-1.89475388316804,-1.89135759085117,-1.8892552415537,-1.887330105921,-1.88486735962884,
-1.88082591679901,-1.85394312515226,-1.80526015606077,-1.79616893882391,
-1.79404968714631,-1.79282933765577,-1.79175538811095,-1.79037715036878,
-1.78810019381254,-1.77431691885455,-1.76539662913765,-1.71538404556458,
-1.70243737393402,-1.69893281989934,-1.69680646879669,-1.69488723702736,
-1.69242956686465,-1.6884941987051,-1.66525029266196,-1.61524846150961,
-1.6038931854412,-1.60162891305741,-1.60037676902164,-1.59930725544581,
-1.59795322331895,-1.59520041140823,-1.56220203872801,-1.53696107782019,
-1.51359987938577,-1.50788181747465,-1.50530390649304,-1.50336769639834,
-1.50154757213365,-1.49902060750673,-1.49244015029847,-1.45788973492034),
 .UNSPECIFIED.);
#1262=B_SPLINE_CURVE_WITH_KNOTS('',3,(#38914,#38915,#38916,#38917,#38918,
#38919,#38920,#38921,#38922,#38923,#38924,#38925,#38926,#38927,#38928,#38929,
#38930,#38931,#38932,#38933,#38934,#38935,#38936,#38937,#38938,#38939,#38940,
#38941,#38942,#38943,#38944,#38945,#38946,#38947,#38948,#38949,#38950,#38951,
#38952,#38953,#38954,#38955,#38956,#38957,#38958,#38959,#38960,#38961,#38962,
#38963,#38964,#38965,#38966,#38967,#38968,#38969,#38970,#38971,#38972,#38973,
#38974,#38975,#38976,#38977,#38978,#38979,#38980,#38981,#38982,#38983,#38984,
#38985,#38986,#38987,#38988,#38989,#38990,#38991,#38992,#38993,#38994,#38995,
#38996,#38997,#38998,#38999,#39000,#39001,#39002,#39003,#39004,#39005,#39006,
#39007,#39008,#39009,#39010,#39011,#39012,#39013,#39014,#39015,#39016,#39017,
#39018,#39019,#39020,#39021,#39022,#39023,#39024,#39025,#39026,#39027,#39028,
#39029,#39030,#39031,#39032,#39033,#39034,#39035,#39036,#39037,#39038,#39039,
#39040,#39041,#39042,#39043,#39044,#39045,#39046,#39047,#39048,#39049,#39050,
#39051,#39052,#39053,#39054,#39055,#39056,#39057,#39058,#39059,#39060,#39061,
#39062,#39063,#39064,#39065,#39066,#39067,#39068,#39069,#39070,#39071,#39072,
#39073,#39074,#39075,#39076,#39077,#39078,#39079,#39080,#39081,#39082,#39083,
#39084,#39085,#39086,#39087,#39088,#39089,#39090,#39091,#39092,#39093,#39094,
#39095,#39096,#39097,#39098,#39099,#39100,#39101,#39102,#39103,#39104,#39105,
#39106,#39107,#39108,#39109,#39110,#39111,#39112,#39113,#39114,#39115,#39116,
#39117,#39118,#39119,#39120,#39121,#39122,#39123,#39124,#39125,#39126,#39127,
#39128,#39129,#39130,#39131,#39132,#39133,#39134,#39135,#39136,#39137),
 .UNSPECIFIED.,.F.,.F.,(4,2,2,2,2,2,2,2,2,2,2,2,2,2,2,2,2,2,2,2,2,2,2,2,
2,2,2,2,2,2,2,2,2,2,2,2,2,2,2,2,2,2,2,2,2,2,2,2,2,2,2,2,2,2,2,2,2,2,2,2,
2,2,2,2,2,2,2,2,2,2,2,2,2,2,2,2,2,2,2,2,2,2,2,2,2,2,2,2,2,2,2,2,2,2,2,2,
2,2,2,2,2,2,2,2,2,2,2,2,2,2,2,4),(-0.974049502300515,-0.939668666783827,
-0.902923410451016,-0.898553856892679,-0.896870898180754,-0.895858753339227,
-0.894759439644448,-0.893198082359334,-0.889285261111349,-0.86969915682471,
-0.844667352004037,-0.83514015638519,-0.807510274807168,-0.803449377040111,
-0.800980594572217,-0.799054239182555,-0.796954101036965,-0.793569227282947,
-0.781884496908835,-0.76184752887367,-0.723102133264661,-0.707765142038601,
-0.705424196294939,-0.704027102049918,-0.702950652573362,-0.701741163373514,
-0.699671497935943,-0.691233737908456,-0.674660025196731,-0.636815037360663,
-0.628950834903638,-0.613886812162755,-0.610079586229558,-0.607863844696181,
-0.605955842977444,-0.603630854330446,-0.599209479812135,-0.567162280502796,
-0.527685699697228,-0.515040673177024,-0.512820090426797,-0.511443784707103,
-0.510372303045744,-0.509135641296099,-0.506942831513843,-0.496781460444001,
-0.474445634807406,-0.425382181390631,-0.419088858583707,-0.416608623625157,
-0.414800587748342,-0.412856970027851,-0.410233845880524,-0.404263746921691,
-0.378908104764982,-0.338480098460455,-0.322748848151743,-0.320166781566477,
-0.318830188286942,-0.317761660335839,-0.316495652641563,-0.314167567347622,
-0.301598113336664,-0.270736343622129,-0.230053644983765,-0.225940254321415,
-0.223456038041966,-0.221527427290404,-0.221482185472768,-0.221442324415341,
-0.221407200191162,-0.221376245849259,-0.221348962512488,-0.221324912356767,
-0.221303710325948,-0.221285015497597,-0.221262112677871,-0.221239852690074,
-0.221218216089607,-0.221197183392619,-0.221176735743261,-0.221156854892689,
-0.221137524412802,-0.221118728486339,-0.221100448669947,-0.221082669150805,
-0.221065374626108,-0.221048550273309,-0.221032181853345,-0.218813215100687,
-0.214830735898025,-0.209901542601693,-0.199420047216925,-0.168749462403717,
-0.132935679079068,-0.128539983970839,-0.126852896933998,-0.12583996423875,
-0.124741321061993,-0.123183460576993,-0.119292453273063,-0.0999190980505376,
-0.0617594859685334,-0.049449157600044,-0.0360612075894408,-0.0323616080679501,
-0.0301919801619317,-0.0284710675814616,-0.0266505210595801,-0.0244014998863868,
-0.0210199944006751,-0.000563417466375508),.UNSPECIFIED.);
#1263=B_SPLINE_CURVE_WITH_KNOTS('',3,(#39138,#39139,#39140,#39141,#39142,
#39143,#39144,#39145,#39146,#39147,#39148,#39149,#39150,#39151,#39152,#39153,
#39154,#39155,#39156,#39157,#39158,#39159,#39160,#39161,#39162,#39163,#39164,
#39165,#39166,#39167,#39168,#39169,#39170,#39171,#39172,#39173,#39174,#39175,
#39176,#39177,#39178,#39179,#39180,#39181,#39182,#39183,#39184,#39185,#39186,
#39187,#39188,#39189,#39190,#39191,#39192,#39193,#39194,#39195,#39196,#39197,
#39198,#39199,#39200,#39201,#39202,#39203,#39204,#39205,#39206,#39207,#39208,
#39209,#39210,#39211,#39212,#39213,#39214,#39215,#39216,#39217),
 .UNSPECIFIED.,.F.,.F.,(4,2,2,2,2,2,2,2,2,2,2,2,2,2,2,2,2,2,2,2,2,2,2,2,
2,2,2,2,2,2,2,2,2,2,2,2,2,2,2,4),(-2.43093834628344,-2.39397070051664,-2.37058048796982,
-2.36630170697331,-2.36468428417007,-2.36357423807792,-2.36257404593918,
-2.3609530259101,-2.35695582068091,-2.31400700300329,-2.29197204327885,
-2.28032579948885,-2.27501349318285,-2.27079475016954,-2.26851854724156,
-2.26850354307076,-2.26848760853789,-2.26847067571557,-2.26845267052536,
-2.26843351207262,-2.26841311178053,-2.26839137246683,-2.26836818735123,
-2.26834343885347,-2.26831699720751,-2.2682887188571,-2.26825844457562,
-2.26822599736379,-2.26819117997167,-2.26815377194733,-2.26811352626145,
-2.26807016525541,-2.26803603321207,-2.26798677368753,-2.2679150619848,
-2.26598972177671,-2.26352362362469,-2.25947007117894,-2.23261266108948,
-2.18907843185636),.UNSPECIFIED.);
#1264=B_SPLINE_CURVE_WITH_KNOTS('',3,(#39218,#39219,#39220,#39221,#39222,
#39223,#39224,#39225,#39226,#39227,#39228,#39229,#39230,#39231,#39232,#39233,
#39234,#39235,#39236,#39237,#39238,#39239,#39240,#39241,#39242,#39243,#39244,
#39245,#39246,#39247,#39248,#39249,#39250,#39251,#39252,#39253,#39254,#39255,
#39256,#39257,#39258,#39259,#39260,#39261,#39262,#39263,#39264,#39265,#39266,
#39267,#39268,#39269,#39270,#39271,#39272,#39273,#39274,#39275,#39276,#39277,
#39278,#39279,#39280,#39281,#39282,#39283,#39284,#39285,#39286,#39287,#39288,
#39289,#39290,#39291,#39292,#39293,#39294,#39295,#39296,#39297,#39298,#39299,
#39300,#39301,#39302,#39303,#39304,#39305,#39306,#39307,#39308,#39309,#39310,
#39311,#39312,#39313,#39314,#39315,#39316,#39317,#39318,#39319,#39320,#39321,
#39322,#39323,#39324,#39325,#39326,#39327,#39328,#39329,#39330,#39331,#39332,
#39333,#39334,#39335,#39336,#39337,#39338,#39339,#39340,#39341,#39342,#39343,
#39344,#39345,#39346,#39347,#39348,#39349,#39350,#39351,#39352,#39353,#39354,
#39355,#39356,#39357,#39358,#39359,#39360,#39361,#39362,#39363,#39364,#39365,
#39366,#39367,#39368,#39369,#39370,#39371,#39372,#39373,#39374,#39375,#39376,
#39377,#39378,#39379,#39380,#39381,#39382,#39383,#39384,#39385,#39386,#39387,
#39388,#39389,#39390,#39391,#39392,#39393,#39394,#39395,#39396,#39397,#39398,
#39399,#39400,#39401,#39402,#39403,#39404,#39405,#39406,#39407,#39408,#39409,
#39410,#39411,#39412,#39413,#39414,#39415,#39416,#39417,#39418,#39419,#39420,
#39421,#39422,#39423,#39424,#39425,#39426,#39427,#39428,#39429,#39430,#39431,
#39432,#39433,#39434,#39435,#39436,#39437,#39438,#39439,#39440,#39441,#39442,
#39443,#39444,#39445,#39446,#39447),.UNSPECIFIED.,.F.,.F.,(4,2,2,2,2,2,
2,2,2,2,2,2,2,2,2,2,2,2,2,2,2,2,2,2,2,2,2,2,2,2,2,2,2,2,2,2,2,2,2,2,2,2,
2,2,2,2,2,2,2,2,2,2,2,2,2,2,2,2,2,2,2,2,2,2,2,2,2,2,2,2,2,2,2,2,2,2,2,2,
2,2,2,2,2,2,2,2,2,2,2,2,2,2,2,2,2,2,2,2,2,2,2,2,2,2,2,2,2,2,2,2,2,2,2,2,
4),(-1.45788973492034,-1.44728121954649,-1.42221084849868,-1.41134474520948,
-1.40910854636243,-1.40786245858797,-1.40679223899318,-1.40542973937949,
-1.40263457398283,-1.37934069475602,-1.34776007851332,-1.32850668156247,
-1.31713696169503,-1.31378416547413,-1.31169109939208,-1.30976257782796,
-1.30727897943553,-1.30316766916123,-1.27332662366873,-1.24564104468246,
-1.2372790077656,-1.22094418203882,-1.21738131340196,-1.21587764868769,
-1.21478874498355,-1.21361746837589,-1.21171940356069,-1.20517837232685,
-1.19380092690107,-1.16600778296183,-1.12688622356108,-1.12274113106383,
-1.12024767241467,-1.118317729489,-1.11622933928657,-1.11289754020751,-1.10172889385284,
-1.08296142385611,-1.04164101264389,-1.03783609150706,-1.02662417221638,
-1.02447889653974,-1.02312541105238,-1.02205586028173,-1.02080312246978,
-1.01853640295204,-1.00713899693282,-0.95665389978429,-0.945426749053942,
-0.932671842151801,-0.929034758466654,-0.926878944805138,-0.925156315206015,
-0.922839388460946,-0.918456085130867,-0.888030943507583,-0.851998564480172,
-0.848374980401106,-0.834363354910915,-0.832076060398842,-0.830694727931788,
-0.829620337708081,-0.828401715525089,-0.826290571027713,-0.817310809208004,
-0.76855785615866,-0.741649187938735,-0.737606931111413,-0.735143775907819,
-0.733218384570893,-0.731115821977663,-0.727719333659612,-0.715916034779185,
-0.666641219987156,-0.642244417329993,-0.639437952269776,-0.63807322854585,
-0.637002842435684,-0.635758366491829,-0.633529526385042,-0.622785929600139,
-0.598210684958713,-0.552407673828893,-0.545865416441603,-0.543344486491743,
-0.541525957326011,-0.539588896706328,-0.537005487422589,-0.531257023365038,
-0.507657095268978,-0.482576703113886,-0.449664012275572,-0.446907720230216,
-0.445552982054528,-0.444483405761475,-0.443231754005791,-0.440969806764859,
-0.429655661080284,-0.38009810743266,-0.356425316092589,-0.352477419128838,
-0.350015888108703,-0.348096098033331,-0.345971635337019,-0.342475977572016,
-0.329629296459239,-0.279504223382021,-0.270580722951042,-0.256753974007734,
-0.254474890966415,-0.253095979900508,-0.252021886514772,-0.250801794960802,
-0.24868397461504,-0.242450017710487),.UNSPECIFIED.);
#1265=B_SPLINE_CURVE_WITH_KNOTS('',3,(#39452,#39453,#39454,#39455,#39456,
#39457,#39458,#39459,#39460,#39461,#39462,#39463,#39464,#39465,#39466,#39467,
#39468,#39469,#39470,#39471,#39472,#39473,#39474,#39475,#39476,#39477,#39478,
#39479,#39480,#39481,#39482,#39483,#39484,#39485,#39486,#39487,#39488,#39489,
#39490,#39491,#39492,#39493,#39494,#39495,#39496,#39497,#39498,#39499,#39500,
#39501,#39502,#39503,#39504,#39505,#39506,#39507,#39508,#39509,#39510,#39511,
#39512,#39513,#39514,#39515,#39516,#39517,#39518,#39519,#39520,#39521,#39522,
#39523,#39524,#39525,#39526,#39527,#39528,#39529,#39530,#39531,#39532,#39533,
#39534,#39535,#39536,#39537,#39538,#39539,#39540,#39541,#39542,#39543,#39544,
#39545,#39546,#39547,#39548,#39549,#39550,#39551,#39552,#39553,#39554,#39555,
#39556,#39557,#39558,#39559,#39560,#39561,#39562,#39563,#39564,#39565,#39566,
#39567,#39568,#39569,#39570,#39571,#39572,#39573,#39574,#39575,#39576,#39577,
#39578,#39579,#39580,#39581,#39582,#39583,#39584,#39585,#39586,#39587,#39588,
#39589,#39590,#39591,#39592,#39593,#39594,#39595,#39596,#39597,#39598,#39599,
#39600,#39601,#39602,#39603,#39604,#39605,#39606,#39607,#39608,#39609,#39610,
#39611,#39612,#39613,#39614,#39615,#39616,#39617,#39618,#39619,#39620,#39621,
#39622,#39623,#39624,#39625,#39626,#39627,#39628,#39629,#39630,#39631,#39632,
#39633,#39634,#39635,#39636,#39637,#39638,#39639,#39640,#39641,#39642,#39643,
#39644,#39645,#39646,#39647,#39648,#39649,#39650,#39651,#39652,#39653,#39654,
#39655,#39656,#39657,#39658,#39659,#39660,#39661,#39662,#39663,#39664,#39665,
#39666,#39667,#39668,#39669,#39670,#39671,#39672,#39673,#39674,#39675,#39676,
#39677,#39678,#39679,#39680,#39681,#39682,#39683,#39684,#39685),
 .UNSPECIFIED.,.F.,.F.,(4,2,2,2,2,2,2,2,2,2,2,2,2,2,2,2,2,2,2,2,2,2,2,2,
2,2,2,2,2,2,2,2,2,2,2,2,2,2,2,2,2,2,2,2,2,2,2,2,2,2,2,2,2,2,2,2,2,2,2,2,
2,2,2,2,2,2,2,2,2,2,2,2,2,2,2,2,2,2,2,2,2,2,2,2,2,2,2,2,2,2,2,2,2,2,2,2,
2,2,2,2,2,2,2,2,2,2,2,2,2,2,2,2,2,2,2,2,4),(-2.18935248187665,-2.18060066749766,
-2.15694016658323,-2.15118407272377,-2.14859960122188,-2.14666268406757,
-2.14484496893962,-2.14232624925915,-2.13579608245308,-2.08978493478155,
-2.06533993589874,-2.05463044068599,-2.05240392987667,-2.05116011334871,
-2.05008988780738,-2.04872485222336,-2.0459159945143,-2.01731507032644,
-1.96501096126273,-1.95884776140898,-1.95619137442189,-1.95424252348692,
-1.95244329808938,-1.94999625583526,-1.94389681699885,-1.89293421326724,
-1.87181669331227,-1.86199324095131,-1.85982296362902,-1.85859145419472,
-1.85751956066189,-1.8561363427705,-1.85389212123688,-1.84075767891242,
-1.83663677628878,-1.79739848954192,-1.77890347580332,-1.76784751087897,
-1.76452805143229,-1.76244264719452,-1.76051222081093,-1.7580135702108,
-1.75384981185473,-1.71962175099484,-1.69700106213779,-1.67043416967073,
-1.6677376184964,-1.66639499276351,-1.66532638013963,-1.66406581435144,
-1.66182497834639,-1.65217686663973,-1.64668268224548,-1.64343190088964,
-1.6071309288505,-1.58718087532719,-1.57553045135644,-1.57214954096179,
-1.57005058069742,-1.56812444738517,-1.56565476177136,-1.5615897988422,
-1.53377242182849,-1.48567445613213,-1.47692957908397,-1.47483618816815,
-1.47362155248537,-1.47254644189409,-1.47115873906295,-1.46884957918566,
-1.45431683617923,-1.41310881236197,-1.3941816503753,-1.38294619856559,
-1.37960763855067,-1.37751789578559,-1.37558866205773,-1.37309886484303,
-1.36896580734986,-1.32913662252565,-1.29758323813264,-1.28487092155145,
-1.28253604786515,-1.28126868035578,-1.28020038155685,-1.27886581316868,
-1.27678224874297,-1.26652794218534,-1.26169040461733,-1.25848401248425,
-1.21625766280637,-1.19236615165704,-1.18841185403942,-1.18594838990454,
-1.18402835893277,-1.18190492033105,-1.17841391748335,-1.1656183993103,
-1.1154512933227,-1.10655266306099,-1.09769458274199,-1.09160171006255,
-1.08967988583714,-1.08850333668462,-1.08741668501776,-1.08592632933243,
-1.08244081493993,-1.07756942812815,-1.0641969279115,-1.01260095594681,
-0.998688442087327,-0.994983744058309,-0.992791771793684,-0.990882235579823,
-0.988527333152801,-0.983960819019553,-0.974049502300515),.UNSPECIFIED.);
#1266=B_SPLINE_CURVE_WITH_KNOTS('',3,(#39687,#39688,#39689,#39690,#39691,
#39692,#39693,#39694,#39695,#39696,#39697,#39698,#39699,#39700,#39701,#39702,
#39703,#39704,#39705,#39706,#39707,#39708,#39709,#39710,#39711,#39712,#39713,
#39714,#39715,#39716,#39717,#39718,#39719,#39720,#39721,#39722,#39723,#39724,
#39725,#39726,#39727,#39728),.UNSPECIFIED.,.F.,.F.,(4,2,2,2,2,2,2,2,2,2,
2,2,2,2,2,2,2,2,2,2,4),(-0.242450017710487,-0.239613473062178,-0.190935717053101,
-0.164054434004285,-0.160012895157732,-0.157549959845364,-0.155624609592036,
-0.153836590607114,-0.150925281606183,-0.142625917540657,-0.130083569029777,
-0.108179587073087,-0.0668015315072034,-0.0626017132925774,-0.0609463002630057,
-0.0599394409044324,-0.0588355042916628,-0.0572500557751757,-0.0531838315658337,
-0.0320590766620085,-0.000564309293417658),.UNSPECIFIED.);
#1267=B_SPLINE_CURVE_WITH_KNOTS('',3,(#39729,#39730,#39731,#39732,#39733,
#39734,#39735,#39736,#39737,#39738,#39739,#39740,#39741,#39742,#39743,#39744,
#39745,#39746,#39747,#39748,#39749,#39750,#39751,#39752,#39753,#39754,#39755,
#39756,#39757,#39758,#39759,#39760,#39761,#39762,#39763,#39764,#39765,#39766,
#39767,#39768,#39769,#39770,#39771,#39772,#39773,#39774,#39775,#39776,#39777,
#39778,#39779,#39780,#39781,#39782,#39783,#39784,#39785,#39786,#39787,#39788,
#39789,#39790,#39791,#39792,#39793,#39794,#39795,#39796,#39797,#39798,#39799,
#39800,#39801,#39802,#39803,#39804,#39805,#39806,#39807,#39808,#39809,#39810,
#39811,#39812,#39813,#39814,#39815,#39816,#39817,#39818,#39819,#39820,#39821,
#39822,#39823,#39824,#39825,#39826,#39827,#39828,#39829,#39830,#39831,#39832,
#39833,#39834,#39835,#39836,#39837,#39838,#39839,#39840,#39841,#39842,#39843,
#39844,#39845,#39846,#39847,#39848,#39849,#39850,#39851,#39852,#39853,#39854,
#39855,#39856,#39857,#39858,#39859,#39860,#39861,#39862,#39863,#39864,#39865,
#39866,#39867,#39868,#39869,#39870,#39871,#39872,#39873,#39874,#39875,#39876,
#39877,#39878,#39879,#39880,#39881,#39882,#39883,#39884,#39885,#39886,#39887,
#39888,#39889,#39890,#39891,#39892,#39893,#39894,#39895,#39896,#39897,#39898,
#39899,#39900,#39901,#39902,#39903,#39904,#39905,#39906,#39907,#39908,#39909,
#39910),.UNSPECIFIED.,.F.,.F.,(4,2,2,2,2,2,2,2,2,2,2,2,2,2,2,2,2,2,2,2,
2,2,2,2,2,2,2,2,2,2,2,2,2,2,2,2,2,2,2,2,2,2,2,2,2,2,2,2,2,2,2,2,2,2,2,2,
2,2,2,2,2,2,2,2,2,2,2,2,2,2,2,2,2,2,2,2,2,2,2,2,2,2,2,2,2,2,2,2,2,2,4),
(-2.43147070535632,-2.40300556094277,-2.39963156188484,-2.39738592739693,
-2.39556668374874,-2.39367853485371,-2.39144549981715,-2.38756058344078,
-2.37147569928083,-2.36550631723452,-2.35221906982282,-2.31294397103424,
-2.3021952056922,-2.29996651027028,-2.29872230187077,-2.29765225773529,
-2.29628812360843,-2.29348337379555,-2.26427055269208,-2.23793401837194,
-2.21916095273017,-2.21175959069598,-2.20624169758611,-2.20371034602944,
-2.20177374242271,-2.19995566421347,-2.19743539402241,-2.19089510865308,
-2.14508228266071,-2.12049602366336,-2.10975125662286,-2.10752268455289,
-2.10627844725858,-2.10520831710629,-2.10384399431071,-2.10103859108146,
-2.07666592890003,-2.02742166491021,-2.01562086601409,-2.0122251247061,
-2.01012301841169,-2.00819803996524,-2.00573540483696,-2.00169395249485,
-1.97479880611712,-1.92608023587121,-1.91703857223042,-1.91492308250195,
-1.91370363088909,-1.91262962485615,-1.91125022976533,-1.90896912756493,
-1.89508957154718,-1.85425176992584,-1.82760849123504,-1.82148173486223,
-1.81883154172982,-1.81688365480492,-1.81508279798496,-1.81262965525182,
-1.80649483109552,-1.75584471168521,-1.73452469544941,-1.72464410995741,
-1.72246991923611,-1.72123749704616,-1.72016565358985,-1.71878360770034,
-1.71654346073459,-1.70349530646087,-1.69586373357149,-1.65962603782693,
-1.63479319467049,-1.62888809174351,-1.62627671094222,-1.62433525630996,
-1.62252453751998,-1.62003325829708,-1.61367269863085,-1.56534582288567,
-1.54249751157193,-1.53220006802035,-1.52999877622483,-1.52876036673041,
-1.5276892968553,-1.52631603775879,-1.52410525764287,-1.51164787092179,
-1.50692332461291,-1.46352326967845,-1.45811225063465),.UNSPECIFIED.);
#1268=B_SPLINE_CURVE_WITH_KNOTS('',3,(#39916,#39917,#39918,#39919,#39920,
#39921,#39922,#39923,#39924,#39925,#39926,#39927,#39928,#39929,#39930,#39931,
#39932,#39933,#39934,#39935,#39936,#39937,#39938,#39939,#39940,#39941,#39942,
#39943,#39944,#39945,#39946,#39947,#39948,#39949,#39950,#39951,#39952,#39953,
#39954,#39955,#39956,#39957,#39958,#39959,#39960,#39961,#39962,#39963,#39964,
#39965,#39966,#39967,#39968,#39969,#39970,#39971,#39972,#39973,#39974,#39975,
#39976,#39977,#39978,#39979,#39980,#39981,#39982,#39983,#39984,#39985,#39986,
#39987,#39988,#39989,#39990,#39991,#39992,#39993,#39994,#39995,#39996,#39997,
#39998,#39999,#40000,#40001,#40002,#40003,#40004,#40005,#40006,#40007,#40008,
#40009,#40010,#40011,#40012,#40013,#40014,#40015,#40016,#40017,#40018,#40019,
#40020,#40021,#40022,#40023,#40024,#40025,#40026,#40027,#40028,#40029,#40030,
#40031,#40032,#40033,#40034,#40035,#40036,#40037,#40038,#40039,#40040,#40041,
#40042,#40043,#40044,#40045,#40046,#40047,#40048,#40049,#40050,#40051,#40052,
#40053,#40054,#40055,#40056,#40057,#40058,#40059,#40060,#40061,#40062,#40063,
#40064,#40065,#40066,#40067,#40068,#40069,#40070,#40071,#40072,#40073,#40074,
#40075,#40076,#40077,#40078,#40079,#40080,#40081,#40082,#40083,#40084,#40085,
#40086,#40087,#40088,#40089,#40090,#40091,#40092,#40093,#40094,#40095,#40096,
#40097,#40098,#40099,#40100,#40101,#40102,#40103,#40104,#40105),
 .UNSPECIFIED.,.F.,.F.,(4,2,2,2,2,2,2,2,2,2,2,2,2,2,2,2,2,2,2,2,2,2,2,2,
2,2,2,2,2,2,2,2,2,2,2,2,2,2,2,2,2,2,2,2,2,2,2,2,2,2,2,2,2,2,2,2,2,2,2,2,
2,2,2,2,2,2,2,2,2,2,2,2,2,2,2,2,2,2,2,2,2,2,2,2,2,2,2,2,2,2,2,2,2,2,4),
(-0.973880464698564,-0.972269911093484,-0.969457378845782,-0.968091411426718,
-0.967020867405405,-0.96577714487014,-0.963551956960564,-0.952870471028589,
-0.928543279543384,-0.882387778249055,-0.875866516807864,-0.873348841111349,
-0.871531099753036,-0.869593431561668,-0.867006721865821,-0.861240473108374,
-0.837503321861841,-0.805408902237263,-0.779763040997667,-0.776947041813183,
-0.775580422480422,-0.774509861087641,-0.773266683782313,-0.771043858624368,
-0.760400345293145,-0.736222472933244,-0.689859125910439,-0.683351558937275,
-0.680836131057608,-0.679019024004365,-0.677081113987435,-0.674492499333955,
-0.668715352300812,-0.64489232770314,-0.612518230785388,-0.587253647670481,
-0.584440197257536,-0.583074112974796,-0.582003634870122,-0.580760169417441,
-0.578535884619285,-0.567867258045739,-0.543589536267181,-0.497370624181562,
-0.490854124820034,-0.488337326480139,-0.486519906768528,-0.484582292073066,
-0.481995155339175,-0.476225861051315,-0.452463280515828,-0.420277869357716,
-0.416501889836401,-0.394702732168843,-0.391925571083226,-0.390566707532061,
-0.389496856009609,-0.388248321095346,-0.386000598833899,-0.37493474536427,
-0.349041885940512,-0.305052298328393,-0.298418648747195,-0.295883577305447,
-0.294061405077351,-0.292126509122557,-0.289556322752951,-0.283880113573802,
-0.260836545559236,-0.235320547067467,-0.202177715473949,-0.199426441543799,
-0.198072752606125,-0.19702906937169,-0.195814034912246,-0.194510415399186,
-0.192500346305293,-0.188709621849118,-0.177852689857685,-0.123605809715138,
-0.10807550640261,-0.104233390007135,-0.102009954033067,-0.100102833316269,
-0.0977882547111115,-0.0934150861284736,-0.0633686667400292,-0.0132863794194273,
-0.00797944871388667,-0.0061591313381461,-0.00512003665360846,-0.00408773129344569,
-0.00302632206325726,-0.00169493168175966,-0.000563682644051655),
 .UNSPECIFIED.);
#1269=B_SPLINE_CURVE_WITH_KNOTS('',3,(#40106,#40107,#40108,#40109,#40110,
#40111,#40112,#40113,#40114,#40115,#40116,#40117,#40118,#40119,#40120,#40121,
#40122,#40123,#40124,#40125,#40126,#40127,#40128,#40129,#40130,#40131,#40132,
#40133,#40134,#40135,#40136,#40137,#40138,#40139,#40140,#40141,#40142,#40143,
#40144,#40145,#40146,#40147,#40148,#40149,#40150,#40151,#40152,#40153,#40154,
#40155,#40156,#40157,#40158,#40159,#40160,#40161,#40162,#40163,#40164,#40165,
#40166,#40167,#40168,#40169,#40170,#40171,#40172,#40173,#40174,#40175,#40176,
#40177,#40178,#40179,#40180,#40181,#40182,#40183,#40184,#40185),
 .UNSPECIFIED.,.F.,.F.,(4,2,2,2,2,2,2,2,2,2,2,2,2,2,2,2,2,2,2,2,2,2,2,2,
2,2,2,2,2,2,2,2,2,2,2,2,2,2,2,4),(-2.4313535774442,-2.42510807129326,-2.39735431592081,
-2.37085249543322,-2.34904123187566,-2.34352840192528,-2.34098866370796,
-2.33905874223842,-2.33722792421159,-2.33414261554579,-2.32583364557825,
-2.32481127129679,-2.27582979560085,-2.24834597515755,-2.24625271318251,
-2.24491477371547,-2.24367413235542,-2.24366896022422,-2.24366374095101,
-2.24365847351217,-2.24365315693452,-2.24364779010072,-2.24364237193938,
-2.24363690125186,-2.24363137687909,-2.24362579761802,-2.2436201623626,
-2.24361446970691,-2.2436087184551,-2.24360290725867,-2.24359703462071,
-2.24359109923169,-2.24358509947373,-2.24357903387616,-2.24357290098285,
-2.24253144952348,-2.24115684924962,-2.23845773220675,-2.20560943320674,
-2.18935248187665),.UNSPECIFIED.);
#1270=B_SPLINE_CURVE_WITH_KNOTS('',3,(#40186,#40187,#40188,#40189,#40190,
#40191,#40192,#40193,#40194,#40195,#40196,#40197,#40198,#40199,#40200,#40201,
#40202,#40203,#40204,#40205,#40206,#40207,#40208,#40209,#40210,#40211,#40212,
#40213,#40214,#40215,#40216,#40217,#40218,#40219,#40220,#40221,#40222,#40223,
#40224,#40225,#40226,#40227,#40228,#40229,#40230,#40231,#40232,#40233,#40234,
#40235,#40236,#40237,#40238,#40239,#40240,#40241,#40242,#40243,#40244,#40245,
#40246,#40247,#40248,#40249,#40250,#40251,#40252,#40253,#40254,#40255,#40256,
#40257,#40258,#40259,#40260,#40261,#40262,#40263,#40264,#40265,#40266,#40267,
#40268,#40269,#40270,#40271,#40272,#40273,#40274,#40275,#40276,#40277,#40278,
#40279,#40280,#40281,#40282,#40283,#40284,#40285,#40286,#40287,#40288,#40289,
#40290,#40291,#40292,#40293,#40294,#40295,#40296,#40297,#40298,#40299,#40300,
#40301,#40302,#40303,#40304,#40305,#40306,#40307,#40308,#40309,#40310,#40311,
#40312,#40313,#40314,#40315,#40316,#40317,#40318,#40319,#40320,#40321,#40322,
#40323,#40324,#40325,#40326,#40327,#40328,#40329,#40330,#40331,#40332,#40333,
#40334,#40335,#40336,#40337,#40338,#40339,#40340,#40341,#40342,#40343,#40344,
#40345,#40346,#40347,#40348,#40349,#40350,#40351,#40352,#40353,#40354,#40355,
#40356,#40357,#40358,#40359,#40360,#40361,#40362,#40363,#40364,#40365,#40366,
#40367,#40368,#40369,#40370,#40371,#40372,#40373,#40374,#40375,#40376,#40377,
#40378,#40379,#40380,#40381,#40382,#40383,#40384,#40385,#40386,#40387,#40388,
#40389,#40390,#40391,#40392,#40393,#40394,#40395,#40396,#40397,#40398,#40399,
#40400,#40401,#40402,#40403,#40404,#40405,#40406,#40407,#40408,#40409,#40410,
#40411,#40412,#40413),.UNSPECIFIED.,.F.,.F.,(4,2,2,2,2,2,2,2,2,2,2,2,2,
2,2,2,2,2,2,2,2,2,2,2,2,2,2,2,2,2,2,2,2,2,2,2,2,2,2,2,2,2,2,2,2,2,2,2,2,
2,2,2,2,2,2,2,2,2,2,2,2,2,2,2,2,2,2,2,2,2,2,2,2,2,2,2,2,2,2,2,2,2,2,2,2,
2,2,2,2,2,2,2,2,2,2,2,2,2,2,2,2,2,2,2,2,2,2,2,2,2,2,2,2,4),(-1.45811225063465,
-1.44170082180132,-1.43618582134325,-1.43364528846694,-1.43171484819826,
-1.42988360138484,-1.42679772386231,-1.41848826947098,-1.4165222193944,
-1.36594710220237,-1.34827985806994,-1.33948849992986,-1.33739143884113,
-1.33617592121108,-1.33510087351288,-1.33371433877708,-1.33140938767511,
-1.3169826198997,-1.31323902374403,-1.30961068878169,-1.26511237152881,
-1.24656587566988,-1.24265254902188,-1.24043611814186,-1.23872004850519,
-1.23647768428818,-1.23255374644359,-1.21593802447899,-1.1793488152984,
-1.16009498377915,-1.14762034011282,-1.145408571095,-1.14403499457011,-1.14296386468914,
-1.14172559042497,-1.13952504904511,-1.12923985212111,-1.10644047917935,
-1.05807986143029,-1.05172470419247,-1.04923426983626,-1.04742372312006,
-1.04548203791393,-1.04286963059341,-1.03695912812163,-1.0120807065289,
-0.975526007447791,-0.968861951198427,-0.955222582590498,-0.952952885198095,
-0.951576775429746,-0.950503058319238,-0.949281334180986,-0.947155945638413,
-0.937980459394101,-0.889391010616536,-0.862543504115506,-0.858502987268429,
-0.85604041671282,-0.854115196466913,-0.852012530416708,-0.848615230141997,
-0.836802501174192,-0.787514522134391,-0.763146661402301,-0.760340605634563,
-0.758976008164643,-0.757905686150994,-0.756661244654995,-0.754432367584388,
-0.743686675979851,-0.719102034132714,-0.67331664825625,-0.666773868535854,
-0.664252939054944,-0.662434474839119,-0.66049754325791,-0.657914408952143,
-0.652166987107334,-0.628573976464478,-0.603490708992825,-0.570577345053661,
-0.567821288068995,-0.566466641813923,-0.565397126535096,-0.564145532806228,
-0.561883656827096,-0.550569161633893,-0.501003570372116,-0.47734334827208,
-0.473396000960714,-0.470934706787354,-0.469015036185457,-0.466890639150764,
-0.463394936107679,-0.450546324335389,-0.400426224341905,-0.37809074440209,
-0.375302693741566,-0.373941669709287,-0.372871649728039,-0.37162468239229,
-0.369384164216112,-0.358441940004316,-0.333061062736163,-0.288376260763831,
-0.281774636441631,-0.279244502087781,-0.27742363244446,-0.275488048658781,
-0.272913409092824,-0.267212729661355,-0.243981066307571,-0.242694324494143),
 .UNSPECIFIED.);
#1271=B_SPLINE_CURVE_WITH_KNOTS('',3,(#40418,#40419,#40420,#40421,#40422,
#40423,#40424,#40425,#40426,#40427,#40428,#40429,#40430,#40431,#40432,#40433,
#40434,#40435,#40436,#40437,#40438,#40439,#40440,#40441,#40442,#40443,#40444,
#40445,#40446,#40447,#40448,#40449,#40450,#40451,#40452,#40453,#40454,#40455,
#40456,#40457,#40458,#40459,#40460,#40461,#40462,#40463,#40464,#40465,#40466,
#40467,#40468,#40469,#40470,#40471,#40472,#40473,#40474,#40475,#40476,#40477,
#40478,#40479,#40480,#40481,#40482,#40483,#40484,#40485,#40486,#40487,#40488,
#40489,#40490,#40491,#40492,#40493,#40494,#40495,#40496,#40497,#40498,#40499,
#40500,#40501,#40502,#40503,#40504,#40505,#40506,#40507,#40508,#40509,#40510,
#40511,#40512,#40513,#40514,#40515,#40516,#40517,#40518,#40519,#40520,#40521,
#40522,#40523,#40524,#40525,#40526,#40527,#40528,#40529,#40530,#40531,#40532,
#40533,#40534,#40535,#40536,#40537,#40538,#40539,#40540,#40541,#40542,#40543,
#40544,#40545,#40546,#40547,#40548,#40549,#40550,#40551,#40552,#40553,#40554,
#40555,#40556,#40557,#40558,#40559,#40560,#40561,#40562,#40563,#40564,#40565,
#40566,#40567,#40568,#40569,#40570,#40571,#40572,#40573,#40574,#40575,#40576,
#40577,#40578,#40579,#40580,#40581,#40582,#40583,#40584,#40585,#40586,#40587,
#40588,#40589,#40590,#40591,#40592,#40593,#40594,#40595,#40596,#40597,#40598,
#40599,#40600,#40601,#40602,#40603,#40604,#40605,#40606,#40607,#40608,#40609,
#40610,#40611,#40612,#40613,#40614,#40615,#40616,#40617,#40618,#40619,#40620,
#40621,#40622,#40623,#40624,#40625,#40626,#40627,#40628,#40629,#40630,#40631,
#40632,#40633),.UNSPECIFIED.,.F.,.F.,(4,2,2,2,2,2,2,2,2,2,2,2,2,2,2,2,2,
2,2,2,2,2,2,2,2,2,2,2,2,2,2,2,2,2,2,2,2,2,2,2,2,2,2,2,2,2,2,2,2,2,2,2,2,
2,2,2,2,2,2,2,2,2,2,2,2,2,2,2,2,2,2,2,2,2,2,2,2,2,2,2,2,2,2,2,2,2,2,2,2,
2,2,2,2,2,2,2,2,2,2,2,2,2,2,2,2,2,2,4),(-2.18940658193359,-2.16144257327339,
-2.13712099329524,-2.12644165044395,-2.12421662887569,-2.12297297834277,
-2.1219024780941,-2.12053655223453,-2.11772404374133,-2.0925695938446,-2.06014355461465,
-2.03630392865665,-2.03052412119434,-2.02793495096009,-2.02599687479963,
-2.02417978858807,-2.02166466999551,-2.01515955612574,-1.96870351955098,
-1.94455905100501,-1.93392429751389,-1.93170188152769,-1.9304587522863,
-1.92938811365604,-1.92802125155263,-1.92520425142244,-1.89935050708435,
-1.8703445606534,-1.84420648875698,-1.83813988678378,-1.83549970273249,
-1.8335530958362,-1.83174912232173,-1.82928508310506,-1.8230881048389,-1.77299492340303,
-1.75448464401906,-1.74160149573924,-1.73925804394325,-1.73798866066294,
-1.73692021949006,-1.73558742889287,-1.73351017519861,-1.72335655509252,
-1.68067243928948,-1.6490806007065,-1.64466924860686,-1.64234623579676,
-1.64043817531106,-1.63822046295688,-1.63440514597119,-1.61924535681772,
-1.61150245729804,-1.57361820968498,-1.55702718568849,-1.54858416943477,
-1.5465139282218,-1.54530423929898,-1.5442276986449,-1.54283061388871,-1.54048996215428,
-1.52516330792117,-1.51783757855562,-1.46768342936896,-1.4548923192832,
-1.45140132442633,-1.44927764382689,-1.44735723351125,-1.44489305927805,
-1.44093713374117,-1.41702272421784,-1.38100908984842,-1.36446838835635,
-1.35604213761666,-1.35397328633343,-1.35276393683969,-1.35168737320398,
-1.35028983644486,-1.34794753345849,-1.33257510891003,-1.2918535263551,
-1.27319073354756,-1.2620639423948,-1.25873635117821,-1.25664875288808,
-1.25471828327463,-1.25222237371355,-1.24806930345205,-1.21578564165102,
-1.19326211510147,-1.16479918968955,-1.16198137568129,-1.16061433404227,
-1.15954366092882,-1.15830060481519,-1.15607861145084,-1.14545084611257,
-1.12133637463227,-1.07487668668413,-1.06837469763743,-1.06586004743169,
-1.0640430517866,-1.06210484214885,-1.05951510558615,-1.05373241602226,
-1.0298677757197,-0.997378655514071,-0.973880464698564),.UNSPECIFIED.);
#1272=B_SPLINE_CURVE_WITH_KNOTS('',3,(#40635,#40636,#40637,#40638,#40639,
#40640,#40641,#40642,#40643,#40644,#40645,#40646,#40647,#40648,#40649,#40650,
#40651,#40652,#40653,#40654,#40655,#40656,#40657,#40658,#40659,#40660,#40661,
#40662,#40663,#40664,#40665,#40666,#40667,#40668,#40669,#40670,#40671,#40672,
#40673,#40674,#40675,#40676,#40677,#40678,#40679,#40680,#40681,#40682,#40683,
#40684,#40685,#40686,#40687,#40688,#40689,#40690,#40691,#40692,#40693,#40694,
#40695,#40696),.UNSPECIFIED.,.F.,.F.,(4,2,2,2,2,2,2,2,2,2,2,2,2,2,2,2,2,
2,2,2,2,2,2,2,2,2,2,2,2,2,4),(-0.242694324494143,-0.218605650932494,-0.185552121754827,
-0.182797511274354,-0.181443159544478,-0.180406009161524,-0.180400810290624,
-0.180395681461162,-0.180390621373856,-0.180385628707869,-0.180380702107863,
-0.180375840415643,-0.18037104225267,-0.180366306480232,-0.180361631974136,
-0.180357017665444,-0.179123693304752,-0.177796221260034,-0.175728472628226,
-0.1717832401797,-0.161960968930813,-0.115026663723998,-0.103806571378454,
-0.0910204854260511,-0.087380530540636,-0.0852242461373569,-0.0835019252520926,
-0.0811862994677313,-0.0768084010236629,-0.0465816149829859,-0.000564402028610045),
 .UNSPECIFIED.);
#1273=B_SPLINE_CURVE_WITH_KNOTS('',3,(#40697,#40698,#40699,#40700,#40701,
#40702,#40703,#40704,#40705,#40706,#40707,#40708,#40709,#40710,#40711,#40712,
#40713,#40714,#40715,#40716,#40717,#40718,#40719,#40720,#40721,#40722,#40723,
#40724,#40725,#40726,#40727,#40728,#40729,#40730,#40731,#40732,#40733,#40734,
#40735,#40736,#40737,#40738,#40739,#40740,#40741,#40742,#40743,#40744,#40745,
#40746,#40747,#40748,#40749,#40750,#40751,#40752,#40753,#40754,#40755,#40756,
#40757,#40758,#40759,#40760,#40761,#40762,#40763,#40764,#40765,#40766,#40767,
#40768,#40769,#40770,#40771,#40772,#40773,#40774,#40775,#40776,#40777,#40778,
#40779,#40780,#40781,#40782,#40783,#40784,#40785,#40786,#40787,#40788,#40789,
#40790,#40791,#40792,#40793,#40794,#40795,#40796,#40797,#40798,#40799,#40800,
#40801,#40802,#40803,#40804,#40805,#40806,#40807,#40808,#40809,#40810,#40811,
#40812,#40813,#40814,#40815,#40816,#40817,#40818,#40819,#40820,#40821,#40822,
#40823,#40824,#40825,#40826,#40827,#40828,#40829,#40830,#40831,#40832,#40833,
#40834,#40835,#40836,#40837,#40838,#40839,#40840,#40841,#40842,#40843,#40844,
#40845,#40846,#40847,#40848,#40849,#40850,#40851,#40852,#40853,#40854,#40855,
#40856,#40857,#40858,#40859,#40860,#40861,#40862,#40863,#40864,#40865,#40866,
#40867,#40868,#40869,#40870,#40871,#40872,#40873,#40874,#40875,#40876,#40877,
#40878,#40879,#40880,#40881,#40882,#40883,#40884,#40885,#40886,#40887,#40888,
#40889,#40890),.UNSPECIFIED.,.F.,.F.,(4,2,2,2,2,2,2,2,2,2,2,2,2,2,2,2,2,
2,2,2,2,2,2,2,2,2,2,2,2,2,2,2,2,2,2,2,2,2,2,2,2,2,2,2,2,2,2,2,2,2,2,2,2,
2,2,2,2,2,2,2,2,2,2,2,2,2,2,2,2,2,2,2,2,2,2,2,2,2,2,2,2,2,2,2,2,2,2,2,2,
2,2,2,2,2,2,2,4),(-2.4317062866866,-2.42631946932063,-2.42284242681522,
-2.42138712823313,-2.42030635631367,-2.41929078546131,-2.41827619804741,
-2.41658068528834,-2.412131014088,-2.4042631093833,-2.35755483301902,-2.33076585912172,
-2.32648682003991,-2.32419183435477,-2.32230310789888,-2.32006893514292,
-2.31618089233947,-2.30006479595078,-2.29414997942651,-2.25400673339955,
-2.23851616165929,-2.2331462770639,-2.2305711188579,-2.22848372097956,-2.22728189948522,
-2.2272783209793,-2.22727472446683,-2.22727111019277,-2.22726707779843,
-2.22726295734438,-2.22627413439945,-2.2249248760073,-2.22219608205174,
-2.20297217965708,-2.16689246046896,-2.14785413817739,-2.13657261230876,
-2.13322903487839,-2.1311380516908,-2.12920896144971,-2.12672115297072,
-2.12259531964831,-2.09204332782668,-2.06523540897104,-2.04143514287707,
-2.0371183630271,-2.03549492471133,-2.03438335856718,-2.03338376108912,
-2.03176742393232,-2.02780017460041,-1.98463327652318,-1.94618210521712,
-1.94165667913121,-1.93931021770443,-1.93740119453352,-1.93520279048105,
-1.93147034085856,-1.91724937590887,-1.90784956577158,-1.85723685355633,
-1.84582687396493,-1.84355937852569,-1.84230645713313,-1.8412368955595,
-1.8398835907454,-1.83713483704096,-1.80394389373345,-1.77834739718764,
-1.75543209513847,-1.74977179704114,-1.74720425223577,-1.74526949748954,
-1.74344609704551,-1.74090712924979,-1.73424975188637,-1.69074788332287,
-1.66445024573998,-1.65328764777817,-1.65103403222151,-1.64978408218889,
-1.64871416178508,-1.64735668774601,-1.64458723953504,-1.62351387319986,
-1.57412066204767,-1.55955581103137,-1.55591398846505,-1.55375701717094,
-1.55184296172285,-1.54943621994816,-1.5456694924275,-1.52595351827851,
-1.4842401133961,-1.46343816530266,-1.4594035702923,-1.45835777854406),
 .UNSPECIFIED.);
#1274=B_SPLINE_CURVE_WITH_KNOTS('',3,(#40896,#40897,#40898,#40899,#40900,
#40901,#40902,#40903,#40904,#40905,#40906,#40907,#40908,#40909,#40910,#40911,
#40912,#40913,#40914,#40915,#40916,#40917,#40918,#40919,#40920,#40921,#40922,
#40923,#40924,#40925,#40926,#40927,#40928,#40929,#40930,#40931,#40932,#40933,
#40934,#40935,#40936,#40937,#40938,#40939,#40940,#40941,#40942,#40943,#40944,
#40945,#40946,#40947,#40948,#40949,#40950,#40951,#40952,#40953,#40954,#40955,
#40956,#40957,#40958,#40959,#40960,#40961,#40962,#40963,#40964,#40965,#40966,
#40967,#40968,#40969,#40970,#40971,#40972,#40973,#40974,#40975,#40976,#40977,
#40978,#40979,#40980,#40981,#40982,#40983,#40984,#40985,#40986,#40987,#40988,
#40989,#40990,#40991,#40992,#40993,#40994,#40995,#40996,#40997,#40998,#40999,
#41000,#41001,#41002,#41003,#41004,#41005,#41006,#41007,#41008,#41009,#41010,
#41011,#41012,#41013,#41014,#41015,#41016,#41017,#41018,#41019,#41020,#41021,
#41022,#41023,#41024,#41025,#41026,#41027,#41028,#41029,#41030,#41031,#41032,
#41033,#41034,#41035,#41036,#41037,#41038,#41039,#41040,#41041,#41042,#41043,
#41044,#41045,#41046,#41047,#41048,#41049,#41050,#41051,#41052,#41053,#41054,
#41055,#41056,#41057,#41058,#41059,#41060,#41061,#41062,#41063,#41064,#41065,
#41066,#41067,#41068,#41069,#41070,#41071),.UNSPECIFIED.,.F.,.F.,(4,2,2,
2,2,2,2,2,2,2,2,2,2,2,2,2,2,2,2,2,2,2,2,2,2,2,2,2,2,2,2,2,2,2,2,2,2,2,2,
2,2,2,2,2,2,2,2,2,2,2,2,2,2,2,2,2,2,2,2,2,2,2,2,2,2,2,2,2,2,2,2,2,2,2,2,
2,2,2,2,2,2,2,2,2,2,2,2,4),(-0.973977657370886,-0.973066225395767,-0.96462553205897,
-0.949890383429859,-0.946108799913681,-0.943898938423955,-0.941990547568084,
-0.939658230341248,-0.93520175623725,-0.901423061709051,-0.864052893434362,
-0.851119013078597,-0.848884067143519,-0.847503440760412,-0.846431544150649,
-0.845197744158303,-0.843018001083116,-0.833057749166896,-0.811456952073632,
-0.761268981829781,-0.755085959307637,-0.752624381878774,-0.75082112682837,
-0.748874263048361,-0.746231906474935,-0.740152187499536,-0.685673665951278,
-0.65907084035136,-0.656250944266086,-0.654883472690943,-0.65381273992442,
-0.652569931773576,-0.650349158675844,-0.639742052545,-0.615709127911285,
-0.569131526530966,-0.562637200983748,-0.560123747126126,-0.558307036457941,
-0.556368592141944,-0.553777612379373,-0.547988227727931,-0.524071730661645,
-0.491451887208981,-0.466531110152501,-0.463719962171692,-0.462354248606782,
-0.461283703094992,-0.460039749030071,-0.457813582313128,-0.447116515032338,
-0.422727974885078,-0.376658171476533,-0.370130551098277,-0.367611826710242,
-0.365793782987993,-0.363856214310271,-0.361270363610149,-0.355509076252417,
-0.331811084214977,-0.299860253176341,-0.274023829522888,-0.271206733979273,
-0.269839878994731,-0.268769274689338,-0.267526209836558,-0.265303983616606,
-0.254670951810799,-0.230534782273424,-0.184107317859786,-0.177605661939579,
-0.175091146612725,-0.173274250402615,-0.171388887920209,-0.168909579784115,
-0.166151510114064,-0.161541700153478,-0.152000034598465,-0.124139661679705,
-0.0836544184238998,-0.0794162098931193,-0.0777545015696333,-0.076746390053646,
-0.0756434506032181,-0.0740634455314549,-0.0700327318928364,-0.0492720935334833,
-0.000564379274226552),.UNSPECIFIED.);
#1275=B_SPLINE_CURVE_WITH_KNOTS('',3,(#41072,#41073,#41074,#41075,#41076,
#41077,#41078,#41079,#41080,#41081,#41082,#41083,#41084,#41085,#41086,#41087,
#41088,#41089,#41090,#41091,#41092,#41093,#41094,#41095,#41096,#41097,#41098,
#41099,#41100,#41101,#41102,#41103,#41104,#41105,#41106,#41107,#41108,#41109,
#41110,#41111,#41112,#41113,#41114,#41115,#41116,#41117,#41118,#41119,#41120,
#41121,#41122,#41123,#41124,#41125,#41126,#41127,#41128,#41129,#41130,#41131),
 .UNSPECIFIED.,.F.,.F.,(4,2,2,2,2,2,2,2,2,2,2,2,2,2,2,2,2,2,2,2,2,2,2,2,
2,2,2,2,2,4),(-2.43155191913647,-2.42280426928896,-2.41717915570413,-2.41472977602384,
-2.4128483970087,-2.4110144659602,-2.40919597385053,-2.40667538762493,-2.4001357854956,
-2.38765704245933,-2.34967338981676,-2.32867441764294,-2.31888358202122,
-2.31671515539217,-2.31548388580663,-2.31441167645972,-2.31302736228571,
-2.31078000750653,-2.29758812567188,-2.2901962096612,-2.24000035791993,
-2.23033265395902,-2.22567929295,-2.22290341575571,-2.22039871392486,-2.21849988363351,
-2.21668231804465,-2.21416509433217,-2.20764625756361,-2.18940658193359),
 .UNSPECIFIED.);
#1276=B_SPLINE_CURVE_WITH_KNOTS('',3,(#41132,#41133,#41134,#41135,#41136,
#41137,#41138,#41139,#41140,#41141,#41142,#41143,#41144,#41145,#41146,#41147,
#41148,#41149,#41150,#41151,#41152,#41153,#41154,#41155,#41156,#41157,#41158,
#41159,#41160,#41161,#41162,#41163,#41164,#41165,#41166,#41167,#41168,#41169,
#41170,#41171,#41172,#41173,#41174,#41175,#41176,#41177,#41178,#41179,#41180,
#41181,#41182,#41183,#41184,#41185,#41186,#41187,#41188,#41189,#41190,#41191,
#41192,#41193,#41194,#41195,#41196,#41197,#41198,#41199,#41200,#41201,#41202,
#41203,#41204,#41205,#41206,#41207,#41208,#41209,#41210,#41211,#41212,#41213,
#41214,#41215,#41216,#41217,#41218,#41219,#41220,#41221,#41222,#41223,#41224,
#41225,#41226,#41227,#41228,#41229,#41230,#41231,#41232,#41233,#41234,#41235,
#41236,#41237,#41238,#41239,#41240,#41241,#41242,#41243,#41244,#41245,#41246,
#41247,#41248,#41249,#41250,#41251,#41252,#41253,#41254,#41255,#41256,#41257,
#41258,#41259,#41260,#41261,#41262,#41263,#41264,#41265,#41266,#41267,#41268,
#41269,#41270,#41271,#41272,#41273,#41274,#41275,#41276,#41277,#41278,#41279,
#41280,#41281,#41282,#41283,#41284,#41285,#41286,#41287,#41288,#41289,#41290,
#41291,#41292,#41293,#41294,#41295,#41296,#41297,#41298,#41299,#41300,#41301,
#41302,#41303,#41304,#41305,#41306,#41307,#41308,#41309,#41310,#41311,#41312,
#41313,#41314,#41315,#41316,#41317,#41318,#41319,#41320,#41321,#41322,#41323,
#41324,#41325,#41326,#41327,#41328,#41329,#41330,#41331,#41332,#41333,#41334,
#41335,#41336,#41337,#41338,#41339,#41340,#41341,#41342,#41343,#41344,#41345,
#41346,#41347,#41348,#41349),.UNSPECIFIED.,.F.,.F.,(4,2,2,2,2,2,2,2,2,2,
2,2,2,2,2,2,2,2,2,2,2,2,2,2,2,2,2,2,2,2,2,2,2,2,2,2,2,2,2,2,2,2,2,2,2,2,
2,2,2,2,2,2,2,2,2,2,2,2,2,2,2,2,2,2,2,2,2,2,2,2,2,2,2,2,2,2,2,2,2,2,2,2,
2,2,2,2,2,2,2,2,2,2,2,2,2,2,2,2,2,2,2,2,2,2,2,2,2,2,4),(-1.45835777854406,
-1.45782292134003,-1.45671982849219,-1.45571180378477,-1.45405068696945,
-1.44981633975645,-1.40941409136322,-1.38151665039056,-1.36702465517826,
-1.36338856292279,-1.36123282708679,-1.35931853250336,-1.35690970377132,
-1.35313623226168,-1.33328607259331,-1.2916715978068,-1.27091053315857,
-1.26687992104755,-1.2652998732437,-1.26419688058157,-1.26318870015759,
-1.26152684151105,-1.25728805457661,-1.21645982195293,-1.17610577553567,
-1.17199274716033,-1.16950859901695,-1.16757995187486,-1.1654870523497,
-1.16213518611104,-1.15077524554465,-1.13154304754217,-1.1093393364444,
-1.07653295911687,-1.07377260196959,-1.07241697662387,-1.0713472429167,
-1.07009603487008,-1.06783646579505,-1.05656721586208,-1.00750575847676,
-0.983309320391648,-0.979345735708968,-0.976879356296229,-0.974958817363028,
-0.972836611528421,-0.969351756039008,-0.956625709477781,-0.906395563822677,
-0.899001585570265,-0.883708004291678,-0.881368651676051,-0.879972002196811,
-0.878895586663093,-0.877685788952901,-0.875614827186638,-0.867161218921143,
-0.850539790563458,-0.81262176389978,-0.805139220166297,-0.78985891896541,
-0.78603554928505,-0.783816063930652,-0.781908216251608,-0.779587630864457,
-0.775187516610344,-0.744082816337828,-0.699986725742051,-0.690597403163341,
-0.688376255545713,-0.687119929725613,-0.686050573033518,-0.684701493744927,
-0.681974206919407,-0.652315578287309,-0.600933311411062,-0.594876274383381,
-0.592438712173165,-0.590641471414158,-0.58868996983462,-0.586021344200863,
-0.579790268987491,-0.55227256029989,-0.532096881767296,-0.498876658231994,
-0.496127792706804,-0.494774448438069,-0.493704865817538,-0.492451924507258,
-0.490184417884345,-0.478774147393955,-0.428145293785074,-0.405566535049798,
-0.401655738212274,-0.399205269930749,-0.397286622876708,-0.395155746347279,
-0.391631723900853,-0.378471888084394,-0.328593100266154,-0.319666177026502,
-0.30594849068588,-0.303673254608417,-0.302295404604407,-0.301221344249222,
-0.300000385996226,-0.297878987119962,-0.288761531407757,-0.242729697819112),
 .UNSPECIFIED.);
#1277=B_SPLINE_CURVE_WITH_KNOTS('',3,(#41354,#41355,#41356,#41357,#41358,
#41359,#41360,#41361,#41362,#41363,#41364,#41365,#41366,#41367,#41368,#41369,
#41370,#41371,#41372,#41373,#41374,#41375,#41376,#41377,#41378,#41379,#41380,
#41381,#41382,#41383,#41384,#41385,#41386,#41387,#41388,#41389,#41390,#41391,
#41392,#41393,#41394,#41395,#41396,#41397,#41398,#41399,#41400,#41401,#41402,
#41403,#41404,#41405,#41406,#41407,#41408,#41409,#41410,#41411,#41412,#41413,
#41414,#41415,#41416,#41417,#41418,#41419,#41420,#41421,#41422,#41423,#41424,
#41425,#41426,#41427,#41428,#41429,#41430,#41431,#41432,#41433,#41434,#41435,
#41436,#41437,#41438,#41439,#41440,#41441,#41442,#41443,#41444,#41445,#41446,
#41447,#41448,#41449,#41450,#41451,#41452,#41453,#41454,#41455,#41456,#41457,
#41458,#41459,#41460,#41461,#41462,#41463,#41464,#41465,#41466,#41467,#41468,
#41469,#41470,#41471,#41472,#41473,#41474,#41475,#41476,#41477,#41478,#41479,
#41480,#41481,#41482,#41483,#41484,#41485,#41486,#41487,#41488,#41489,#41490,
#41491,#41492,#41493,#41494,#41495,#41496,#41497,#41498,#41499,#41500,#41501,
#41502,#41503,#41504,#41505,#41506,#41507,#41508,#41509,#41510,#41511,#41512,
#41513,#41514,#41515,#41516,#41517,#41518,#41519,#41520,#41521,#41522,#41523,
#41524,#41525,#41526,#41527,#41528,#41529,#41530,#41531,#41532,#41533,#41534,
#41535,#41536,#41537,#41538,#41539,#41540,#41541,#41542,#41543,#41544,#41545,
#41546,#41547,#41548,#41549,#41550,#41551,#41552,#41553,#41554,#41555,#41556,
#41557,#41558,#41559,#41560,#41561),.UNSPECIFIED.,.F.,.F.,(4,2,2,2,2,2,
2,2,2,2,2,2,2,2,2,2,2,2,2,2,2,2,2,2,2,2,2,2,2,2,2,2,2,2,2,2,2,2,2,2,2,2,
2,2,2,2,2,2,2,2,2,2,2,2,2,2,2,2,2,2,2,2,2,2,2,2,2,2,2,2,2,2,2,2,2,2,2,2,
2,2,2,2,2,2,2,2,2,2,2,2,2,2,2,2,2,2,2,2,2,2,2,2,2,4),(-2.18956623962693,
-2.18041265317692,-2.13479112283698,-2.11558000051423,-2.10806267563156,
-2.10249362892436,-2.09991061012686,-2.09797378248252,-2.09615542362863,
-2.09363465227258,-2.08709241093975,-2.04127798422216,-2.01668662835424,
-2.00593999991555,-2.00371111203506,-2.00246670807316,-2.0013964405585,
-2.00003195016963,-1.99722622749472,-1.97285484915736,-1.92360185617187,
-1.91179798530528,-1.90840165225533,-1.90629924087623,-1.90437402379684,
-1.90191113941125,-1.89786939745731,-1.87097988132194,-1.82227944897952,
-1.81320701320005,-1.81108907851394,-1.80986899017584,-1.80879493893445,
-1.80741614584906,-1.80513739766206,-1.7913846509769,-1.78245491750448,
-1.73248156176817,-1.71948358905235,-1.71597432518676,-1.71384687906953,
-1.71192779210242,-1.70947187810071,-1.70554249779532,-1.68249449319403,
-1.6323005931622,-1.62092793367482,-1.61866262219051,-1.61741022173571,
-1.61634068419027,-1.61498687122962,-1.61223532245761,-1.57918186518307,
-1.55384116306093,-1.53060519866613,-1.52490326666873,-1.52232822463779,
-1.52039240101882,-1.51857134679561,-1.51604102130604,-1.50943936924016,
-1.46469168750852,-1.43029296130569,-1.42682568940314,-1.42533842521348,
-1.42425221684062,-1.42307425013789,-1.42114633521858,-1.41500392814279,
-1.36095873132179,-1.33797549667318,-1.33230655794222,-1.32973757283408,
-1.32780273420643,-1.32597998967863,-1.32344311596424,-1.3167986002539,
-1.2729999316692,-1.24692916359499,-1.23582081263044,-1.23357045616619,
-1.23232128218876,-1.23125138826584,-1.22989312832399,-1.2277321321533,
-1.21620561414111,-1.16169534723097,-1.14295010261025,-1.1392392790364,
-1.13684979219599,-1.1349375347666,-1.13276982262447,-1.12907855463261,
-1.1138696923037,-1.05923312898293,-1.04382162424118,-1.04147786111809,
-1.04007993791724,-1.0390033692011,-1.03779432903114,-1.03572672259374,
-1.02731503206474,-1.01082014887421,-0.973977657370886),.UNSPECIFIED.);
#1278=B_SPLINE_CURVE_WITH_KNOTS('',3,(#41563,#41564,#41565,#41566,#41567,
#41568,#41569,#41570,#41571,#41572,#41573,#41574,#41575,#41576,#41577,#41578,
#41579,#41580,#41581,#41582,#41583,#41584,#41585,#41586,#41587,#41588,#41589,
#41590,#41591,#41592,#41593,#41594,#41595,#41596,#41597,#41598,#41599,#41600,
#41601,#41602,#41603,#41604,#41605,#41606,#41607,#41608,#41609,#41610,#41611,
#41612,#41613,#41614,#41615,#41616),.UNSPECIFIED.,.F.,.F.,(4,2,2,2,2,2,
2,2,2,2,2,2,2,2,2,2,2,2,2,2,2,2,2,2,2,2,4),(-0.242729697819112,-0.240116437798231,
-0.213250307360193,-0.209206621585435,-0.206742923171201,-0.204871176334209,
-0.202830447661773,-0.200707670511219,-0.197631835711563,-0.192234493795022,
-0.152249128627421,-0.116231805408894,-0.111837027572666,-0.11014999390269,
-0.109137008829852,-0.108038232994759,-0.106480058163093,-0.102587620031566,
-0.0832020359993201,-0.0292996200280103,-0.0187066474130954,-0.0153142652421365,
-0.0132125172705519,-0.0113620376163737,-0.00949737249079776,-0.00709833961708263,
-0.000563576427226659),.UNSPECIFIED.);
#1279=B_SPLINE_CURVE_WITH_KNOTS('',3,(#41617,#41618,#41619,#41620,#41621,
#41622,#41623,#41624,#41625,#41626,#41627,#41628,#41629,#41630,#41631,#41632,
#41633,#41634,#41635,#41636,#41637,#41638,#41639,#41640,#41641,#41642,#41643,
#41644,#41645,#41646,#41647,#41648,#41649,#41650,#41651,#41652,#41653,#41654,
#41655,#41656,#41657,#41658,#41659,#41660,#41661,#41662,#41663,#41664,#41665,
#41666,#41667,#41668,#41669,#41670,#41671,#41672,#41673,#41674,#41675,#41676,
#41677,#41678,#41679,#41680,#41681,#41682,#41683,#41684,#41685,#41686,#41687,
#41688,#41689,#41690,#41691,#41692,#41693,#41694,#41695,#41696,#41697,#41698,
#41699,#41700,#41701,#41702,#41703,#41704,#41705,#41706,#41707,#41708,#41709,
#41710,#41711,#41712,#41713,#41714,#41715,#41716,#41717,#41718,#41719,#41720,
#41721,#41722,#41723,#41724,#41725,#41726,#41727,#41728,#41729,#41730,#41731,
#41732,#41733,#41734,#41735,#41736,#41737,#41738,#41739,#41740,#41741,#41742,
#41743,#41744,#41745,#41746,#41747,#41748,#41749,#41750,#41751,#41752,#41753,
#41754,#41755,#41756,#41757,#41758,#41759,#41760,#41761,#41762,#41763,#41764,
#41765,#41766,#41767,#41768,#41769,#41770,#41771,#41772,#41773,#41774,#41775,
#41776,#41777,#41778,#41779,#41780,#41781,#41782,#41783,#41784,#41785,#41786,
#41787,#41788,#41789,#41790,#41791,#41792),.UNSPECIFIED.,.F.,.F.,(4,2,2,
2,2,2,2,2,2,2,2,2,2,2,2,2,2,2,2,2,2,2,2,2,2,2,2,2,2,2,2,2,2,2,2,2,2,2,2,
2,2,2,2,2,2,2,2,2,2,2,2,2,2,2,2,2,2,2,2,2,2,2,2,2,2,2,2,2,2,2,2,2,2,2,2,
2,2,2,2,2,2,2,2,2,2,2,2,4),(-2.43098705841732,-2.37325618589629,-2.35138393235581,
-2.34875985260428,-2.34743194285922,-2.34646736735063,-2.3452364712295,
-2.34312480058049,-2.33501171342135,-2.27302956465628,-2.26259037357187,
-2.25767556453552,-2.25479368631527,-2.25228619365899,-2.25038948750831,
-2.24860670909135,-2.2457786052043,-2.23907951341181,-2.19696091665691,
-2.18432879521766,-2.16671728089558,-2.15794472848786,-2.15584958042758,
-2.15463474084651,-2.15356000158624,-2.15217348935786,-2.14986779371891,
-2.13540917988652,-2.13123953293945,-2.09601883338496,-2.07583864161764,
-2.06409693795727,-2.06070716390939,-2.05860642407425,-2.05668114419651,
-2.05421598368269,-2.05016581307431,-2.02329630499217,-1.97460122937902,
-1.96553340523322,-1.96341604761062,-1.96219621060087,-1.96112232655666,
-1.95974367908389,-1.95746502960675,-1.94363919822089,-1.93474313249465,
-1.88468173806665,-1.87180449230982,-1.86830651259571,-1.8661817859668,
-1.86426249635717,-1.86180263470978,-1.85785946586743,-1.834341149538,-1.7846128941192,
-1.77328309330995,-1.77102045824447,-1.76976876684499,-1.76869936167858,
-1.76734511062723,-1.76459068609666,-1.73166584694355,-1.70655132012922,
-1.68303418847249,-1.67729631933894,-1.67471501209352,-1.67277846273196,
-1.67095963252408,-1.66843703924917,-1.66188321649084,-1.61625853492399,
-1.59153190985087,-1.58075152837653,-1.57852062830689,-1.57727579023372,
-1.57620558036129,-1.57484172014555,-1.57203916236646,-1.54800005779068,
-1.49855239847719,-1.48662910198961,-1.48322097845794,-1.48111597163792,
-1.479191501112,-1.47673385895048,-1.47270984440081,-1.45772415786055),
 .UNSPECIFIED.);
#1280=B_SPLINE_CURVE_WITH_KNOTS('',3,(#41798,#41799,#41800,#41801,#41802,
#41803,#41804,#41805,#41806,#41807,#41808,#41809,#41810,#41811,#41812,#41813,
#41814,#41815,#41816,#41817,#41818,#41819,#41820,#41821,#41822,#41823,#41824,
#41825,#41826,#41827,#41828,#41829,#41830,#41831,#41832,#41833,#41834,#41835,
#41836,#41837,#41838,#41839,#41840,#41841,#41842,#41843,#41844,#41845,#41846,
#41847,#41848,#41849,#41850,#41851,#41852,#41853,#41854,#41855,#41856,#41857,
#41858,#41859,#41860,#41861,#41862,#41863,#41864,#41865,#41866,#41867,#41868,
#41869,#41870,#41871,#41872,#41873,#41874,#41875,#41876,#41877,#41878,#41879,
#41880,#41881,#41882,#41883,#41884,#41885,#41886,#41887,#41888,#41889,#41890,
#41891,#41892,#41893,#41894,#41895,#41896,#41897,#41898,#41899,#41900,#41901,
#41902,#41903,#41904,#41905,#41906,#41907,#41908,#41909,#41910,#41911,#41912,
#41913,#41914,#41915,#41916,#41917,#41918,#41919,#41920,#41921,#41922,#41923,
#41924,#41925,#41926,#41927,#41928,#41929,#41930,#41931,#41932,#41933,#41934,
#41935,#41936,#41937,#41938,#41939,#41940,#41941,#41942,#41943,#41944,#41945,
#41946,#41947,#41948,#41949,#41950,#41951,#41952,#41953,#41954,#41955,#41956,
#41957,#41958,#41959,#41960,#41961,#41962,#41963,#41964,#41965,#41966,#41967,
#41968,#41969,#41970,#41971,#41972,#41973,#41974,#41975,#41976,#41977,#41978,
#41979),.UNSPECIFIED.,.F.,.F.,(4,2,2,2,2,2,2,2,2,2,2,2,2,2,2,2,2,2,2,2,
2,2,2,2,2,2,2,2,2,2,2,2,2,2,2,2,2,2,2,2,2,2,2,2,2,2,2,2,2,2,2,2,2,2,2,2,
2,2,2,2,2,2,2,2,2,2,2,2,2,2,2,2,2,2,2,2,2,2,2,2,2,2,2,2,2,2,2,2,2,2,4),
(-0.97400982262004,-0.939077207573621,-0.923181086866272,-0.920592913881418,
-0.919255111714498,-0.918186661183434,-0.916921971078261,-0.914599507770575,
-0.902139044537373,-0.869753821135637,-0.830541542481921,-0.826400310588078,
-0.823908117647993,-0.821978531220479,-0.819889906012371,-0.816556386446665,
-0.805369159224853,-0.786555882087239,-0.745091495181054,-0.730596384167335,
-0.728288657443566,-0.726901365223826,-0.725826291228361,-0.724611365664025,
-0.722516746509033,-0.713755870225364,-0.696186004762857,-0.666729273318793,
-0.637976146905596,-0.633889137744435,-0.631412792417983,-0.629485492526718,
-0.6273893194661,-0.624021829572349,-0.612506891380457,-0.592891960217706,
-0.551826433120587,-0.538073516635675,-0.535794992344142,-0.534416253167552,
-0.533342189652874,-0.532122013407345,-0.530003774144425,-0.520927345024398,
-0.472255137139017,-0.445376108802911,-0.441334664061433,-0.438871769675417,
-0.436946441493308,-0.434843804970809,-0.431446879756632,-0.419638807746116,
-0.370357049030402,-0.345974416967848,-0.343168126153214,-0.341803450348783,
-0.340733084123659,-0.339488610814658,-0.337259724835709,-0.326514921370215,
-0.301934525120386,-0.256146755451947,-0.249599617232489,-0.247077940087878,
-0.245259234433548,-0.243322321543413,-0.240739686153191,-0.235184684216764,
-0.22768443090503,-0.208537529894372,-0.176131543099938,-0.169617438007437,
-0.153220540271922,-0.150613800178691,-0.149271979345731,-0.148203282914577,
-0.146941770713721,-0.145599792217739,-0.140316164913045,-0.117843485008567,
-0.0976712951451026,-0.0872716329576706,-0.0603973523829484,-0.0563558450857691,
-0.0538928630504517,-0.051967436578634,-0.0498646624896345,-0.0477046383277412,
-0.0445379818388593,-0.0338137111492761,-0.000563923203056516),
 .UNSPECIFIED.);
#1281=B_SPLINE_CURVE_WITH_KNOTS('',3,(#41980,#41981,#41982,#41983,#41984,
#41985,#41986,#41987,#41988,#41989,#41990,#41991,#41992,#41993,#41994,#41995,
#41996,#41997,#41998,#41999,#42000,#42001,#42002,#42003,#42004,#42005,#42006,
#42007,#42008,#42009,#42010,#42011,#42012,#42013,#42014,#42015,#42016,#42017,
#42018,#42019,#42020,#42021,#42022,#42023,#42024,#42025,#42026,#42027,#42028,
#42029,#42030,#42031,#42032,#42033,#42034,#42035),.UNSPECIFIED.,.F.,.F.,
(4,2,2,2,2,2,2,2,2,2,2,2,2,2,2,2,2,2,2,2,2,2,2,2,2,2,2,4),(-2.43140076039871,
-2.39440475956086,-2.39129067200828,-2.38954019459536,-2.38799018084422,
-2.38689320294571,-2.38587875790501,-2.38418299704171,-2.37972988241132,
-2.34792437241353,-2.32909866248134,-2.30836358721486,-2.29682048211597,
-2.29431824636313,-2.29197312934567,-2.29006450344343,-2.28786578274992,
-2.28413092789478,-2.26987859822957,-2.26054060536068,-2.20991829103546,
-2.19852196334369,-2.19629771777738,-2.1950285003781,-2.19396036929867,
-2.1926281795813,-2.19055224883826,-2.18956623962693),.UNSPECIFIED.);
#1282=B_SPLINE_CURVE_WITH_KNOTS('',3,(#42036,#42037,#42038,#42039,#42040,
#42041,#42042,#42043,#42044,#42045,#42046,#42047,#42048,#42049,#42050,#42051,
#42052,#42053,#42054,#42055,#42056,#42057,#42058,#42059,#42060,#42061,#42062,
#42063,#42064,#42065,#42066,#42067,#42068,#42069,#42070,#42071,#42072,#42073,
#42074,#42075,#42076,#42077,#42078,#42079,#42080,#42081,#42082,#42083,#42084,
#42085,#42086,#42087,#42088,#42089,#42090,#42091,#42092,#42093,#42094,#42095,
#42096,#42097,#42098,#42099,#42100,#42101,#42102,#42103,#42104,#42105,#42106,
#42107,#42108,#42109,#42110,#42111,#42112,#42113,#42114,#42115,#42116,#42117,
#42118,#42119,#42120,#42121,#42122,#42123,#42124,#42125,#42126,#42127,#42128,
#42129,#42130,#42131,#42132,#42133,#42134,#42135,#42136,#42137,#42138,#42139,
#42140,#42141,#42142,#42143,#42144,#42145,#42146,#42147,#42148,#42149,#42150,
#42151,#42152,#42153,#42154,#42155,#42156,#42157,#42158,#42159,#42160,#42161,
#42162,#42163,#42164,#42165,#42166,#42167,#42168,#42169,#42170,#42171,#42172,
#42173,#42174,#42175,#42176,#42177,#42178,#42179,#42180,#42181,#42182,#42183,
#42184,#42185,#42186,#42187,#42188,#42189,#42190,#42191,#42192,#42193,#42194,
#42195,#42196,#42197,#42198,#42199,#42200,#42201,#42202,#42203,#42204,#42205,
#42206,#42207,#42208,#42209,#42210,#42211,#42212,#42213,#42214,#42215,#42216,
#42217,#42218,#42219,#42220,#42221,#42222,#42223,#42224,#42225,#42226,#42227,
#42228,#42229,#42230,#42231,#42232,#42233,#42234,#42235,#42236,#42237,#42238,
#42239,#42240,#42241,#42242,#42243,#42244,#42245,#42246,#42247,#42248,#42249,
#42250,#42251),.UNSPECIFIED.,.F.,.F.,(4,2,2,2,2,2,2,2,2,2,2,2,2,2,2,2,2,
2,2,2,2,2,2,2,2,2,2,2,2,2,2,2,2,2,2,2,2,2,2,2,2,2,2,2,2,2,2,2,2,2,2,2,2,
2,2,2,2,2,2,2,2,2,2,2,2,2,2,2,2,2,2,2,2,2,2,2,2,2,2,2,2,2,2,2,2,2,2,2,2,
2,2,2,2,2,2,2,2,2,2,2,2,2,2,2,2,2,2,4),(-1.45772415786055,-1.44648434475585,
-1.43513039397568,-1.40967403196687,-1.39074676278327,-1.38690250508643,
-1.38535233027771,-1.38425527651423,-1.38324079143602,-1.38154502484505,
-1.37709224739574,-1.3449684202107,-1.31108999243359,-1.29486807041862,
-1.29110383623707,-1.28892025104236,-1.28701015439179,-1.28464439998024,
-1.28101018914932,-1.26346220473926,-1.2155886220444,-1.21093664919579,
-1.19636012794277,-1.19404918426374,-1.1926609905796,-1.19158585557495,
-1.1903715819739,-1.1882797105454,-1.17955374255117,-1.1315309774056,-1.1036593126324,
-1.09959323249244,-1.09712319924799,-1.09519700462702,-1.09309819062394,
-1.08971798837394,-1.07807494897275,-1.05814031916614,-1.04074491082258,
-1.00670630617543,-1.00227142637631,-1.00057839813368,-0.999564432201041,
-0.998466938314348,-0.996914481307998,-0.993056149466106,-0.973996176335221,
-0.948646457345167,-0.937299141324565,-0.911151612309999,-0.907129967764425,
-0.904672987294396,-0.902748572346378,-0.900643156020368,-0.897233322069521,
-0.885293358341514,-0.835797164451535,-0.81178497768871,-0.808982338963741,
-0.807618426931977,-0.806548173500303,-0.805303273309203,-0.803072247896647,
-0.792290346122666,-0.7675604210291,-0.721978599471011,-0.715424152550581,
-0.712901398121786,-0.711082469351578,-0.709145831571899,-0.706564443645755,
-0.700826566101351,-0.677307378585801,-0.652167948477815,-0.619222189382195,
-0.616467190145176,-0.615112764116153,-0.614043276000622,-0.612791544283018,
-0.610528992148389,-0.599202139297834,-0.549499317175386,-0.525982640659287,
-0.522039541800048,-0.519579543467754,-0.517660048940116,-0.515534994928404,
-0.512036246785498,-0.499153791500606,-0.449062050911271,-0.440125765073548,
-0.426324651551249,-0.424046827146197,-0.42266833520035,-0.421594353973553,
-0.420374145751427,-0.418255563646169,-0.409173297016571,-0.360509019333671,
-0.33363333921505,-0.329592172348819,-0.327129433694186,-0.325204219123834,
-0.323101698460661,-0.319704942270411,-0.308665781953824,-0.289895743865608,
-0.242394817054379),.UNSPECIFIED.);
#1283=B_SPLINE_CURVE_WITH_KNOTS('',3,(#42256,#42257,#42258,#42259,#42260,
#42261,#42262,#42263,#42264,#42265,#42266,#42267,#42268,#42269,#42270,#42271,
#42272,#42273,#42274,#42275,#42276,#42277,#42278,#42279,#42280,#42281,#42282,
#42283,#42284,#42285,#42286,#42287,#42288,#42289,#42290,#42291,#42292,#42293,
#42294,#42295,#42296,#42297,#42298,#42299,#42300,#42301,#42302,#42303,#42304,
#42305,#42306,#42307,#42308,#42309,#42310,#42311,#42312,#42313,#42314,#42315,
#42316,#42317,#42318,#42319,#42320,#42321,#42322,#42323,#42324,#42325,#42326,
#42327,#42328,#42329,#42330,#42331,#42332,#42333,#42334,#42335,#42336,#42337,
#42338,#42339,#42340,#42341,#42342,#42343,#42344,#42345,#42346,#42347,#42348,
#42349,#42350,#42351,#42352,#42353,#42354,#42355,#42356,#42357,#42358,#42359,
#42360,#42361,#42362,#42363,#42364,#42365,#42366,#42367,#42368,#42369,#42370,
#42371,#42372,#42373,#42374,#42375,#42376,#42377,#42378,#42379,#42380,#42381,
#42382,#42383,#42384,#42385,#42386,#42387,#42388,#42389,#42390,#42391,#42392,
#42393,#42394,#42395,#42396,#42397,#42398,#42399,#42400,#42401,#42402,#42403,
#42404,#42405,#42406,#42407,#42408,#42409,#42410,#42411,#42412,#42413,#42414,
#42415,#42416,#42417,#42418,#42419,#42420,#42421,#42422,#42423,#42424,#42425,
#42426,#42427,#42428,#42429,#42430,#42431,#42432,#42433,#42434,#42435,#42436,
#42437,#42438,#42439,#42440,#42441,#42442,#42443,#42444,#42445,#42446,#42447,
#42448,#42449,#42450,#42451,#42452,#42453,#42454,#42455,#42456,#42457,#42458,
#42459,#42460,#42461,#42462,#42463,#42464,#42465,#42466,#42467,#42468,#42469,
#42470,#42471,#42472,#42473,#42474,#42475,#42476,#42477,#42478,#42479,#42480,
#42481,#42482,#42483),.UNSPECIFIED.,.F.,.F.,(4,2,2,2,2,2,2,2,2,2,2,2,2,
2,2,2,2,2,2,2,2,2,2,2,2,2,2,2,2,2,2,2,2,2,2,2,2,2,2,2,2,2,2,2,2,2,2,2,2,
2,2,2,2,2,2,2,2,2,2,2,2,2,2,2,2,2,2,2,2,2,2,2,2,2,2,2,2,2,2,2,2,2,2,2,2,
2,2,2,2,2,2,2,2,2,2,2,2,2,2,2,2,2,2,2,2,2,2,2,2,2,2,2,2,4),(-2.18931141726403,
-2.17971667832203,-2.1740160498697,-2.17144169112358,-2.16950641917689,
-2.16768591172043,-2.16515639046521,-2.15855710585837,-2.11381318737296,
-2.08845504588565,-2.07751962371634,-2.07527973837221,-2.07403303835293,
-2.07296319011424,-2.07160231875026,-2.06881434908441,-2.04651619031018,
-1.99647970394439,-1.98357334229189,-1.98007276618586,-1.97794748921928,
-1.97602836410324,-1.97356963236718,-1.96963013729441,-1.94623392849253,
-1.89638959941177,-1.88504946072947,-1.88278627299703,-1.88153447453714,
-1.88046509985247,-1.87911104334982,-1.87635752577091,-1.84340404869804,
-1.81823856230869,-1.79478852897057,-1.78905936872617,-1.78647966632284,
-1.78454339589489,-1.78272415279415,-1.78019990948715,-1.77363543732423,
-1.72820385303824,-1.70333934205701,-1.69252478179074,-1.69029187121616,
-1.68904660853373,-1.68797646898426,-1.68661326000842,-1.68381392304517,
-1.66009019981957,-1.62676371955206,-1.60247045374809,-1.5966332703778,
-1.59403400930359,-1.59209453001447,-1.59028057654964,-1.58777683567353,
-1.581340693591,-1.53394559694203,-1.51046266617043,-1.49999852998953,-1.49778680719362,
-1.49654611858245,-1.49547534836201,-1.49410542088859,-1.49190568130833,
-1.47966149467538,-1.47672048794915,-1.4356436480993,-1.41692899715293,
-1.40578127281034,-1.40245184674131,-1.40036407711228,-1.39843411649277,
-1.39593980305544,-1.3917914385534,-1.35985865087689,-1.35502115868795,
-1.33287401204694,-1.31050544791138,-1.30632060236034,-1.30471701458361,
-1.30360952762794,-1.30260636232229,-1.30097041016749,-1.29688593766107,
-1.25474407604486,-1.21610189115401,-1.21116629859234,-1.20873697248221,
-1.20682091850222,-1.20467841387701,-1.20110095985851,-1.18731908359201,
-1.13793039812803,-1.1297063610522,-1.12806946511162,-1.11543397322218,
-1.11321409396405,-1.11183809978535,-1.11076678014907,-1.10953021389148,
-1.10733735324484,-1.09717180774499,-1.07481837312228,-1.02579318475135,
-1.01949783413441,-1.01701745831222,-1.0152095509318,-1.01326628957882,
-1.01064402995532,-1.00467757573562,-0.979348183379391,-0.97400982262004),
 .UNSPECIFIED.);
#1284=B_SPLINE_CURVE_WITH_KNOTS('',3,(#42485,#42486,#42487,#42488,#42489,
#42490,#42491,#42492,#42493,#42494,#42495,#42496,#42497,#42498,#42499,#42500,
#42501,#42502,#42503,#42504,#42505,#42506,#42507,#42508,#42509,#42510,#42511,
#42512,#42513,#42514,#42515,#42516,#42517,#42518,#42519,#42520,#42521,#42522,
#42523,#42524,#42525,#42526,#42527,#42528,#42529,#42530,#42531,#42532,#42533,
#42534,#42535,#42536,#42537,#42538,#42539,#42540),.UNSPECIFIED.,.F.,.F.,
(4,2,2,2,2,2,2,2,2,2,2,2,2,2,2,2,2,2,2,2,2,2,2,2,2,2,2,4),(-0.242394817054379,
-0.239477933129532,-0.232834969013898,-0.230848793020402,-0.229657925746363,
-0.228576461818301,-0.227148180620264,-0.224012380099846,-0.21970251570913,
-0.208538470225524,-0.176092779368492,-0.141350239810987,-0.137184531408027,
-0.134685091467156,-0.132754290951723,-0.130668717402813,-0.1273494967973,
-0.116541451371545,-0.0910614130852629,-0.0701399243704446,-0.0417834508299576,
-0.0389659377043969,-0.0375990719874846,-0.0365285510021365,-0.035285688115564,
-0.0339701702088994,-0.0319313914060394,-0.000563637760111814),
 .UNSPECIFIED.);
#1285=B_SPLINE_CURVE_WITH_KNOTS('',3,(#42541,#42542,#42543,#42544,#42545,
#42546,#42547,#42548,#42549,#42550,#42551,#42552,#42553,#42554,#42555,#42556,
#42557,#42558,#42559,#42560,#42561,#42562,#42563,#42564,#42565,#42566,#42567,
#42568,#42569,#42570,#42571,#42572,#42573,#42574,#42575,#42576,#42577,#42578,
#42579,#42580,#42581,#42582,#42583,#42584,#42585,#42586,#42587,#42588,#42589,
#42590,#42591,#42592,#42593,#42594,#42595,#42596,#42597,#42598,#42599,#42600,
#42601,#42602,#42603,#42604,#42605,#42606,#42607,#42608,#42609,#42610,#42611,
#42612,#42613,#42614,#42615,#42616,#42617,#42618,#42619,#42620,#42621,#42622,
#42623,#42624,#42625,#42626,#42627,#42628,#42629,#42630,#42631,#42632,#42633,
#42634,#42635,#42636,#42637,#42638,#42639,#42640,#42641,#42642,#42643,#42644,
#42645,#42646,#42647,#42648,#42649,#42650,#42651,#42652,#42653,#42654,#42655,
#42656,#42657,#42658,#42659,#42660,#42661,#42662,#42663,#42664,#42665,#42666,
#42667,#42668,#42669,#42670,#42671,#42672,#42673,#42674,#42675,#42676,#42677,
#42678,#42679,#42680,#42681,#42682,#42683,#42684,#42685,#42686,#42687,#42688,
#42689,#42690,#42691,#42692,#42693,#42694,#42695,#42696,#42697,#42698,#42699,
#42700,#42701,#42702,#42703,#42704,#42705,#42706,#42707,#42708,#42709,#42710,
#42711,#42712,#42713,#42714,#42715,#42716,#42717,#42718,#42719,#42720),
 .UNSPECIFIED.,.F.,.F.,(4,2,2,2,2,2,2,2,2,2,2,2,2,2,2,2,2,2,2,2,2,2,2,2,
2,2,2,2,2,2,2,2,2,2,2,2,2,2,2,2,2,2,2,2,2,2,2,2,2,2,2,2,2,2,2,2,2,2,2,2,
2,2,2,2,2,2,2,2,2,2,2,2,2,2,2,2,2,2,2,2,2,2,2,2,2,2,2,2,2,4),(-2.43111332147802,
-2.38917177521858,-2.37884381470538,-2.37580751112802,-2.37308011772945,
-2.37111920558706,-2.36933623067966,-2.36650413856717,-2.35976992812447,
-2.32022875543692,-2.29877245339659,-2.28568114122789,-2.27850715033665,
-2.27654687080474,-2.27553356051292,-2.27446559778252,-2.2731247373101,
-2.27051997682063,-2.25413707293724,-2.21586026107291,-2.19633288980105,
-2.18488724238658,-2.18150859397224,-2.17941088462658,-2.17748579658507,
-2.17501730932659,-2.17095401451103,-2.14312784627585,-2.09507485649955,
-2.08634084768317,-2.0842490787659,-2.08303521959261,-2.08196068488694,
-2.08057358187924,-2.07826512068986,-2.06372609292791,-2.06029014083134,
-2.02810348766952,-1.99442956914285,-1.98997799626856,-1.98764768423892,
-1.98575840755453,-1.98355640874775,-1.97980490657129,-1.96535729195556,
-1.95637900899021,-1.9187883770378,-1.9023298071914,-1.89393293524496,-1.89186744927816,
-1.89065939691659,-1.88958352682837,-1.88818629131251,-1.8858432234415,
-1.87041570169094,-1.83244271815857,-1.80480911101898,-1.79856606812766,
-1.79589652110466,-1.7939458995574,-1.79215054933956,-1.7892510245597,-1.78210809499121,
-1.78069897318267,-1.7142709818317,-1.70188807520945,-1.6995699185117,-1.6983063758211,
-1.69723817732583,-1.69589979053953,-1.69330788042781,-1.67729613578746,
-1.67070292700316,-1.62055405819952,-1.60779490314547,-1.60430804402985,
-1.60218598415125,-1.60026646040368,-1.59780261663732,-1.59384557993601,
-1.56983497879135,-1.52059092707837,-1.50930636683371,-1.50704653351831,
-1.50579556926187,-1.50472627945938,-1.50337152633243,-1.50061395219292,
-1.48014739334638,-1.45804903820686),.UNSPECIFIED.);
#1286=B_SPLINE_CURVE_WITH_KNOTS('',3,(#42726,#42727,#42728,#42729,#42730,
#42731,#42732,#42733,#42734,#42735,#42736,#42737,#42738,#42739,#42740,#42741,
#42742,#42743,#42744,#42745,#42746,#42747,#42748,#42749,#42750,#42751,#42752,
#42753,#42754,#42755,#42756,#42757,#42758,#42759,#42760,#42761,#42762,#42763,
#42764,#42765,#42766,#42767,#42768,#42769,#42770,#42771,#42772,#42773,#42774,
#42775,#42776,#42777,#42778,#42779,#42780,#42781,#42782,#42783,#42784,#42785,
#42786,#42787,#42788,#42789,#42790,#42791,#42792,#42793,#42794,#42795,#42796,
#42797,#42798,#42799,#42800,#42801,#42802,#42803,#42804,#42805,#42806,#42807,
#42808,#42809,#42810,#42811,#42812,#42813,#42814,#42815,#42816,#42817,#42818,
#42819,#42820,#42821,#42822,#42823,#42824,#42825,#42826,#42827,#42828,#42829,
#42830,#42831,#42832,#42833,#42834,#42835,#42836,#42837,#42838,#42839,#42840,
#42841,#42842,#42843,#42844,#42845,#42846,#42847,#42848,#42849,#42850,#42851,
#42852,#42853,#42854,#42855,#42856,#42857,#42858,#42859,#42860,#42861,#42862,
#42863,#42864,#42865,#42866,#42867,#42868,#42869,#42870,#42871,#42872,#42873,
#42874,#42875,#42876,#42877,#42878,#42879,#42880,#42881,#42882,#42883,#42884,
#42885,#42886,#42887,#42888,#42889,#42890,#42891,#42892,#42893,#42894,#42895,
#42896,#42897,#42898,#42899,#42900,#42901,#42902,#42903,#42904,#42905,#42906,
#42907),.UNSPECIFIED.,.F.,.F.,(4,2,2,2,2,2,2,2,2,2,2,2,2,2,2,2,2,2,2,2,
2,2,2,2,2,2,2,2,2,2,2,2,2,2,2,2,2,2,2,2,2,2,2,2,2,2,2,2,2,2,2,2,2,2,2,2,
2,2,2,2,2,2,2,2,2,2,2,2,2,2,2,2,2,2,2,2,2,2,2,2,2,2,2,2,2,2,2,2,2,2,4),
(-0.973731148246856,-0.951279812783102,-0.905142557312427,-0.898619654373167,
-0.896101639113266,-0.894283747865263,-0.892346008287853,-0.889759355501773,
-0.883993872523863,-0.86026380526683,-0.828197165487885,-0.802510932731893,
-0.799694562950635,-0.798327827824749,-0.797257206352008,-0.79601399436364,
-0.793791193224789,-0.783149442324522,-0.758979449522965,-0.712600691950234,
-0.706093629737283,-0.703578205223135,-0.701761038045641,-0.699823005805383,
-0.697234127711926,-0.691455971181448,-0.667626182897352,-0.635234174815842,
-0.609990764968893,-0.607177324877824,-0.605811199954283,-0.604740668152728,
-0.603497115284924,-0.601272612648773,-0.590601759538253,-0.566316174829597,
-0.520104127674435,-0.513586693973118,-0.511069668712476,-0.509252128619224,
-0.507314425935313,-0.504727241235337,-0.498958132026518,-0.475198112371053,
-0.443023778988662,-0.417481873302499,-0.414669410318262,-0.413303510126237,
-0.412233034873776,-0.410989410663569,-0.408764443935391,-0.39808489115552,
-0.373764168679482,-0.327604860820988,-0.321084461622554,-0.318567021058041,
-0.316749417787192,-0.314811867403475,-0.31222526435995,-0.306459040839527,
-0.282720685501049,-0.248079315716744,-0.224952367324629,-0.22215746487591,
-0.220795062430265,-0.219724907147974,-0.218503915405194,-0.216363456341239,
-0.21369578096127,-0.208053508523378,-0.191338861194781,-0.154619482139047,
-0.131651989982077,-0.127725350969118,-0.125270166743044,-0.123351054218838,
-0.121222969280775,-0.117711239986985,-0.104687879315528,-0.0677131483839322,
-0.0520824168507651,-0.0460575312679607,-0.03206964115021,-0.0297834579716761,
-0.0284024794595397,-0.0273281666610978,-0.0263227736782593,-0.0251172576095525,
-0.0233453054434443,-0.0170509377124757,-0.000563395908633966),
 .UNSPECIFIED.);
#1287=B_SPLINE_CURVE_WITH_KNOTS('',3,(#42908,#42909,#42910,#42911,#42912,
#42913,#42914,#42915,#42916,#42917,#42918,#42919,#42920,#42921,#42922,#42923,
#42924,#42925,#42926,#42927,#42928,#42929,#42930,#42931,#42932,#42933,#42934,
#42935,#42936,#42937,#42938,#42939,#42940,#42941,#42942,#42943,#42944,#42945,
#42946,#42947,#42948,#42949,#42950,#42951),.UNSPECIFIED.,.F.,.F.,(4,2,2,
2,2,2,2,2,2,2,2,2,2,2,2,2,2,2,2,2,2,4),(-2.43151735467866,-2.38290482253618,
-2.37358794232629,-2.36693454650074,-2.36419561173252,-2.3622317610133,
-2.36044974366734,-2.35762693889216,-2.35095445542579,-2.30791896744605,
-2.28692218296531,-2.27580139030319,-2.27150343763058,-2.26838780436255,
-2.26695602206332,-2.26587417418831,-2.26468527150582,-2.26270735505003,
-2.25613545544025,-2.25465941024578,-2.20294860238536,-2.18931141726403),
 .UNSPECIFIED.);
#1288=B_SPLINE_CURVE_WITH_KNOTS('',3,(#42952,#42953,#42954,#42955,#42956,
#42957,#42958,#42959,#42960,#42961,#42962,#42963,#42964,#42965,#42966,#42967,
#42968,#42969,#42970,#42971,#42972,#42973,#42974,#42975,#42976,#42977,#42978,
#42979,#42980,#42981,#42982,#42983,#42984,#42985,#42986,#42987,#42988,#42989,
#42990,#42991,#42992,#42993,#42994,#42995,#42996,#42997,#42998,#42999,#43000,
#43001,#43002,#43003,#43004,#43005,#43006,#43007,#43008,#43009,#43010,#43011,
#43012,#43013,#43014,#43015,#43016,#43017,#43018,#43019,#43020,#43021,#43022,
#43023,#43024,#43025,#43026,#43027,#43028,#43029,#43030,#43031,#43032,#43033,
#43034,#43035,#43036,#43037,#43038,#43039,#43040,#43041,#43042,#43043,#43044,
#43045,#43046,#43047,#43048,#43049,#43050,#43051,#43052,#43053,#43054,#43055,
#43056,#43057,#43058,#43059,#43060,#43061,#43062,#43063,#43064,#43065,#43066,
#43067,#43068,#43069,#43070,#43071,#43072,#43073,#43074,#43075,#43076,#43077,
#43078,#43079,#43080,#43081,#43082,#43083,#43084,#43085,#43086,#43087,#43088,
#43089,#43090,#43091,#43092,#43093,#43094,#43095,#43096,#43097,#43098,#43099,
#43100,#43101,#43102,#43103,#43104,#43105,#43106,#43107,#43108,#43109,#43110,
#43111,#43112,#43113,#43114,#43115,#43116,#43117,#43118,#43119,#43120,#43121,
#43122,#43123,#43124,#43125,#43126,#43127,#43128,#43129,#43130,#43131,#43132,
#43133,#43134,#43135,#43136,#43137,#43138,#43139,#43140,#43141,#43142,#43143,
#43144,#43145,#43146,#43147,#43148,#43149,#43150,#43151,#43152,#43153,#43154,
#43155,#43156,#43157,#43158,#43159,#43160,#43161,#43162,#43163,#43164,#43165,
#43166,#43167,#43168,#43169,#43170,#43171,#43172,#43173,#43174,#43175,#43176,
#43177),.UNSPECIFIED.,.F.,.F.,(4,2,2,2,2,2,2,2,2,2,2,2,2,2,2,2,2,2,2,2,
2,2,2,2,2,2,2,2,2,2,2,2,2,2,2,2,2,2,2,2,2,2,2,2,2,2,2,2,2,2,2,2,2,2,2,2,
2,2,2,2,2,2,2,2,2,2,2,2,2,2,2,2,2,2,2,2,2,2,2,2,2,2,2,2,2,2,2,2,2,2,2,2,
2,2,2,2,2,2,2,2,2,2,2,2,2,2,2,2,2,2,2,2,4),(-1.45804903820686,-1.44411603124442,
-1.41931364947825,-1.41341293944206,-1.41080266413045,-1.40886170535669,
-1.40705121483662,-1.40455988171319,-1.39819720383853,-1.34992058120615,
-1.32704990428333,-1.31674740446581,-1.31454611555658,-1.31330786400848,
-1.31223703005821,-1.31086420267533,-1.30865436736672,-1.29620903696286,
-1.29147679578464,-1.25491697527206,-1.22448400536502,-1.22010159717905,
-1.21778520182247,-1.21606298734725,-1.21390772642402,-1.21027164814994,
-1.19576936065448,-1.16782955717974,-1.12746451440361,-1.12323445350922,
-1.12157433395621,-1.12056671343561,-1.11946387646818,-1.11788328292449,
-1.11384713031036,-1.0930257268107,-1.05130305455471,-1.03167762524489,
-1.02791629846846,-1.02551156463125,-1.02359819413678,-1.02144102670644,
-1.01779652651438,-1.00318901473943,-0.95347066733627,-0.932750620208573,
-0.929985602457105,-0.928629224592126,-0.927559646597564,-0.926309486657909,
-0.924053979952481,-0.912850070776156,-0.864469000500925,-0.839580014824916,
-0.835596204323731,-0.833124017428689,-0.831203106510309,-0.829084695636985,
-0.825615686110968,-0.813055540777542,-0.762700454526518,-0.759610199259253,
-0.754164578701645,-0.739887822884978,-0.73758930351271,-0.736204759388913,
-0.735130087216258,-0.733913657859962,-0.731812017309895,-0.722957160454548,
-0.705090431905975,-0.676230134081205,-0.647297656289903,-0.643206856889482,
-0.640729480188029,-0.638802131026579,-0.63670666226202,-0.633341967401709,
-0.621853038839032,-0.602301877085459,-0.561006757549835,-0.54737630866855,
-0.545107171359372,-0.543731243198401,-0.542657568539581,-0.541435779445196,
-0.53931001710087,-0.530128889112639,-0.481545305103937,-0.454700250067968,
-0.450659873189332,-0.448197373453389,-0.446272199864192,-0.444169575928009,
-0.44077232405153,-0.428959561920595,-0.37967224122419,-0.355305788630056,
-0.352499805782322,-0.351135241544172,-0.350064944526133,-0.348820530864299,
-0.346591700623393,-0.335846176064526,-0.31126177525271,-0.265477914632111,
-0.258935259735816,-0.256414384522101,-0.254595961428509,-0.252659075479142,
-0.250076005176255,-0.244328738901846,-0.242792485946247),.UNSPECIFIED.);
#1289=B_SPLINE_CURVE_WITH_KNOTS('',3,(#43182,#43183,#43184,#43185,#43186,
#43187,#43188,#43189,#43190,#43191,#43192,#43193,#43194,#43195,#43196,#43197,
#43198,#43199,#43200,#43201,#43202,#43203,#43204,#43205,#43206,#43207,#43208,
#43209,#43210,#43211,#43212,#43213,#43214,#43215,#43216,#43217,#43218,#43219,
#43220,#43221,#43222,#43223,#43224,#43225,#43226,#43227,#43228,#43229,#43230,
#43231,#43232,#43233,#43234,#43235,#43236,#43237,#43238,#43239,#43240,#43241,
#43242,#43243,#43244,#43245,#43246,#43247,#43248,#43249,#43250,#43251,#43252,
#43253,#43254,#43255,#43256,#43257,#43258,#43259,#43260,#43261,#43262,#43263,
#43264,#43265,#43266,#43267,#43268,#43269,#43270,#43271,#43272,#43273,#43274,
#43275,#43276,#43277,#43278,#43279,#43280,#43281,#43282,#43283,#43284,#43285,
#43286,#43287,#43288,#43289,#43290,#43291,#43292,#43293,#43294,#43295,#43296,
#43297,#43298,#43299,#43300,#43301,#43302,#43303,#43304,#43305,#43306,#43307,
#43308,#43309,#43310,#43311,#43312,#43313,#43314,#43315,#43316,#43317,#43318,
#43319,#43320,#43321,#43322,#43323,#43324,#43325,#43326,#43327,#43328,#43329,
#43330,#43331,#43332,#43333,#43334,#43335,#43336,#43337,#43338,#43339,#43340,
#43341,#43342,#43343,#43344,#43345,#43346,#43347,#43348,#43349,#43350,#43351,
#43352,#43353,#43354,#43355,#43356,#43357,#43358,#43359,#43360,#43361,#43362,
#43363,#43364,#43365,#43366,#43367,#43368,#43369,#43370,#43371,#43372,#43373,
#43374,#43375,#43376,#43377,#43378,#43379,#43380,#43381,#43382,#43383,#43384,
#43385,#43386,#43387,#43388,#43389,#43390,#43391,#43392,#43393,#43394,#43395,
#43396,#43397,#43398,#43399,#43400,#43401,#43402,#43403,#43404,#43405,#43406,
#43407),.UNSPECIFIED.,.F.,.F.,(4,2,2,2,2,2,2,2,2,2,2,2,2,2,2,2,2,2,2,2,
2,2,2,2,2,2,2,2,2,2,2,2,2,2,2,2,2,2,2,2,2,2,2,2,2,2,2,2,2,2,2,2,2,2,2,2,
2,2,2,2,2,2,2,2,2,2,2,2,2,2,2,2,2,2,2,2,2,2,2,2,2,2,2,2,2,2,2,2,2,2,2,2,
2,2,2,2,2,2,2,2,2,2,2,2,2,2,2,2,2,2,2,2,4),(-2.1891488065354,-2.18407159117508,
-2.15979983031995,-2.14913383485187,-2.14690988386288,-2.14566659310058,
-2.14459625283958,-2.14323033751547,-2.1404171979368,-2.11511152414759,
-2.0828027222587,-2.05900520967905,-2.053231249635,-2.05064339136501,-2.04870577796628,
-2.0468887483205,-2.04437310819771,-2.03786320923401,-1.99150154532939,
-1.96730017783045,-1.95665173129801,-1.9544287463143,-1.95318561927294,
-1.95211518375039,-1.95074884127597,-1.94793379090312,-1.9223556952876,
-1.89024525756908,-1.86650790491974,-1.86074148965835,-1.85815489694462,
-1.85621738975707,-1.85439984798862,-1.85188252569995,-1.84536267515809,
-1.79916055671009,-1.77484177475619,-1.76416333267218,-1.76193843312834,
-1.76069484164971,-1.75962438649371,-1.75825851074869,-1.75544608042783,
-1.73028692675401,-1.69786638536991,-1.67402924025756,-1.66824986706944,
-1.66566084130567,-1.66372285341205,-1.66190583552197,-1.65939078855576,
-1.65288572872909,-1.60644531195937,-1.58229151716934,-1.5716545869198,
-1.5694321061222,-1.56818899521187,-1.5671184066517,-1.565751652834,-1.56293502569036,
-1.53713253224363,-1.50518579944361,-1.48149220271351,-1.47573106818268,
-1.47314523773344,-1.47120766213391,-1.46938959103355,-1.46687079517596,
-1.46034284864737,-1.41425149688032,-1.38984698160783,-1.3791463523992,
-1.37691991724136,-1.37567589707743,-1.37460534222759,-1.37323968742848,
-1.37105445594421,-1.35908847320552,-1.35390478039994,-1.31033055912168,
-1.28857470422758,-1.28306825710304,-1.28052907871686,-1.27859859569926,
-1.27676650936933,-1.27367727812995,-1.26575457493155,-1.21565024412149,
-1.18756778685796,-1.18474933794885,-1.18338212841215,-1.18231139074868,
-1.18106833635763,-1.17884653393905,-1.16822327014345,-1.14412742366844,
-1.09763702710024,-1.09113657392201,-1.08862209291068,-1.08680508048344,
-1.08486672374035,-1.0822765677241,-1.07649200246857,-1.05261382074484,
-1.02009029026644,-0.99502696360631,-0.992214634511519,-0.990848664520793,
-0.98977807000532,-0.988534233238302,-0.986308704469612,-0.975622953818306,
-0.973731148246856),.UNSPECIFIED.);
#1290=B_SPLINE_CURVE_WITH_KNOTS('',3,(#43409,#43410,#43411,#43412,#43413,
#43414,#43415,#43416,#43417,#43418,#43419,#43420,#43421,#43422,#43423,#43424,
#43425,#43426,#43427,#43428,#43429,#43430,#43431,#43432,#43433,#43434,#43435,
#43436,#43437,#43438,#43439,#43440,#43441,#43442,#43443,#43444,#43445,#43446,
#43447,#43448,#43449,#43450),.UNSPECIFIED.,.F.,.F.,(4,2,2,2,2,2,2,2,2,2,
2,2,2,2,2,2,2,2,2,2,4),(-0.242792485946247,-0.236606260475716,-0.216603844230613,
-0.177600472048637,-0.162467956475159,-0.160135070365004,-0.158740433278701,
-0.157664438586877,-0.156660436687939,-0.154845479375884,-0.14911953504362,
-0.139586203035983,-0.114635212441782,-0.0732474400545378,-0.0665302659882875,
-0.0636998826889005,-0.0619163984637437,-0.0599536284970733,-0.0572212430688076,
-0.0506087548470122,-0.000564233396250174),.UNSPECIFIED.);
#1291=B_SPLINE_CURVE_WITH_KNOTS('',3,(#43451,#43452,#43453,#43454,#43455,
#43456,#43457,#43458,#43459,#43460,#43461,#43462,#43463,#43464,#43465,#43466,
#43467,#43468,#43469,#43470,#43471,#43472,#43473,#43474,#43475,#43476,#43477,
#43478,#43479,#43480,#43481,#43482,#43483,#43484,#43485,#43486,#43487,#43488,
#43489,#43490,#43491,#43492,#43493,#43494,#43495,#43496,#43497,#43498,#43499,
#43500,#43501,#43502,#43503,#43504,#43505,#43506,#43507,#43508,#43509,#43510,
#43511,#43512,#43513,#43514,#43515,#43516,#43517,#43518,#43519,#43520,#43521,
#43522,#43523,#43524,#43525,#43526,#43527,#43528,#43529,#43530,#43531,#43532,
#43533,#43534,#43535,#43536,#43537,#43538,#43539,#43540,#43541,#43542,#43543,
#43544,#43545,#43546,#43547,#43548,#43549,#43550,#43551,#43552,#43553,#43554,
#43555,#43556,#43557,#43558,#43559,#43560,#43561,#43562,#43563,#43564,#43565,
#43566,#43567,#43568,#43569,#43570,#43571,#43572,#43573,#43574,#43575,#43576,
#43577,#43578,#43579,#43580,#43581,#43582,#43583,#43584,#43585,#43586,#43587,
#43588,#43589,#43590,#43591,#43592,#43593,#43594,#43595,#43596,#43597,#43598,
#43599,#43600,#43601,#43602,#43603,#43604,#43605,#43606,#43607,#43608,#43609,
#43610,#43611,#43612,#43613,#43614,#43615,#43616,#43617,#43618,#43619,#43620,
#43621,#43622,#43623,#43624,#43625,#43626),.UNSPECIFIED.,.F.,.F.,(4,2,2,
2,2,2,2,2,2,2,2,2,2,2,2,2,2,2,2,2,2,2,2,2,2,2,2,2,2,2,2,2,2,2,2,2,2,2,2,
2,2,2,2,2,2,2,2,2,2,2,2,2,2,2,2,2,2,2,2,2,2,2,2,2,2,2,2,2,2,2,2,2,2,2,2,
2,2,2,2,2,2,2,2,2,2,2,2,4),(-2.43144843030508,-2.40785000583015,-2.40081715584106,
-2.39898955012162,-2.39776127716115,-2.3967514418594,-2.3956810271092,-2.39431407568053,
-2.39149562376289,-2.36415626395074,-2.3429661710446,-2.31721727850622,
-2.3060587865771,-2.30270362049879,-2.30061026573823,-2.2986822823544,-2.29620049811193,
-2.29209461855544,-2.26247961134774,-2.21309749852176,-2.20704719263268,
-2.20523873696824,-2.20423118381301,-2.20315890103114,-2.20177342189852,
-2.1995220676231,-2.18630323603844,-2.17896668854862,-2.15998733635828,
-2.11753435018015,-2.11178986444075,-2.10920716907905,-2.10727021236919,
-2.10545146162796,-2.10292971542693,-2.09638241916073,-2.050624999603,-2.02598654668394,
-2.01522759358309,-2.01299778004289,-2.01175308504504,-2.01068270850339,
-2.00931826178519,-2.00651324271827,-1.98225073594355,-1.93292688948208,
-1.9210808995237,-1.91768012732984,-1.91557657668874,-1.91365138680606,
-1.91119000910201,-1.90715387836146,-1.88071562406883,-1.86976129225014,
-1.84451043018516,-1.82524940226418,-1.82137031370429,-1.81981441394241,
-1.81871618686855,-1.81770287689808,-1.81601363388956,-1.81160379997301,
-1.77640226859393,-1.73071783308773,-1.72611796769222,-1.72375628374654,
-1.72184635426832,-1.71965954041639,-1.7159769004447,-1.70230398963697,
-1.64234000250745,-1.63025924291869,-1.62795571378017,-1.62669498537163,
-1.62562607093029,-1.62428286458477,-1.62167018288379,-1.6051099103036,
-1.56739941498058,-1.54051901546667,-1.53436308508751,-1.53170741605176,
-1.5297581860298,-1.5279579738794,-1.52550861096656,-1.51939831583559,-1.46849685491709,
-1.45815955314769),.UNSPECIFIED.);
#1292=B_SPLINE_CURVE_WITH_KNOTS('',3,(#43632,#43633,#43634,#43635,#43636,
#43637,#43638,#43639,#43640,#43641,#43642,#43643,#43644,#43645,#43646,#43647,
#43648,#43649,#43650,#43651,#43652,#43653,#43654,#43655,#43656,#43657,#43658,
#43659,#43660,#43661,#43662,#43663,#43664,#43665,#43666,#43667,#43668,#43669,
#43670,#43671,#43672,#43673,#43674,#43675,#43676,#43677,#43678,#43679,#43680,
#43681,#43682,#43683,#43684,#43685,#43686,#43687,#43688,#43689,#43690,#43691,
#43692,#43693,#43694,#43695,#43696,#43697,#43698,#43699,#43700,#43701,#43702,
#43703,#43704,#43705,#43706,#43707,#43708,#43709,#43710,#43711,#43712,#43713,
#43714,#43715,#43716,#43717,#43718,#43719,#43720,#43721,#43722,#43723,#43724,
#43725,#43726,#43727,#43728,#43729,#43730,#43731,#43732,#43733,#43734,#43735,
#43736,#43737,#43738,#43739,#43740,#43741,#43742,#43743,#43744,#43745,#43746,
#43747,#43748,#43749,#43750,#43751,#43752,#43753,#43754,#43755,#43756,#43757,
#43758,#43759,#43760,#43761,#43762,#43763,#43764,#43765,#43766,#43767,#43768,
#43769,#43770,#43771,#43772,#43773,#43774,#43775,#43776,#43777,#43778,#43779,
#43780,#43781,#43782,#43783,#43784,#43785,#43786,#43787,#43788,#43789,#43790,
#43791,#43792,#43793,#43794,#43795,#43796,#43797,#43798,#43799,#43800,#43801,
#43802,#43803,#43804,#43805,#43806,#43807,#43808,#43809,#43810,#43811,#43812,
#43813,#43814,#43815,#43816,#43817),.UNSPECIFIED.,.F.,.F.,(4,2,2,2,2,2,
2,2,2,2,2,2,2,2,2,2,2,2,2,2,2,2,2,2,2,2,2,2,2,2,2,2,2,2,2,2,2,2,2,2,2,2,
2,2,2,2,2,2,2,2,2,2,2,2,2,2,2,2,2,2,2,2,2,2,2,2,2,2,2,2,2,2,2,2,2,2,2,2,
2,2,2,2,2,2,2,2,2,2,2,2,2,2,4),(-0.974056705393386,-0.970767599827482,-0.968248849743031,
-0.966430598933844,-0.964492634670361,-0.961905954975287,-0.956141557687982,
-0.932423006446969,-0.90040565164778,-0.874644663389221,-0.871827496807036,
-0.870460487489761,-0.869389705003979,-0.868146367639386,-0.865923493353298,
-0.855284282705457,-0.831126855210087,-0.784718647842081,-0.778212138159034,
-0.77569658979416,-0.773879222992864,-0.771940875529662,-0.769351399913293,
-0.763571167113192,-0.739728233207329,-0.707303473089765,-0.68209559271628,
-0.679282025970213,-0.677915759069537,-0.676845077488844,-0.675601306485995,
-0.67337630525633,-0.662700976143061,-0.638400270170196,-0.592197954215753,
-0.585678539654812,-0.583160985107273,-0.581343139305016,-0.579405181685472,
-0.576817778872307,-0.571048696888105,-0.547291951846117,-0.515135657007328,
-0.489564133311662,-0.486748260051386,-0.485381570228107,-0.484310890681449,
-0.483067504073187,-0.480844127845821,-0.470194587867565,-0.445995046599982,
-0.399654341647386,-0.393143278441079,-0.390627117579252,-0.388809682585953,
-0.386871609996702,-0.384283100823115,-0.378507546406061,-0.354699458675277,
-0.322375054238652,-0.297033738475139,-0.294219448791694,-0.292853103622761,
-0.291782491249627,-0.290538950233659,-0.28831472761058,-0.277650190713819,
-0.25339073855881,-0.207134540309728,-0.200620242929509,-0.197880099369848,
-0.195947412270461,-0.194001118338801,-0.192026745997686,-0.186780676933051,
-0.179902354445663,-0.163049726484927,-0.137558298351062,-0.104416941036746,
-0.101666486621136,-0.100312839959541,-0.0992432537594365,-0.0979905807456046,
-0.0957242462049522,-0.084334456591408,-0.0339378912075332,-0.0199576090708968,
-0.0140702961719974,-0.00792603025400796,-0.00525623048890964,-0.00332710256047799,
-0.00169315958314438,-0.000563811939861371),.UNSPECIFIED.);
#1293=B_SPLINE_CURVE_WITH_KNOTS('',3,(#43818,#43819,#43820,#43821,#43822,
#43823,#43824,#43825,#43826,#43827,#43828,#43829,#43830,#43831,#43832,#43833,
#43834,#43835,#43836,#43837,#43838,#43839,#43840,#43841,#43842,#43843,#43844,
#43845,#43846,#43847,#43848,#43849,#43850,#43851,#43852,#43853,#43854,#43855,
#43856,#43857,#43858,#43859),.UNSPECIFIED.,.F.,.F.,(4,2,2,2,2,2,2,2,2,2,
2,2,2,2,2,2,2,2,2,2,4),(-2.43117239107418,-2.4290930149489,-2.42472570548591,
-2.40006531117722,-2.3614222198719,-2.34391340408118,-2.34022028516732,
-2.33869485427737,-2.33760229782761,-2.33658159640704,-2.33485398169207,
-2.33019147478549,-2.28681939009497,-2.2531026138123,-2.24618984956439,
-2.24347381374301,-2.24152886814728,-2.23958583461733,-2.23684613990076,
-2.23033209340117,-2.1891488065354),.UNSPECIFIED.);
#1294=B_SPLINE_CURVE_WITH_KNOTS('',3,(#43860,#43861,#43862,#43863,#43864,
#43865,#43866,#43867,#43868,#43869,#43870,#43871,#43872,#43873,#43874,#43875,
#43876,#43877,#43878,#43879,#43880,#43881,#43882,#43883,#43884,#43885,#43886,
#43887,#43888,#43889,#43890,#43891,#43892,#43893,#43894,#43895,#43896,#43897,
#43898,#43899,#43900,#43901,#43902,#43903,#43904,#43905,#43906,#43907,#43908,
#43909,#43910,#43911,#43912,#43913,#43914,#43915,#43916,#43917,#43918,#43919,
#43920,#43921,#43922,#43923,#43924,#43925,#43926,#43927,#43928,#43929,#43930,
#43931,#43932,#43933,#43934,#43935,#43936,#43937,#43938,#43939,#43940,#43941,
#43942,#43943,#43944,#43945,#43946,#43947,#43948,#43949,#43950,#43951,#43952,
#43953,#43954,#43955,#43956,#43957,#43958,#43959,#43960,#43961,#43962,#43963,
#43964,#43965,#43966,#43967,#43968,#43969,#43970,#43971,#43972,#43973,#43974,
#43975,#43976,#43977,#43978,#43979,#43980,#43981,#43982,#43983,#43984,#43985,
#43986,#43987,#43988,#43989,#43990,#43991,#43992,#43993,#43994,#43995,#43996,
#43997,#43998,#43999,#44000,#44001,#44002,#44003,#44004,#44005,#44006,#44007,
#44008,#44009,#44010,#44011,#44012,#44013,#44014,#44015,#44016,#44017,#44018,
#44019,#44020,#44021,#44022,#44023,#44024,#44025,#44026,#44027,#44028,#44029,
#44030,#44031,#44032,#44033,#44034,#44035,#44036,#44037,#44038,#44039,#44040,
#44041,#44042,#44043,#44044,#44045,#44046,#44047,#44048,#44049,#44050,#44051,
#44052,#44053,#44054,#44055,#44056,#44057,#44058,#44059,#44060,#44061,#44062,
#44063,#44064,#44065,#44066,#44067,#44068,#44069,#44070,#44071,#44072,#44073,
#44074,#44075,#44076,#44077,#44078,#44079,#44080,#44081,#44082,#44083,#44084,
#44085,#44086,#44087,#44088,#44089),.UNSPECIFIED.,.F.,.F.,(4,2,2,2,2,2,
2,2,2,2,2,2,2,2,2,2,2,2,2,2,2,2,2,2,2,2,2,2,2,2,2,2,2,2,2,2,2,2,2,2,2,2,
2,2,2,2,2,2,2,2,2,2,2,2,2,2,2,2,2,2,2,2,2,2,2,2,2,2,2,2,2,2,2,2,2,2,2,2,
2,2,2,2,2,2,2,2,2,2,2,2,2,2,2,2,2,2,2,2,2,2,2,2,2,2,2,2,2,2,2,2,2,2,2,2,
4),(-1.45815955314769,-1.44732239483162,-1.4374815980845,-1.43530965035556,
-1.43407751885901,-1.43300529456673,-1.43162192643633,-1.42937800453873,
-1.41626097458002,-1.37521302751139,-1.34801416757412,-1.34182015784328,
-1.33915781988152,-1.33720733922246,-1.33540852808946,-1.33296499174635,
-1.32686946064739,-1.27577362846622,-1.25471878594145,-1.24491146276283,
-1.24274165989903,-1.24150995294707,-1.24043758552606,-1.23905335993059,
-1.2368067246399,-1.22363569591481,-1.21620278656998,-1.19055413225765,
-1.18075585925275,-1.1529041864578,-1.14883716538906,-1.14636632028527,
-1.14443934880887,-1.14233954307896,-1.13895742295031,-1.12730455185172,
-1.10734920133301,-1.0720558348165,-1.06769069478283,-1.05308523263596,
-1.05077249566933,-1.04938351750842,-1.04830795561214,-1.04709340405836,
-1.0450015131953,-1.03628206747524,-0.988270978654193,-0.960350687990752,
-0.956282198022534,-0.953810991505604,-0.951884055767852,-0.949784609839112,
-0.946403777433049,-0.934762463204984,-0.914835477492735,-0.888896014969876,
-0.86094318007732,-0.858124467330395,-0.856757192695807,-0.855686434128333,
-0.854443390088617,-0.852221691153655,-0.841600547227164,-0.817513338268695,
-0.771009110740899,-0.76450940249591,-0.761995017413554,-0.760178011403446,
-0.758239603075399,-0.75564927736428,-0.749863908874753,-0.725979799604828,
-0.693441324549237,-0.668398089841144,-0.665585869300714,-0.664219907676432,
-0.663149298508304,-0.661905420581649,-0.65967975904056,-0.648992234575457,
-0.624642378329538,-0.578513036397747,-0.571989464154865,-0.569471318334955,
-0.567653374251944,-0.565715616815219,-0.563129006459453,-0.557363896546726,
-0.533637087329864,-0.501583030661506,-0.475878850358701,-0.473062334996994,
-0.471695558087341,-0.470624917716716,-0.469381699807339,-0.467158927530579,
-0.456518072773769,-0.432351920759021,-0.385967102003845,-0.379459667396208,
-0.376944159485018,-0.375126951867793,-0.373188894923825,-0.370600015649461,
-0.364821990738335,-0.340993582725157,-0.308606257880663,-0.283354963533916,
-0.280541423394484,-0.279175265685267,-0.278104715785658,-0.276861150774939,
-0.274636648374459,-0.263966221290074,-0.242629061483656),.UNSPECIFIED.);
#1295=B_SPLINE_CURVE_WITH_KNOTS('',3,(#44094,#44095,#44096,#44097,#44098,
#44099,#44100,#44101,#44102,#44103,#44104,#44105,#44106,#44107,#44108,#44109,
#44110,#44111,#44112,#44113,#44114,#44115,#44116,#44117,#44118,#44119,#44120,
#44121,#44122,#44123,#44124,#44125,#44126,#44127,#44128,#44129,#44130,#44131,
#44132,#44133,#44134,#44135,#44136,#44137,#44138,#44139,#44140,#44141,#44142,
#44143,#44144,#44145,#44146,#44147,#44148,#44149,#44150,#44151,#44152,#44153,
#44154,#44155,#44156,#44157,#44158,#44159,#44160,#44161,#44162,#44163,#44164,
#44165,#44166,#44167,#44168,#44169,#44170,#44171,#44172,#44173,#44174,#44175,
#44176,#44177,#44178,#44179,#44180,#44181,#44182,#44183,#44184,#44185,#44186,
#44187,#44188,#44189,#44190,#44191,#44192,#44193,#44194,#44195,#44196,#44197,
#44198,#44199,#44200,#44201,#44202,#44203,#44204,#44205,#44206,#44207,#44208,
#44209,#44210,#44211,#44212,#44213,#44214,#44215,#44216,#44217,#44218,#44219,
#44220,#44221,#44222,#44223,#44224,#44225,#44226,#44227,#44228,#44229,#44230,
#44231,#44232,#44233,#44234,#44235,#44236,#44237,#44238,#44239,#44240,#44241,
#44242,#44243,#44244,#44245,#44246,#44247,#44248,#44249,#44250,#44251,#44252,
#44253,#44254,#44255,#44256,#44257,#44258,#44259,#44260,#44261,#44262,#44263,
#44264,#44265,#44266,#44267,#44268,#44269,#44270,#44271,#44272,#44273,#44274,
#44275,#44276,#44277,#44278,#44279,#44280,#44281,#44282,#44283,#44284,#44285,
#44286,#44287,#44288,#44289,#44290,#44291,#44292,#44293,#44294,#44295,#44296,
#44297,#44298,#44299,#44300,#44301,#44302,#44303,#44304,#44305),
 .UNSPECIFIED.,.F.,.F.,(4,2,2,2,2,2,2,2,2,2,2,2,2,2,2,2,2,2,2,2,2,2,2,2,
2,2,2,2,2,2,2,2,2,2,2,2,2,2,2,2,2,2,2,2,2,2,2,2,2,2,2,2,2,2,2,2,2,2,2,2,
2,2,2,2,2,2,2,2,2,2,2,2,2,2,2,2,2,2,2,2,2,2,2,2,2,2,2,2,2,2,2,2,2,2,2,2,
2,2,2,2,2,2,2,2,2,4),(-2.18988230660751,-2.18020862884737,-2.15522474485167,
-2.13149902818363,-2.12573340665907,-2.12314655975065,-2.12120861939381,
-2.11939049471598,-2.11687208411056,-2.11034779308784,-2.06417767717913,
-2.03982150278388,-2.02913245352607,-2.02690650664556,-2.0256624917424,
-2.02459177367733,-2.02322569379073,-2.02041328568376,-1.99604239516536,
-1.9467732584526,-1.93496561450914,-1.93156816678215,-1.92946505929063,
-1.9275392007042,-1.92507549006123,-1.92103238023235,-1.8941329993509,-1.84541388260516,
-1.83634145487599,-1.83422303722388,-1.83300259187793,-1.83192817379636,
-1.83054884247138,-1.82826906621039,-1.81443650002443,-1.80553599538707,
-1.75544982617297,-1.74256616896649,-1.73906644883103,-1.73694066510838,
-1.73502042061606,-1.73255933509714,-1.72861420416093,-1.70508409941534,
-1.65533141517052,-1.64399602008472,-1.64173226192497,-1.64047994836713,
-1.63941001106574,-1.63805508519747,-1.63529928491342,-1.60235842677999,
-1.57723192580991,-1.55370258545975,-1.54796179730585,-1.54537919422741,
-1.54344167957483,-1.54162194773606,-1.53909811186514,-1.53254110687688,
-1.48689272750605,-1.46215469980333,-1.45136918546287,-1.44913718945494,
-1.44789173510909,-1.44682099239685,-1.44545644904185,-1.44265247361283,
-1.41859883477889,-1.36912828860013,-1.35720003965533,-1.35379031711478,
-1.35168428436138,-1.34975885042809,-1.34729994298328,-1.34327378224955,
-1.31703011668517,-1.30567420457458,-1.28020291482538,-1.26126991671715,
-1.25742413169721,-1.2558732479088,-1.25477565994706,-1.25376065521533,
-1.25206396782874,-1.24760847225538,-1.21635576050806,-1.1698077613698,
-1.1633097746501,-1.16079547791974,-1.15897834638018,-1.1570396280807,-1.15444858428883,
-1.14866033077609,-1.1247563834069,-1.09217127843988,-1.06718673213728,
-1.06437463042073,-1.06300858835561,-1.06193784993263,-1.06069374575655,
-1.05846749233913,-1.04777351747286,-1.02340036986222,-0.977293775021958,
-0.974056705393386),.UNSPECIFIED.);
#1296=B_SPLINE_CURVE_WITH_KNOTS('',3,(#44307,#44308,#44309,#44310,#44311,
#44312,#44313,#44314,#44315,#44316,#44317,#44318,#44319,#44320,#44321,#44322,
#44323,#44324,#44325,#44326,#44327,#44328,#44329,#44330,#44331,#44332,#44333,
#44334,#44335,#44336,#44337,#44338,#44339,#44340,#44341,#44342,#44343,#44344,
#44345,#44346),.UNSPECIFIED.,.F.,.F.,(4,2,2,2,2,2,2,2,2,2,2,2,2,2,2,2,2,
2,2,4),(-0.242629061483656,-0.239682634531744,-0.1934641037118,-0.186947916218177,
-0.184431248901112,-0.182613783776822,-0.18074272676804,-0.178246011784779,
-0.175487868287805,-0.170877890135219,-0.13846529255783,-0.0991266652829539,
-0.0898702697162213,-0.0876598718599338,-0.0864060717597737,-0.0853365957900867,
-0.0839844673452894,-0.0812415895493274,-0.0491039633603923,-0.000564216032066522),
 .UNSPECIFIED.);
#1297=B_SPLINE_CURVE_WITH_KNOTS('',3,(#44347,#44348,#44349,#44350,#44351,
#44352,#44353,#44354,#44355,#44356,#44357,#44358,#44359,#44360,#44361,#44362,
#44363,#44364,#44365,#44366,#44367,#44368,#44369,#44370,#44371,#44372,#44373,
#44374,#44375,#44376,#44377,#44378,#44379,#44380,#44381,#44382,#44383,#44384,
#44385,#44386,#44387,#44388,#44389,#44390,#44391,#44392,#44393,#44394,#44395,
#44396,#44397,#44398,#44399,#44400,#44401,#44402,#44403,#44404,#44405,#44406,
#44407,#44408,#44409,#44410,#44411,#44412,#44413,#44414,#44415,#44416,#44417,
#44418,#44419,#44420,#44421,#44422,#44423,#44424,#44425,#44426,#44427,#44428,
#44429,#44430,#44431,#44432,#44433,#44434,#44435,#44436,#44437,#44438,#44439,
#44440,#44441,#44442,#44443,#44444,#44445,#44446,#44447,#44448,#44449,#44450,
#44451,#44452,#44453,#44454,#44455,#44456,#44457,#44458,#44459,#44460,#44461,
#44462,#44463,#44464,#44465,#44466,#44467,#44468,#44469,#44470,#44471,#44472,
#44473,#44474,#44475,#44476,#44477,#44478,#44479,#44480,#44481,#44482,#44483,
#44484,#44485,#44486,#44487,#44488,#44489,#44490,#44491,#44492,#44493,#44494,
#44495,#44496,#44497,#44498,#44499,#44500,#44501,#44502,#44503,#44504,#44505,
#44506,#44507,#44508,#44509,#44510,#44511,#44512,#44513,#44514,#44515,#44516,
#44517,#44518,#44519,#44520,#44521,#44522,#44523,#44524,#44525,#44526),
 .UNSPECIFIED.,.F.,.F.,(4,2,2,2,2,2,2,2,2,2,2,2,2,2,2,2,2,2,2,2,2,2,2,2,
2,2,2,2,2,2,2,2,2,2,2,2,2,2,2,2,2,2,2,2,2,2,2,2,2,2,2,2,2,2,2,2,2,2,2,2,
2,2,2,2,2,2,2,2,2,2,2,2,2,2,2,2,2,2,2,2,2,2,2,2,2,2,2,2,2,4),(-2.43140689233801,
-2.42730802413046,-2.42384966764435,-2.42197678520656,-2.42013632541179,
-2.41805381072676,-2.41474657866191,-2.40482494816618,-2.35006798177995,
-2.33068438956821,-2.32679299369968,-2.32523527200865,-2.3241368317781,
-2.3231241666317,-2.32143768962451,-2.31704448475864,-2.28112899585354,
-2.24110509170697,-2.23570914056281,-2.23263405531163,-2.23051182522825,
-2.22847121329233,-2.22659964598011,-2.22413640967445,-2.22009303974486,
-2.1932117185811,-2.14452097237056,-2.13544349917663,-2.13332534236296,
-2.1321052809959,-2.13103135690177,-2.12965285963222,-2.12737487317794,
-2.1135662627697,-2.10465940377763,-2.05461570128677,-2.04171198600117,
-2.03821145889551,-2.03608608258357,-2.03416678461417,-2.03170771598067,
-2.02776744732415,-2.00410984452807,-1.95449874146468,-1.94317912566083,
-1.94091696075749,-1.93966532352435,-1.93859583811702,-1.93724132341471,
-1.93448583098649,-1.90158806500461,-1.87652216896889,-1.85293812903845,
-1.84719146553272,-1.84460846852694,-1.84267155586909,-1.84085304339472,
-1.83833194146579,-1.83178815509688,-1.78598031300878,-1.7613814106052,
-1.75063262164552,-1.74840351230983,-1.74715901618346,-1.74608868915105,
-1.74472414859095,-1.74191840928341,-1.71756171542954,-1.66829638977874,
-1.6564858775608,-1.65308875597319,-1.65098609224484,-1.64906080114486,
-1.64659803823337,-1.64255695708556,-1.61570163208136,-1.56709302049328,
-1.55790361113352,-1.55577708686118,-1.5545550599976,-1.55348130266044,
-1.55210544329499,-1.54983678596374,-1.53621703957684,-1.49492499433258,
-1.47538716047664,-1.46390196080592,-1.4605373999802,-1.45844179702659,
-1.45799153533436),.UNSPECIFIED.);
#1298=B_SPLINE_CURVE_WITH_KNOTS('',3,(#44532,#44533,#44534,#44535,#44536,
#44537,#44538,#44539,#44540,#44541,#44542,#44543,#44544,#44545,#44546,#44547,
#44548,#44549,#44550,#44551,#44552,#44553,#44554,#44555,#44556,#44557,#44558,
#44559,#44560,#44561,#44562,#44563,#44564,#44565,#44566,#44567,#44568,#44569,
#44570,#44571,#44572,#44573,#44574,#44575,#44576,#44577,#44578,#44579,#44580,
#44581,#44582,#44583,#44584,#44585,#44586,#44587,#44588,#44589,#44590,#44591,
#44592,#44593,#44594,#44595,#44596,#44597,#44598,#44599,#44600,#44601,#44602,
#44603,#44604,#44605,#44606,#44607,#44608,#44609,#44610,#44611,#44612,#44613,
#44614,#44615,#44616,#44617,#44618,#44619,#44620,#44621,#44622,#44623,#44624,
#44625,#44626,#44627,#44628,#44629,#44630,#44631,#44632,#44633,#44634,#44635,
#44636,#44637,#44638,#44639,#44640,#44641,#44642,#44643,#44644,#44645,#44646,
#44647,#44648,#44649,#44650,#44651,#44652,#44653,#44654,#44655,#44656,#44657,
#44658,#44659,#44660,#44661,#44662,#44663,#44664,#44665,#44666,#44667,#44668,
#44669,#44670,#44671,#44672,#44673,#44674,#44675,#44676,#44677,#44678,#44679,
#44680,#44681,#44682,#44683,#44684,#44685,#44686,#44687,#44688,#44689,#44690,
#44691,#44692,#44693,#44694,#44695,#44696,#44697,#44698,#44699,#44700,#44701,
#44702,#44703,#44704,#44705,#44706,#44707,#44708,#44709,#44710,#44711,#44712,
#44713,#44714,#44715,#44716,#44717,#44718,#44719,#44720,#44721,#44722,#44723,
#44724,#44725,#44726,#44727,#44728,#44729,#44730,#44731),.UNSPECIFIED.,
 .F.,.F.,(4,2,2,2,2,2,2,2,2,2,2,2,2,2,2,2,2,2,2,2,2,2,2,2,2,2,2,2,2,2,2,
2,2,2,2,2,2,2,2,2,2,2,2,2,2,2,2,2,2,2,2,2,2,2,2,2,2,2,2,2,2,2,2,2,2,2,2,
2,2,2,2,2,2,2,2,2,2,2,2,2,2,2,2,2,2,2,2,2,2,2,2,2,2,2,2,2,2,2,2,4),(-0.97398342740053,
-0.968789361277668,-0.965266725663231,-0.960570416671455,-0.946002141715252,
-0.943691261956634,-0.942302975570392,-0.941227687795161,-0.94001314994702,
-0.937920616691668,-0.929188913039654,-0.881145465576063,-0.853287025028794,
-0.849220735468894,-0.846750441118566,-0.84482396273153,-0.84272475851091,
-0.839343748850874,-0.82769612619938,-0.80775146912542,-0.77275384054031,
-0.768060200998447,-0.753492154119069,-0.751181382289118,-0.749793168302248,
-0.748717941271087,-0.747503477310026,-0.745411083233981,-0.736680131350044,
-0.688640198281378,-0.660782354850949,-0.656716274212725,-0.65424611436532,
-0.652319745407183,-0.65022066500978,-0.646839864898028,-0.635193065905695,
-0.615249941840422,-0.58027423357657,-0.575552480206659,-0.560992661202858,
-0.558682321382804,-0.557294274842584,-0.556219120642795,-0.555004674660426,
-0.552912166829224,-0.544178656171066,-0.496132215096054,-0.468288168448986,
-0.464222616924401,-0.461752686018684,-0.459826440263581,-0.457727438197202,
-0.454346640793039,-0.442698609209978,-0.422751877753202,-0.3822367226858,
-0.368432767544484,-0.366154858310516,-0.364776359165642,-0.363702399926604,
-0.362482247943189,-0.360363834948695,-0.351283378875099,-0.302619137294814,
-0.275743799216676,-0.271702727583868,-0.269240048974191,-0.26731488249938,
-0.265212415497841,-0.26181574843141,-0.250008412649237,-0.200730365289813,
-0.17635237101312,-0.173545085341349,-0.172180280486157,-0.171109983227981,
-0.171104885878602,-0.17109985722943,-0.171094896126241,-0.171090001282427,
-0.171085171468235,-0.171080405514773,-0.171075702294062,-0.171071060659346,
-0.169836383949264,-0.167670621475185,-0.164939434463173,-0.159107639417711,
-0.141509908166866,-0.112041215706876,-0.0833372334848896,-0.0792513797624821,
-0.0767753920112682,-0.0748481662874705,-0.0727518684183954,-0.069383726633986,
-0.0578620861435787,-0.0382304328438444,-0.000564480343473832),
 .UNSPECIFIED.);
#1299=B_SPLINE_CURVE_WITH_KNOTS('',3,(#44732,#44733,#44734,#44735,#44736,
#44737,#44738,#44739,#44740,#44741,#44742,#44743,#44744,#44745,#44746,#44747,
#44748,#44749,#44750,#44751,#44752,#44753,#44754,#44755,#44756,#44757,#44758,
#44759,#44760,#44761,#44762,#44763,#44764,#44765,#44766,#44767,#44768,#44769,
#44770,#44771,#44772,#44773,#44774,#44775,#44776,#44777,#44778,#44779,#44780,
#44781,#44782,#44783,#44784,#44785,#44786,#44787),.UNSPECIFIED.,.F.,.F.,
(4,2,2,2,2,2,2,2,2,2,2,2,2,2,2,2,2,2,2,2,2,2,2,2,2,2,2,4),(-2.43183342158011,
-2.41479196364183,-2.41296275867932,-2.41173372599316,-2.41072356638809,
-2.40965298480507,-2.40828648451585,-2.40609834958051,-2.39407687652996,
-2.3855012686747,-2.35151229207745,-2.33166344231834,-2.32005262071449,
-2.31667513422864,-2.31457657965056,-2.31264966593554,-2.31017738443359,
-2.30610472255568,-2.27800301443796,-2.23010211394347,-2.22433170748115,
-2.22162094479725,-2.2194489721092,-2.21822263232837,-2.21715280704875,
-2.21579726637834,-2.21303773047925,-2.18988230660751),.UNSPECIFIED.);
#1300=B_SPLINE_CURVE_WITH_KNOTS('',3,(#44788,#44789,#44790,#44791,#44792,
#44793,#44794,#44795,#44796,#44797,#44798,#44799,#44800,#44801,#44802,#44803,
#44804,#44805,#44806,#44807,#44808,#44809,#44810,#44811,#44812,#44813,#44814,
#44815,#44816,#44817,#44818,#44819,#44820,#44821,#44822,#44823,#44824,#44825,
#44826,#44827,#44828,#44829,#44830,#44831,#44832,#44833,#44834,#44835,#44836,
#44837,#44838,#44839,#44840,#44841,#44842,#44843,#44844,#44845,#44846,#44847,
#44848,#44849,#44850,#44851,#44852,#44853,#44854,#44855,#44856,#44857,#44858,
#44859,#44860,#44861,#44862,#44863,#44864,#44865,#44866,#44867,#44868,#44869,
#44870,#44871,#44872,#44873,#44874,#44875,#44876,#44877,#44878,#44879,#44880,
#44881,#44882,#44883,#44884,#44885,#44886,#44887,#44888,#44889,#44890,#44891,
#44892,#44893,#44894,#44895,#44896,#44897,#44898,#44899,#44900,#44901,#44902,
#44903,#44904,#44905,#44906,#44907,#44908,#44909,#44910,#44911,#44912,#44913,
#44914,#44915,#44916,#44917,#44918,#44919,#44920,#44921,#44922,#44923,#44924,
#44925,#44926,#44927,#44928,#44929,#44930,#44931,#44932,#44933,#44934,#44935,
#44936,#44937,#44938,#44939,#44940,#44941,#44942,#44943,#44944,#44945,#44946,
#44947,#44948,#44949,#44950,#44951,#44952,#44953,#44954,#44955,#44956,#44957,
#44958,#44959,#44960,#44961,#44962,#44963,#44964,#44965,#44966,#44967,#44968,
#44969,#44970,#44971,#44972,#44973,#44974,#44975,#44976,#44977,#44978,#44979,
#44980,#44981,#44982,#44983,#44984,#44985,#44986,#44987,#44988,#44989,#44990,
#44991,#44992,#44993,#44994,#44995,#44996,#44997,#44998,#44999,#45000,#45001,
#45002,#45003,#45004,#45005,#45006,#45007),.UNSPECIFIED.,.F.,.F.,(4,2,2,
2,2,2,2,2,2,2,2,2,2,2,2,2,2,2,2,2,2,2,2,2,2,2,2,2,2,2,2,2,2,2,2,2,2,2,2,
2,2,2,2,2,2,2,2,2,2,2,2,2,2,2,2,2,2,2,2,2,2,2,2,2,2,2,2,2,2,2,2,2,2,2,2,
2,2,2,2,2,2,2,2,2,2,2,2,2,2,2,2,2,2,2,2,2,2,2,2,2,2,2,2,2,2,2,2,2,2,4),
(-1.45799153533436,-1.45651417706466,-1.45403624613571,-1.44994405409045,
-1.42097709480293,-1.39209919572151,-1.36867732705061,-1.36439485985391,
-1.362776523103,-1.36166600052332,-1.3606654929809,-1.35904417830258,-1.3550473207155,
-1.312064391649,-1.28580827308421,-1.27660644739737,-1.27001644747882,-1.26728761919184,
-1.26532537659116,-1.26354098881585,-1.26070621604771,-1.25396336127136,
-1.21576901676488,-1.17622344647632,-1.17197318108443,-1.17030952396949,
-1.16930104917613,-1.168198464086,-1.16662023684018,-1.16260083811927,-1.14195464856034,
-1.10018730489828,-1.08040023259733,-1.07663015773493,-1.07422242216828,
-1.07230832110076,-1.07015208760232,-1.0665134259311,-1.05198792680941,
-1.02398010559419,-0.983675247784505,-0.979450802613525,-0.977791304773497,
-0.976783596635041,-0.975680235883655,-0.974098167166473,-0.970054359585526,
-0.921162681269848,-0.88856605718916,-0.884410662117065,-0.88191416045053,
-0.87998371854712,-0.877896633990358,-0.874570909331996,-0.863460421535659,
-0.844833376384835,-0.804420847416611,-0.788672332436125,-0.786089591973712,
-0.784752853919872,-0.783684319587785,-0.782418433068192,-0.780090907330598,
-0.767532812312541,-0.736725087439566,-0.695994912039856,-0.691871033066363,
-0.689383743796099,-0.687454677948254,-0.685363344218717,-0.682018387597583,
-0.670724481050623,-0.651653325621746,-0.612535221539828,-0.59619701944811,
-0.593592138557923,-0.592250623469297,-0.59118182495394,-0.589919787918668,
-0.587610145699826,-0.575409100155573,-0.513140824030563,-0.501526108351775,
-0.49801047818145,-0.495881615044767,-0.493962817257088,-0.49150944246179,
-0.48645173660807,-0.479883294958928,-0.464121348109848,-0.42038480522287,
-0.415022082955552,-0.403241580038739,-0.401066651294722,-0.399704232860486,
-0.398634098053535,-0.397388125173552,-0.395152186636372,-0.384287760935015,
-0.359224624415685,-0.314103749499636,-0.307524123919663,-0.304997410533382,
-0.3031774375461,-0.301241361157506,-0.298663590341235,-0.292945697496344,
-0.269581291711543,-0.244309336638491,-0.242475885032187),.UNSPECIFIED.);
#1301=B_SPLINE_CURVE_WITH_KNOTS('',3,(#45012,#45013,#45014,#45015,#45016,
#45017,#45018,#45019,#45020,#45021,#45022,#45023,#45024,#45025,#45026,#45027,
#45028,#45029,#45030,#45031,#45032,#45033,#45034,#45035,#45036,#45037,#45038,
#45039,#45040,#45041,#45042,#45043,#45044,#45045,#45046,#45047,#45048,#45049,
#45050,#45051,#45052,#45053,#45054,#45055,#45056,#45057,#45058,#45059,#45060,
#45061,#45062,#45063,#45064,#45065,#45066,#45067,#45068,#45069,#45070,#45071,
#45072,#45073,#45074,#45075,#45076,#45077,#45078,#45079,#45080,#45081,#45082,
#45083,#45084,#45085,#45086,#45087,#45088,#45089,#45090,#45091,#45092,#45093,
#45094,#45095,#45096,#45097,#45098,#45099,#45100,#45101,#45102,#45103,#45104,
#45105,#45106,#45107,#45108,#45109,#45110,#45111,#45112,#45113,#45114,#45115,
#45116,#45117,#45118,#45119,#45120,#45121,#45122,#45123,#45124,#45125,#45126,
#45127,#45128,#45129,#45130,#45131,#45132,#45133,#45134,#45135,#45136,#45137,
#45138,#45139,#45140,#45141,#45142,#45143,#45144,#45145,#45146,#45147,#45148,
#45149,#45150,#45151,#45152,#45153,#45154,#45155,#45156,#45157,#45158,#45159,
#45160,#45161,#45162,#45163,#45164,#45165,#45166,#45167,#45168,#45169,#45170,
#45171,#45172,#45173,#45174,#45175,#45176,#45177,#45178,#45179,#45180,#45181,
#45182,#45183,#45184,#45185,#45186,#45187,#45188,#45189,#45190,#45191,#45192,
#45193,#45194,#45195,#45196,#45197,#45198,#45199,#45200,#45201,#45202,#45203,
#45204,#45205,#45206,#45207,#45208,#45209,#45210,#45211,#45212,#45213,#45214,
#45215,#45216,#45217,#45218,#45219,#45220,#45221,#45222,#45223,#45224,#45225,
#45226,#45227),.UNSPECIFIED.,.F.,.F.,(4,2,2,2,2,2,2,2,2,2,2,2,2,2,2,2,2,
2,2,2,2,2,2,2,2,2,2,2,2,2,2,2,2,2,2,2,2,2,2,2,2,2,2,2,2,2,2,2,2,2,2,2,2,
2,2,2,2,2,2,2,2,2,2,2,2,2,2,2,2,2,2,2,2,2,2,2,2,2,2,2,2,2,2,2,2,2,2,2,2,
2,2,2,2,2,2,2,2,2,2,2,2,2,2,2,2,2,2,4),(-2.18954711984868,-2.18843508427736,
-2.18217025824943,-2.13183465909379,-2.11041638015107,-2.10062439548328,
-2.09839846759916,-2.09714683209159,-2.09607728962157,-2.09472262747542,
-2.09196658823948,-2.05908052686512,-2.03399035419614,-2.01041420920415,
-2.004668434598,-2.00208552494448,-2.000148553169,-1.99832989437154,-1.99580844475497,
-1.98926290823627,-1.9434473845648,-1.91885340361622,-1.90810563330579,
-1.90587650964589,-1.90463197419128,-1.90356159367554,-1.90219695933854,
-1.89939094106571,-1.8750170619244,-1.82575882625216,-1.81395368239914,
-1.81055698808115,-1.8084543541203,-1.80652893391879,-1.80406579064773,
-1.80002362590504,-1.77313142876445,-1.7244262815198,-1.71535236617163,
-1.71323416964948,-1.71201394404838,-1.71093978102919,-1.7095608560479,
-1.70728191373387,-1.69352812041669,-1.68459733085101,-1.63461952082228,
-1.62161915620125,-1.61810943021373,-1.61598173919837,-1.61406245397801,
-1.61160631766428,-1.60767664512738,-1.58463005044965,-1.53442712766417,
-1.5230529366638,-1.52078736744537,-1.51953483070341,-1.51846518057668,
-1.51711122998332,-1.51435941743451,-1.48130136576737,-1.45595594057811,
-1.43272012602413,-1.42701792996058,-1.42444267747988,-1.42250665901046,
-1.42068539468321,-1.41815473433718,-1.41155194896732,-1.36660946282598,
-1.34138433543342,-1.3304795426544,-1.32824082624815,-1.32699407969633,
-1.32592375764581,-1.32456172450014,-1.32176950947304,-1.298758299962,-1.26487566894333,
-1.24695088769403,-1.23977632115703,-1.2343519312359,-1.2318279227496,-1.22989946552966,
-1.2280621674189,-1.22494669344176,-1.21644189586132,-1.2159940573012,-1.20206001071282,
-1.17281884631323,-1.15957262311967,-1.13887344489183,-1.13610865929863,
-1.13475219517047,-1.13368245149794,-1.13243198490166,-1.13017564181538,
-1.11896171069095,-1.07048639413291,-1.04568353353247,-1.04170182323602,
-1.03923005824389,-1.03730893557505,-1.03518974466993,-1.03171821005687,
-1.01913498544038,-0.97398342740053),.UNSPECIFIED.);
#1302=B_SPLINE_CURVE_WITH_KNOTS('',3,(#45229,#45230,#45231,#45232,#45233,
#45234,#45235,#45236,#45237,#45238,#45239,#45240,#45241,#45242,#45243,#45244,
#45245,#45246,#45247,#45248,#45249,#45250,#45251,#45252,#45253,#45254,#45255,
#45256,#45257,#45258,#45259,#45260,#45261,#45262,#45263,#45264,#45265,#45266,
#45267,#45268,#45269,#45270,#45271,#45272,#45273,#45274,#45275,#45276,#45277,
#45278,#45279,#45280,#45281,#45282,#45283,#45284,#45285,#45286,#45287,#45288,
#45289,#45290,#45291,#45292,#45293,#45294,#45295,#45296,#45297,#45298,#45299,
#45300,#45301,#45302,#45303,#45304,#45305,#45306,#45307,#45308,#45309,#45310,
#45311,#45312,#45313,#45314,#45315,#45316,#45317,#45318,#45319,#45320,#45321,
#45322),.UNSPECIFIED.,.F.,.F.,(4,2,2,2,2,2,2,2,2,2,2,2,2,2,2,2,2,2,2,2,
2,2,2,2,2,2,2,2,2,2,2,2,2,2,2,2,2,2,2,2,2,2,2,2,2,2,4),(-0.242475885032187,
-0.211311516992314,-0.208556292319953,-0.207201817003389,-0.206208042780248,
-0.206203817915274,-0.206199683161047,-0.206195636544027,-0.206192019441469,
-0.206188420176096,-0.206184838611877,-0.206181274743271,-0.206177728430791,
-0.206174199566654,-0.206170688246241,-0.206167194404566,-0.206163717687113,
-0.20616025810502,-0.206156815386804,-0.206153389527791,-0.206149980554044,
-0.206146588168098,-0.204925604908831,-0.20276948903304,-0.200088336227301,
-0.194405976488265,-0.177506579186398,-0.159876697351341,-0.121865362242285,
-0.11512466485239,-0.112290320204464,-0.110506058339158,-0.108543830494773,
-0.105814801981801,-0.0992232583093638,-0.0900175597048242,-0.0637414610418433,
-0.030333017612405,-0.0224419710486729,-0.0186641397871498,-0.0160563233359045,
-0.0147142666500038,-0.0137075916180399,-0.0126989203002053,-0.0114764548261663,
-0.00966312529024703,-0.000563390165638188),.UNSPECIFIED.);
#1303=B_SPLINE_CURVE_WITH_KNOTS('',3,(#45323,#45324,#45325,#45326,#45327,
#45328,#45329,#45330,#45331,#45332,#45333,#45334,#45335,#45336,#45337,#45338,
#45339,#45340,#45341,#45342,#45343,#45344,#45345,#45346,#45347,#45348,#45349,
#45350,#45351,#45352,#45353,#45354,#45355,#45356,#45357,#45358,#45359,#45360,
#45361,#45362,#45363,#45364,#45365,#45366,#45367,#45368,#45369,#45370,#45371,
#45372,#45373,#45374,#45375,#45376,#45377,#45378,#45379,#45380,#45381,#45382,
#45383,#45384,#45385,#45386,#45387,#45388,#45389,#45390,#45391,#45392,#45393,
#45394,#45395,#45396,#45397,#45398,#45399,#45400,#45401,#45402,#45403,#45404,
#45405,#45406,#45407,#45408,#45409,#45410,#45411,#45412,#45413,#45414,#45415,
#45416,#45417,#45418,#45419,#45420,#45421,#45422,#45423,#45424,#45425,#45426,
#45427,#45428,#45429,#45430,#45431,#45432,#45433,#45434,#45435,#45436,#45437,
#45438,#45439,#45440,#45441,#45442,#45443,#45444,#45445,#45446,#45447,#45448,
#45449,#45450,#45451,#45452,#45453,#45454,#45455,#45456,#45457,#45458,#45459,
#45460,#45461,#45462,#45463,#45464,#45465,#45466,#45467,#45468,#45469,#45470,
#45471,#45472,#45473,#45474,#45475,#45476,#45477,#45478,#45479,#45480,#45481,
#45482,#45483,#45484,#45485,#45486,#45487,#45488,#45489,#45490,#45491,#45492,
#45493,#45494,#45495,#45496,#45497,#45498),.UNSPECIFIED.,.F.,.F.,(4,2,2,
2,2,2,2,2,2,2,2,2,2,2,2,2,2,2,2,2,2,2,2,2,2,2,2,2,2,2,2,2,2,2,2,2,2,2,2,
2,2,2,2,2,2,2,2,2,2,2,2,2,2,2,2,2,2,2,2,2,2,2,2,2,2,2,2,2,2,2,2,2,2,2,2,
2,2,2,2,2,2,2,2,2,2,2,2,4),(-2.43201023192336,-2.41829679723027,-2.36793049198057,
-2.35539612686519,-2.35192890121182,-2.34981050631577,-2.34788890998877,
-2.34541485945137,-2.34142600117818,-2.31640932036142,-2.27985334704831,
-2.26453959265631,-2.25920982259474,-2.25664833554951,-2.25459398025459,
-2.2533838605833,-2.25234705228238,-2.25098690718971,-2.24820391392017,
-2.22587235576064,-2.17578201699542,-2.16291765311221,-2.15942013393211,
-2.15729509797618,-2.15537514895323,-2.15291391380682,-2.14896747144052,
-2.125371311619,-2.07569592984939,-2.06436883949363,-2.062105862622,-2.06085386588979,
-2.05978412844462,-2.05842936515504,-2.05567359874798,-2.02276743251201,
-1.99769575491309,-1.97410569598012,-1.96835760453313,-1.9657739773459,
-1.96383659677978,-1.96201764838483,-1.95949594751044,-1.95295063806469,
-1.90713085053513,-1.88252667180167,-1.8717754558079,-1.86954581916108,
-1.86830102531784,-1.86723044015574,-1.86586556782549,-1.86305913731539,
-1.83869492073372,-1.78941868214392,-1.7776059289547,-1.7742080489118,-1.7721048918289,
-1.77017913307196,-1.76771575004489,-1.76367360461862,-1.73680818062124,
-1.68817847211972,-1.67899846068376,-1.67687226288339,-1.67565012657541,
-1.67457607582821,-1.67319958845993,-1.67092937937136,-1.65728919869154,
-1.61602007559205,-1.59646825030886,-1.58497652423159,-1.58161076819369,
-1.57951457513966,-1.5775865162642,-1.57510816548938,-1.57101559162511,
-1.5420689196837,-1.51317274152033,-1.49528784424624,-1.48642682118663,
-1.48432416439205,-1.48310723498795,-1.48203217347373,-1.48064720948833,
-1.47834817101076,-1.46407236322947,-1.45834644240502),.UNSPECIFIED.);
#1304=B_SPLINE_CURVE_WITH_KNOTS('',3,(#45504,#45505,#45506,#45507,#45508,
#45509,#45510,#45511,#45512,#45513,#45514,#45515,#45516,#45517,#45518,#45519,
#45520,#45521,#45522,#45523,#45524,#45525,#45526,#45527,#45528,#45529,#45530,
#45531,#45532,#45533,#45534,#45535,#45536,#45537,#45538,#45539,#45540,#45541,
#45542,#45543,#45544,#45545,#45546,#45547,#45548,#45549,#45550,#45551,#45552,
#45553,#45554,#45555,#45556,#45557,#45558,#45559,#45560,#45561,#45562,#45563,
#45564,#45565,#45566,#45567,#45568,#45569,#45570,#45571,#45572,#45573,#45574,
#45575,#45576,#45577,#45578,#45579,#45580,#45581,#45582,#45583,#45584,#45585,
#45586,#45587,#45588,#45589,#45590,#45591,#45592,#45593,#45594,#45595,#45596,
#45597,#45598,#45599,#45600,#45601,#45602,#45603,#45604,#45605,#45606,#45607,
#45608,#45609,#45610,#45611,#45612,#45613,#45614,#45615,#45616,#45617,#45618,
#45619,#45620,#45621,#45622,#45623,#45624,#45625,#45626,#45627,#45628,#45629,
#45630,#45631,#45632,#45633,#45634,#45635,#45636,#45637,#45638,#45639,#45640,
#45641,#45642,#45643,#45644,#45645,#45646,#45647,#45648,#45649,#45650,#45651,
#45652,#45653,#45654,#45655,#45656,#45657,#45658,#45659,#45660,#45661,#45662,
#45663,#45664,#45665,#45666,#45667,#45668,#45669,#45670,#45671,#45672,#45673,
#45674,#45675,#45676,#45677,#45678,#45679,#45680,#45681),.UNSPECIFIED.,
 .F.,.F.,(4,2,2,2,2,2,2,2,2,2,2,2,2,2,2,2,2,2,2,2,2,2,2,2,2,2,2,2,2,2,2,
2,2,2,2,2,2,2,2,2,2,2,2,2,2,2,2,2,2,2,2,2,2,2,2,2,2,2,2,2,2,2,2,2,2,2,2,
2,2,2,2,2,2,2,2,2,2,2,2,2,2,2,2,2,2,2,2,2,4),(-0.973746388460305,-0.964026499357242,
-0.925008914880137,-0.920865169477403,-0.918372219975626,-0.916442493527153,
-0.914354160686515,-0.911022069794456,-0.899848797001676,-0.88106940061312,
-0.839700173427234,-0.833881447720076,-0.824522836744943,-0.822304412055297,
-0.821048852704035,-0.819979656117997,-0.81863015094139,-0.815899968897619,
-0.785792992478453,-0.734974663461587,-0.728860798445624,-0.726411095616516,
-0.724611015576052,-0.722662294579658,-0.720007982801653,-0.713858226769834,
-0.687021263813445,-0.64776263229401,-0.632581134377751,-0.630246352083531,
-0.628851155971027,-0.627775081247309,-0.626564790244736,-0.624491037538719,
-0.615999144676198,-0.599259944139691,-0.562511411147729,-0.539607283698179,
-0.535682879100219,-0.533228434301822,-0.531309492542256,-0.529181179666661,
-0.525668107005635,-0.512628410796253,-0.462660004739359,-0.45370597408244,
-0.439975617433199,-0.437699381671416,-0.43632131094361,-0.435247319506291,
-0.434026713992213,-0.431906557439573,-0.422804055243892,-0.374152722725726,
-0.3472814055064,-0.343240129129532,-0.340777274139774,-0.338851938760359,
-0.336749255803814,-0.333352169891232,-0.321732819678866,-0.301779703417091,
-0.257494562288134,-0.247107054256051,-0.245014733199427,-0.243677455637427,
-0.242608974608807,-0.241343720371571,-0.23901884340004,-0.226644628619756,
-0.194653327343986,-0.160038725792635,-0.15207563127623,-0.149041812479143,
-0.147220511019105,-0.14528495563211,-0.143388340674838,-0.139122847388627,
-0.113835882725883,-0.0937843897785946,-0.0578023244281912,-0.0534078898783422,
-0.0517209993357558,-0.0507081033863247,-0.0496094269939885,-0.0480513976124226,
-0.0462896458552489,-0.0431471780912219,-0.000564085736078712),
 .UNSPECIFIED.);
#1305=B_SPLINE_CURVE_WITH_KNOTS('',3,(#45682,#45683,#45684,#45685,#45686,
#45687,#45688,#45689,#45690,#45691,#45692,#45693,#45694,#45695,#45696,#45697,
#45698,#45699,#45700,#45701,#45702,#45703,#45704,#45705,#45706,#45707,#45708,
#45709,#45710,#45711,#45712,#45713,#45714,#45715,#45716,#45717,#45718,#45719,
#45720,#45721,#45722,#45723,#45724,#45725,#45726,#45727,#45728,#45729,#45730,
#45731,#45732,#45733,#45734,#45735),.UNSPECIFIED.,.F.,.F.,(4,2,2,2,2,2,
2,2,2,2,2,2,2,2,2,2,2,2,2,2,2,2,2,2,2,2,4),(-2.43166641639941,-2.4035822623252,
-2.39321099227628,-2.39010269405064,-2.38796676598012,-2.38588059230468,
-2.38395033182375,-2.38145313275954,-2.37729450241099,-2.34422996694495,
-2.32249358193877,-2.29712234873137,-2.29217173168749,-2.29085510082182,
-2.28961152279337,-2.28854122649356,-2.28717574386714,-2.28436476465057,
-2.25935341469091,-2.23098557959375,-2.21075322911876,-2.20297145278707,
-2.19723601869153,-2.19466096879313,-2.19271686184005,-2.19091029731729,
-2.18954711984868),.UNSPECIFIED.);
#1306=B_SPLINE_CURVE_WITH_KNOTS('',3,(#45736,#45737,#45738,#45739,#45740,
#45741,#45742,#45743,#45744,#45745,#45746,#45747,#45748,#45749,#45750,#45751,
#45752,#45753,#45754,#45755,#45756,#45757,#45758,#45759,#45760,#45761,#45762,
#45763,#45764,#45765,#45766,#45767,#45768,#45769,#45770,#45771,#45772,#45773,
#45774,#45775,#45776,#45777,#45778,#45779,#45780,#45781,#45782,#45783,#45784,
#45785,#45786,#45787,#45788,#45789,#45790,#45791,#45792,#45793,#45794,#45795,
#45796,#45797,#45798,#45799,#45800,#45801,#45802,#45803,#45804,#45805,#45806,
#45807,#45808,#45809,#45810,#45811,#45812,#45813,#45814,#45815,#45816,#45817,
#45818,#45819,#45820,#45821,#45822,#45823,#45824,#45825,#45826,#45827,#45828,
#45829,#45830,#45831,#45832,#45833,#45834,#45835,#45836,#45837,#45838,#45839,
#45840,#45841,#45842,#45843,#45844,#45845,#45846,#45847,#45848,#45849,#45850,
#45851,#45852,#45853,#45854,#45855,#45856,#45857,#45858,#45859,#45860,#45861,
#45862,#45863,#45864,#45865,#45866,#45867,#45868,#45869,#45870,#45871,#45872,
#45873,#45874,#45875,#45876,#45877,#45878,#45879,#45880,#45881,#45882,#45883,
#45884,#45885,#45886,#45887,#45888,#45889,#45890,#45891,#45892,#45893,#45894,
#45895,#45896,#45897,#45898,#45899,#45900,#45901,#45902,#45903,#45904,#45905,
#45906,#45907,#45908,#45909,#45910,#45911,#45912,#45913,#45914,#45915,#45916,
#45917,#45918,#45919,#45920,#45921,#45922,#45923,#45924,#45925,#45926,#45927,
#45928,#45929,#45930,#45931,#45932,#45933,#45934,#45935,#45936,#45937,#45938,
#45939,#45940,#45941,#45942,#45943),.UNSPECIFIED.,.F.,.F.,(4,2,2,2,2,2,
2,2,2,2,2,2,2,2,2,2,2,2,2,2,2,2,2,2,2,2,2,2,2,2,2,2,2,2,2,2,2,2,2,2,2,2,
2,2,2,2,2,2,2,2,2,2,2,2,2,2,2,2,2,2,2,2,2,2,2,2,2,2,2,2,2,2,2,2,2,2,2,2,
2,2,2,2,2,2,2,2,2,2,2,2,2,2,2,2,2,2,2,2,2,2,2,2,2,4),(-1.45834644240502,
-1.42374471371173,-1.39700114213766,-1.39086112834712,-1.38820797082164,
-1.38625894713713,-1.38445777320206,-1.38200532844103,-1.37587813168322,
-1.3251133445948,-1.3222390361035,-1.29486859212337,-1.29216182246573,-1.29081674281652,
-1.28974749362049,-1.28848771402035,-1.28625195090993,-1.27667900905391,
-1.216226484536,-1.20075922531249,-1.19692105602227,-1.1946980654169,-1.19279023294875,
-1.19047343204715,-1.18609194423199,-1.15576595879912,-1.12851542892481,
-1.10243564931261,-1.09961715089813,-1.09824993184173,-1.09717919368131,
-1.09593614685932,-1.09371437808789,-1.08309166203224,-1.05899798684945,
-1.01250427586629,-1.00600402375574,-1.00348957544059,-1.00167257192859,
-0.999734211052079,-0.997144026022698,-0.991359297349661,-0.967479841021998,
-0.934952977495644,-0.909894206510875,-0.907081910778686,-0.905715947616078,
-0.904645353996951,-0.90340151334074,-0.901175965658991,-0.890489896755449,
-0.866145513954071,-0.820009780551091,-0.813486763016654,-0.810968729891711,
-0.809150834333133,-0.807213098156615,-0.804626463728066,-0.798861080013256,
-0.775131789383233,-0.743067991407038,-0.717377792553701,-0.714561399194917,
-0.713194659663292,-0.712124038135746,-0.710880830152675,-0.708658046312723,
-0.698016575058588,-0.673847703047412,-0.627467128808157,-0.620960165856165,
-0.618444757656858,-0.616627595116704,-0.614689561211031,-0.6121006695439,
-0.606322435305216,-0.582492043188745,-0.550098296407065,-0.524857081595505,
-0.52204365583862,-0.52067753398953,-0.519607002770865,-0.518363448664692,
-0.516138939268841,-0.505467969160891,-0.481181940966927,-0.434971472167958,
-0.4284531672314,-0.425936003306884,-0.424118427322185,-0.42218074601925,
-0.419593692658138,-0.413825308436699,-0.39007094459325,-0.365100651915328,
-0.332263432392804,-0.329504468238845,-0.328149175243173,-0.327079531844555,
-0.325828230566595,-0.323567994022054,-0.312284983825815,-0.263069673735912,
-0.242708007470264),.UNSPECIFIED.);
#1307=B_SPLINE_CURVE_WITH_KNOTS('',3,(#45948,#45949,#45950,#45951,#45952,
#45953,#45954,#45955,#45956,#45957,#45958,#45959,#45960,#45961,#45962,#45963,
#45964,#45965,#45966,#45967,#45968,#45969,#45970,#45971,#45972,#45973,#45974,
#45975,#45976,#45977,#45978,#45979,#45980,#45981,#45982,#45983,#45984,#45985,
#45986,#45987,#45988,#45989,#45990,#45991,#45992,#45993,#45994,#45995,#45996,
#45997,#45998,#45999,#46000,#46001,#46002,#46003,#46004,#46005,#46006,#46007,
#46008,#46009,#46010,#46011,#46012,#46013,#46014,#46015,#46016,#46017,#46018,
#46019,#46020,#46021,#46022,#46023,#46024,#46025,#46026,#46027,#46028,#46029,
#46030,#46031,#46032,#46033,#46034,#46035,#46036,#46037,#46038,#46039,#46040,
#46041,#46042,#46043,#46044,#46045,#46046,#46047,#46048,#46049,#46050,#46051,
#46052,#46053,#46054,#46055,#46056,#46057,#46058,#46059,#46060,#46061,#46062,
#46063,#46064,#46065,#46066,#46067,#46068,#46069,#46070,#46071,#46072,#46073,
#46074,#46075,#46076,#46077,#46078,#46079,#46080,#46081,#46082,#46083,#46084,
#46085,#46086,#46087,#46088,#46089,#46090,#46091,#46092,#46093,#46094,#46095,
#46096,#46097,#46098,#46099,#46100,#46101,#46102,#46103,#46104,#46105,#46106,
#46107,#46108,#46109,#46110,#46111,#46112,#46113,#46114,#46115,#46116,#46117,
#46118,#46119,#46120,#46121,#46122,#46123,#46124,#46125,#46126,#46127,#46128,
#46129,#46130,#46131,#46132,#46133,#46134,#46135,#46136,#46137,#46138,#46139,
#46140,#46141,#46142,#46143,#46144,#46145,#46146,#46147,#46148,#46149,#46150,
#46151,#46152,#46153,#46154,#46155,#46156,#46157,#46158,#46159,#46160,#46161,
#46162,#46163,#46164,#46165,#46166,#46167,#46168,#46169,#46170,#46171,#46172,
#46173,#46174,#46175,#46176,#46177),.UNSPECIFIED.,.F.,.F.,(4,2,2,2,2,2,
2,2,2,2,2,2,2,2,2,2,2,2,2,2,2,2,2,2,2,2,2,2,2,2,2,2,2,2,2,2,2,2,2,2,2,2,
2,2,2,2,2,2,2,2,2,2,2,2,2,2,2,2,2,2,2,2,2,2,2,2,2,2,2,2,2,2,2,2,2,2,2,2,
2,2,2,2,2,2,2,2,2,2,2,2,2,2,2,2,2,2,2,2,2,2,2,2,2,2,2,2,2,2,2,2,2,2,2,2,
4),(-2.18892388094417,-2.1843488704546,-2.17199046622995,-2.16967335405779,
-2.16840995352589,-2.16734162029971,-2.16600274244,-2.16340894683327,-2.14735269665759,
-2.1407038627092,-2.09031069828951,-2.07783695997642,-2.07437631571477,
-2.07225991018016,-2.07033879336962,-2.06786349888921,-2.06386881771297,
-2.03877015875202,-1.99057038181363,-1.97938330526312,-1.97712884419471,
-1.97587897099879,-1.97480945309321,-1.97345292163124,-1.97068682159884,
-1.94992345679077,-1.91985680301451,-1.88711406842814,-1.88267922302751,
-1.88035180266203,-1.87844416353084,-1.87623150446256,-1.87243612394093,
-1.85752223922304,-1.84935861118924,-1.81155852248697,-1.78976721460458,
-1.78563730698772,-1.78404221216232,-1.78293651519665,-1.78193185046896,
-1.78028742345155,-1.77615192579642,-1.73433178542166,-1.69480400245381,
-1.69026818711351,-1.68791986831109,-1.68601108594607,-1.68381490241827,
-1.68009089967871,-1.66595926189511,-1.65640861839957,-1.60585411835963,
-1.59445066798587,-1.59218386973542,-1.59093125500479,-1.58986190700698,
-1.5885088105629,-1.58576027760468,-1.55259324215636,-1.52703410495093,
-1.5040829436025,-1.49841850040637,-1.49585051131698,-1.49391600210762,
-1.49209325908414,-1.48955589128635,-1.4829069899875,-1.43923754022666,
-1.41307723349706,-1.40194816402122,-1.3996968001989,-1.39844749429663,
-1.39737775150074,-1.39602002263345,-1.39324846733114,-1.37205880270645,
-1.33841266162355,-1.31911370763122,-1.3077258025411,-1.30437137600113,
-1.30227810235601,-1.30034993680233,-1.29786755992181,-1.29375992426504,
-1.26407275131254,-1.23619952520191,-1.2277150158654,-1.21569054920526,
-1.2090190516832,-1.2070297305276,-1.20583820086272,-1.2047570216075,-1.20330108139657,
-1.20001032803684,-1.19548653160004,-1.18350163005669,-1.14508698648702,
-1.11734597306032,-1.11328274193258,-1.11081342320432,-1.10888717753662,
-1.10678769304258,-1.10340505283826,-1.09173993784322,-1.07175099433473,
-1.03349084653365,-1.01764228267197,-1.01505590478967,-1.01371847762994,
-1.01265003097012,-1.01138499820538,-1.0090609999237,-0.996570127006823,
-0.973746388460305),.UNSPECIFIED.);
#1308=B_SPLINE_CURVE_WITH_KNOTS('',3,(#46179,#46180,#46181,#46182,#46183,
#46184,#46185,#46186,#46187,#46188,#46189,#46190,#46191,#46192,#46193,#46194,
#46195,#46196,#46197,#46198,#46199,#46200,#46201,#46202,#46203,#46204,#46205,
#46206,#46207,#46208,#46209,#46210,#46211,#46212,#46213,#46214,#46215,#46216,
#46217,#46218,#46219,#46220,#46221,#46222,#46223,#46224,#46225,#46226,#46227,
#46228,#46229,#46230,#46231,#46232,#46233,#46234,#46235,#46236),
 .UNSPECIFIED.,.F.,.F.,(4,2,2,2,2,2,2,2,2,2,2,2,2,2,2,2,2,2,2,2,2,2,2,2,
2,2,2,2,4),(-0.242708007470264,-0.239038576650452,-0.235080102347808,-0.232615348612138,
-0.230695119825303,-0.228905579258431,-0.225960965083586,-0.217282374486274,
-0.203984666361365,-0.173075737777023,-0.142287490478921,-0.137838005971676,
-0.136142596534498,-0.135128081889868,-0.13403077769428,-0.13247988995464,
-0.128632028598946,-0.112421686013435,-0.0933912558259936,-0.0727848811857325,
-0.0467009348712936,-0.0426806923945847,-0.0402239591333887,-0.03829937000933,
-0.0365110374283958,-0.0344440954814045,-0.0315055729894532,-0.0221457821256158,
-0.000563535122424079),.UNSPECIFIED.);
#1309=B_SPLINE_CURVE_WITH_KNOTS('',3,(#46237,#46238,#46239,#46240,#46241,
#46242,#46243,#46244,#46245,#46246,#46247,#46248,#46249,#46250,#46251,#46252,
#46253,#46254,#46255,#46256,#46257,#46258,#46259,#46260,#46261,#46262,#46263,
#46264,#46265,#46266,#46267,#46268,#46269,#46270,#46271,#46272,#46273,#46274,
#46275,#46276,#46277,#46278,#46279,#46280,#46281,#46282,#46283,#46284,#46285,
#46286,#46287,#46288,#46289,#46290,#46291,#46292,#46293,#46294,#46295,#46296,
#46297,#46298,#46299,#46300,#46301,#46302,#46303,#46304,#46305,#46306,#46307,
#46308,#46309,#46310,#46311,#46312,#46313,#46314,#46315,#46316,#46317,#46318,
#46319,#46320,#46321,#46322,#46323,#46324,#46325,#46326,#46327,#46328,#46329,
#46330,#46331,#46332,#46333,#46334,#46335,#46336,#46337,#46338,#46339,#46340,
#46341,#46342,#46343,#46344,#46345,#46346,#46347,#46348,#46349,#46350,#46351,
#46352,#46353,#46354,#46355,#46356,#46357,#46358,#46359,#46360,#46361,#46362,
#46363,#46364,#46365,#46366,#46367,#46368,#46369,#46370,#46371,#46372,#46373,
#46374,#46375,#46376,#46377,#46378,#46379,#46380,#46381,#46382,#46383,#46384,
#46385,#46386,#46387,#46388,#46389,#46390,#46391,#46392,#46393,#46394,#46395,
#46396,#46397,#46398,#46399,#46400,#46401,#46402,#46403,#46404,#46405,#46406,
#46407,#46408,#46409,#46410,#46411,#46412),.UNSPECIFIED.,.F.,.F.,(4,2,2,
2,2,2,2,2,2,2,2,2,2,2,2,2,2,2,2,2,2,2,2,2,2,2,2,2,2,2,2,2,2,2,2,2,2,2,2,
2,2,2,2,2,2,2,2,2,2,2,2,2,2,2,2,2,2,2,2,2,2,2,2,2,2,2,2,2,2,2,2,2,2,2,2,
2,2,2,2,2,2,2,2,2,2,2,2,4),(-2.43194619973958,-2.38643680506946,-2.38052321123352,
-2.37647803904974,-2.37489573106975,-2.37379230532373,-2.37278461431682,
-2.37112529738533,-2.36690211191859,-2.32662888658048,-2.306188174032,-2.28517197525235,
-2.28102647635352,-2.27914198623931,-2.27721235382981,-2.27537824489537,
-2.27227871178857,-2.26388014691298,-2.26313491361184,-2.26123166742741,
-2.22060196103296,-2.19600030640739,-2.1852500502366,-2.18302058437965,
-2.18177588197233,-2.18070537300041,-2.17934059463958,-2.1765343467141,
-2.1521699206584,-2.1028983301243,-2.09108713368274,-2.08768956717104,-2.08558657596555,
-2.08366095032344,-2.08119771174316,-2.07715574821591,-2.05028796985693,
-2.00165062761665,-1.99248499313785,-1.9903599399778,-1.98913810992845,
-1.98806409468184,-1.98668735416955,-1.98441611556206,-1.97075747964463,
-1.9616618011355,-1.91156201494552,-1.89870278912326,-1.89520553501889,
-1.89308044058222,-1.89116029706932,-1.88869861559295,-1.88475105782276,
-1.86112640155451,-1.81147215585378,-1.80014639200279,-1.79788334906934,
-1.79663127219778,-1.79556143949831,-1.79420652127494,-1.79145032717075,
-1.75853536815557,-1.73345028878398,-1.70987286559356,-1.70412616749733,
-1.7015426591062,-1.69960516512639,-1.69778596271455,-1.69526367446354,
-1.68871546402137,-1.64293149103429,-1.61829670759328,-1.60753744098217,
-1.60530718476164,-1.60406219037432,-1.60299152366787,-1.60162666482692,
-1.59882065663587,-1.5745261215384,-1.52520397167212,-1.51336406308118,
-1.50996329741003,-1.50785938644611,-1.50593362436087,-1.50347118179144,
-1.49943259432383,-1.47272844074429,-1.45847283624988),.UNSPECIFIED.);
#1310=B_SPLINE_CURVE_WITH_KNOTS('',3,(#46418,#46419,#46420,#46421,#46422,
#46423,#46424,#46425,#46426,#46427,#46428,#46429,#46430,#46431,#46432,#46433,
#46434,#46435,#46436,#46437,#46438,#46439,#46440,#46441,#46442,#46443,#46444,
#46445,#46446,#46447,#46448,#46449,#46450,#46451,#46452,#46453,#46454,#46455,
#46456,#46457,#46458,#46459,#46460,#46461,#46462,#46463,#46464,#46465,#46466,
#46467,#46468,#46469,#46470,#46471,#46472,#46473,#46474,#46475,#46476,#46477,
#46478,#46479,#46480,#46481,#46482,#46483,#46484,#46485,#46486,#46487,#46488,
#46489,#46490,#46491,#46492,#46493,#46494,#46495,#46496,#46497,#46498,#46499,
#46500,#46501,#46502,#46503,#46504,#46505,#46506,#46507,#46508,#46509,#46510,
#46511,#46512,#46513,#46514,#46515,#46516,#46517,#46518,#46519,#46520,#46521,
#46522,#46523,#46524,#46525,#46526,#46527,#46528,#46529,#46530,#46531,#46532,
#46533,#46534,#46535,#46536,#46537,#46538,#46539,#46540,#46541,#46542,#46543,
#46544,#46545,#46546,#46547,#46548,#46549,#46550,#46551,#46552,#46553,#46554,
#46555,#46556,#46557,#46558,#46559,#46560,#46561,#46562,#46563,#46564,#46565,
#46566,#46567,#46568),.UNSPECIFIED.,.F.,.F.,(4,3,3,3,3,3,3,3,3,3,3,3,3,
3,3,3,3,3,3,3,3,3,3,3,3,3,3,3,3,3,3,3,3,3,3,3,3,3,3,3,3,3,3,3,3,3,3,3,3,
3,4),(135.088484104361,135.19457077706,135.300665273228,135.406886595447,
135.513169775309,135.619670278263,135.719134631849,135.825008513915,135.93617421847,
136.041760973883,136.147283992731,136.25277968045,136.358284400424,136.463902842808,
136.569587321621,136.67545053338,136.714334150354,136.82020803242,136.931373736974,
137.036960492388,137.142483511235,137.247979198954,137.353483918929,137.459102361313,
137.564786840126,137.670650051885,137.709533668858,137.815407550924,137.926573255479,
138.032160010892,138.13768302974,138.243178717459,138.348683437433,138.454301879818,
138.55998635863,138.66584957039,138.704733187363,138.810607069429,138.921772773984,
139.027359529397,139.132882548245,139.238378235964,139.343882955938,139.449501398322,
139.555185877135,139.661049088894,139.699932705868,139.805771670952,139.911472047979,
140.017065096305,140.120587878827),.UNSPECIFIED.);
#1311=B_SPLINE_CURVE_WITH_KNOTS('',3,(#46569,#46570,#46571,#46572,#46573,
#46574,#46575,#46576,#46577,#46578,#46579,#46580,#46581,#46582,#46583,#46584,
#46585,#46586,#46587,#46588,#46589,#46590,#46591,#46592,#46593,#46594,#46595,
#46596,#46597,#46598,#46599,#46600,#46601,#46602,#46603,#46604,#46605,#46606,
#46607,#46608,#46609,#46610),.UNSPECIFIED.,.F.,.F.,(4,2,2,2,2,2,2,2,2,2,
2,2,2,2,2,2,2,2,2,2,4),(-2.43085120260907,-2.4218930692744,-2.3732304159689,
-2.36414340232433,-2.36202507088455,-2.36080524156356,-2.35973174341889,
-2.35835407650429,-2.35607804526844,-2.34229979991363,-2.33357368029187,
-2.29450145198639,-2.27936350646572,-2.27297675430417,-2.2680761656219,
-2.26566166773466,-2.26381204113711,-2.26197018280592,-2.25882689403973,
-2.25012351517351,-2.18892388094417),.UNSPECIFIED.);
#1312=B_SPLINE_CURVE_WITH_KNOTS('',3,(#46611,#46612,#46613,#46614,#46615,
#46616,#46617,#46618,#46619,#46620,#46621,#46622,#46623,#46624,#46625,#46626,
#46627,#46628,#46629,#46630,#46631,#46632,#46633,#46634,#46635,#46636,#46637,
#46638,#46639,#46640,#46641,#46642,#46643,#46644,#46645,#46646,#46647,#46648,
#46649,#46650,#46651,#46652,#46653,#46654,#46655,#46656,#46657,#46658,#46659,
#46660,#46661,#46662,#46663,#46664,#46665,#46666,#46667,#46668,#46669,#46670,
#46671,#46672,#46673,#46674,#46675,#46676,#46677,#46678,#46679,#46680,#46681,
#46682,#46683,#46684,#46685,#46686,#46687,#46688,#46689,#46690,#46691,#46692,
#46693,#46694,#46695,#46696,#46697,#46698,#46699,#46700,#46701,#46702,#46703,
#46704,#46705,#46706,#46707,#46708,#46709,#46710,#46711,#46712,#46713,#46714,
#46715,#46716,#46717,#46718,#46719,#46720,#46721,#46722,#46723,#46724,#46725,
#46726,#46727,#46728,#46729,#46730,#46731,#46732,#46733,#46734,#46735,#46736,
#46737,#46738,#46739,#46740,#46741,#46742,#46743,#46744,#46745,#46746,#46747,
#46748,#46749,#46750,#46751,#46752,#46753,#46754,#46755,#46756,#46757,#46758,
#46759,#46760,#46761,#46762,#46763,#46764,#46765,#46766,#46767,#46768,#46769,
#46770,#46771,#46772,#46773,#46774,#46775,#46776,#46777,#46778,#46779,#46780,
#46781,#46782,#46783,#46784,#46785,#46786,#46787,#46788,#46789,#46790,#46791,
#46792,#46793,#46794,#46795,#46796,#46797,#46798,#46799,#46800,#46801,#46802,
#46803,#46804,#46805,#46806,#46807,#46808,#46809,#46810,#46811,#46812,#46813,
#46814,#46815,#46816,#46817,#46818,#46819,#46820,#46821,#46822,#46823,#46824,
#46825,#46826,#46827,#46828,#46829,#46830,#46831,#46832,#46833,#46834,#46835,
#46836,#46837,#46838),.UNSPECIFIED.,.F.,.F.,(4,2,2,2,2,2,2,2,2,2,2,2,2,
2,2,2,2,2,2,2,2,2,2,2,2,2,2,2,2,2,2,2,2,2,2,2,2,2,2,2,2,2,2,2,2,2,2,2,2,
2,2,2,2,2,2,2,2,2,2,2,2,2,2,2,2,2,2,2,2,2,2,2,2,2,2,2,2,2,2,2,2,2,2,2,2,
2,2,2,2,2,2,2,2,2,2,2,2,2,2,2,2,2,2,2,2,2,2,2,2,2,2,2,2,4),(-1.45847283624988,
-1.42448104976427,-1.41480729857782,-1.41264633664841,-1.41141648204844,
-1.41034366997905,-1.40895616369512,-1.40669886288321,-1.39331110372,-1.38939161230587,
-1.35220191876228,-1.33235836169835,-1.32074869529503,-1.31737074171904,
-1.3152717257304,-1.31334427360727,-1.31087114249934,-1.30679673990829,
-1.27865968173235,-1.23076682075486,-1.22209487069045,-1.22000632946136,
-1.21879237462672,-1.21771641841138,-1.21632575396059,-1.21330956422072,
-1.18514208765776,-1.13244841661113,-1.12655765196056,-1.12414557315679,
-1.12235435477634,-1.12039696035579,-1.11769762176706,-1.11128841518579,
-1.08223935854675,-1.04294581977014,-1.03014229915132,-1.02791330905034,
-1.02653425910949,-1.02546223213671,-1.02422674637145,-1.0220403522293,
-1.01198545223261,-0.990045532705057,-0.94035466596778,-0.934117946781772,
-0.931646853860487,-0.929840811876034,-0.927894911801151,-0.925260896532167,
-0.919231601188733,-0.893401491294308,-0.852753394268094,-0.847835417932028,
-0.837305384501196,-0.835203382475635,-0.83386287443638,-0.832793836131314,
-0.831530294760042,-0.829214734453587,-0.81690711207722,-0.752415906348205,
-0.750508920171359,-0.742220614031927,-0.739137165946123,-0.737306079560877,
-0.735374861676985,-0.732831725764556,-0.727304785851107,-0.705395560581283,
-0.662189960510224,-0.658083806982385,-0.644917449006924,-0.642670973943648,
-0.641286796220091,-0.640214428578387,-0.63898266929941,-0.636812666993299,
-0.627002141650751,-0.60593849674924,-0.554897578235623,-0.548799145697978,
-0.546355118445305,-0.54455616808783,-0.54260575003587,-0.539943890108808,
-0.533752805864446,-0.50657520393874,-0.469630588248447,-0.465537757261919,
-0.452356649907539,-0.450109552699725,-0.448725228570267,-0.447652898983027,
-0.446421354464429,-0.444252135798799,-0.434452030859449,-0.413424504584609,
-0.362328485355368,-0.356238497188287,-0.353795949088853,-0.35199743903901,
-0.350046874928202,-0.347383695745733,-0.34118442484052,-0.313936337359388,
-0.286171739665607,-0.260335079083255,-0.257517883491338,-0.256150979568555,
-0.255080336776874,-0.253837227238005,-0.251614921289972,-0.242510440294479),
 .UNSPECIFIED.);
#1313=B_SPLINE_CURVE_WITH_KNOTS('',3,(#46844,#46845,#46846,#46847,#46848,
#46849,#46850,#46851,#46852,#46853,#46854,#46855,#46856,#46857,#46858,#46859,
#46860,#46861,#46862,#46863,#46864,#46865,#46866,#46867,#46868,#46869,#46870,
#46871,#46872,#46873,#46874,#46875,#46876,#46877,#46878,#46879,#46880,#46881,
#46882,#46883,#46884,#46885,#46886,#46887,#46888,#46889,#46890,#46891,#46892,
#46893,#46894,#46895,#46896,#46897,#46898,#46899,#46900,#46901,#46902,#46903,
#46904,#46905,#46906,#46907,#46908,#46909,#46910,#46911,#46912,#46913,#46914,
#46915,#46916,#46917,#46918,#46919,#46920,#46921,#46922,#46923,#46924,#46925,
#46926,#46927,#46928,#46929,#46930,#46931,#46932,#46933,#46934,#46935,#46936,
#46937,#46938,#46939,#46940,#46941,#46942,#46943,#46944,#46945,#46946,#46947,
#46948,#46949,#46950,#46951,#46952,#46953,#46954,#46955,#46956,#46957,#46958,
#46959,#46960,#46961,#46962,#46963,#46964,#46965,#46966,#46967,#46968,#46969,
#46970,#46971,#46972,#46973,#46974,#46975,#46976,#46977,#46978,#46979,#46980,
#46981,#46982,#46983,#46984,#46985,#46986,#46987,#46988,#46989,#46990,#46991,
#46992,#46993,#46994,#46995,#46996,#46997,#46998,#46999,#47000,#47001,#47002,
#47003,#47004,#47005,#47006,#47007,#47008,#47009,#47010,#47011,#47012,#47013,
#47014,#47015,#47016,#47017,#47018,#47019,#47020,#47021,#47022,#47023,#47024,
#47025),.UNSPECIFIED.,.F.,.F.,(4,2,2,2,2,2,2,2,2,2,2,2,2,2,2,2,2,2,2,2,
2,2,2,2,2,2,2,2,2,2,2,2,2,2,2,2,2,2,2,2,2,2,2,2,2,2,2,2,2,2,2,2,2,2,2,2,
2,2,2,2,2,2,2,2,2,2,2,2,2,2,2,2,2,2,2,2,2,2,2,2,2,2,2,2,2,2,2,2,2,2,4),
(-0.97396649970557,-0.963160677049242,-0.936493329974217,-0.932456435089873,
-0.92999466299771,-0.928069219250143,-0.925965447727417,-0.922564446150021,
-0.910719168795666,-0.861372828057179,-0.837082522994241,-0.834276636619951,
-0.832911899907758,-0.831841362256304,-0.830596547743831,-0.828366701262137,
-0.817610474823226,-0.792987604902333,-0.747238785022208,-0.740691912692005,
-0.73817001886883,-0.736351054949499,-0.734413772548259,-0.731830482143081,
-0.726084016251074,-0.702502908975983,-0.677401453655629,-0.644473610654205,
-0.641717208988461,-0.64036232220085,-0.639292582175733,-0.638040684943666,
-0.63577815854317,-0.624458264319718,-0.57484907492696,-0.55121838206422,
-0.547271206301607,-0.544809692621628,-0.542889649515154,-0.540764634857739,
-0.537267442119368,-0.524407900964139,-0.474283930768112,-0.465354681437526,
-0.451533540689114,-0.449254447227754,-0.447875421872581,-0.44680117185509,
-0.445580825225109,-0.44346238522139,-0.434386540518391,-0.38570445419734,
-0.358836444568864,-0.354785521745208,-0.35231961929378,-0.350393601061566,
-0.348291895541077,-0.344900210592264,-0.333148490768363,-0.31294369840165,
-0.277719852171861,-0.273534786846673,-0.259052848455541,-0.256745409839309,
-0.255358096443446,-0.254282885854908,-0.253067669961399,-0.250972243616042,
-0.242203552825536,-0.224610651414523,-0.175037354543392,-0.173210348356956,
-0.171921917447971,-0.170072966897399,-0.163187272095047,-0.160329254175153,
-0.158540649031897,-0.156725911650928,-0.154172490534364,-0.14854749344977,
-0.140942067916782,-0.121393663295704,-0.0800739361752444,-0.0664513076675939,
-0.064182412995454,-0.0628064564478728,-0.0617326493067222,-0.0605105833603781,
-0.0583840487260259,-0.0491950908041694,-0.000564353419034184),
 .UNSPECIFIED.);
#1314=B_SPLINE_CURVE_WITH_KNOTS('',3,(#47026,#47027,#47028,#47029,#47030,
#47031,#47032,#47033,#47034,#47035,#47036,#47037,#47038,#47039,#47040,#47041,
#47042,#47043,#47044,#47045,#47046,#47047,#47048,#47049,#47050,#47051,#47052,
#47053,#47054,#47055,#47056,#47057,#47058,#47059,#47060,#47061,#47062,#47063,
#47064,#47065),.UNSPECIFIED.,.F.,.F.,(4,3,3,3,3,3,3,3,3,3,3,3,3,4),(140.120587878827,
140.226084307905,140.331587186861,140.437202184293,140.542880897559,140.648740549922,
140.695132224372,140.800694341929,140.906103434911,141.011396551526,141.116620100793,
141.221803227789,141.327013037885,141.371669411541),.UNSPECIFIED.);
#1315=B_SPLINE_CURVE_WITH_KNOTS('',3,(#47067,#47068,#47069,#47070,#47071,
#47072,#47073,#47074,#47075,#47076,#47077,#47078,#47079,#47080,#47081,#47082,
#47083,#47084,#47085,#47086,#47087,#47088,#47089,#47090,#47091,#47092,#47093,
#47094,#47095,#47096,#47097,#47098,#47099,#47100,#47101,#47102,#47103,#47104,
#47105,#47106,#47107,#47108),.UNSPECIFIED.,.F.,.F.,(4,2,2,2,2,2,2,2,2,2,
2,2,2,2,2,2,2,2,2,2,4),(-0.242510440294479,-0.240981513752686,-0.21684452742106,
-0.169409698756096,-0.163471707480922,-0.161115789464972,-0.15916083636883,
-0.157365049449781,-0.15482361530898,-0.148704683956145,-0.140251434050436,
-0.117292739366224,-0.0803531418467185,-0.0672818280338345,-0.0650402297128775,
-0.0636576336542719,-0.0625855799040149,-0.0613531507775264,-0.0591795220341944,
-0.0493108473116508,-0.000564367400856858),.UNSPECIFIED.);
#1316=B_SPLINE_CURVE_WITH_KNOTS('',3,(#47109,#47110,#47111,#47112,#47113,
#47114,#47115,#47116,#47117,#47118,#47119,#47120,#47121,#47122,#47123,#47124,
#47125,#47126,#47127,#47128,#47129,#47130,#47131,#47132,#47133,#47134,#47135,
#47136,#47137,#47138,#47139,#47140,#47141,#47142,#47143,#47144,#47145,#47146,
#47147,#47148,#47149,#47150,#47151,#47152,#47153,#47154,#47155,#47156,#47157,
#47158,#47159,#47160,#47161,#47162,#47163,#47164,#47165,#47166,#47167,#47168,
#47169,#47170,#47171,#47172,#47173,#47174,#47175,#47176,#47177,#47178,#47179,
#47180,#47181,#47182,#47183,#47184,#47185,#47186,#47187,#47188,#47189,#47190,
#47191,#47192,#47193,#47194,#47195,#47196,#47197,#47198,#47199,#47200,#47201,
#47202,#47203,#47204,#47205,#47206,#47207,#47208,#47209,#47210,#47211,#47212,
#47213,#47214,#47215,#47216,#47217,#47218,#47219,#47220,#47221,#47222,#47223,
#47224,#47225,#47226,#47227,#47228,#47229,#47230,#47231,#47232,#47233,#47234,
#47235,#47236,#47237,#47238,#47239,#47240,#47241,#47242,#47243,#47244,#47245,
#47246,#47247,#47248,#47249,#47250,#47251,#47252,#47253,#47254,#47255,#47256,
#47257,#47258,#47259,#47260,#47261,#47262,#47263,#47264,#47265,#47266,#47267,
#47268,#47269,#47270,#47271,#47272,#47273,#47274,#47275,#47276,#47277,#47278,
#47279,#47280,#47281,#47282,#47283,#47284,#47285,#47286,#47287,#47288,#47289,
#47290,#47291,#47292,#47293,#47294,#47295,#47296,#47297,#47298,#47299,#47300,
#47301,#47302,#47303,#47304,#47305,#47306,#47307,#47308,#47309,#47310,#47311,
#47312,#47313,#47314,#47315,#47316,#47317,#47318,#47319,#47320,#47321,#47322,
#47323,#47324,#47325,#47326,#47327,#47328,#47329,#47330,#47331,#47332,#47333,
#47334,#47335,#47336,#47337,#47338),.UNSPECIFIED.,.F.,.F.,(4,2,2,2,2,2,
2,2,2,2,2,2,2,2,2,2,2,2,2,2,2,2,2,2,2,2,2,2,2,2,2,2,2,2,2,2,2,2,2,2,2,2,
2,2,2,2,2,2,2,2,2,2,2,2,2,2,2,2,2,2,2,2,2,2,2,2,2,2,2,2,2,2,2,2,2,2,2,2,
2,2,2,2,2,2,2,2,2,2,2,2,2,2,2,2,2,2,2,2,2,2,2,2,2,2,2,2,2,2,2,2,2,2,2,2,
4),(-2.43130179521416,-2.40521661328843,-2.40210741262236,-2.39997151240219,
-2.3981760791286,-2.39626619950669,-2.39389373123154,-2.39023600490332,
-2.37230348877159,-2.35969568972471,-2.31584478156482,-2.30511357571031,
-2.30288634235593,-2.30164264811573,-2.30057285711815,-2.29920880146605,
-2.29640339207263,-2.27193528943643,-2.25973863257918,-2.2275793913354,
-2.2171313737183,-2.21221386664805,-2.20824241610447,-2.20602490885012,
-2.20600881579687,-2.20599227243346,-2.20597526443617,-2.20595777695779,
-2.20593979463704,-2.20592130162841,-2.20590228038918,-2.20588271280846,
-2.2058625834411,-2.20584187399575,-2.20582056545482,-2.20579863810674,
-2.20577607186008,-2.20575886829018,-2.20573933453463,-2.20571715025449,
-2.20569195021371,-2.20566332153779,-2.20563079088278,-2.20559381851842,
-2.20555178906137,-2.20362595385859,-2.20115553039861,-2.19708694822443,
-2.16926467954086,-2.12119390049976,-2.11245615078168,-2.11036367085829,
-2.10914943017043,-2.10807457879296,-2.10668709414727,-2.10437805449337,
-2.08983741058363,-2.08559487402455,-2.07411127348399,-2.05073267941089,
-2.0304300153756,-2.01863966990622,-2.01524501322652,-2.01314317408843,
-2.01121817092183,-2.008755133366,-2.00471222892042,-1.97781857453458,-1.92909608301112,
-1.92006057449843,-1.91794556695003,-1.91672623711903,-1.91565223400078,
-1.9142727089416,-1.91199111632163,-1.89809976450573,-1.85728076763408,
-1.83763625946661,-1.82610867045518,-1.82274023405638,-1.82064405160731,
-1.81871713202263,-1.81624181394433,-1.81215762847284,-1.7835168878772,
-1.75406980019526,-1.73638282186629,-1.72758586797076,-1.72548868611437,
-1.72427330133332,-1.72319850816391,-1.72181247819941,-1.71950873369246,
-1.70510219572368,-1.70099261770262,-1.66547840417381,-1.6382961237278,
-1.63210507254481,-1.62944377751171,-1.62749397557211,-1.62569573055,-1.62325287152882,
-1.61715853509714,-1.56608715218077,-1.54503470288607,-1.53522934655712,
-1.53306018122405,-1.53182886676045,-1.53075686085098,-1.52937312788663,
-1.52712734324978,-1.51396277641544,-1.51293567800882,-1.47638090775202,
-1.45815515730985),.UNSPECIFIED.);
#1317=B_SPLINE_CURVE_WITH_KNOTS('',3,(#47343,#47344,#47345,#47346,#47347,
#47348,#47349,#47350,#47351,#47352,#47353,#47354,#47355,#47356,#47357,#47358,
#47359,#47360,#47361,#47362,#47363,#47364,#47365,#47366,#47367,#47368,#47369,
#47370,#47371,#47372,#47373,#47374,#47375,#47376,#47377,#47378,#47379,#47380,
#47381,#47382,#47383,#47384,#47385,#47386,#47387,#47388,#47389,#47390,#47391,
#47392,#47393,#47394,#47395,#47396,#47397,#47398,#47399,#47400,#47401,#47402,
#47403,#47404,#47405,#47406,#47407,#47408,#47409,#47410,#47411,#47412,#47413,
#47414,#47415,#47416,#47417,#47418,#47419,#47420,#47421,#47422,#47423,#47424,
#47425,#47426,#47427,#47428,#47429,#47430,#47431,#47432,#47433,#47434,#47435,
#47436,#47437,#47438,#47439,#47440,#47441,#47442,#47443,#47444,#47445,#47446,
#47447,#47448,#47449,#47450,#47451,#47452,#47453,#47454,#47455,#47456,#47457,
#47458,#47459,#47460,#47461,#47462,#47463,#47464,#47465,#47466,#47467,#47468,
#47469,#47470,#47471,#47472,#47473,#47474,#47475,#47476,#47477,#47478,#47479,
#47480,#47481,#47482,#47483,#47484,#47485,#47486,#47487,#47488,#47489,#47490,
#47491,#47492,#47493,#47494,#47495,#47496,#47497,#47498,#47499,#47500,#47501,
#47502,#47503,#47504,#47505,#47506,#47507,#47508,#47509,#47510,#47511,#47512,
#47513,#47514,#47515,#47516,#47517,#47518,#47519,#47520,#47521,#47522,#47523,
#47524,#47525,#47526,#47527,#47528,#47529,#47530,#47531,#47532,#47533,#47534,
#47535,#47536,#47537,#47538,#47539,#47540,#47541,#47542,#47543,#47544,#47545,
#47546,#47547,#47548,#47549,#47550,#47551,#47552,#47553,#47554,#47555,#47556,
#47557,#47558,#47559,#47560,#47561,#47562,#47563,#47564,#47565,#47566,#47567,
#47568),.UNSPECIFIED.,.F.,.F.,(4,2,2,2,2,2,2,2,2,2,2,2,2,2,2,2,2,2,2,2,
2,2,2,2,2,2,2,2,2,2,2,2,2,2,2,2,2,2,2,2,2,2,2,2,2,2,2,2,2,2,2,2,2,2,2,2,
2,2,2,2,2,2,2,2,2,2,2,2,2,2,2,2,2,2,2,2,2,2,2,2,2,2,2,2,2,2,2,2,2,2,2,2,
2,2,2,2,2,2,2,2,2,2,2,2,2,2,2,2,2,2,2,2,4),(-2.18949906292891,-2.1838650089922,
-2.18163622273672,-2.18039187561649,-2.17932165705407,-2.17795722915846,
-2.17515163526715,-2.15078142330274,-2.10153065279031,-2.08972730276351,
-2.08633112314776,-2.08422880749848,-2.08230367858015,-2.07984090766426,
-2.07579935338851,-2.04891117986127,-2.00021327939007,-1.99114088668074,
-1.98902302161969,-1.98780298306768,-1.98672898210937,-1.98535026184121,
-1.98307165100038,-1.96925110501733,-1.96033552537047,-1.91024334543028,
-1.89739515281065,-1.89389953573463,-1.89177517123471,-1.88985551632921,
-1.88739422344208,-1.8834468060302,-1.85979651054343,-1.81018684308953,
-1.79886699722579,-1.79660473021298,-1.79535302900298,-1.79428348427921,
-1.79292888830024,-1.79017321020061,-1.75727490009547,-1.73220967725323,
-1.70862182618849,-1.70287452413093,-1.70029132676813,-1.69835429837472,
-1.69653570234955,-1.69401452457364,-1.68747077470464,-1.64165405685319,
-1.6170585313395,-1.60631034109623,-1.60408118071565,-1.60283663173836,
-1.60176624395849,-1.60040160600074,-1.59759559923776,-1.57322502826008,
-1.52396442077986,-1.51215791530036,-1.5087610695415,-1.50665839230684,
-1.50473296609692,-1.50226986140283,-1.49822785870703,-1.47134306991988,
-1.42265799690053,-1.41355905152598,-1.41143901428331,-1.41021837699256,
-1.40914428396779,-1.40776600229934,-1.40548926104755,-1.39175626157772,
-1.38282361888464,-1.34832797823272,-1.33030636996907,-1.32310576586014,
-1.31766596056196,-1.31513921693266,-1.31321053141478,-1.31137441314844,
-1.30826436637587,-1.29979490709798,-1.29925333107365,-1.25003776607155,
-1.22305935265615,-1.21967214806597,-1.21819883416083,-1.2171148038492,
-1.21607845635969,-1.21427264755552,-1.20857237311552,-1.19919355257488,
-1.15742761264654,-1.1291123391115,-1.12503472450797,-1.12256091445563,
-1.12063370358738,-1.11853572832477,-1.11516116513808,-1.10358047589121,
-1.08380399239698,-1.0440534653287,-1.04245188977587,-1.0291650673599,-1.02691289616834,
-1.02552706368613,-1.02445459794764,-1.02322406119448,-1.02105937004265,
-1.01132613546075,-0.97396649970557),.UNSPECIFIED.);
#1318=B_SPLINE_CURVE_WITH_KNOTS('',3,(#47569,#47570,#47571,#47572,#47573,
#47574,#47575,#47576,#47577,#47578,#47579,#47580,#47581,#47582,#47583,#47584,
#47585,#47586,#47587,#47588,#47589,#47590,#47591,#47592,#47593,#47594,#47595,
#47596,#47597,#47598,#47599,#47600,#47601,#47602,#47603,#47604,#47605,#47606,
#47607,#47608,#47609,#47610,#47611,#47612,#47613,#47614,#47615,#47616,#47617,
#47618,#47619,#47620,#47621,#47622,#47623,#47624,#47625,#47626,#47627,#47628,
#47629,#47630,#47631,#47632,#47633,#47634,#47635,#47636,#47637,#47638,#47639,
#47640,#47641,#47642,#47643,#47644,#47645,#47646,#47647,#47648,#47649,#47650,
#47651,#47652,#47653,#47654,#47655,#47656,#47657,#47658,#47659,#47660,#47661,
#47662,#47663,#47664,#47665,#47666,#47667,#47668,#47669,#47670,#47671,#47672,
#47673,#47674,#47675,#47676,#47677,#47678,#47679,#47680,#47681,#47682,#47683,
#47684,#47685,#47686,#47687,#47688,#47689,#47690,#47691,#47692,#47693,#47694,
#47695,#47696,#47697,#47698,#47699,#47700,#47701,#47702,#47703,#47704,#47705,
#47706,#47707,#47708,#47709,#47710,#47711,#47712,#47713,#47714,#47715,#47716,
#47717,#47718,#47719,#47720,#47721,#47722,#47723,#47724,#47725,#47726,#47727,
#47728,#47729,#47730,#47731,#47732,#47733,#47734,#47735,#47736,#47737,#47738,
#47739,#47740,#47741,#47742,#47743,#47744,#47745,#47746,#47747,#47748,#47749,
#47750,#47751,#47752,#47753,#47754,#47755,#47756,#47757,#47758,#47759,#47760,
#47761,#47762,#47763,#47764,#47765,#47766,#47767,#47768,#47769,#47770,#47771,
#47772,#47773,#47774,#47775,#47776,#47777,#47778,#47779,#47780,#47781,#47782,
#47783,#47784,#47785,#47786,#47787,#47788,#47789,#47790),.UNSPECIFIED.,
 .F.,.F.,(4,2,2,2,2,2,2,2,2,2,2,2,2,2,2,2,2,2,2,2,2,2,2,2,2,2,2,2,2,2,2,
2,2,2,2,2,2,2,2,2,2,2,2,2,2,2,2,2,2,2,2,2,2,2,2,2,2,2,2,2,2,2,2,2,2,2,2,
2,2,2,2,2,2,2,2,2,2,2,2,2,2,2,2,2,2,2,2,2,2,2,2,2,2,2,2,2,2,2,2,2,2,2,2,
2,2,2,2,2,2,2,4),(-1.45815515730985,-1.44311106714501,-1.43866533437122,
-1.43633552712416,-1.43461173462009,-1.43246533009513,-1.42887016732215,
-1.41651973983777,-1.36941026717677,-1.35148688200421,-1.34261472047773,
-1.34051166933253,-1.33929488460142,-1.33822020196588,-1.33683604894193,
-1.33453902675744,-1.32029853381343,-1.31483766688885,-1.26395783223085,
-1.24919663170449,-1.24553987342171,-1.24337987025709,-1.2414667039106,
-1.23906584830869,-1.23531757631766,-1.21597119432106,-1.16386542523579,
-1.15073996967145,-1.14849586366893,-1.14711256823274,-1.14604051464259,
-1.14480869864457,-1.14263760631898,-1.13280530404366,-1.11166108054614,
-1.06076806319143,-1.05466226608335,-1.05221390748264,-1.05041414743598,
-1.0484651328367,-1.04580927574224,-1.03965074470046,-1.01274074458945,
-0.975751174046082,-0.972106143030279,-0.958288283245352,-0.956009703561393,
-0.954630986116154,-0.953556974136883,-0.952336896014332,-0.950218917922291,
-0.94114499006314,-0.892473640758535,-0.865595297937176,-0.861554049098209,
-0.859091280809838,-0.857166055288193,-0.855063535065136,-0.851666807129734,
-0.839859519543243,-0.790580579910545,-0.766198655561951,-0.763392508246637,
-0.762027904358827,-0.760957595598691,-0.759713190493695,-0.757484430253501,
-0.746740305406103,-0.722161659370576,-0.676369047836385,-0.669826827451264,
-0.667306007928953,-0.665487589227804,-0.663550674810742,-0.66096750956867,
-0.655219793739925,-0.63162419573825,-0.606543529041573,-0.573631955430268,
-0.570875896002742,-0.569521260885908,-0.568451760439797,-0.567200191055959,
-0.564938376631638,-0.553624558266521,-0.504065332566312,-0.480399575278229,
-0.476452113126949,-0.473990802682898,-0.472071153495024,-0.469946814942489,
-0.466451288270663,-0.453604246946545,-0.403483737066874,-0.381147891239907,
-0.378359998669721,-0.376999017612909,-0.37592901488986,-0.37468204864494,
-0.372441485254584,-0.361498098158943,-0.336112164974224,-0.291435410883938,
-0.284833521049669,-0.282303367205749,-0.280482509045716,-0.278546960999872,
-0.275972409223171,-0.270272090904166,-0.247042911606363,-0.242695174128374),
 .UNSPECIFIED.);
#1319=B_SPLINE_CURVE_WITH_KNOTS('',3,(#47796,#47797,#47798,#47799,#47800,
#47801,#47802,#47803,#47804,#47805,#47806,#47807,#47808,#47809,#47810,#47811,
#47812,#47813,#47814,#47815,#47816,#47817,#47818,#47819,#47820,#47821,#47822,
#47823,#47824,#47825,#47826,#47827,#47828,#47829,#47830,#47831,#47832,#47833,
#47834,#47835,#47836,#47837,#47838,#47839,#47840,#47841,#47842,#47843,#47844,
#47845,#47846,#47847,#47848,#47849,#47850,#47851,#47852,#47853,#47854,#47855,
#47856,#47857,#47858,#47859,#47860,#47861,#47862,#47863,#47864,#47865,#47866,
#47867,#47868,#47869,#47870,#47871,#47872,#47873,#47874,#47875,#47876,#47877,
#47878,#47879,#47880,#47881,#47882,#47883,#47884,#47885,#47886,#47887,#47888,
#47889,#47890,#47891,#47892,#47893,#47894,#47895,#47896,#47897,#47898,#47899,
#47900,#47901,#47902,#47903,#47904,#47905,#47906,#47907,#47908,#47909,#47910,
#47911,#47912,#47913,#47914,#47915,#47916,#47917,#47918,#47919,#47920,#47921,
#47922,#47923,#47924,#47925,#47926,#47927,#47928,#47929,#47930,#47931,#47932,
#47933,#47934,#47935,#47936,#47937,#47938,#47939,#47940,#47941,#47942,#47943,
#47944,#47945,#47946,#47947,#47948,#47949,#47950,#47951,#47952,#47953,#47954,
#47955,#47956,#47957,#47958,#47959,#47960,#47961,#47962,#47963,#47964,#47965,
#47966,#47967,#47968,#47969,#47970,#47971,#47972,#47973,#47974,#47975,#47976,
#47977),.UNSPECIFIED.,.F.,.F.,(4,2,2,2,2,2,2,2,2,2,2,2,2,2,2,2,2,2,2,2,
2,2,2,2,2,2,2,2,2,2,2,2,2,2,2,2,2,2,2,2,2,2,2,2,2,2,2,2,2,2,2,2,2,2,2,2,
2,2,2,2,2,2,2,2,2,2,2,2,2,2,2,2,2,2,2,2,2,2,2,2,2,2,2,2,2,2,2,2,2,2,4),
(-0.974174670753132,-0.9634387478963,-0.922534947998271,-0.908680419082317,
-0.906395898254317,-0.905015325265116,-0.903940954268919,-0.902721703837313,
-0.900607987060405,-0.89159499936821,-0.842865170768955,-0.815964168702849,
-0.811921841013154,-0.809458563378312,-0.80753302865571,-0.805430261039978,
-0.802033333848669,-0.790227404450901,-0.740946061260547,-0.716552111482368,
-0.713745467792079,-0.712380644009616,-0.711310173068138,-0.710065591037871,
-0.707836542352759,-0.697091576444547,-0.67251230267429,-0.626708770399057,
-0.620165826363481,-0.617644669076387,-0.615825987798593,-0.613888776131545,
-0.611305184223749,-0.605556392203509,-0.581955589606329,-0.556872547144106,
-0.523956906786774,-0.521200410334773,-0.519845567067463,-0.518775905501424,
-0.517524151110571,-0.515262011105729,-0.503946744883425,-0.454382696229716,
-0.430710883651648,-0.426762757290848,-0.424301055522499,-0.422381115143407,
-0.420256468606168,-0.416760467897113,-0.403912057978495,-0.353783679746306,
-0.344859167237714,-0.331031955283378,-0.328752719201692,-0.327373706518535,
-0.326299528299217,-0.32507933374179,-0.322961319235643,-0.313889751013021,
-0.265208494141045,-0.238325315169799,-0.23428346188979,-0.231820332296355,
-0.229894828515189,-0.228106666535456,-0.225163619444972,-0.216726004108841,
-0.203920218771785,-0.172858848314652,-0.158376967495467,-0.152739973468462,
-0.149077644592055,-0.138231396142488,-0.13611016384228,-0.134764044901729,
-0.133695047108698,-0.132436819832506,-0.130144541429449,-0.118274896887299,
-0.0813224857394244,-0.0677146962907497,-0.0597956969094492,-0.0447636751811699,
-0.0409592442672668,-0.0387442253970217,-0.0368363035725809,-0.0350092001075732,
-0.0327352983580613,-0.0292939652422515,-0.00056352101036781),
 .UNSPECIFIED.);
#1320=B_SPLINE_CURVE_WITH_KNOTS('',3,(#47978,#47979,#47980,#47981,#47982,
#47983,#47984,#47985,#47986,#47987,#47988,#47989,#47990,#47991,#47992,#47993,
#47994,#47995,#47996,#47997,#47998,#47999,#48000,#48001,#48002,#48003,#48004,
#48005,#48006,#48007,#48008,#48009,#48010,#48011,#48012,#48013,#48014,#48015,
#48016,#48017,#48018,#48019,#48020,#48021,#48022,#48023),.UNSPECIFIED.,
 .F.,.F.,(4,2,2,2,2,2,2,2,2,2,2,2,2,2,2,2,2,2,2,2,2,2,4),(-2.43136994263749,
-2.38857942322587,-2.37646857526415,-2.37416389819509,-2.37290310662602,
-2.37183447809935,-2.37049206108053,-2.36838263494433,-2.35772255734863,
-2.31573744321584,-2.294466988112,-2.28642387945132,-2.28054678715594,-2.27800435161223,
-2.27604735945959,-2.27425783159587,-2.27139336340267,-2.26446612094389,
-2.2627043812287,-2.26099926603054,-2.21920140266554,-2.19461115105961,
-2.18949906292891),.UNSPECIFIED.);
#1321=B_SPLINE_CURVE_WITH_KNOTS('',3,(#48025,#48026,#48027,#48028,#48029,
#48030,#48031,#48032,#48033,#48034,#48035,#48036,#48037,#48038,#48039,#48040,
#48041,#48042,#48043,#48044,#48045,#48046,#48047,#48048,#48049,#48050,#48051,
#48052,#48053,#48054,#48055,#48056,#48057,#48058,#48059,#48060,#48061,#48062,
#48063,#48064,#48065,#48066,#48067,#48068,#48069,#48070,#48071,#48072,#48073,
#48074,#48075,#48076,#48077,#48078,#48079,#48080,#48081,#48082,#48083,#48084),
 .UNSPECIFIED.,.F.,.F.,(4,2,2,2,2,2,2,2,2,2,2,2,2,2,2,2,2,2,2,2,2,2,2,2,
2,2,2,2,2,4),(-0.242695174128374,-0.221667875824946,-0.188612152567491,
-0.185857636448818,-0.184503315098143,-0.183464484460551,-0.183459264182677,
-0.183454111818551,-0.183449026147903,-0.183444005663323,-0.183439049352269,
-0.18343415586448,-0.183429324011531,-0.183424552649247,-0.183419840616554,
-0.183415186829067,-0.182181080759297,-0.180852488616711,-0.178781995938101,
-0.174829325467977,-0.128017800485001,-0.0957595023227357,-0.0916081614258372,
-0.0891131162241835,-0.0871832241910747,-0.0850961611120692,-0.0817692317479223,
-0.0706430063604701,-0.0519763481601277,-0.000564321818699808),
 .UNSPECIFIED.);
#1322=B_SPLINE_CURVE_WITH_KNOTS('',3,(#48085,#48086,#48087,#48088,#48089,
#48090,#48091,#48092,#48093,#48094,#48095,#48096,#48097,#48098,#48099,#48100,
#48101,#48102,#48103,#48104,#48105,#48106,#48107,#48108,#48109,#48110,#48111,
#48112,#48113,#48114,#48115,#48116,#48117,#48118,#48119,#48120,#48121,#48122,
#48123,#48124,#48125,#48126,#48127,#48128,#48129,#48130,#48131,#48132,#48133,
#48134,#48135,#48136,#48137,#48138,#48139,#48140,#48141,#48142,#48143,#48144,
#48145,#48146,#48147,#48148,#48149,#48150,#48151,#48152,#48153,#48154,#48155,
#48156,#48157,#48158,#48159,#48160,#48161,#48162,#48163,#48164,#48165,#48166,
#48167,#48168,#48169,#48170,#48171,#48172,#48173,#48174,#48175,#48176,#48177,
#48178,#48179,#48180,#48181,#48182,#48183,#48184,#48185,#48186,#48187,#48188,
#48189,#48190,#48191,#48192,#48193,#48194,#48195,#48196,#48197,#48198,#48199,
#48200,#48201,#48202,#48203,#48204,#48205,#48206,#48207,#48208,#48209,#48210,
#48211,#48212,#48213,#48214,#48215,#48216,#48217,#48218,#48219,#48220,#48221,
#48222,#48223,#48224,#48225,#48226,#48227,#48228,#48229,#48230,#48231,#48232,
#48233,#48234,#48235,#48236,#48237,#48238,#48239,#48240,#48241),
 .UNSPECIFIED.,.F.,.F.,(4,3,3,3,3,3,3,3,3,3,3,3,3,3,3,3,3,3,3,3,3,3,3,3,
3,3,3,3,3,3,3,3,3,3,3,3,3,3,3,3,3,3,3,3,3,3,3,3,3,3,3,3,4),(153.9380400259,
153.986061433838,154.091935315901,154.203101020456,154.308687775867,154.414210794711,
154.519706482428,154.625211202399,154.730829644781,154.836514123591,154.942377335347,
154.981260952343,155.087134834418,155.198300538972,155.303887294394,155.409410313251,
155.51490600098,155.620410720963,155.726029163356,155.831713642178,155.937576853946,
155.976460470847,156.082334352903,156.19350005746,156.299086812864,156.404609831702,
156.510105519413,156.615610239378,156.721228681754,156.826913160558,156.932776372309,
156.971659989352,157.077533871402,157.188699575959,157.294286331357,157.399809350189,
157.505305037892,157.610809757851,157.716428200219,157.822112679016,157.92797589076,
157.966859507857,158.07273338999,158.183899094536,158.289485850017,158.395008868932,
158.500504556718,158.606009276758,158.711627719208,158.817312198086,158.923175409909,
158.962059026361,158.969960932636),.UNSPECIFIED.);
#1323=B_SPLINE_CURVE_WITH_KNOTS('',3,(#48246,#48247,#48248,#48249,#48250,
#48251,#48252,#48253,#48254,#48255,#48256,#48257,#48258,#48259,#48260,#48261,
#48262,#48263,#48264,#48265,#48266,#48267,#48268,#48269,#48270,#48271,#48272,
#48273,#48274,#48275,#48276,#48277,#48278,#48279,#48280,#48281,#48282,#48283,
#48284,#48285,#48286,#48287,#48288,#48289,#48290,#48291,#48292,#48293,#48294,
#48295,#48296,#48297,#48298,#48299,#48300,#48301,#48302,#48303,#48304,#48305,
#48306,#48307,#48308,#48309,#48310,#48311,#48312,#48313,#48314,#48315,#48316,
#48317,#48318,#48319,#48320,#48321,#48322,#48323,#48324,#48325,#48326,#48327,
#48328,#48329,#48330,#48331,#48332,#48333,#48334,#48335,#48336,#48337,#48338,
#48339,#48340,#48341,#48342,#48343,#48344,#48345,#48346,#48347,#48348,#48349,
#48350,#48351,#48352,#48353,#48354,#48355,#48356,#48357,#48358,#48359,#48360,
#48361,#48362,#48363,#48364,#48365,#48366,#48367,#48368,#48369,#48370,#48371,
#48372,#48373,#48374,#48375,#48376,#48377,#48378,#48379,#48380,#48381,#48382,
#48383,#48384,#48385,#48386,#48387,#48388,#48389,#48390,#48391,#48392,#48393,
#48394,#48395,#48396,#48397,#48398,#48399,#48400,#48401,#48402,#48403,#48404,
#48405,#48406,#48407,#48408,#48409,#48410,#48411,#48412,#48413,#48414,#48415,
#48416,#48417,#48418,#48419,#48420,#48421,#48422,#48423,#48424,#48425,#48426,
#48427,#48428,#48429,#48430,#48431,#48432,#48433,#48434,#48435,#48436,#48437,
#48438,#48439,#48440,#48441,#48442,#48443,#48444,#48445,#48446,#48447,#48448,
#48449,#48450,#48451,#48452,#48453,#48454,#48455,#48456,#48457,#48458,#48459,
#48460,#48461,#48462,#48463,#48464,#48465,#48466,#48467,#48468,#48469,#48470,
#48471,#48472,#48473,#48474,#48475),.UNSPECIFIED.,.F.,.F.,(4,2,2,2,2,2,
2,2,2,2,2,2,2,2,2,2,2,2,2,2,2,2,2,2,2,2,2,2,2,2,2,2,2,2,2,2,2,2,2,2,2,2,
2,2,2,2,2,2,2,2,2,2,2,2,2,2,2,2,2,2,2,2,2,2,2,2,2,2,2,2,2,2,2,2,2,2,2,2,
2,2,2,2,2,2,2,2,2,2,2,2,2,2,2,2,2,2,2,2,2,2,2,2,2,2,2,2,2,2,2,2,2,2,2,2,
4),(-2.18940064281308,-2.17324077329001,-2.16143901298114,-2.15804337874734,
-2.15594141928606,-2.15401662894101,-2.15155430825681,-2.14751352942863,
-2.12063290814333,-2.07195154041407,-2.06287088315446,-2.0607526661771,
-2.05953268093726,-2.05845889606584,-2.05708067089078,-2.05480332804314,
-2.04106172224337,-2.02899930501495,-1.99673047286814,-1.97294744453886,
-1.96717565764364,-1.96458837116913,-1.9626510260713,-1.96083413186644,
-1.95831849451821,-1.95180754209415,-1.90549285637228,-1.88126409108669,
-1.87060922949552,-1.86838603843297,-1.86714295435572,-1.86607265609163,
-1.8647066178964,-1.86189262734673,-1.83643587887034,-1.8042409334404,-1.78048012410981,
-1.77471102086373,-1.77212412516464,-1.77018674989406,-1.7683695927781,
-1.76585321828434,-1.75933821327124,-1.71307730131563,-1.68880685303427,
-1.67814116167038,-1.67591722009928,-1.67467392709753,-1.67360358004846,
-1.6722376499123,-1.66942445955091,-1.64411367538752,-1.61180827260133,
-1.58801179027351,-1.58223794572398,-1.57965009899405,-1.57771247826308,
-1.57589543013712,-1.57337974598009,-1.56686962725001,-1.52052379582618,
-1.49630993073737,-1.48565828834039,-1.48343509997932,-1.4821919240161,
-1.4811214868796,-1.47975519484316,-1.47756743927912,-1.46554922553989,
-1.46041753794372,-1.42183749947843,-1.39590787138247,-1.38986717267425,
-1.38723180943733,-1.3852862970197,-1.38348159235791,-1.38101384680097,
-1.37479343072953,-1.32495224273226,-1.30630021147244,-1.29336314441733,
-1.29101746019944,-1.28974773989311,-1.28867952837314,-1.28734766856046,
-1.28527302782054,-1.2751548719539,-1.23243264931515,-1.21630057327133,
-1.20006270971042,-1.19616594145952,-1.19392979701521,-1.19221358907431,
-1.18999115510297,-1.18605015542787,-1.16702391464143,-1.11964043772659,
-1.11560984042451,-1.10120413887445,-1.09889995817399,-1.09751363668171,
-1.09643859637109,-1.09522289538876,-1.09312510277461,-1.08432429177742,
-1.066629920425,-1.03722858135862,-1.0085775388757,-1.00449249691808,-1.0020166049989,
-1.00008921775498,-0.99799250647038,-0.994623178058371,-0.983092297038724,
-0.974174670753132),.UNSPECIFIED.);
#1324=B_SPLINE_CURVE_WITH_KNOTS('',3,(#48477,#48478,#48479,#48480,#48481,
#48482,#48483,#48484,#48485,#48486,#48487,#48488,#48489,#48490,#48491,#48492,
#48493,#48494,#48495,#48496,#48497,#48498,#48499,#48500,#48501,#48502,#48503,
#48504,#48505,#48506,#48507,#48508,#48509,#48510,#48511,#48512,#48513),
 .UNSPECIFIED.,.F.,.F.,(4,3,3,3,3,3,3,3,3,3,3,3,4),(158.969960932636,159.075821542289,
159.186001167611,159.291582644725,159.397102766328,159.502597933955,159.608104509553,
159.713726266565,159.819416195121,159.925282860653,159.957258544866,160.090976876507,
160.22122533308),.UNSPECIFIED.);
#1325=B_SPLINE_CURVE_WITH_KNOTS('',3,(#48514,#48515,#48516,#48517,#48518,
#48519,#48520,#48521,#48522,#48523,#48524,#48525,#48526,#48527,#48528,#48529,
#48530,#48531,#48532,#48533,#48534,#48535,#48536,#48537,#48538,#48539,#48540,
#48541,#48542,#48543,#48544,#48545,#48546,#48547,#48548,#48549,#48550,#48551,
#48552,#48553,#48554,#48555,#48556,#48557,#48558,#48559,#48560,#48561,#48562,
#48563,#48564,#48565,#48566,#48567,#48568,#48569,#48570,#48571,#48572,#48573,
#48574,#48575,#48576,#48577,#48578,#48579,#48580,#48581,#48582,#48583,#48584,
#48585,#48586,#48587,#48588,#48589,#48590,#48591,#48592,#48593,#48594,#48595,
#48596,#48597,#48598,#48599,#48600,#48601,#48602,#48603,#48604,#48605,#48606,
#48607,#48608,#48609,#48610,#48611,#48612,#48613,#48614,#48615,#48616,#48617,
#48618,#48619,#48620,#48621,#48622,#48623,#48624,#48625,#48626,#48627,#48628,
#48629,#48630,#48631,#48632,#48633,#48634,#48635,#48636,#48637,#48638,#48639,
#48640,#48641,#48642,#48643,#48644,#48645,#48646,#48647,#48648,#48649,#48650,
#48651,#48652,#48653,#48654,#48655,#48656,#48657,#48658,#48659,#48660,#48661,
#48662,#48663,#48664,#48665,#48666,#48667,#48668,#48669,#48670,#48671,#48672,
#48673,#48674,#48675,#48676,#48677,#48678,#48679,#48680,#48681,#48682,#48683,
#48684,#48685,#48686,#48687,#48688,#48689,#48690,#48691,#48692,#48693),
 .UNSPECIFIED.,.F.,.F.,(4,2,2,2,2,2,2,2,2,2,2,2,2,2,2,2,2,2,2,2,2,2,2,2,
2,2,2,2,2,2,2,2,2,2,2,2,2,2,2,2,2,2,2,2,2,2,2,2,2,2,2,2,2,2,2,2,2,2,2,2,
2,2,2,2,2,2,2,2,2,2,2,2,2,2,2,2,2,2,2,2,2,2,2,2,2,2,2,2,2,4),(-2.43128894848558,
-2.40402165749699,-2.39373143610476,-2.39061926341053,-2.38848190111966,
-2.38639485731439,-2.38446536562597,-2.381971374362,-2.37782292549865,-2.34580085899753,
-2.32528912137062,-2.30423921586788,-2.29362190367919,-2.29139181401887,
-2.29014733693218,-2.28907738036556,-2.28771376932007,-2.28491147647599,
-2.2608355911699,-2.21142526738758,-2.20355201278584,-2.19776263617866,
-2.19517879997975,-2.19323359120059,-2.19142993049838,-2.18896479492237,
-2.18275705001053,-2.1324153038027,-2.11095636463804,-2.10118862433269,
-2.09892725589144,-2.09767596541003,-2.09660671859089,-2.09525243215069,
-2.09249716145065,-2.05961979425454,-2.03453719648145,-2.01096712398314,
-2.00522287890918,-2.00264067241323,-2.00070423422888,-1.9988860810328,
-1.99636533978075,-1.98982168574514,-1.94401719922651,-1.91943099357456,
-1.90868643179094,-1.90645793826304,-1.90521374980516,-1.90414366480947,
-1.90277940364899,-1.89997414073687,-1.87560501050664,-1.82636135044212,
-1.81456011900504,-1.81116442769963,-1.80906238900794,-1.80713749688047,
-1.80467500577902,-1.80063386151756,-1.77374535134339,-1.72504381292472,
-1.71598427736919,-1.71386753606527,-1.71264783961755,-1.71157393599248,
-1.71019507990167,-1.7079157081721,-1.69408155483174,-1.65317816574383,
-1.6335503869198,-1.62202963000177,-1.6186619369908,-1.61656594808735,-1.61463902552569,
-1.61216345251823,-1.60807830527806,-1.57939167990488,-1.54989364667247,
-1.53228040212644,-1.5235069661649,-1.52141160076482,-1.52019663410166,
-1.51912178188801,-1.51773512312131,-1.51542918186865,-1.50096896070186,
-1.49602903682948,-1.46162491485128,-1.45803638872278),.UNSPECIFIED.);
#1326=B_SPLINE_CURVE_WITH_KNOTS('',3,(#48699,#48700,#48701,#48702,#48703,
#48704,#48705,#48706,#48707,#48708,#48709,#48710,#48711,#48712,#48713,#48714,
#48715,#48716,#48717,#48718,#48719,#48720,#48721,#48722,#48723,#48724,#48725,
#48726,#48727,#48728,#48729,#48730,#48731,#48732,#48733,#48734,#48735,#48736,
#48737,#48738,#48739,#48740,#48741,#48742,#48743,#48744,#48745,#48746,#48747,
#48748,#48749,#48750,#48751,#48752,#48753,#48754,#48755,#48756,#48757,#48758,
#48759,#48760,#48761,#48762,#48763,#48764,#48765,#48766,#48767,#48768,#48769,
#48770,#48771,#48772,#48773,#48774,#48775,#48776,#48777,#48778,#48779,#48780,
#48781,#48782,#48783,#48784,#48785,#48786,#48787,#48788,#48789,#48790,#48791,
#48792,#48793,#48794,#48795,#48796,#48797,#48798,#48799,#48800,#48801,#48802,
#48803,#48804,#48805,#48806,#48807,#48808,#48809,#48810,#48811,#48812,#48813,
#48814,#48815,#48816,#48817,#48818,#48819,#48820,#48821,#48822,#48823,#48824,
#48825,#48826,#48827,#48828,#48829,#48830,#48831,#48832,#48833,#48834,#48835,
#48836,#48837,#48838,#48839,#48840,#48841,#48842,#48843,#48844,#48845,#48846,
#48847,#48848,#48849,#48850,#48851,#48852,#48853,#48854,#48855,#48856,#48857,
#48858,#48859,#48860,#48861,#48862,#48863,#48864,#48865,#48866,#48867,#48868,
#48869,#48870,#48871,#48872,#48873,#48874,#48875,#48876,#48877,#48878,#48879,
#48880,#48881,#48882,#48883,#48884,#48885,#48886,#48887,#48888,#48889,#48890,
#48891,#48892,#48893,#48894,#48895,#48896,#48897,#48898,#48899,#48900,#48901,
#48902,#48903,#48904),.UNSPECIFIED.,.F.,.F.,(4,2,2,2,2,2,2,2,2,2,2,2,2,
2,2,2,2,2,2,2,2,2,2,2,2,2,2,2,2,2,2,2,2,2,2,2,2,2,2,2,2,2,2,2,2,2,2,2,2,
2,2,2,2,2,2,2,2,2,2,2,2,2,2,2,2,2,2,2,2,2,2,2,2,2,2,2,2,2,2,2,2,2,2,2,2,
2,2,2,2,2,2,2,2,2,2,2,2,2,2,2,2,2,4),(-0.973787058187152,-0.971801940687298,
-0.960595339333787,-0.912180463585337,-0.887328913404492,-0.883346693228246,
-0.880875193661627,-0.878954635845838,-0.876836432945466,-0.873367354718714,
-0.86080253907915,-0.810461687935693,-0.807784069226913,-0.801407631248591,
-0.787603698148841,-0.785326082540803,-0.783947804096976,-0.782873995668262,
-0.781653932042932,-0.77953575922172,-0.770457641318477,-0.721794527897309,
-0.694920470067691,-0.690879506929976,-0.688416876728683,-0.686491736509972,
-0.684389285437468,-0.680992612966264,-0.669184854826154,-0.619903294147924,
-0.59553936461531,-0.592733518051818,-0.591368985761278,-0.590298723959279,
-0.589054378667964,-0.586825602932509,-0.576078994605386,-0.551488665258547,
-0.505721719980875,-0.499179053126231,-0.496658315310316,-0.4948400368633,
-0.492903347186302,-0.49032061117294,-0.484574393320205,-0.460988384462475,
-0.435903714829837,-0.402990880561689,-0.400235401362543,-0.398880976192795,
-0.397811604865909,-0.396560145736941,-0.394298429990437,-0.382983009438961,
-0.333398190501279,-0.309766546414575,-0.305820446084308,-0.303359692352746,
-0.301440297380349,-0.299316056740722,-0.29582026906562,-0.282967424203672,
-0.23285865727467,-0.210527785598441,-0.207739529436496,-0.206378568735993,
-0.20538523922618,-0.205380733840351,-0.205376324848768,-0.205372010222191,
-0.205367788043043,-0.205363656126608,-0.205359612456606,-0.205355996019009,
-0.205352397622671,-0.20534881725101,-0.205345254614244,-0.205341709628195,
-0.205338182293948,-0.204132906833308,-0.202029515594048,-0.199429825637415,
-0.193988040782058,-0.178178988109144,-0.136499636818045,-0.116920683751525,
-0.113161382794714,-0.110757150155002,-0.1088436693764,-0.106685836783518,
-0.10303889847966,-0.0884033904650566,-0.0384822875238028,-0.0286042439439895,
-0.020731486639263,-0.0161192246366164,-0.0143991075754617,-0.0133797956866168,
-0.0123611384337308,-0.0112848240284811,-0.00984155426457022,-0.00629937579403202,
-0.000566239655952785),.UNSPECIFIED.);
#1327=B_SPLINE_CURVE_WITH_KNOTS('',3,(#48905,#48906,#48907,#48908,#48909,
#48910,#48911,#48912,#48913,#48914,#48915,#48916,#48917,#48918,#48919,#48920,
#48921,#48922,#48923,#48924,#48925,#48926,#48927,#48928,#48929,#48930,#48931,
#48932,#48933,#48934,#48935,#48936,#48937,#48938,#48939,#48940,#48941,#48942,
#48943,#48944,#48945,#48946,#48947,#48948,#48949,#48950,#48951,#48952,#48953,
#48954,#48955,#48956,#48957,#48958,#48959,#48960,#48961,#48962,#48963,#48964,
#48965,#48966,#48967,#48968,#48969,#48970,#48971,#48972,#48973,#48974),
 .UNSPECIFIED.,.F.,.F.,(4,2,2,2,2,2,2,2,2,2,2,2,2,2,2,2,2,2,2,2,2,2,2,2,
2,2,2,2,2,2,2,2,2,2,4),(-2.43149354648851,-2.38992219825084,-2.35583090092751,
-2.35137061176593,-2.3490381223182,-2.34713050883852,-2.34492257878601,
-2.34114681995311,-2.32646952177799,-2.31789549330984,-2.27056566194237,
-2.26071202374391,-2.25675850045035,-2.25468785090749,-2.25335928637703,
-2.25212528419966,-2.25212070094854,-2.25211605802304,-2.25211135431886,
-2.25210658860967,-2.25210175976448,-2.25209686677358,-2.25209190816784,
-2.2520868826371,-2.25208178896488,-2.25207662590736,-2.25207139196767,
-2.2520660857715,-2.25206070583709,-2.25205525071632,-2.25101812014064,
-2.24965406848819,-2.24684966234465,-2.22248366788433,-2.18940064281308),
 .UNSPECIFIED.);
#1328=B_SPLINE_CURVE_WITH_KNOTS('',3,(#48975,#48976,#48977,#48978,#48979,
#48980,#48981,#48982,#48983,#48984,#48985,#48986,#48987,#48988,#48989,#48990,
#48991,#48992,#48993,#48994,#48995,#48996,#48997,#48998,#48999,#49000,#49001,
#49002,#49003,#49004,#49005,#49006,#49007,#49008,#49009,#49010,#49011,#49012,
#49013,#49014,#49015,#49016,#49017,#49018,#49019,#49020,#49021,#49022,#49023,
#49024,#49025,#49026,#49027,#49028,#49029,#49030,#49031,#49032,#49033,#49034,
#49035,#49036,#49037,#49038,#49039,#49040,#49041,#49042,#49043,#49044,#49045,
#49046,#49047,#49048,#49049,#49050,#49051,#49052,#49053,#49054,#49055,#49056,
#49057,#49058,#49059,#49060,#49061,#49062,#49063,#49064,#49065,#49066,#49067,
#49068,#49069,#49070,#49071,#49072,#49073,#49074,#49075,#49076,#49077,#49078,
#49079,#49080,#49081,#49082,#49083,#49084,#49085,#49086,#49087,#49088,#49089,
#49090,#49091,#49092,#49093,#49094,#49095,#49096,#49097,#49098,#49099,#49100,
#49101,#49102,#49103,#49104,#49105,#49106,#49107,#49108,#49109,#49110,#49111,
#49112,#49113,#49114,#49115,#49116,#49117,#49118,#49119,#49120,#49121,#49122,
#49123,#49124,#49125,#49126,#49127,#49128,#49129,#49130,#49131,#49132,#49133,
#49134,#49135,#49136,#49137,#49138,#49139,#49140,#49141,#49142,#49143,#49144,
#49145,#49146,#49147,#49148,#49149,#49150,#49151,#49152,#49153,#49154,#49155,
#49156,#49157,#49158,#49159,#49160,#49161,#49162,#49163,#49164,#49165,#49166,
#49167,#49168,#49169,#49170,#49171,#49172,#49173,#49174,#49175,#49176,#49177,
#49178,#49179,#49180,#49181,#49182,#49183,#49184,#49185,#49186,#49187,#49188,
#49189,#49190,#49191,#49192,#49193,#49194,#49195,#49196,#49197,#49198,#49199,
#49200),.UNSPECIFIED.,.F.,.F.,(4,2,2,2,2,2,2,2,2,2,2,2,2,2,2,2,2,2,2,2,
2,2,2,2,2,2,2,2,2,2,2,2,2,2,2,2,2,2,2,2,2,2,2,2,2,2,2,2,2,2,2,2,2,2,2,2,
2,2,2,2,2,2,2,2,2,2,2,2,2,2,2,2,2,2,2,2,2,2,2,2,2,2,2,2,2,2,2,2,2,2,2,2,
2,2,2,2,2,2,2,2,2,2,2,2,2,2,2,2,2,2,2,2,4),(-1.45803638872278,-1.44140955810846,
-1.4296534867198,-1.42626204032791,-1.42416078601136,-1.42223538283188,
-1.41977054438492,-1.41572192907757,-1.38905345093723,-1.34083188303034,
-1.33115650017217,-1.32899609162502,-1.32776669246211,-1.32669436926324,
-1.32530761571122,-1.32305177729499,-1.30967949560475,-1.27115914898039,
-1.24205315011539,-1.23563848956805,-1.23293901479649,-1.23098229959912,
-1.22919223408246,-1.22632517787012,-1.21938271153818,-1.21764312031094,
-1.21594715762074,-1.20052166719741,-1.15783440869433,-1.15376778767004,
-1.13935889970063,-1.13705478431023,-1.13566856520255,-1.13459364289385,
-1.13337811845707,-1.13128073068624,-1.12248307646172,-1.10479748624807,
-1.07538906341804,-1.04674257577078,-1.04265803567621,-1.04018243940552,
-1.03825527724496,-1.03615880572939,-1.0327898514745,-1.02126014157823,
-1.00160846489221,-0.960711118130644,-0.946850192664359,-0.944569636386252,
-0.943190312833635,-0.942116198371843,-0.940896425614768,-0.938779939005228,
-0.929726983933022,-0.881036635156126,-0.854150880649193,-0.850109336714403,
-0.847646441396319,-0.845721148342182,-0.843618586646655,-0.840221863469916,
-0.828415329485479,-0.779136643502452,-0.754750652140122,-0.75194438598397,
-0.750579733526155,-0.74950939152889,-0.748264953939066,-0.746036149132539,
-0.735292080389934,-0.71071426842235,-0.664917481742959,-0.658375171359847,
-0.655854289806948,-0.65403581763451,-0.652098838204596,-0.649515572455393,
-0.64376757539928,-0.620170461854027,-0.595089597553438,-0.56217733182469,
-0.559421166843357,-0.558066482533499,-0.556996940095799,-0.5557453144805,
-0.553483399505891,-0.542169078215479,-0.492606658186242,-0.46894245453169,
-0.46499491262841,-0.462533525070197,-0.460613798585893,-0.458489356844486,
-0.454993619330617,-0.442145320835569,-0.392023602689026,-0.369687981125468,
-0.366899631130225,-0.365538528973036,-0.364468487942502,-0.363221548241199,
-0.360981174973554,-0.350041577124906,-0.324671736470178,-0.279970060321373,
-0.273369105584581,-0.270839068375085,-0.269018219490698,-0.267082612598111,
-0.264507865315939,-0.258806630483864,-0.242686067170977),.UNSPECIFIED.);
#1329=B_SPLINE_CURVE_WITH_KNOTS('',3,(#49205,#49206,#49207,#49208,#49209,
#49210,#49211,#49212,#49213,#49214,#49215,#49216,#49217,#49218,#49219,#49220,
#49221,#49222,#49223,#49224,#49225,#49226,#49227,#49228,#49229,#49230,#49231,
#49232,#49233,#49234,#49235,#49236,#49237,#49238,#49239,#49240,#49241,#49242,
#49243,#49244,#49245,#49246,#49247,#49248,#49249,#49250,#49251,#49252,#49253,
#49254,#49255,#49256,#49257,#49258,#49259,#49260,#49261,#49262,#49263,#49264,
#49265,#49266,#49267,#49268,#49269,#49270,#49271,#49272,#49273,#49274,#49275,
#49276,#49277,#49278,#49279,#49280,#49281,#49282,#49283,#49284,#49285,#49286,
#49287,#49288,#49289,#49290,#49291,#49292,#49293,#49294,#49295,#49296,#49297,
#49298,#49299,#49300,#49301,#49302,#49303,#49304,#49305,#49306,#49307,#49308,
#49309,#49310,#49311,#49312,#49313,#49314,#49315,#49316,#49317,#49318,#49319,
#49320,#49321,#49322,#49323,#49324,#49325,#49326,#49327,#49328,#49329,#49330,
#49331,#49332,#49333,#49334,#49335,#49336,#49337,#49338,#49339,#49340,#49341,
#49342,#49343,#49344,#49345,#49346,#49347,#49348,#49349,#49350,#49351,#49352,
#49353,#49354,#49355,#49356,#49357,#49358,#49359,#49360,#49361,#49362,#49363,
#49364,#49365,#49366,#49367,#49368,#49369,#49370,#49371,#49372,#49373,#49374,
#49375,#49376,#49377,#49378,#49379,#49380,#49381,#49382,#49383,#49384,#49385,
#49386,#49387,#49388,#49389,#49390,#49391,#49392,#49393,#49394,#49395,#49396,
#49397,#49398,#49399,#49400,#49401,#49402,#49403,#49404,#49405,#49406,#49407,
#49408,#49409,#49410,#49411,#49412,#49413,#49414,#49415,#49416,#49417,#49418,
#49419,#49420,#49421,#49422,#49423,#49424,#49425,#49426,#49427,#49428,#49429,
#49430),.UNSPECIFIED.,.F.,.F.,(4,2,2,2,2,2,2,2,2,2,2,2,2,2,2,2,2,2,2,2,
2,2,2,2,2,2,2,2,2,2,2,2,2,2,2,2,2,2,2,2,2,2,2,2,2,2,2,2,2,2,2,2,2,2,2,2,
2,2,2,2,2,2,2,2,2,2,2,2,2,2,2,2,2,2,2,2,2,2,2,2,2,2,2,2,2,2,2,2,2,2,2,2,
2,2,2,2,2,2,2,2,2,2,2,2,2,2,2,2,2,2,2,2,4),(-2.18872254859161,-2.17002179167717,
-2.14518703702611,-2.13436880140523,-2.13213379750711,-2.13088725221948,
-2.1298202530721,-2.12846565382737,-2.12568523544807,-2.10286441602397,
-2.05273787376312,-2.04036827364099,-2.03693304534607,-2.0348319028284,
-2.03292456959959,-2.0304670764821,-2.02650167534777,-2.00157162747401,
-1.95288089662249,-1.94164785102387,-1.93940343155684,-1.93816201436535,
-1.93709567204078,-1.93574240420877,-1.93299254007081,-1.89988676028501,
-1.8744524822172,-1.85130855558775,-1.84561366357324,-1.84303709746159,
-1.84109817253612,-1.83927272957644,-1.83673388794344,-1.83009470939507,
-1.78675857011873,-1.76061031150067,-1.74948407283173,-1.74722745902251,
-1.74597424423193,-1.74490219310406,-1.74354187372541,-1.74137583650298,
-1.72977515162387,-1.72614881771714,-1.68511277778045,-1.65967148131973,
-1.65369141651281,-1.65106669689131,-1.64912295297693,-1.64731554730339,
-1.64483734031946,-1.63855528126412,-1.58929534984329,-1.56703951088787,
-1.55690152001526,-1.55471121639564,-1.55347563711939,-1.55240534684621,
-1.55103072082867,-1.54881253115325,-1.53617323809864,-1.53392130142186,
-1.52985906274059,-1.49432363324139,-1.47447130805812,-1.46286312171031,
-1.45948896163682,-1.45739307116101,-1.45546901860655,-1.45300100078151,
-1.44893669643834,-1.42102214697608,-1.3730010914805,-1.36426263461768,
-1.36217147279774,-1.36095827606882,-1.35988371443071,-1.3584964621511,
-1.35618846503178,-1.3416774818303,-1.33754025779713,-1.30077359602667,
-1.28164390005165,-1.27032487363905,-1.26697735413578,-1.26488545258997,
-1.26295655598157,-1.26047044261958,-1.25635052086089,-1.21563973324288,
-1.17521405567067,-1.1709811870584,-1.1693200889352,-1.16831190363125,-1.16720889430082,
-1.16562808483523,-1.16159118187243,-1.14076347097502,-1.09905033095437,
-1.07943385000551,-1.07567306488648,-1.07326852833733,-1.07135521780413,
-1.06919801497672,-1.06555320581034,-1.05094112500672,-1.0011947216004,
-0.980497079700009,-0.977732889705016,-0.976376773378501,-0.975307352126593,
-0.974057341062226,-0.973787058187152),.UNSPECIFIED.);
#1330=B_SPLINE_CURVE_WITH_KNOTS('',3,(#49432,#49433,#49434,#49435,#49436,
#49437,#49438,#49439,#49440,#49441,#49442,#49443,#49444,#49445,#49446,#49447,
#49448,#49449,#49450,#49451,#49452,#49453,#49454,#49455,#49456,#49457,#49458,
#49459,#49460,#49461,#49462,#49463,#49464,#49465,#49466,#49467,#49468,#49469,
#49470,#49471,#49472,#49473,#49474,#49475,#49476,#49477,#49478,#49479,#49480,
#49481,#49482,#49483),.UNSPECIFIED.,.F.,.F.,(4,2,2,2,2,2,2,2,2,2,2,2,2,
2,2,2,2,2,2,2,2,2,2,2,2,4),(-0.242686067170977,-0.235570833340653,-0.210241480296161,
-0.177143687126316,-0.174389806930583,-0.173035598851322,-0.17196612060904,
-0.171961294888966,-0.171956533088919,-0.171951833918979,-0.171947196490059,
-0.170712853535879,-0.168546913769349,-0.165816510750283,-0.159987017369551,
-0.142400060987175,-0.112933959948163,-0.0842115242191416,-0.0801252663193682,
-0.0776491721637786,-0.0757219466205869,-0.0736257326623009,-0.0702579098612493,
-0.0587391870800611,-0.0391146113794489,-0.000564882367464451),
 .UNSPECIFIED.);
#1331=B_SPLINE_CURVE_WITH_KNOTS('',3,(#49484,#49485,#49486,#49487,#49488,
#49489,#49490,#49491,#49492,#49493,#49494,#49495,#49496,#49497,#49498,#49499,
#49500,#49501,#49502,#49503,#49504,#49505,#49506,#49507,#49508,#49509,#49510,
#49511,#49512,#49513,#49514,#49515,#49516,#49517,#49518,#49519,#49520,#49521,
#49522,#49523,#49524,#49525,#49526,#49527,#49528,#49529,#49530,#49531,#49532,
#49533,#49534,#49535,#49536,#49537,#49538,#49539,#49540,#49541,#49542,#49543,
#49544,#49545,#49546,#49547,#49548,#49549,#49550,#49551,#49552,#49553,#49554,
#49555,#49556,#49557,#49558,#49559,#49560,#49561,#49562,#49563,#49564,#49565,
#49566,#49567,#49568,#49569,#49570,#49571,#49572,#49573,#49574,#49575,#49576,
#49577,#49578,#49579,#49580,#49581,#49582,#49583,#49584,#49585,#49586,#49587,
#49588,#49589,#49590,#49591,#49592,#49593,#49594,#49595,#49596,#49597,#49598,
#49599,#49600,#49601,#49602,#49603,#49604,#49605,#49606,#49607,#49608,#49609,
#49610,#49611,#49612,#49613,#49614,#49615,#49616,#49617,#49618,#49619,#49620,
#49621,#49622,#49623,#49624,#49625,#49626,#49627,#49628,#49629,#49630,#49631,
#49632,#49633,#49634),.UNSPECIFIED.,.F.,.F.,(4,3,3,3,3,3,3,3,3,3,3,3,3,
3,3,3,3,3,3,3,3,3,3,3,3,3,3,3,3,3,3,3,3,3,3,3,3,3,3,3,3,3,3,3,3,3,3,3,3,
3,4),(172.787595947439,172.894852285427,173.000727023252,173.111892620837,
173.217480244213,173.32300413316,173.428500691763,173.534006282056,173.639625588321,
173.745310928324,173.851174989247,173.890051803932,173.995923020582,174.107089058314,
174.212673151851,174.318193517071,174.423686563397,174.529188658208,174.63480451627,
174.740486431252,174.846347133457,174.885251322437,174.991127614625,175.102293017914,
175.207882130164,175.313407480416,175.418905470766,175.524412461228,175.63003311208,
175.735719766205,175.841585083887,175.880450840942,175.98632964872,176.097494737561,
176.203086517862,176.308614584271,176.414115334286,176.519625123373,176.625248612265,
176.730938130519,176.836806324186,176.875650359446,176.981508508061,177.0871824446,
177.192752734883,177.298255901997,177.403728384724,177.509271423133,177.61484564062,
177.720590257694,177.819192458502),.UNSPECIFIED.);
#1332=B_SPLINE_CURVE_WITH_KNOTS('',3,(#49638,#49639,#49640,#49641,#49642,
#49643,#49644,#49645,#49646,#49647,#49648,#49649,#49650,#49651,#49652,#49653,
#49654,#49655,#49656,#49657,#49658,#49659,#49660,#49661,#49662,#49663,#49664,
#49665,#49666,#49667,#49668,#49669,#49670,#49671,#49672,#49673,#49674,#49675,
#49676,#49677,#49678,#49679,#49680,#49681,#49682,#49683,#49684,#49685,#49686,
#49687,#49688,#49689,#49690,#49691,#49692,#49693,#49694,#49695,#49696,#49697,
#49698,#49699,#49700,#49701,#49702,#49703,#49704),.UNSPECIFIED.,.F.,.F.,
(4,3,3,3,3,3,3,3,3,3,3,3,3,3,3,3,3,3,3,3,3,3,4),(-4.03543298028442,-3.98079807401883,
-3.87997784099943,-3.77930285740571,-3.67874561621863,-3.57825284400111,
-3.47779351922475,-3.3773366620498,-3.27678386921224,-3.17618423154693,
-3.0754091542649,-2.98559855551413,-2.88484766263545,-2.78423921728324,
-2.68374404659775,-2.58331059978388,-2.48290779801925,-2.38250460150961,
-2.28200066564049,-2.18144732608841,-2.08071375859153,-1.99039903700942,
-1.98502202421793),.UNSPECIFIED.);
#1333=B_SPLINE_CURVE_WITH_KNOTS('',3,(#49708,#49709,#49710,#49711,#49712),
 .UNSPECIFIED.,.F.,.F.,(4,1,4),(0.,0.995199518504699,1.09118169752335),
 .UNSPECIFIED.);
#1334=B_SPLINE_CURVE_WITH_KNOTS('',3,(#49714,#49715,#49716,#49717,#49718,
#49719,#49720,#49721,#49722,#49723,#49724,#49725,#49726,#49727,#49728,#49729,
#49730,#49731,#49732,#49733,#49734,#49735,#49736,#49737,#49738,#49739,#49740,
#49741,#49742,#49743,#49744,#49745,#49746,#49747,#49748,#49749,#49750,#49751,
#49752,#49753,#49754,#49755,#49756,#49757,#49758,#49759,#49760,#49761,#49762,
#49763,#49764,#49765,#49766,#49767,#49768,#49769,#49770,#49771,#49772,#49773,
#49774,#49775,#49776,#49777,#49778,#49779,#49780,#49781,#49782,#49783,#49784,
#49785,#49786,#49787,#49788,#49789,#49790,#49791,#49792,#49793,#49794,#49795,
#49796,#49797,#49798,#49799,#49800,#49801,#49802,#49803,#49804,#49805,#49806,
#49807,#49808,#49809,#49810,#49811,#49812,#49813,#49814,#49815,#49816,#49817,
#49818,#49819,#49820,#49821,#49822,#49823,#49824,#49825,#49826,#49827,#49828,
#49829,#49830,#49831,#49832,#49833,#49834,#49835,#49836,#49837,#49838,#49839,
#49840,#49841,#49842,#49843,#49844,#49845,#49846,#49847,#49848,#49849,#49850,
#49851,#49852,#49853,#49854,#49855,#49856,#49857,#49858,#49859,#49860,#49861,
#49862,#49863,#49864,#49865,#49866,#49867,#49868,#49869,#49870,#49871,#49872,
#49873,#49874,#49875,#49876,#49877,#49878,#49879,#49880,#49881,#49882,#49883,
#49884,#49885,#49886,#49887,#49888,#49889,#49890,#49891,#49892,#49893,#49894,
#49895,#49896,#49897,#49898,#49899,#49900,#49901,#49902,#49903),
 .UNSPECIFIED.,.F.,.F.,(4,3,3,3,3,3,3,3,3,3,3,3,3,3,3,3,3,3,3,3,3,3,3,3,
3,3,3,3,3,3,3,3,3,3,3,3,3,3,3,3,3,3,3,3,3,3,3,3,3,3,3,3,3,3,3,3,3,3,3,3,
3,3,3,4),(1.09118169752335,1.18963615437418,1.28973151470358,1.38794123898432,
1.48609770063967,1.58423432078809,1.68577549984342,1.78403284001534,1.88721593851237,
1.99039903700941,2.09116037479013,2.19177691929166,2.29227662977098,2.39271244684173,
2.49311545338774,2.59351669119274,2.69401529414065,2.79456144284928,2.89528477765136,
2.98559855551411,3.08640030485475,3.18706082314412,3.28760969790442,3.38809782241632,
3.48855621210923,3.58901584426918,3.68957719963664,3.79018858726309,3.89098063411128,
3.98079807401882,4.08130696164147,4.18166936812423,4.28191363655008,4.38209334175167,
4.4822399338952,4.58238482155049,4.68262899353893,4.78292135853078,4.88339499444592,
4.97599759252353,5.07665610324085,5.17717000061932,5.27756785995971,5.37790236639782,
5.47820475574583,5.57850622331588,5.67890711758334,5.77935653576083,5.87998594870358,
5.97119711102824,6.07184943593958,6.17235746762015,6.27274997609054,6.3730794484051,
6.47337712835462,6.57367421953878,6.67407129617918,6.77451719672591,6.87514364485227,
6.96639662953295,7.077331363177,7.18794283858982,7.29800909371209,7.37436700431324),
 .UNSPECIFIED.);
#1335=B_SPLINE_CURVE_WITH_KNOTS('',3,(#49905,#49906,#49907,#49908,#49909,
#49910,#49911,#49912,#49913,#49914,#49915,#49916,#49917,#49918,#49919,#49920,
#49921,#49922,#49923,#49924,#49925,#49926,#49927,#49928,#49929,#49930,#49931,
#49932,#49933,#49934,#49935,#49936,#49937,#49938,#49939,#49940,#49941,#49942,
#49943,#49944,#49945,#49946,#49947,#49948,#49949,#49950,#49951,#49952,#49953,
#49954,#49955,#49956,#49957,#49958,#49959,#49960,#49961,#49962,#49963,#49964,
#49965,#49966,#49967,#49968,#49969,#49970,#49971,#49972,#49973,#49974,#49975,
#49976,#49977,#49978,#49979,#49980,#49981,#49982,#49983,#49984,#49985,#49986,
#49987,#49988,#49989,#49990,#49991,#49992,#49993,#49994,#49995,#49996,#49997,
#49998,#49999,#50000,#50001,#50002,#50003,#50004,#50005,#50006,#50007,#50008,
#50009,#50010,#50011,#50012,#50013,#50014,#50015,#50016,#50017,#50018,#50019,
#50020,#50021,#50022,#50023,#50024,#50025,#50026,#50027,#50028,#50029,#50030,
#50031,#50032,#50033,#50034,#50035,#50036,#50037,#50038,#50039,#50040,#50041,
#50042,#50043,#50044,#50045,#50046,#50047,#50048,#50049,#50050,#50051,#50052,
#50053,#50054,#50055,#50056,#50057,#50058,#50059,#50060,#50061,#50062,#50063,
#50064,#50065,#50066,#50067,#50068,#50069,#50070,#50071,#50072,#50073,#50074,
#50075,#50076,#50077,#50078,#50079,#50080,#50081,#50082,#50083,#50084,#50085,
#50086,#50087,#50088,#50089,#50090,#50091,#50092,#50093,#50094,#50095,#50096,
#50097),.UNSPECIFIED.,.F.,.F.,(4,3,3,3,3,3,3,3,3,3,3,3,3,3,3,3,3,3,3,3,
3,3,3,3,3,3,3,3,3,3,3,3,3,3,3,3,3,3,3,3,3,3,3,3,3,3,3,3,3,3,3,3,3,3,3,3,
3,3,3,3,3,3,3,3,4),(7.37436700470293,7.47623210060709,7.57814056338098,
7.68020247595503,7.78234477542899,7.88469717684685,7.96159614803766,8.06223414660923,
8.16272746632172,8.26310474994611,8.36341869192005,8.46370055755739,8.56398157169686,
8.66436226855847,8.76479159750012,8.86540134129867,8.95679566654237,9.05743094783625,
9.15792156441644,9.25829617966797,9.35860747576356,9.45888672184735,9.55916514661096,
9.65954332022051,9.75997015810087,9.86057749497037,9.95199518504709,10.0526261103251,
10.1531122834455,10.2534823443239,10.3537890205745,10.4540635877761,10.5543372809956,
10.6547106729914,10.7551326942182,10.8557352111616,10.9471947035518,11.0478287988039,
11.148318187236,11.2486915164575,11.3490014918313,11.4492793843046,11.54955642434,
11.6499331736749,11.7503585633559,11.8509644282025,11.9423942220565,12.0430276962745,
12.1435164614777,12.2438891671998,12.3441985192097,12.4444757893439,12.5447522089552,
12.6451283452818,12.7455531250382,12.8461583923753,12.9375937405612,13.0373122504327,
13.1368975488485,13.2363822102156,13.3357986874663,13.4352009865847,13.5345968719368,
13.6340503460223,13.6575523118825),.UNSPECIFIED.);
#1336=B_SPLINE_CURVE_WITH_KNOTS('',3,(#50099,#50100,#50101,#50102,#50103,
#50104,#50105,#50106,#50107,#50108,#50109,#50110,#50111,#50112,#50113,#50114,
#50115,#50116,#50117,#50118,#50119,#50120,#50121,#50122,#50123,#50124,#50125,
#50126,#50127,#50128,#50129,#50130,#50131,#50132,#50133,#50134,#50135,#50136,
#50137,#50138,#50139,#50140,#50141,#50142,#50143,#50144,#50145,#50146,#50147,
#50148,#50149,#50150,#50151,#50152,#50153,#50154,#50155,#50156,#50157,#50158,
#50159,#50160,#50161,#50162,#50163,#50164,#50165,#50166,#50167,#50168,#50169,
#50170,#50171,#50172,#50173,#50174,#50175,#50176,#50177,#50178,#50179,#50180,
#50181,#50182,#50183,#50184,#50185,#50186,#50187,#50188,#50189,#50190,#50191,
#50192,#50193,#50194,#50195,#50196,#50197,#50198,#50199,#50200,#50201,#50202,
#50203,#50204,#50205,#50206,#50207,#50208,#50209,#50210,#50211,#50212,#50213,
#50214,#50215,#50216,#50217,#50218,#50219,#50220,#50221,#50222,#50223,#50224,
#50225,#50226,#50227,#50228,#50229,#50230,#50231,#50232,#50233,#50234,#50235,
#50236,#50237,#50238,#50239,#50240,#50241,#50242,#50243,#50244,#50245,#50246,
#50247,#50248,#50249,#50250,#50251,#50252,#50253,#50254,#50255,#50256,#50257,
#50258,#50259,#50260,#50261,#50262,#50263,#50264,#50265,#50266,#50267,#50268,
#50269,#50270,#50271,#50272,#50273,#50274,#50275,#50276,#50277,#50278,#50279,
#50280,#50281,#50282,#50283,#50284,#50285,#50286,#50287,#50288,#50289,#50290,
#50291),.UNSPECIFIED.,.F.,.F.,(4,3,3,3,3,3,3,3,3,3,3,3,3,3,3,3,3,3,3,3,
3,3,3,3,3,3,3,3,3,3,3,3,3,3,3,3,3,3,3,3,3,3,3,3,3,3,3,3,3,3,3,3,3,3,3,3,
3,3,3,3,3,3,3,3,4),(13.6575523121158,13.7815219879644,13.9076259063269,
13.9327932590659,14.0334266816178,14.1339153909878,14.2342880348259,14.3345973212899,
14.4348745223014,14.5351508692947,14.6355269279752,14.7359516272088,14.8365568100598,
14.9279927775706,15.0286260828516,15.1291146740881,15.2294871990636,15.3297963662775,
15.4300734478205,15.5303496752957,15.6307256152235,15.7311501959341,15.8317552620445,
15.9231922960753,16.0238255491891,16.1243140869664,16.2246865567843,16.324995667831,
16.425272692275,16.525548861796,16.6259247428236,16.7263492640218,16.8269542702739,
16.9183918145801,17.019025128215,17.1195137274687,17.2198862599111,17.3201954342525,
17.4204725225729,17.5207487564637,17.6211247021888,17.7215492883672,17.8221543593193,
17.9135913330848,18.0142246266121,18.1147132055655,18.2150857175149,18.3153948712555,
18.4156719388965,18.5159481520584,18.6163240771223,18.7167486426438,18.8173536931884,
18.9087908515895,19.0094241403,19.1099127142906,19.2102852210797,19.3105943695423,
19.4108714317945,19.5111476394641,19.6115235589104,19.7119481187367,19.8125531635206,
19.9039903700942,19.9407376190621),.UNSPECIFIED.);
#1337=B_SPLINE_CURVE_WITH_KNOTS('',3,(#50293,#50294,#50295,#50296,#50297,
#50298,#50299,#50300,#50301,#50302,#50303,#50304,#50305,#50306,#50307,#50308,
#50309,#50310,#50311,#50312,#50313,#50314,#50315,#50316,#50317,#50318,#50319,
#50320,#50321,#50322,#50323,#50324,#50325,#50326,#50327,#50328,#50329,#50330,
#50331,#50332,#50333,#50334,#50335,#50336,#50337,#50338,#50339,#50340,#50341,
#50342,#50343,#50344,#50345,#50346,#50347,#50348,#50349,#50350,#50351,#50352,
#50353,#50354,#50355,#50356,#50357,#50358,#50359,#50360,#50361,#50362,#50363,
#50364,#50365,#50366,#50367,#50368,#50369,#50370,#50371,#50372,#50373,#50374,
#50375,#50376,#50377,#50378,#50379,#50380,#50381,#50382,#50383,#50384,#50385,
#50386,#50387,#50388,#50389,#50390,#50391,#50392,#50393,#50394,#50395,#50396,
#50397,#50398,#50399,#50400,#50401,#50402,#50403,#50404,#50405,#50406,#50407,
#50408,#50409,#50410,#50411,#50412,#50413,#50414,#50415,#50416,#50417,#50418,
#50419,#50420,#50421,#50422,#50423,#50424,#50425,#50426,#50427,#50428,#50429,
#50430,#50431,#50432,#50433,#50434,#50435,#50436,#50437,#50438,#50439,#50440,
#50441,#50442,#50443,#50444,#50445,#50446,#50447,#50448,#50449,#50450,#50451,
#50452,#50453,#50454,#50455,#50456,#50457,#50458,#50459,#50460,#50461,#50462,
#50463,#50464,#50465,#50466,#50467,#50468,#50469,#50470,#50471,#50472,#50473,
#50474,#50475,#50476,#50477,#50478,#50479,#50480,#50481,#50482),
 .UNSPECIFIED.,.F.,.F.,(4,3,3,3,3,3,3,3,3,3,3,3,3,3,3,3,3,3,3,3,3,3,3,3,
3,3,3,3,3,3,3,3,3,3,3,3,3,3,3,3,3,3,3,3,3,3,3,3,3,3,3,3,3,3,3,3,3,3,3,3,
3,3,3,4),(19.9407376193107,20.0407702233511,20.1406607870345,20.2404402949026,
20.3401604465629,20.4398532798881,20.539550795928,20.639349904067,20.739204086973,
20.8392274864441,20.8991898885989,20.9998231821237,21.1003117610257,21.2006842728501,
21.3009934264208,21.4012704938471,21.5015467067495,21.601922631485,21.7023471966396,
21.8029522467564,21.8943894071036,21.9950227003054,22.0955112788694,22.195883790334,
22.2961929435321,22.3964700105732,22.4967462230784,22.5971221474006,22.6975467121326,
22.7981517618153,22.8895889256083,22.990222219855,23.0907107994821,23.1910833120322,
23.2913924663288,23.3916695344803,23.4919457481059,23.5923216735563,23.6927462394227,
23.7933512902372,23.884788444113,23.9854217378588,24.0859103169787,24.1862828290149,
24.2865919827936,24.3868690504238,24.4871452635258,24.5875211884525,24.6879457537941,
24.7885508040885,24.8799879626177,24.9806212563667,25.0811098354885,25.1814823475244,
25.2817915013017,25.3820685689291,25.4823447820271,25.5827207069478,25.683145272282,
25.7837503225673,25.8751874811224,25.9913760242763,26.1076493578189,26.2239226913614),
 .UNSPECIFIED.);
#1338=B_SPLINE_CURVE_WITH_KNOTS('',3,(#50484,#50485,#50486,#50487,#50488,
#50489,#50490,#50491,#50492,#50493),.UNSPECIFIED.,.F.,.F.,(4,1,1,1,1,1,
1,4),(26.2239229262417,26.8703869996271,27.8655865181318,28.8607860366366,
29.8559855551413,30.851185073646,31.8463845921507,32.5071082334213),
 .UNSPECIFIED.);
#1339=B_SPLINE_CURVE_WITH_KNOTS('',3,(#50495,#50496,#50497,#50498,#50499,
#50500,#50501,#50502,#50503,#50504),.UNSPECIFIED.,.F.,.F.,(4,1,1,1,1,1,
1,4),(32.5071082334213,32.8415841106554,33.8367836291601,34.8319831476648,
35.8271826661695,36.8223821846742,37.8175817031789,38.7902935406009),
 .UNSPECIFIED.);
#1340=B_SPLINE_CURVE_WITH_KNOTS('',3,(#50506,#50507,#50508,#50509,#50510,
#50511,#50512,#50513,#50514,#50515,#50516),.UNSPECIFIED.,.F.,.F.,(4,1,1,
1,1,1,1,1,4),(38.7902935406009,38.8127812216836,39.8079807401883,40.803180258693,
41.7983797771977,42.7935792957025,43.7887788142072,44.7839783327119,45.0734788477805),
 .UNSPECIFIED.);
#1341=B_SPLINE_CURVE_WITH_KNOTS('',3,(#50518,#50519,#50520,#50521,#50522,
#50523,#50524,#50525,#50526,#50527),.UNSPECIFIED.,.F.,.F.,(4,1,1,1,1,1,
1,4),(45.0734788477805,45.7791778512166,46.7743773697213,47.769576888226,
48.7647764067307,49.7599759252354,50.7551754437401,51.35666415496),
 .UNSPECIFIED.);
#1342=B_SPLINE_CURVE_WITH_KNOTS('',3,(#50529,#50530,#50531,#50532,#50533,
#50534,#50535,#50536,#50537,#50538),.UNSPECIFIED.,.F.,.F.,(4,1,1,1,1,1,
1,4),(51.35666415496,51.7503749622449,52.7455744807496,53.7407739992543,
54.735973517759,55.7311730362637,56.7263725547684,57.6398494621397),
 .UNSPECIFIED.);
#1343=B_SPLINE_CURVE_WITH_KNOTS('',3,(#50540,#50541,#50542,#50543,#50544,
#50545,#50546,#50547,#50548,#50549,#50550),.UNSPECIFIED.,.F.,.F.,(4,1,1,
1,1,1,1,1,4),(57.6398494621397,57.7215720732731,58.7167715917778,59.7119711102825,
60.7071706287872,61.7023701472919,62.6975696657966,63.6927691843013,63.9230347693192),
 .UNSPECIFIED.);
#1344=B_SPLINE_CURVE_WITH_KNOTS('',3,(#50552,#50553,#50554,#50555,#50556,
#50557,#50558,#50559,#50560,#50561),.UNSPECIFIED.,.F.,.F.,(4,1,1,1,1,1,
1,4),(63.9230347693192,64.687968702806,65.6831682213108,66.6783677398155,
67.6735672583202,68.6687667768249,69.6639662953296,70.2062200764988),
 .UNSPECIFIED.);
#1345=B_SPLINE_CURVE_WITH_KNOTS('',3,(#50563,#50564,#50565,#50566,#50567,
#50568,#50569,#50570,#50571,#50572),.UNSPECIFIED.,.F.,.F.,(4,1,1,1,1,1,
1,4),(70.2062200764988,70.6591658138343,71.654365332339,72.6495648508437,
73.6447643693484,74.6399638878531,75.6351634063578,76.4893976728457),
 .UNSPECIFIED.);
#1346=B_SPLINE_CURVE_WITH_KNOTS('',3,(#50574,#50575,#50576,#50577,#50578,
#50579,#50580,#50581,#50582,#50583,#50584,#50585,#50586,#50587,#50588,#50589,
#50590,#50591,#50592,#50593,#50594,#50595,#50596,#50597,#50598,#50599,#50600,
#50601,#50602,#50603,#50604,#50605,#50606,#50607,#50608,#50609,#50610,#50611,
#50612,#50613,#50614,#50615,#50616,#50617,#50618,#50619,#50620,#50621,#50622,
#50623,#50624,#50625,#50626,#50627,#50628,#50629,#50630,#50631,#50632,#50633,
#50634,#50635,#50636,#50637,#50638,#50639,#50640,#50641,#50642,#50643,#50644,
#50645,#50646,#50647,#50648,#50649,#50650,#50651,#50652,#50653,#50654,#50655,
#50656,#50657,#50658,#50659,#50660,#50661,#50662,#50663,#50664,#50665,#50666,
#50667,#50668,#50669,#50670,#50671,#50672,#50673,#50674,#50675,#50676,#50677,
#50678,#50679,#50680,#50681,#50682,#50683,#50684,#50685,#50686,#50687,#50688,
#50689,#50690,#50691,#50692,#50693,#50694,#50695,#50696,#50697,#50698,#50699,
#50700,#50701,#50702,#50703,#50704,#50705,#50706,#50707,#50708,#50709,#50710,
#50711,#50712,#50713,#50714,#50715,#50716,#50717,#50718,#50719,#50720,#50721,
#50722,#50723,#50724,#50725,#50726,#50727,#50728,#50729,#50730,#50731,#50732,
#50733,#50734,#50735,#50736,#50737,#50738,#50739,#50740,#50741,#50742,#50743,
#50744,#50745,#50746,#50747,#50748,#50749,#50750,#50751,#50752,#50753,#50754,
#50755,#50756,#50757,#50758,#50759,#50760,#50761,#50762,#50763),
 .UNSPECIFIED.,.F.,.F.,(4,3,3,3,3,3,3,3,3,3,3,3,3,3,3,3,3,3,3,3,3,3,3,3,
3,3,3,3,3,3,3,3,3,3,3,3,3,3,3,3,3,3,3,3,3,3,3,3,3,3,3,3,3,3,3,3,3,3,3,3,
3,3,3,4),(76.4894053836784,76.6303629248626,76.7309962186831,76.8314847978778,
76.9318573099886,77.0321664638419,77.1324435315463,77.2327197447224,77.333095669722,
77.433520235136,77.534125285501,77.6255624433673,77.726195737188,77.826684316383,
77.9270568284941,78.0273659823476,78.1276430500524,78.2279192632286,78.3282951882285,
78.4287197536428,78.5293248040081,78.620761961872,78.7213952556924,78.8218838348872,
78.922256346998,79.0225655008513,79.1228425685558,79.2231187817318,79.3234947067314,
79.4239192721455,79.5245243225105,79.6159614803767,79.7165947741972,79.817083353392,
79.9174558655028,80.0177650193562,80.1180420870607,80.2183183002368,80.3186942252365,
80.4191187906506,80.5197238410157,80.6111609988814,80.711794292702,80.8122828718968,
80.9126553840076,81.0129645378611,81.1132416055656,81.2135178187418,81.3138937437415,
81.4143183091556,81.5149233595208,81.6063605173861,81.7069938112066,81.8074823904016,
81.9078549025124,82.0081640563658,82.1084411240703,82.2087173372464,82.309093262246,
82.4095178276602,82.5101228780253,82.6015600358908,82.7574881024976,82.772590690858),
 .UNSPECIFIED.);
#1347=B_SPLINE_CURVE_WITH_KNOTS('',3,(#50765,#50766,#50767,#50768,#50769,
#50770,#50771,#50772,#50773,#50774,#50775,#50776,#50777,#50778,#50779,#50780,
#50781,#50782,#50783,#50784,#50785,#50786,#50787,#50788,#50789,#50790,#50791,
#50792,#50793,#50794,#50795,#50796,#50797,#50798,#50799,#50800,#50801,#50802,
#50803,#50804,#50805,#50806,#50807,#50808,#50809,#50810,#50811,#50812,#50813,
#50814,#50815,#50816,#50817,#50818,#50819,#50820,#50821,#50822,#50823,#50824,
#50825,#50826,#50827,#50828,#50829,#50830,#50831,#50832,#50833,#50834,#50835,
#50836,#50837,#50838,#50839,#50840,#50841,#50842,#50843,#50844,#50845,#50846,
#50847,#50848,#50849,#50850,#50851,#50852,#50853,#50854,#50855,#50856,#50857,
#50858,#50859,#50860,#50861,#50862,#50863,#50864,#50865,#50866,#50867,#50868,
#50869,#50870,#50871,#50872,#50873,#50874,#50875,#50876,#50877,#50878,#50879,
#50880,#50881,#50882,#50883,#50884,#50885,#50886,#50887,#50888,#50889,#50890,
#50891,#50892,#50893,#50894,#50895,#50896,#50897,#50898,#50899,#50900,#50901,
#50902,#50903,#50904,#50905,#50906,#50907,#50908,#50909,#50910,#50911,#50912,
#50913,#50914,#50915,#50916,#50917,#50918,#50919,#50920,#50921,#50922,#50923,
#50924,#50925,#50926,#50927,#50928,#50929,#50930,#50931,#50932,#50933,#50934,
#50935,#50936,#50937,#50938,#50939,#50940,#50941,#50942,#50943,#50944,#50945,
#50946,#50947,#50948,#50949,#50950,#50951,#50952,#50953,#50954,#50955,#50956,
#50957),.UNSPECIFIED.,.F.,.F.,(4,3,3,3,3,3,3,3,3,3,3,3,3,3,3,3,3,3,3,3,
3,3,3,3,3,3,3,3,3,3,3,3,3,3,3,3,3,3,3,3,3,3,3,3,3,3,3,3,3,3,3,3,3,3,3,3,
3,3,3,3,3,3,3,3,4),(82.7725906911482,82.8756117990541,82.9744965836673,
83.0733239779893,83.1721269406444,83.2709383939143,83.3698510039825,83.4688238473439,
83.5679537129612,83.5967595543955,83.6973928482161,83.797881427411,83.8982539395219,
83.9985630933753,84.0988401610799,84.1991163742559,84.2994922992556,84.3999168646698,
84.500521915035,84.5919590729002,84.6925923667207,84.7930809459153,84.8934534580262,
84.9937626118795,85.0940396795841,85.19431589276,85.2946918177597,85.3951163831737,
85.4957214335389,85.5871585914049,85.6877918852255,85.7882804644204,85.8886529765312,
85.9889621303845,86.089239198089,86.1895154112653,86.2898913362649,86.390315901679,
86.4909209520441,86.5823581099096,86.6829914037301,86.7834799829251,86.8838524950361,
86.9841616488894,87.0844387165938,87.1847149297701,87.2850908547698,87.385515420184,
87.4861204705492,87.5775576284143,87.6781909222347,87.7786795014294,87.8790520135402,
87.9793611673935,88.0796382350979,88.1799144482744,88.280290373274,88.3807149386882,
88.4813199890532,88.572757146919,88.679242924783,88.7854091588012,88.8913805263008,
88.9970953238284,89.0557759977323),.UNSPECIFIED.);
#1348=B_SPLINE_CURVE_WITH_KNOTS('',3,(#50959,#50960,#50961,#50962,#50963,
#50964,#50965,#50966,#50967,#50968,#50969,#50970,#50971,#50972,#50973,#50974,
#50975,#50976,#50977,#50978,#50979,#50980,#50981,#50982,#50983,#50984,#50985,
#50986,#50987,#50988,#50989,#50990,#50991,#50992,#50993,#50994,#50995,#50996,
#50997,#50998,#50999,#51000,#51001,#51002,#51003,#51004,#51005,#51006,#51007,
#51008,#51009,#51010,#51011,#51012,#51013,#51014,#51015,#51016,#51017,#51018,
#51019,#51020,#51021,#51022,#51023,#51024,#51025,#51026,#51027,#51028,#51029,
#51030,#51031,#51032,#51033,#51034,#51035,#51036,#51037,#51038,#51039,#51040,
#51041,#51042,#51043,#51044,#51045,#51046,#51047,#51048,#51049,#51050,#51051,
#51052,#51053,#51054,#51055,#51056,#51057,#51058,#51059,#51060,#51061,#51062,
#51063,#51064,#51065,#51066,#51067,#51068,#51069,#51070,#51071,#51072,#51073,
#51074,#51075,#51076,#51077,#51078,#51079,#51080,#51081,#51082,#51083,#51084,
#51085,#51086,#51087,#51088,#51089,#51090,#51091,#51092,#51093,#51094,#51095,
#51096,#51097,#51098,#51099,#51100,#51101,#51102,#51103,#51104,#51105,#51106,
#51107,#51108,#51109,#51110,#51111,#51112,#51113,#51114,#51115,#51116,#51117,
#51118,#51119,#51120,#51121,#51122,#51123,#51124,#51125,#51126,#51127,#51128,
#51129,#51130,#51131,#51132,#51133,#51134,#51135,#51136,#51137,#51138,#51139,
#51140,#51141,#51142,#51143,#51144,#51145,#51146,#51147,#51148),
 .UNSPECIFIED.,.F.,.F.,(4,3,3,3,3,3,3,3,3,3,3,3,3,3,3,3,3,3,3,3,3,3,3,3,
3,3,3,3,3,3,3,3,3,3,3,3,3,3,3,3,3,3,3,3,3,3,3,3,3,3,3,3,3,3,3,3,3,3,3,3,
3,3,3,4),(89.0557759980376,89.1601699110528,89.264818149268,89.3695947912726,
89.4746481648271,89.5679566654238,89.6685899592442,89.7690785384391,89.8694510505499,
89.9697602044032,90.0700372721077,90.1703134852838,90.2706894102834,90.3711139756975,
90.4717190260625,90.5631561839285,90.6637894777491,90.764278056944,90.8646505690549,
90.9649597229083,91.0652367906129,91.1655130037891,91.2658889287888,91.366313494203,
91.4669185445681,91.5583557024332,91.6589889962538,91.7594775754488,91.8598500875596,
91.960159241413,92.0604363091175,92.1607125222936,92.2610884472932,92.3615130127074,
92.4621180630725,92.5535552209379,92.6541885147583,92.7546770939531,92.8550496060639,
92.9553587599173,93.0556358276219,93.155912040798,93.2562879657976,93.3567125312118,
93.4573175815769,93.5487547394426,93.6493880332632,93.7498766124577,93.8502491245687,
93.9505582784219,94.0508353461266,94.1511115593032,94.2514874843028,94.3519120497171,
94.4525171000822,94.5439542579473,94.6433301388161,94.7423600398394,94.841295548215,
94.9401696642849,95.0398675744382,95.1387542395913,95.2388577722446,95.3389613048979),
 .UNSPECIFIED.);
#1349=B_SPLINE_CURVE_WITH_KNOTS('',3,(#51150,#51151,#51152,#51153,#51154,
#51155,#51156,#51157,#51158,#51159,#51160,#51161,#51162,#51163,#51164,#51165,
#51166,#51167,#51168,#51169,#51170,#51171,#51172,#51173,#51174,#51175,#51176,
#51177,#51178,#51179,#51180,#51181,#51182,#51183,#51184,#51185,#51186,#51187,
#51188,#51189,#51190,#51191,#51192,#51193,#51194,#51195,#51196,#51197,#51198,
#51199,#51200,#51201,#51202,#51203,#51204,#51205,#51206,#51207,#51208,#51209,
#51210,#51211,#51212,#51213,#51214,#51215,#51216,#51217,#51218,#51219,#51220,
#51221,#51222,#51223,#51224,#51225,#51226,#51227,#51228,#51229,#51230,#51231,
#51232,#51233,#51234,#51235,#51236,#51237,#51238,#51239,#51240,#51241,#51242,
#51243,#51244,#51245,#51246,#51247,#51248,#51249,#51250,#51251,#51252,#51253,
#51254,#51255,#51256,#51257,#51258,#51259,#51260,#51261,#51262,#51263,#51264,
#51265,#51266,#51267,#51268,#51269,#51270,#51271,#51272,#51273,#51274,#51275,
#51276,#51277,#51278,#51279,#51280,#51281,#51282,#51283,#51284,#51285,#51286,
#51287,#51288,#51289,#51290,#51291,#51292,#51293,#51294,#51295,#51296,#51297,
#51298,#51299,#51300,#51301,#51302,#51303,#51304,#51305,#51306,#51307,#51308,
#51309,#51310,#51311,#51312,#51313,#51314,#51315,#51316,#51317,#51318,#51319,
#51320,#51321,#51322,#51323,#51324,#51325,#51326,#51327,#51328,#51329,#51330,
#51331,#51332,#51333,#51334,#51335,#51336,#51337,#51338,#51339),
 .UNSPECIFIED.,.F.,.F.,(4,3,3,3,3,3,3,3,3,3,3,3,3,3,3,3,3,3,3,3,3,3,3,3,
3,3,3,3,3,3,3,3,3,3,3,3,3,3,3,3,3,3,3,3,3,3,3,3,3,3,3,3,3,3,3,3,3,3,3,3,
3,3,3,4),(95.3389613052172,95.4822566433568,95.539153776452,95.6397870702726,
95.7402756494674,95.8406481615783,95.9409573154316,96.0412343831361,96.1415105963123,
96.241886521312,96.3423110867261,96.4429161370912,96.5343532949567,96.6349865887773,
96.7354751679722,96.8358476800831,96.9361568339365,97.0364339016411,97.1367101148173,
97.237086039817,97.3375106052312,97.4381156555964,97.5295528134614,97.6301861072819,
97.7306746864767,97.8310471985875,97.9313563524409,98.0316334201454,98.1319096333215,
98.2322855583211,98.3327101237352,98.4333151741003,98.5247523319661,98.6253856257866,
98.7258742049813,98.8262467170921,98.9265558709454,99.0268329386499,99.1271091518259,
99.2274850768255,99.3279096422396,99.4285146926046,99.5199518504708,99.6205851442916,
99.7210737234867,99.8214462355978,99.9217553894514,100.022032457156,100.122308670332,
100.222684595332,100.323109160747,100.423714211112,100.515151368976,100.615784662796,
100.716273241991,100.816645754102,100.916954907955,101.017231975659,101.117508188835,
101.217884113834,101.318308679248,101.418913729613,101.51035088748,101.622146612397),
 .UNSPECIFIED.);
#1350=B_SPLINE_CURVE_WITH_KNOTS('',3,(#51341,#51342,#51343,#51344,#51345,
#51346,#51347,#51348,#51349,#51350,#51351,#51352,#51353,#51354,#51355,#51356,
#51357,#51358,#51359,#51360,#51361,#51362,#51363,#51364,#51365,#51366,#51367,
#51368,#51369,#51370,#51371,#51372,#51373,#51374,#51375,#51376,#51377,#51378,
#51379,#51380,#51381,#51382,#51383,#51384,#51385,#51386,#51387,#51388,#51389,
#51390,#51391,#51392,#51393,#51394,#51395,#51396,#51397,#51398,#51399,#51400,
#51401,#51402,#51403,#51404,#51405,#51406,#51407,#51408,#51409,#51410,#51411,
#51412,#51413,#51414,#51415,#51416,#51417,#51418,#51419,#51420,#51421,#51422,
#51423,#51424,#51425,#51426,#51427,#51428,#51429,#51430,#51431,#51432,#51433,
#51434,#51435,#51436,#51437,#51438,#51439,#51440,#51441,#51442,#51443,#51444,
#51445,#51446,#51447,#51448,#51449,#51450,#51451,#51452,#51453,#51454,#51455,
#51456,#51457,#51458,#51459,#51460,#51461,#51462,#51463,#51464,#51465,#51466,
#51467,#51468,#51469,#51470,#51471,#51472,#51473,#51474,#51475,#51476,#51477,
#51478,#51479,#51480,#51481,#51482,#51483,#51484,#51485,#51486,#51487,#51488,
#51489,#51490,#51491,#51492,#51493,#51494,#51495,#51496,#51497,#51498,#51499,
#51500,#51501,#51502,#51503,#51504,#51505,#51506,#51507,#51508,#51509,#51510,
#51511,#51512,#51513,#51514,#51515,#51516,#51517,#51518,#51519,#51520,#51521,
#51522,#51523,#51524,#51525,#51526,#51527,#51528,#51529,#51530),
 .UNSPECIFIED.,.F.,.F.,(4,3,3,3,3,3,3,3,3,3,3,3,3,3,3,3,3,3,3,3,3,3,3,3,
3,3,3,3,3,3,3,3,3,3,3,3,3,3,3,3,3,3,3,3,3,3,3,3,3,3,3,3,3,3,3,3,3,3,3,3,
3,3,3,4),(101.622146612616,101.721379451865,101.820473882863,101.919491887866,
102.018466315808,102.11742995792,102.216482812235,102.31557830438,102.414849627253,
102.505550405985,102.606183699806,102.706672279001,102.807044791112,102.907353944965,
103.00763101267,103.107907225847,103.208283150846,103.308707716261,103.409312766626,
103.50074992449,103.60138321831,103.701871797505,103.802244309615,103.902553463469,
104.002830531173,104.103106744349,104.203482669348,104.303907234762,104.404512285127,
104.495949442994,104.596582736814,104.697071316009,104.79744382812,104.897752981973,
104.998030049678,105.098306262854,105.198682187854,105.299106753268,105.399711803633,
105.491148961499,105.59178225532,105.692270834515,105.792643346626,105.892952500479,
105.993229568184,106.09350578136,106.19388170636,106.294306271774,106.394911322139,
106.486348480004,106.586981773825,106.68747035302,106.787842865131,106.888152018984,
106.988429086689,107.088705299865,107.189081224865,107.289505790279,107.390110840645,
107.481547998509,107.591388936057,107.700941320827,107.810012207032,107.905331919234),
 .UNSPECIFIED.);
#1351=B_SPLINE_CURVE_WITH_KNOTS('',3,(#51532,#51533,#51534,#51535,#51536,
#51537,#51538,#51539,#51540,#51541,#51542,#51543,#51544,#51545,#51546,#51547,
#51548,#51549,#51550,#51551,#51552,#51553,#51554,#51555,#51556,#51557,#51558,
#51559,#51560,#51561,#51562,#51563,#51564,#51565,#51566,#51567,#51568,#51569,
#51570,#51571,#51572,#51573,#51574,#51575,#51576,#51577,#51578,#51579,#51580,
#51581,#51582,#51583,#51584,#51585,#51586,#51587,#51588,#51589,#51590,#51591,
#51592,#51593,#51594,#51595,#51596,#51597,#51598,#51599,#51600,#51601,#51602,
#51603,#51604,#51605,#51606,#51607,#51608,#51609,#51610,#51611,#51612,#51613,
#51614,#51615,#51616,#51617,#51618,#51619,#51620,#51621,#51622,#51623,#51624,
#51625,#51626,#51627,#51628,#51629,#51630,#51631,#51632,#51633,#51634,#51635,
#51636,#51637,#51638,#51639,#51640,#51641,#51642,#51643,#51644,#51645,#51646,
#51647,#51648,#51649,#51650,#51651,#51652,#51653,#51654,#51655,#51656,#51657,
#51658,#51659,#51660,#51661,#51662,#51663,#51664,#51665,#51666,#51667,#51668,
#51669,#51670,#51671,#51672,#51673,#51674,#51675,#51676,#51677,#51678,#51679,
#51680,#51681,#51682,#51683,#51684,#51685,#51686,#51687,#51688,#51689,#51690,
#51691,#51692,#51693,#51694,#51695,#51696,#51697,#51698,#51699,#51700,#51701,
#51702,#51703,#51704,#51705,#51706,#51707,#51708,#51709,#51710,#51711,#51712,
#51713,#51714,#51715,#51716,#51717,#51718,#51719,#51720,#51721,#51722,#51723,
#51724),.UNSPECIFIED.,.F.,.F.,(4,3,3,3,3,3,3,3,3,3,3,3,3,3,3,3,3,3,3,3,
3,3,3,3,3,3,3,3,3,3,3,3,3,3,3,3,3,3,3,3,3,3,3,3,3,3,3,3,3,3,3,3,3,3,3,3,
3,3,3,3,3,3,3,3,4),(107.905331919576,108.007663280982,108.110054337197,
108.212614455041,108.31526669938,108.418130027842,108.476747517013,108.577380810834,
108.677869390028,108.778241902139,108.878551055993,108.978828123697,109.079104336873,
109.179480261873,109.279904827287,109.380509877652,109.471947035518,109.572580329339,
109.673068908534,109.773441420645,109.873750574498,109.974027642203,110.074303855379,
110.174679780379,110.275104345793,110.375709396159,110.467146554023,110.567779847843,
110.668268427038,110.768640939148,110.868950093001,110.969227160706,111.069503373882,
111.169879298881,111.270303864295,111.37090891466,111.462346072527,111.562979366347,
111.663467945542,111.763840457653,111.864149611506,111.964426679211,112.064702892387,
112.165078817386,112.265503382801,112.366108433166,112.457545591032,112.558178884853,
112.658667464048,112.759039976159,112.859349130012,112.959626197717,113.059902410893,
113.160278335893,113.260702901308,113.361307951673,113.452745109537,113.552293832374,
113.651710936125,113.751029175624,113.850281183029,113.949525277683,114.048764705495,
114.148072690965,114.188517226756),.UNSPECIFIED.);
#1352=B_SPLINE_CURVE_WITH_KNOTS('',3,(#51726,#51727,#51728,#51729,#51730,
#51731,#51732,#51733,#51734,#51735,#51736,#51737,#51738,#51739,#51740,#51741,
#51742,#51743,#51744,#51745,#51746,#51747,#51748,#51749,#51750,#51751,#51752,
#51753,#51754,#51755,#51756,#51757,#51758,#51759,#51760,#51761,#51762,#51763,
#51764,#51765,#51766,#51767,#51768,#51769,#51770,#51771,#51772,#51773,#51774,
#51775,#51776,#51777,#51778,#51779,#51780,#51781,#51782,#51783,#51784,#51785,
#51786,#51787,#51788,#51789,#51790,#51791,#51792,#51793,#51794,#51795,#51796,
#51797,#51798,#51799,#51800,#51801,#51802,#51803,#51804,#51805,#51806,#51807,
#51808,#51809,#51810,#51811,#51812,#51813,#51814,#51815,#51816,#51817,#51818,
#51819,#51820,#51821,#51822,#51823,#51824,#51825,#51826,#51827,#51828,#51829,
#51830,#51831,#51832,#51833,#51834,#51835,#51836,#51837,#51838,#51839,#51840,
#51841,#51842,#51843,#51844,#51845,#51846,#51847,#51848,#51849,#51850,#51851,
#51852,#51853,#51854,#51855,#51856,#51857,#51858,#51859,#51860,#51861,#51862,
#51863,#51864,#51865,#51866,#51867,#51868,#51869,#51870,#51871,#51872,#51873,
#51874,#51875,#51876,#51877,#51878,#51879,#51880,#51881,#51882,#51883,#51884,
#51885,#51886,#51887,#51888,#51889,#51890,#51891,#51892,#51893,#51894,#51895,
#51896,#51897,#51898,#51899,#51900,#51901,#51902,#51903,#51904,#51905,#51906,
#51907,#51908,#51909,#51910,#51911,#51912,#51913,#51914,#51915),
 .UNSPECIFIED.,.F.,.F.,(4,3,3,3,3,3,3,3,3,3,3,3,3,3,3,3,3,3,3,3,3,3,3,3,
3,3,3,3,3,3,3,3,3,3,3,3,3,3,3,3,3,3,3,3,3,3,3,3,3,3,3,3,3,3,3,3,3,3,3,3,
3,3,3,4),(114.188517227063,114.318230927552,114.447944628041,114.548577921862,
114.649066501058,114.749439013169,114.849748167023,114.950025234728,115.050301447905,
115.150677372905,115.25110193832,115.351706988686,115.443144146546,115.543777440367,
115.644266019562,115.744638531672,115.844947685526,115.94522475323,116.045500966407,
116.145876891406,116.246301456821,116.346906507186,116.438343665051,116.538976958872,
116.639465538066,116.739838050177,116.840147204031,116.940424271735,117.040700484911,
117.141076409911,117.241500975325,117.34210602569,117.433543183556,117.534176477376,
117.634665056571,117.735037568682,117.835346722535,117.935623790239,118.035900003415,
118.136275928415,118.236700493829,118.337305544194,118.42874270206,118.52937599588,
118.629864575075,118.730237087186,118.830546241039,118.930823308744,119.03109952192,
119.13147544692,119.231900012334,119.332505062699,119.423942220565,119.524575514386,
119.625064093581,119.725436605692,119.825745759545,119.92602282725,120.026299040426,
120.126674965426,120.22709953084,120.327704581206,120.41914173907,120.471702533936),
 .UNSPECIFIED.);
#1353=B_SPLINE_CURVE_WITH_KNOTS('',3,(#51917,#51918,#51919,#51920,#51921,
#51922,#51923,#51924,#51925,#51926,#51927,#51928,#51929,#51930,#51931,#51932,
#51933,#51934,#51935,#51936,#51937,#51938,#51939,#51940,#51941,#51942,#51943,
#51944,#51945,#51946,#51947,#51948,#51949,#51950,#51951,#51952,#51953,#51954,
#51955,#51956,#51957,#51958,#51959,#51960,#51961,#51962,#51963,#51964,#51965,
#51966,#51967,#51968,#51969,#51970,#51971,#51972,#51973,#51974,#51975,#51976,
#51977,#51978,#51979,#51980,#51981,#51982,#51983,#51984,#51985,#51986,#51987,
#51988,#51989,#51990,#51991,#51992,#51993,#51994,#51995,#51996,#51997,#51998,
#51999,#52000,#52001,#52002,#52003,#52004,#52005,#52006,#52007,#52008,#52009,
#52010,#52011,#52012,#52013,#52014,#52015,#52016,#52017,#52018,#52019,#52020,
#52021,#52022,#52023,#52024,#52025,#52026,#52027,#52028,#52029,#52030,#52031,
#52032,#52033,#52034,#52035,#52036,#52037,#52038,#52039,#52040,#52041,#52042,
#52043,#52044,#52045,#52046,#52047,#52048,#52049,#52050,#52051,#52052,#52053,
#52054,#52055,#52056,#52057,#52058,#52059,#52060,#52061,#52062,#52063,#52064,
#52065,#52066,#52067,#52068,#52069,#52070,#52071,#52072,#52073,#52074,#52075,
#52076,#52077,#52078,#52079,#52080,#52081,#52082,#52083,#52084,#52085,#52086,
#52087,#52088,#52089,#52090,#52091,#52092,#52093,#52094,#52095,#52096,#52097,
#52098,#52099,#52100,#52101,#52102,#52103,#52104,#52105,#52106,#52107,#52108,
#52109),.UNSPECIFIED.,.F.,.F.,(4,3,3,3,3,3,3,3,3,3,3,3,3,3,3,3,3,3,3,3,
3,3,3,3,3,3,3,3,3,3,3,3,3,3,3,3,3,3,3,3,3,3,3,3,3,3,3,3,3,3,3,3,3,3,3,3,
3,3,3,3,3,3,3,3,4),(120.471702534264,120.571519365994,120.671196490433,
120.77076613455,120.870279000662,120.96976735932,121.069263446661,121.168862437348,
121.268519683046,121.368341435402,121.414341257574,121.514974551395,121.61546313059,
121.715835642701,121.816144796554,121.916421864259,122.016698077435,122.117074002435,
122.217498567849,122.318103618214,122.409540776079,122.5101740699,122.610662649095,
122.711035161206,122.811344315059,122.911621382764,123.01189759594,123.11227352094,
123.212698086354,123.313303136719,123.404740294584,123.505373588405,123.6058621676,
123.70623467971,123.806543833564,123.906820901268,124.007097114444,124.107473039444,
124.207897604858,124.308502655223,124.399939813089,124.500573106909,124.601061686104,
124.701434198214,124.801743352067,124.902020419772,125.002296632948,125.102672557947,
125.203097123361,125.303702173726,125.395139331593,125.495772625413,125.596261204608,
125.696633716719,125.796942870573,125.897219938277,125.997496151453,126.097872076453,
126.198296641867,126.298901692233,126.390338850098,126.504950337584,126.619096027427,
126.732458632805,126.754887840888),.UNSPECIFIED.);
#1354=B_SPLINE_CURVE_WITH_KNOTS('',3,(#52111,#52112,#52113,#52114,#52115,
#52116,#52117,#52118,#52119,#52120,#52121,#52122,#52123,#52124,#52125,#52126,
#52127,#52128,#52129,#52130,#52131,#52132,#52133,#52134,#52135,#52136,#52137,
#52138,#52139,#52140,#52141,#52142,#52143,#52144,#52145,#52146,#52147,#52148,
#52149,#52150,#52151,#52152,#52153,#52154,#52155,#52156,#52157,#52158,#52159,
#52160,#52161,#52162,#52163,#52164,#52165,#52166,#52167,#52168,#52169,#52170,
#52171,#52172,#52173,#52174,#52175,#52176,#52177,#52178,#52179,#52180,#52181,
#52182,#52183,#52184,#52185,#52186,#52187,#52188,#52189,#52190,#52191,#52192,
#52193,#52194,#52195,#52196,#52197,#52198,#52199,#52200,#52201,#52202,#52203,
#52204,#52205,#52206,#52207,#52208,#52209,#52210,#52211,#52212,#52213,#52214,
#52215,#52216,#52217,#52218,#52219,#52220,#52221,#52222,#52223,#52224,#52225,
#52226,#52227,#52228,#52229,#52230,#52231,#52232,#52233,#52234,#52235,#52236,
#52237,#52238,#52239,#52240,#52241,#52242,#52243,#52244,#52245,#52246,#52247,
#52248,#52249,#52250,#52251,#52252,#52253,#52254,#52255,#52256,#52257,#52258,
#52259,#52260,#52261,#52262,#52263,#52264,#52265,#52266,#52267,#52268,#52269,
#52270,#52271,#52272,#52273,#52274,#52275,#52276,#52277,#52278,#52279,#52280,
#52281,#52282,#52283,#52284,#52285,#52286,#52287,#52288,#52289,#52290,#52291,
#52292,#52293,#52294,#52295,#52296,#52297,#52298,#52299,#52300,#52301,#52302,
#52303),.UNSPECIFIED.,.F.,.F.,(4,3,3,3,3,3,3,3,3,3,3,3,3,3,3,3,3,3,3,3,
3,3,3,3,3,3,3,3,3,3,3,3,3,3,3,3,3,3,3,3,3,3,3,3,3,3,3,3,3,3,3,3,3,3,3,3,
3,3,3,3,3,3,3,3,4),(126.754887841115,126.855723392772,126.956565229927,
127.057443412667,127.158455072141,127.259546174342,127.360812752503,127.385538368603,
127.486171662423,127.586660241617,127.687032753728,127.787341907581,127.887618975285,
127.987895188461,128.08827111346,128.188695678874,128.289300729239,128.380737887107,
128.481371180928,128.581859760122,128.682232272233,128.782541426087,128.882818493791,
128.983094706967,129.083470631967,129.183895197381,129.284500247746,129.375937405612,
129.476570699433,129.577059278628,129.677431790739,129.777740944592,129.878018012297,
129.978294225474,130.078670150473,130.179094715888,130.279699766253,130.371136924117,
130.471770217938,130.572258797132,130.672631309243,130.772940463097,130.873217530801,
130.973493743977,131.073869668977,131.174294234391,131.274899284756,131.366336442622,
131.466969736442,131.567458315637,131.667830827747,131.768139981601,131.868417049305,
131.96869326248,132.06906918748,132.169493752893,132.270098803258,132.361535961126,
132.461872922284,132.562070807988,132.662161436375,132.762184969317,132.862166822976,
132.962174894668,133.038073148295),.UNSPECIFIED.);
#1355=B_SPLINE_CURVE_WITH_KNOTS('',3,(#52305,#52306,#52307,#52308,#52309,
#52310,#52311,#52312,#52313,#52314,#52315,#52316,#52317,#52318,#52319,#52320,
#52321,#52322,#52323,#52324,#52325,#52326,#52327,#52328,#52329,#52330,#52331,
#52332,#52333,#52334,#52335,#52336,#52337,#52338,#52339,#52340,#52341,#52342,
#52343,#52344,#52345,#52346,#52347,#52348,#52349,#52350,#52351,#52352,#52353,
#52354,#52355,#52356,#52357,#52358,#52359,#52360,#52361,#52362,#52363,#52364,
#52365,#52366,#52367,#52368,#52369,#52370,#52371,#52372,#52373,#52374,#52375,
#52376,#52377,#52378,#52379,#52380,#52381,#52382,#52383,#52384,#52385,#52386,
#52387,#52388,#52389,#52390,#52391,#52392,#52393,#52394,#52395,#52396,#52397,
#52398,#52399,#52400,#52401,#52402,#52403,#52404,#52405,#52406,#52407,#52408,
#52409,#52410,#52411,#52412,#52413,#52414,#52415,#52416,#52417,#52418,#52419,
#52420,#52421,#52422,#52423,#52424,#52425,#52426,#52427,#52428,#52429,#52430,
#52431,#52432,#52433,#52434,#52435,#52436,#52437,#52438,#52439,#52440,#52441,
#52442,#52443,#52444,#52445,#52446,#52447,#52448,#52449,#52450,#52451,#52452,
#52453,#52454,#52455,#52456,#52457,#52458,#52459,#52460,#52461,#52462,#52463,
#52464,#52465,#52466,#52467,#52468,#52469,#52470,#52471,#52472,#52473,#52474,
#52475,#52476,#52477,#52478,#52479,#52480,#52481,#52482,#52483,#52484,#52485,
#52486,#52487,#52488,#52489,#52490,#52491,#52492,#52493,#52494),
 .UNSPECIFIED.,.F.,.F.,(4,3,3,3,3,3,3,3,3,3,3,3,3,3,3,3,3,3,3,3,3,3,3,3,
3,3,3,3,3,3,3,3,3,3,3,3,3,3,3,3,3,3,3,3,3,3,3,3,3,3,3,3,3,3,3,3,3,3,3,3,
3,3,3,4),(133.03807314869,133.156219331711,133.275714063615,133.356735479631,
133.457368773452,133.557857352647,133.658229864758,133.758539018612,133.858816086317,
133.959092299493,134.059468224493,134.159892789908,134.260497840273,134.351934998136,
134.452568291956,134.553056871151,134.653429383261,134.753738537115,134.854015604819,
134.954291817995,135.054667742994,135.155092308408,135.255697358773,135.34713451664,
135.447767810461,135.548256389655,135.648628901766,135.74893805562,135.849215123324,
135.9494913365,136.0498672615,136.150291826914,136.250896877279,136.342334035145,
136.442967328966,136.543455908161,136.643828420272,136.744137574125,136.84441464183,
136.944690855007,137.045066780006,137.145491345421,137.246096395786,137.33753355365,
137.43816684747,137.538655426665,137.639027938776,137.739337092629,137.839614160334,
137.93989037351,138.040266298509,138.140690863923,138.241295914288,138.332733072154,
138.433247204163,138.533616703136,138.633870529462,138.73406141901,138.834220810923,
138.934380104271,139.034639201367,139.134947940025,139.235434997304,139.321258455253),
 .UNSPECIFIED.);
#1356=B_SPLINE_CURVE_WITH_KNOTS('',3,(#52496,#52497,#52498,#52499,#52500,
#52501,#52502,#52503,#52504,#52505,#52506,#52507,#52508,#52509,#52510,#52511,
#52512,#52513,#52514,#52515,#52516,#52517,#52518,#52519,#52520,#52521,#52522,
#52523,#52524,#52525,#52526,#52527,#52528,#52529,#52530,#52531,#52532,#52533,
#52534,#52535,#52536,#52537,#52538,#52539,#52540,#52541,#52542,#52543,#52544,
#52545,#52546,#52547,#52548,#52549,#52550,#52551,#52552,#52553,#52554,#52555,
#52556,#52557,#52558,#52559,#52560,#52561,#52562,#52563,#52564,#52565,#52566,
#52567,#52568,#52569,#52570,#52571,#52572,#52573,#52574,#52575,#52576,#52577,
#52578,#52579,#52580,#52581,#52582,#52583,#52584,#52585,#52586,#52587,#52588,
#52589,#52590,#52591,#52592,#52593,#52594,#52595,#52596,#52597,#52598,#52599,
#52600,#52601,#52602,#52603,#52604,#52605,#52606,#52607,#52608,#52609,#52610,
#52611,#52612,#52613,#52614,#52615,#52616,#52617,#52618,#52619,#52620,#52621,
#52622,#52623,#52624,#52625,#52626,#52627,#52628,#52629,#52630,#52631,#52632,
#52633,#52634,#52635,#52636,#52637,#52638,#52639,#52640,#52641,#52642,#52643,
#52644,#52645,#52646,#52647,#52648,#52649,#52650,#52651,#52652,#52653,#52654,
#52655,#52656,#52657,#52658,#52659,#52660,#52661,#52662,#52663,#52664,#52665,
#52666,#52667,#52668,#52669,#52670,#52671,#52672,#52673,#52674,#52675,#52676,
#52677,#52678,#52679,#52680,#52681,#52682,#52683,#52684,#52685,#52686,#52687,
#52688),.UNSPECIFIED.,.F.,.F.,(4,3,3,3,3,3,3,3,3,3,3,3,3,3,3,3,3,3,3,3,
3,3,3,3,3,3,3,3,3,3,3,3,3,3,3,3,3,3,3,3,3,3,3,3,3,3,3,3,3,3,3,3,3,3,3,3,
3,3,3,3,3,3,3,3,4),(139.321258455474,139.327932590659,139.428565884479,
139.529054463673,139.629426975784,139.729736129637,139.830013197341,139.930289410516,
140.030665335515,140.131089900929,140.231694951294,140.323132109164,140.423765402986,
140.524253982182,140.624626494294,140.724935648149,140.825212715855,140.925488929032,
141.025864854033,141.126289419449,141.226894469815,141.318331627669,141.418964921488,
141.519453500682,141.619826012792,141.720135166644,141.820412234348,141.920688447523,
142.021064372521,142.121488937934,142.222093988298,142.313531146173,142.414164439991,
142.514653019183,142.615025531291,142.715334685142,142.815611752844,142.915887966017,
143.016263891014,143.116688456426,143.217293506788,143.308730664678,143.409363958508,
143.509852537712,143.610225049831,143.710534203694,143.810811271407,143.911087484593,
144.011463409601,144.111887975024,144.212493025398,144.303930183183,144.404563476994,
144.50505205618,144.605424568282,144.705733722127,144.806010789822,144.90628700299,
145.006662927981,145.107087493387,145.207692543744,145.299129701687,145.420579631092,
145.540533774723,145.604443762298),.UNSPECIFIED.);
#1357=B_SPLINE_CURVE_WITH_KNOTS('',3,(#52690,#52691,#52692,#52693,#52694,
#52695,#52696,#52697,#52698,#52699,#52700,#52701,#52702,#52703,#52704,#52705,
#52706,#52707,#52708,#52709,#52710,#52711,#52712,#52713,#52714,#52715,#52716,
#52717,#52718,#52719,#52720,#52721,#52722,#52723,#52724,#52725,#52726,#52727,
#52728,#52729,#52730,#52731,#52732,#52733,#52734,#52735,#52736,#52737,#52738,
#52739,#52740,#52741,#52742,#52743,#52744,#52745,#52746,#52747,#52748,#52749,
#52750,#52751,#52752,#52753,#52754,#52755,#52756,#52757,#52758,#52759,#52760,
#52761,#52762,#52763,#52764,#52765,#52766,#52767,#52768,#52769,#52770,#52771,
#52772,#52773,#52774,#52775,#52776,#52777,#52778,#52779,#52780,#52781,#52782,
#52783,#52784,#52785,#52786,#52787,#52788,#52789,#52790,#52791,#52792,#52793,
#52794,#52795,#52796,#52797,#52798,#52799,#52800,#52801,#52802,#52803,#52804,
#52805,#52806,#52807,#52808,#52809,#52810,#52811,#52812,#52813,#52814,#52815,
#52816,#52817,#52818,#52819,#52820,#52821,#52822,#52823,#52824,#52825,#52826,
#52827,#52828,#52829,#52830,#52831,#52832,#52833,#52834,#52835,#52836,#52837,
#52838,#52839,#52840,#52841,#52842,#52843,#52844,#52845,#52846,#52847,#52848,
#52849,#52850,#52851,#52852,#52853,#52854,#52855,#52856,#52857,#52858,#52859,
#52860,#52861,#52862,#52863,#52864,#52865,#52866,#52867,#52868,#52869,#52870,
#52871,#52872,#52873,#52874,#52875,#52876,#52877,#52878,#52879),
 .UNSPECIFIED.,.F.,.F.,(4,3,3,3,3,3,3,3,3,3,3,3,3,3,3,3,3,3,3,3,3,3,3,3,
3,3,3,3,3,3,3,3,3,3,3,3,3,3,3,3,3,3,3,3,3,3,3,3,3,3,3,3,3,3,3,3,3,3,3,3,
3,3,3,4),(145.604443762654,145.704257784809,145.804039315887,145.903820193958,
146.003702819992,146.103635283292,146.203751666778,146.294329220192,146.394962514076,
146.495451093335,146.59582360551,146.696132759426,146.796409827195,146.896686040434,
146.997061965496,147.097486530972,147.198091581398,147.289528738697,147.390162032438,
147.490650611553,147.591023123586,147.691332277361,147.791609344988,147.891885558087,
147.992261483012,148.092686048352,148.193291098645,148.284728257202,148.385361550952,
148.485850130075,148.586222642113,148.686531795893,148.786808863523,148.887085076624,
148.987461001549,149.087885566887,149.188490617177,149.279927775706,149.380561069975,
149.481049649619,149.581422162179,149.681731316481,149.782008384634,149.882284598256,
149.982660523697,150.083085089549,150.183690140343,150.275127294211,150.37576058735,
150.476249165865,150.576621677301,150.676930830484,150.777207897522,150.877484110037,
150.977860034389,151.078284599162,151.178889648903,151.270326812716,151.37189564131,
151.473312380576,151.57689155289,151.678083381926,151.78285622588,151.887629069833),
 .UNSPECIFIED.);
#1358=B_SPLINE_CURVE_WITH_KNOTS('',3,(#52881,#52882,#52883,#52884,#52885,
#52886,#52887,#52888,#52889,#52890,#52891,#52892,#52893,#52894,#52895,#52896,
#52897,#52898,#52899,#52900,#52901,#52902,#52903,#52904,#52905,#52906,#52907,
#52908,#52909,#52910,#52911,#52912,#52913,#52914,#52915,#52916,#52917,#52918,
#52919,#52920,#52921,#52922,#52923,#52924,#52925,#52926,#52927,#52928,#52929,
#52930,#52931,#52932,#52933,#52934,#52935,#52936,#52937,#52938,#52939,#52940,
#52941,#52942,#52943,#52944,#52945,#52946,#52947,#52948,#52949,#52950,#52951,
#52952,#52953,#52954,#52955,#52956,#52957,#52958,#52959,#52960,#52961,#52962,
#52963,#52964,#52965,#52966,#52967,#52968,#52969,#52970,#52971,#52972,#52973,
#52974,#52975,#52976,#52977,#52978,#52979,#52980,#52981,#52982,#52983,#52984,
#52985,#52986,#52987,#52988,#52989,#52990,#52991,#52992,#52993,#52994,#52995,
#52996,#52997,#52998,#52999,#53000,#53001,#53002,#53003,#53004,#53005,#53006,
#53007,#53008,#53009,#53010,#53011,#53012,#53013,#53014,#53015,#53016,#53017,
#53018,#53019,#53020,#53021,#53022,#53023,#53024,#53025,#53026,#53027,#53028,
#53029,#53030,#53031,#53032,#53033,#53034,#53035,#53036,#53037,#53038,#53039,
#53040,#53041,#53042,#53043,#53044,#53045,#53046,#53047,#53048,#53049,#53050,
#53051,#53052,#53053,#53054,#53055,#53056,#53057,#53058,#53059,#53060,#53061,
#53062,#53063,#53064,#53065,#53066,#53067,#53068,#53069,#53070,#53071,#53072,
#53073),.UNSPECIFIED.,.F.,.F.,(4,3,3,3,3,3,3,3,3,3,3,3,3,3,3,3,3,3,3,3,
3,3,3,3,3,3,3,3,3,3,3,3,3,3,3,3,3,3,3,3,3,3,3,3,3,3,3,3,3,3,3,3,3,3,3,3,
3,3,3,3,3,3,3,3,4),(151.887629070056,152.000026667646,152.112903200505,
152.226374334767,152.26552633122,152.366159628119,152.466648210403,152.567020725605,
152.667329882549,152.76760695334,152.867883169593,152.968259097634,153.068683666076,
153.169288719408,153.260725849725,153.361359137971,153.461847711597,153.562220218176,
153.662529366523,153.762806428752,153.863082636492,153.963458556155,154.063883116278,
154.16448816149,154.25592536823,154.35655866225,154.457047241589,154.557419753761,
154.657728907625,154.758005975291,154.858282188378,154.958658113213,155.05908267842,
155.159687728511,155.251124886735,155.351758201077,155.452246800884,155.552619333645,
155.652928508164,155.753205596519,155.853481830302,155.953857775697,156.054282361424,
156.154887431724,156.246324405239,156.34695765501,156.447446190172,156.54781865848,
156.64812776869,156.748404792969,156.848680962997,156.949056845581,157.049481368912,
157.150086378246,157.241523923744,157.341206650669,157.444907616414,157.544329788682,
157.643693026811,157.743029769444,157.842372418137,157.94181121822,158.041307175409,
158.140955160636,158.170814376628),.UNSPECIFIED.);
#1359=B_SPLINE_CURVE_WITH_KNOTS('',3,(#53075,#53076,#53077,#53078,#53079,
#53080,#53081,#53082,#53083,#53084,#53085,#53086,#53087,#53088,#53089,#53090,
#53091,#53092,#53093,#53094,#53095,#53096,#53097,#53098,#53099,#53100,#53101,
#53102,#53103,#53104,#53105,#53106,#53107,#53108,#53109,#53110,#53111,#53112,
#53113,#53114,#53115,#53116,#53117,#53118,#53119,#53120,#53121,#53122,#53123,
#53124,#53125,#53126,#53127,#53128,#53129,#53130,#53131,#53132,#53133,#53134,
#53135,#53136,#53137,#53138,#53139,#53140,#53141,#53142,#53143,#53144,#53145,
#53146,#53147,#53148,#53149,#53150,#53151,#53152,#53153,#53154,#53155,#53156,
#53157,#53158,#53159,#53160,#53161,#53162,#53163,#53164,#53165,#53166,#53167,
#53168,#53169,#53170,#53171,#53172,#53173,#53174,#53175,#53176,#53177,#53178,
#53179,#53180,#53181,#53182,#53183,#53184,#53185,#53186,#53187,#53188,#53189,
#53190,#53191,#53192,#53193,#53194,#53195,#53196,#53197,#53198,#53199,#53200,
#53201,#53202,#53203,#53204,#53205,#53206,#53207,#53208,#53209,#53210,#53211,
#53212,#53213,#53214,#53215,#53216,#53217,#53218,#53219,#53220,#53221,#53222,
#53223,#53224,#53225,#53226,#53227,#53228,#53229,#53230,#53231,#53232,#53233,
#53234,#53235,#53236,#53237,#53238,#53239,#53240,#53241,#53242,#53243,#53244,
#53245,#53246,#53247,#53248,#53249,#53250,#53251,#53252,#53253,#53254,#53255,
#53256,#53257,#53258,#53259,#53260,#53261,#53262,#53263,#53264),
 .UNSPECIFIED.,.F.,.F.,(4,3,3,3,3,3,3,3,3,3,3,3,3,3,3,3,3,3,3,3,3,3,3,3,
3,3,3,3,3,3,3,3,3,3,3,3,3,3,3,3,3,3,3,3,3,3,3,3,3,3,3,3,3,3,3,3,3,3,3,3,
3,3,3,4),(158.170814377013,158.236723442249,158.337356868079,158.437845580013,
158.53821822533,158.638527512613,158.738804713784,158.839081060277,158.939457117427,
159.039881814564,159.140486994388,159.231922960753,159.332555916466,159.433044157425,
159.533416332682,159.633725150674,159.734001883964,159.834277764629,159.934653362397,
160.03507760295,160.13568233623,160.227122479258,160.327755990604,160.428244784854,
160.528617507349,160.628926868655,160.729204140619,160.829480554602,160.929856673644,
161.030281429708,161.130886662821,161.222321997763,161.322956102713,161.423445498732,
161.523818832335,161.624128810136,161.724406703087,161.824683741651,161.92506048647,
162.025485869961,162.126091725867,162.217521516267,162.318152281655,162.418638329688,
162.519008318335,162.619314954555,162.719589513872,162.819863231331,162.920236697757,
163.020658821013,163.121261485342,163.212721034772,163.31335661715,163.413847469277,
163.51422222054,163.614533592008,163.714812852928,163.815091232034,163.915469265471,
164.015895911207,164.116502970526,164.207920553277,164.338551892289,164.453999601362),
 .UNSPECIFIED.);
#1360=B_SPLINE_CURVE_WITH_KNOTS('',3,(#53266,#53267,#53268,#53269,#53270,
#53271,#53272,#53273,#53274,#53275),.UNSPECIFIED.,.F.,.F.,(4,1,1,1,1,1,
1,4),(164.453999684193,165.203120071782,166.198319590286,167.193519108791,
168.188718627296,169.1839181458,170.179117664305,170.737184991372),
 .UNSPECIFIED.);
#1361=B_SPLINE_CURVE_WITH_KNOTS('',3,(#53277,#53278,#53279,#53280,#53281,
#53282,#53283,#53284,#53285,#53286,#53287,#53288,#53289,#53290,#53291,#53292),
 .UNSPECIFIED.,.F.,.F.,(4,3,3,3,3,4),(170.737185295228,170.846468267123,
170.955913585094,171.065828907702,171.17431718281,171.179694195601),
 .UNSPECIFIED.);
#1362=B_SPLINE_CURVE_WITH_KNOTS('',3,(#53298,#53299,#53300,#53301,#53302,
#53303,#53304,#53305,#53306,#53307,#53308,#53309,#53310,#53311,#53312,#53313,
#53314,#53315,#53316,#53317,#53318,#53319,#53320,#53321,#53322,#53323,#53324,
#53325,#53326,#53327,#53328,#53329,#53330,#53331,#53332,#53333,#53334,#53335,
#53336,#53337,#53338,#53339,#53340,#53341,#53342,#53343,#53344,#53345,#53346,
#53347,#53348,#53349,#53350,#53351,#53352,#53353,#53354,#53355,#53356,#53357,
#53358,#53359,#53360,#53361,#53362,#53363,#53364,#53365,#53366,#53367,#53368,
#53369,#53370,#53371,#53372,#53373,#53374,#53375,#53376,#53377,#53378,#53379,
#53380,#53381,#53382,#53383,#53384,#53385,#53386,#53387,#53388,#53389,#53390,
#53391,#53392,#53393,#53394,#53395,#53396,#53397,#53398,#53399,#53400,#53401,
#53402,#53403,#53404,#53405,#53406,#53407,#53408,#53409,#53410,#53411,#53412,
#53413,#53414,#53415,#53416,#53417,#53418,#53419,#53420,#53421,#53422,#53423,
#53424,#53425,#53426,#53427,#53428,#53429,#53430,#53431,#53432,#53433,#53434,
#53435,#53436,#53437,#53438,#53439,#53440,#53441,#53442,#53443,#53444,#53445,
#53446,#53447,#53448,#53449,#53450,#53451,#53452,#53453,#53454,#53455,#53456,
#53457,#53458,#53459,#53460,#53461,#53462,#53463,#53464,#53465,#53466,#53467,
#53468,#53469,#53470,#53471,#53472),.UNSPECIFIED.,.F.,.F.,(4,3,3,3,3,3,
3,3,3,3,3,3,3,3,3,3,3,3,3,3,3,3,3,3,3,3,3,3,3,3,3,3,3,3,3,3,3,3,3,3,3,3,
3,3,3,3,3,3,3,3,3,3,3,3,3,3,3,3,4),(-173.164716219819,-173.061774232127,
-172.958895354895,-172.856027311868,-172.753161388755,-172.650272247811,
-172.547334532095,-172.444243715141,-172.341071938644,-172.237700988273,
-172.169516701315,-172.069856695818,-171.970355940224,-171.870851095547,
-171.771557886023,-171.672305896722,-171.57306266092,-171.473376291392,
-171.373994982198,-171.274156082504,-171.17431718281,-171.073555542376,
-170.972938691585,-170.872438670844,-170.772002541256,-170.671599220397,
-170.57119766694,-170.470698748472,-170.370152283834,-170.2694286361,-170.179117664305,
-170.07831586765,-169.977655300651,-169.877106375297,-169.776618199067,
-169.676159756601,-169.575700070683,-169.475138660369,-169.374527217061,
-169.273735113921,-169.1839181458,-169.083409385862,-168.983047108886,-168.882802972129,
-168.782623399859,-168.682476941737,-168.582332189017,-168.482088152488,
-168.381795923466,-168.281322422809,-168.188718627296,-168.089497529044,
-167.990404250906,-167.891405724206,-167.792469004558,-167.693521041499,
-167.594574193245,-167.495518831768,-167.398250967225),.UNSPECIFIED.);
#1363=B_SPLINE_CURVE_WITH_KNOTS('',3,(#53474,#53475,#53476,#53477,#53478,
#53479,#53480,#53481,#53482,#53483,#53484,#53485,#53486,#53487,#53488,#53489,
#53490,#53491,#53492,#53493,#53494,#53495,#53496,#53497,#53498,#53499,#53500,
#53501,#53502,#53503,#53504,#53505,#53506,#53507,#53508,#53509,#53510,#53511,
#53512,#53513,#53514,#53515,#53516,#53517,#53518,#53519,#53520,#53521,#53522,
#53523,#53524,#53525,#53526,#53527,#53528,#53529,#53530,#53531,#53532,#53533,
#53534,#53535,#53536,#53537,#53538,#53539,#53540,#53541,#53542,#53543,#53544,
#53545,#53546,#53547,#53548,#53549,#53550,#53551,#53552,#53553,#53554,#53555,
#53556,#53557,#53558,#53559,#53560,#53561,#53562,#53563,#53564,#53565,#53566,
#53567,#53568,#53569,#53570,#53571,#53572,#53573,#53574,#53575,#53576,#53577,
#53578,#53579,#53580,#53581,#53582,#53583,#53584,#53585,#53586,#53587,#53588,
#53589,#53590,#53591,#53592,#53593,#53594,#53595,#53596,#53597,#53598,#53599,
#53600,#53601,#53602,#53603,#53604,#53605,#53606,#53607,#53608,#53609,#53610,
#53611,#53612,#53613,#53614,#53615,#53616,#53617,#53618,#53619,#53620,#53621,
#53622,#53623,#53624,#53625,#53626,#53627,#53628,#53629,#53630,#53631,#53632,
#53633,#53634,#53635,#53636,#53637,#53638,#53639,#53640,#53641,#53642,#53643,
#53644,#53645,#53646,#53647,#53648,#53649,#53650,#53651,#53652,#53653,#53654,
#53655,#53656,#53657,#53658,#53659,#53660,#53661,#53662,#53663),
 .UNSPECIFIED.,.F.,.F.,(4,3,3,3,3,3,3,3,3,3,3,3,3,3,3,3,3,3,3,3,3,3,3,3,
3,3,3,3,3,3,3,3,3,3,3,3,3,3,3,3,3,3,3,3,3,3,3,3,3,3,3,3,3,3,3,3,3,3,3,3,
3,3,3,4),(-167.398250966954,-167.256843477477,-167.193519108791,-167.092866771413,
-166.992358726914,-166.891966205152,-166.791636719264,-166.691339025476,
-166.591041920208,-166.490644829191,-166.390198914085,-166.289572451256,
-166.198319590286,-166.097703708367,-165.997232803737,-165.896878278283,
-165.796587292888,-165.696328550035,-165.596070792856,-165.495713401586,
-165.395307442073,-165.294720902516,-165.203120071782,-165.102482061844,
-165.001988730649,-164.901611435422,-164.801297481778,-164.701015604418,
-164.600734578522,-164.50035386993,-164.399924529254,-164.299314773851,
-164.207920553277,-164.10728527015,-164.006794651673,-163.906420034439,
-163.806108736309,-163.705829488141,-163.605551061247,-163.505172885449,
-163.404746045344,-163.304138706214,-163.212721034772,-163.112090114221,
-163.011603945902,-162.911233889915,-162.810927218609,-162.710652656398,
-162.610378968209,-162.51000558127,-162.409583565122,-162.308981053238,
-162.217521516268,-162.116887418798,-162.016398028124,-161.916024696634,
-161.815714718978,-161.71543682421,-161.615159781871,-161.514783030236,
-161.414357638253,-161.313751771128,-161.222321997763,-161.115065659774),
 .UNSPECIFIED.);
#1364=B_SPLINE_CURVE_WITH_KNOTS('',3,(#53665,#53666,#53667,#53668,#53669,
#53670,#53671,#53672,#53673,#53674,#53675,#53676,#53677,#53678,#53679,#53680,
#53681,#53682,#53683,#53684,#53685,#53686,#53687,#53688,#53689,#53690,#53691,
#53692,#53693,#53694,#53695,#53696,#53697,#53698,#53699,#53700,#53701,#53702,
#53703,#53704,#53705,#53706,#53707,#53708,#53709,#53710,#53711,#53712,#53713,
#53714,#53715,#53716,#53717,#53718,#53719,#53720,#53721,#53722,#53723,#53724,
#53725,#53726,#53727,#53728,#53729,#53730,#53731,#53732,#53733,#53734,#53735,
#53736,#53737,#53738,#53739,#53740,#53741,#53742,#53743,#53744,#53745,#53746,
#53747,#53748,#53749,#53750,#53751,#53752,#53753,#53754,#53755,#53756,#53757,
#53758,#53759,#53760,#53761,#53762,#53763,#53764,#53765,#53766,#53767,#53768,
#53769,#53770,#53771,#53772,#53773,#53774,#53775,#53776,#53777,#53778,#53779,
#53780,#53781,#53782,#53783,#53784,#53785,#53786,#53787,#53788,#53789,#53790,
#53791,#53792,#53793,#53794,#53795,#53796,#53797,#53798,#53799,#53800,#53801,
#53802,#53803,#53804,#53805,#53806,#53807,#53808,#53809,#53810,#53811,#53812,
#53813,#53814,#53815,#53816,#53817,#53818,#53819,#53820,#53821,#53822,#53823,
#53824,#53825,#53826,#53827,#53828,#53829,#53830,#53831,#53832,#53833,#53834,
#53835,#53836,#53837,#53838,#53839,#53840,#53841,#53842,#53843,#53844,#53845,
#53846,#53847,#53848,#53849,#53850,#53851,#53852,#53853,#53854),
 .UNSPECIFIED.,.F.,.F.,(4,3,3,3,3,3,3,3,3,3,3,3,3,3,3,3,3,3,3,3,3,3,3,3,
3,3,3,3,3,3,3,3,3,3,3,3,3,3,3,3,3,3,3,3,3,3,3,3,3,3,3,3,3,3,3,3,3,3,3,3,
3,3,3,4),(-161.115065659554,-161.015800200422,-160.916674940153,-160.817627264428,
-160.718624347641,-160.619633423009,-160.520554010525,-160.421433091436,
-160.322134850872,-160.227122479258,-160.12648950089,-160.02600124239,-159.925629057356,
-159.825320234315,-159.725043500696,-159.624767624419,-159.524392038399,
-159.423967813645,-159.323363102809,-159.231922960753,-159.131289537792,
-159.030800828007,-158.93042818375,-158.830118896863,-158.729841695426,
-158.629565348006,-158.529189288898,-158.428764589237,-158.328159405962,
-158.236723442249,-158.136090136973,-158.03560154574,-157.935229020767,
-157.834919853554,-157.734642772011,-157.634366544534,-157.533990604604,
-157.43356602389,-157.332960957774,-157.241523923744,-157.14089067075,-157.040402133095,
-156.940029663402,-156.839720552481,-156.739443528165,-156.639167358773,
-156.538791477875,-156.438366956807,-156.337761950686,-156.246324405239,
-156.145691091532,-156.045202492206,-155.94482995969,-155.844520785274,
-155.744243696879,-155.643967462913,-155.543591517113,-155.443166930859,
-155.342561859832,-155.251124886735,-155.140971132557,-155.031115086589,
-154.921757951068,-154.83188035295),.UNSPECIFIED.);
#1365=B_SPLINE_CURVE_WITH_KNOTS('',3,(#53856,#53857,#53858,#53859,#53860,
#53861,#53862,#53863,#53864,#53865,#53866,#53867,#53868,#53869,#53870,#53871,
#53872,#53873,#53874,#53875,#53876,#53877,#53878,#53879,#53880,#53881,#53882,
#53883,#53884,#53885,#53886,#53887,#53888,#53889,#53890,#53891,#53892,#53893,
#53894,#53895,#53896,#53897,#53898,#53899,#53900,#53901,#53902,#53903,#53904,
#53905,#53906,#53907,#53908,#53909,#53910,#53911,#53912,#53913,#53914,#53915,
#53916,#53917,#53918,#53919,#53920,#53921,#53922,#53923,#53924,#53925,#53926,
#53927,#53928,#53929,#53930,#53931,#53932,#53933,#53934,#53935,#53936,#53937,
#53938,#53939,#53940,#53941,#53942,#53943,#53944,#53945,#53946,#53947,#53948,
#53949,#53950,#53951,#53952,#53953,#53954,#53955,#53956,#53957,#53958,#53959,
#53960,#53961,#53962,#53963,#53964,#53965,#53966,#53967,#53968,#53969,#53970,
#53971,#53972,#53973,#53974,#53975,#53976,#53977,#53978,#53979,#53980,#53981,
#53982,#53983,#53984,#53985,#53986,#53987,#53988,#53989,#53990,#53991,#53992,
#53993,#53994,#53995,#53996,#53997,#53998,#53999,#54000,#54001,#54002,#54003,
#54004,#54005,#54006,#54007,#54008,#54009,#54010,#54011,#54012,#54013,#54014,
#54015,#54016,#54017,#54018,#54019,#54020,#54021,#54022,#54023,#54024,#54025,
#54026,#54027,#54028,#54029,#54030,#54031,#54032,#54033,#54034,#54035,#54036,
#54037,#54038,#54039,#54040,#54041,#54042,#54043,#54044,#54045,#54046,#54047,
#54048),.UNSPECIFIED.,.F.,.F.,(4,3,3,3,3,3,3,3,3,3,3,3,3,3,3,3,3,3,3,3,
3,3,3,3,3,3,3,3,3,3,3,3,3,3,3,3,3,3,3,3,3,3,3,3,3,3,3,3,3,3,3,3,3,3,3,3,
3,3,3,3,3,3,3,3,4),(-154.831880352595,-154.729682229563,-154.627429231303,
-154.525011782519,-154.422505655058,-154.319788821663,-154.25592536823,
-154.155292079537,-154.054803505564,-153.954430998793,-153.854121850349,
-153.753844788115,-153.653568580465,-153.553192661038,-153.452768101231,
-153.352163056466,-153.260725849725,-153.160092552944,-153.059603970749,
-152.959231455593,-152.858922298669,-152.758645227872,-152.658369011587,
-152.557993083472,-152.457568514935,-152.356963461469,-152.26552633122,
-152.164893037697,-152.064404458798,-151.964031946975,-151.863722793407,
-151.763445725983,-151.663169513082,-151.562793588349,-151.462369023196,
-151.361763973081,-151.270326812716,-151.169693519517,-151.069204940955,
-150.968832429493,-150.868523276298,-150.768246209259,-150.667969996757,
-150.567594072437,-150.467169507708,-150.366564458028,-150.275127294211,
-150.174493999962,-150.074005420332,-149.97363290778,-149.873323753481,
-149.773046685327,-149.672770471699,-149.572394546247,-149.471969980378,
-149.371364929561,-149.279927775706,-149.180333143564,-149.080870560533,
-148.981507319459,-148.882210835513,-148.782924030068,-148.683642355602,
-148.584295310261,-148.548695045415),.UNSPECIFIED.);
#1366=B_SPLINE_CURVE_WITH_KNOTS('',3,(#54050,#54051,#54052,#54053,#54054,
#54055,#54056,#54057,#54058,#54059,#54060,#54061,#54062,#54063,#54064,#54065,
#54066,#54067,#54068,#54069,#54070,#54071,#54072,#54073,#54074,#54075,#54076,
#54077,#54078,#54079,#54080,#54081,#54082,#54083,#54084,#54085,#54086,#54087,
#54088,#54089,#54090,#54091,#54092,#54093,#54094,#54095,#54096,#54097,#54098,
#54099,#54100,#54101,#54102,#54103,#54104,#54105,#54106,#54107,#54108,#54109,
#54110,#54111,#54112,#54113,#54114,#54115,#54116,#54117,#54118,#54119,#54120,
#54121,#54122,#54123,#54124,#54125,#54126,#54127,#54128,#54129,#54130,#54131,
#54132,#54133,#54134,#54135,#54136,#54137,#54138,#54139,#54140,#54141,#54142,
#54143,#54144,#54145,#54146,#54147,#54148,#54149,#54150,#54151,#54152,#54153,
#54154,#54155,#54156,#54157,#54158,#54159,#54160,#54161,#54162,#54163,#54164,
#54165,#54166,#54167,#54168,#54169,#54170,#54171,#54172,#54173,#54174,#54175,
#54176,#54177,#54178,#54179,#54180,#54181,#54182,#54183,#54184,#54185,#54186,
#54187,#54188,#54189,#54190,#54191,#54192,#54193,#54194,#54195,#54196,#54197,
#54198,#54199,#54200,#54201,#54202,#54203,#54204,#54205,#54206,#54207,#54208,
#54209,#54210,#54211,#54212,#54213,#54214,#54215,#54216,#54217,#54218,#54219,
#54220,#54221,#54222,#54223,#54224,#54225,#54226,#54227,#54228,#54229,#54230,
#54231,#54232,#54233,#54234,#54235,#54236,#54237,#54238,#54239),
 .UNSPECIFIED.,.F.,.F.,(4,3,3,3,3,3,3,3,3,3,3,3,3,3,3,3,3,3,3,3,3,3,3,3,
3,3,3,3,3,3,3,3,3,3,3,3,3,3,3,3,3,3,3,3,3,3,3,3,3,3,3,3,3,3,3,3,3,3,3,3,
3,3,3,4),(-148.548695045061,-148.416711651131,-148.284728257202,-148.184094963453,
-148.083606384331,-147.983233872294,-147.882924718517,-147.782647650889,
-147.682371437791,-147.58199551287,-147.481570947536,-147.38096589725,-147.289528738697,
-147.188895444816,-147.08840686556,-146.988034353387,-146.887725199471,
-146.787448131702,-146.687171918462,-146.586795993399,-146.48637142792,
-146.385766377491,-146.294329220192,-146.193695926386,-146.093207347206,
-145.99283483511,-145.892525681272,-145.792248613582,-145.691972400421,
-145.591596475436,-145.491171910037,-145.390566859687,-145.299129701687,
-145.198496407874,-145.098007828688,-144.997635316585,-144.89732616274,
-144.797049095044,-144.696772881877,-144.596396956886,-144.495972391481,
-144.395367341125,-144.303930183183,-144.203296889354,-144.102808310151,
-144.002435798032,-143.902126644169,-143.801849576456,-143.701573363271,
-143.601197438263,-143.50077287284,-143.400167822466,-143.308730664678,
-143.20809737086,-143.107608791668,-143.007236279559,-142.906927125708,
-142.806650058006,-142.706373844833,-142.605997919835,-142.505573354424,
-142.404968304061,-142.313531146173,-142.265509738235),.UNSPECIFIED.);
#1367=B_SPLINE_CURVE_WITH_KNOTS('',3,(#54241,#54242,#54243,#54244,#54245,
#54246,#54247,#54248,#54249,#54250,#54251,#54252,#54253,#54254,#54255,#54256,
#54257,#54258,#54259,#54260,#54261,#54262,#54263,#54264,#54265,#54266,#54267,
#54268,#54269,#54270,#54271,#54272,#54273,#54274,#54275,#54276,#54277,#54278,
#54279,#54280,#54281,#54282,#54283,#54284,#54285,#54286,#54287,#54288,#54289,
#54290,#54291,#54292,#54293,#54294,#54295,#54296,#54297,#54298,#54299,#54300,
#54301,#54302,#54303,#54304,#54305,#54306,#54307,#54308,#54309,#54310,#54311,
#54312,#54313,#54314,#54315,#54316,#54317,#54318,#54319,#54320,#54321,#54322,
#54323,#54324,#54325,#54326,#54327,#54328,#54329,#54330,#54331,#54332,#54333,
#54334,#54335,#54336,#54337,#54338,#54339,#54340,#54341,#54342,#54343,#54344,
#54345,#54346,#54347,#54348,#54349,#54350,#54351,#54352,#54353,#54354,#54355,
#54356,#54357,#54358,#54359,#54360,#54361,#54362,#54363,#54364,#54365,#54366,
#54367,#54368,#54369,#54370,#54371,#54372,#54373,#54374,#54375,#54376,#54377,
#54378,#54379,#54380,#54381,#54382,#54383,#54384,#54385,#54386,#54387,#54388,
#54389,#54390,#54391,#54392,#54393,#54394,#54395,#54396,#54397,#54398,#54399,
#54400,#54401,#54402,#54403,#54404,#54405,#54406,#54407,#54408,#54409,#54410,
#54411,#54412,#54413,#54414,#54415,#54416,#54417,#54418,#54419,#54420,#54421,
#54422,#54423,#54424,#54425,#54426,#54427,#54428,#54429,#54430,#54431,#54432,
#54433),.UNSPECIFIED.,.F.,.F.,(4,3,3,3,3,3,3,3,3,3,3,3,3,3,3,3,3,3,3,3,
3,3,3,3,3,3,3,3,3,3,3,3,3,3,3,3,3,3,3,3,3,3,3,3,3,3,3,3,3,3,3,3,3,3,3,3,
3,3,3,3,3,3,3,3,4),(-142.265509737928,-142.165633574489,-142.065897851332,
-141.966270709277,-141.866701131734,-141.767156909997,-141.667605870528,
-141.567952330949,-141.468241472944,-141.368364768051,-141.318331627669,
-141.217698333847,-141.117209754651,-141.016837242539,-140.916528088684,
-140.816251020978,-140.715974807801,-140.6155988828,-140.515174317384,-140.414569267018,
-140.323132109164,-140.222498815344,-140.122010236149,-140.021637724038,
-139.921328570185,-139.821051502481,-139.720775289305,-139.620399364306,
-139.519974798892,-139.419369748527,-139.327932590659,-139.227299296839,
-139.126810717644,-139.026438205534,-138.926129051681,-138.825851983977,
-138.725575770801,-138.625199845802,-138.524775280388,-138.424170230023,
-138.332733072155,-138.232099778334,-138.131611199139,-138.031238687028,
-137.930929533175,-137.83065246547,-137.730376252294,-137.630000327294,
-137.52957576188,-137.428970711514,-137.33753355365,-137.236900259829,-137.136411680635,
-137.036039168524,-136.93573001467,-136.835452946965,-136.735176733789,
-136.634800808789,-136.534376243375,-136.433771193009,-136.342334035145,
-136.227285324675,-136.112723200038,-135.998976348791,-135.982324431284),
 .UNSPECIFIED.);
#1368=B_SPLINE_CURVE_WITH_KNOTS('',3,(#54435,#54436,#54437,#54438,#54439,
#54440,#54441,#54442,#54443,#54444,#54445,#54446,#54447,#54448,#54449,#54450,
#54451,#54452,#54453,#54454,#54455,#54456,#54457,#54458,#54459,#54460,#54461,
#54462,#54463,#54464,#54465,#54466,#54467,#54468,#54469,#54470,#54471,#54472,
#54473,#54474,#54475,#54476,#54477,#54478,#54479,#54480,#54481,#54482,#54483,
#54484,#54485,#54486,#54487,#54488,#54489,#54490,#54491,#54492,#54493,#54494,
#54495,#54496,#54497,#54498,#54499,#54500,#54501,#54502,#54503,#54504,#54505,
#54506,#54507,#54508,#54509,#54510,#54511,#54512,#54513,#54514,#54515,#54516,
#54517,#54518,#54519,#54520,#54521,#54522,#54523,#54524,#54525,#54526,#54527,
#54528,#54529,#54530,#54531,#54532,#54533,#54534,#54535,#54536,#54537,#54538,
#54539,#54540,#54541,#54542,#54543,#54544,#54545,#54546,#54547,#54548,#54549,
#54550,#54551,#54552,#54553,#54554,#54555,#54556,#54557,#54558,#54559,#54560,
#54561,#54562,#54563,#54564,#54565,#54566,#54567,#54568,#54569,#54570,#54571,
#54572,#54573,#54574,#54575,#54576,#54577,#54578,#54579,#54580,#54581,#54582,
#54583,#54584,#54585,#54586,#54587,#54588,#54589,#54590,#54591,#54592,#54593,
#54594,#54595,#54596,#54597,#54598,#54599,#54600,#54601,#54602,#54603,#54604,
#54605,#54606,#54607,#54608,#54609,#54610,#54611,#54612,#54613,#54614,#54615,
#54616,#54617,#54618,#54619,#54620,#54621,#54622,#54623,#54624,#54625,#54626,
#54627),.UNSPECIFIED.,.F.,.F.,(4,3,3,3,3,3,3,3,3,3,3,3,3,3,3,3,3,3,3,3,
3,3,3,3,3,3,3,3,3,3,3,3,3,3,3,3,3,3,3,3,3,3,3,3,3,3,3,3,3,3,3,3,3,3,3,3,
3,3,3,3,3,3,3,3,4),(-135.982324431056,-135.881583024083,-135.780838722731,
-135.680061277593,-135.579153091099,-135.478167949569,-135.377006907812,
-135.34713451664,-135.24650122282,-135.146012643626,-135.045640131515,-134.945330977662,
-134.845053909958,-134.744777696782,-134.644401771783,-134.543977206369,
-134.443372156005,-134.351934998136,-134.251301704315,-134.150813125121,
-134.05044061301,-133.950131459156,-133.849854391452,-133.749578178276,
-133.649202253276,-133.548777687862,-133.448172637497,-133.356735479631,
-133.25610218581,-133.155613606615,-133.055241094504,-132.95493194065,-132.854654872945,
-132.754378659769,-132.654002734769,-132.553578169354,-132.452973118989,
-132.361535961126,-132.260902667306,-132.160414088112,-132.060041576001,
-131.959732422148,-131.859455354444,-131.759179141268,-131.658803216269,
-131.558378650855,-131.45777360049,-131.366336442622,-131.265703148802,
-131.165214569607,-131.064842057496,-130.964532903643,-130.864255835938,
-130.763979622762,-130.663603697762,-130.563179132348,-130.462574081983,
-130.371136924117,-130.270722015059,-130.170446946524,-130.07028000736,
-129.970182457444,-129.870127451158,-129.770050097071,-129.699139123876),
 .UNSPECIFIED.);
#1369=B_SPLINE_CURVE_WITH_KNOTS('',3,(#54629,#54630,#54631,#54632,#54633,
#54634,#54635,#54636,#54637,#54638,#54639,#54640,#54641,#54642,#54643,#54644,
#54645,#54646,#54647,#54648,#54649,#54650,#54651,#54652,#54653,#54654,#54655,
#54656,#54657,#54658,#54659,#54660,#54661,#54662,#54663,#54664,#54665,#54666,
#54667,#54668,#54669,#54670,#54671,#54672,#54673,#54674,#54675,#54676,#54677,
#54678,#54679,#54680,#54681,#54682,#54683,#54684,#54685,#54686,#54687,#54688,
#54689,#54690,#54691,#54692,#54693,#54694,#54695,#54696,#54697,#54698,#54699,
#54700,#54701,#54702,#54703,#54704,#54705,#54706,#54707,#54708,#54709,#54710,
#54711,#54712,#54713,#54714,#54715,#54716,#54717,#54718,#54719,#54720,#54721,
#54722,#54723,#54724,#54725,#54726,#54727,#54728,#54729,#54730,#54731,#54732,
#54733,#54734,#54735,#54736,#54737,#54738,#54739,#54740,#54741,#54742,#54743,
#54744,#54745,#54746,#54747,#54748,#54749,#54750,#54751,#54752,#54753,#54754,
#54755,#54756,#54757,#54758,#54759,#54760,#54761,#54762,#54763,#54764,#54765,
#54766,#54767,#54768,#54769,#54770,#54771,#54772,#54773,#54774,#54775,#54776,
#54777,#54778,#54779,#54780,#54781,#54782,#54783,#54784,#54785,#54786,#54787,
#54788,#54789,#54790,#54791,#54792,#54793,#54794,#54795,#54796,#54797,#54798,
#54799,#54800,#54801,#54802,#54803,#54804,#54805,#54806,#54807,#54808,#54809,
#54810,#54811,#54812,#54813,#54814,#54815,#54816,#54817,#54818),
 .UNSPECIFIED.,.F.,.F.,(4,3,3,3,3,3,3,3,3,3,3,3,3,3,3,3,3,3,3,3,3,3,3,3,
3,3,3,3,3,3,3,3,3,3,3,3,3,3,3,3,3,3,3,3,3,3,3,3,3,3,3,3,3,3,3,3,3,3,3,3,
3,3,3,4),(-129.69913912347,-129.581509782298,-129.462588504636,-129.375937405612,
-129.275304111791,-129.174815532596,-129.074443020485,-128.974133866631,
-128.873856798926,-128.77358058575,-128.67320466075,-128.572780095335,-128.47217504497,
-128.380737887107,-128.280104593287,-128.179616014092,-128.079243501981,
-127.978934348128,-127.878657280424,-127.778381067248,-127.678005142249,
-127.577580576835,-127.47697552647,-127.385538368603,-127.284905074783,
-127.184416495588,-127.084043983477,-126.983734829624,-126.883457761919,
-126.783181548743,-126.682805623744,-126.58238105833,-126.481776007964,
-126.390338850098,-126.289705556277,-126.189216977082,-126.088844464971,
-125.988535311117,-125.888258243412,-125.787982030236,-125.687606105236,
-125.587181539821,-125.486576489456,-125.395139331593,-125.294506037773,
-125.194017458578,-125.093644946467,-124.993335792614,-124.89305872491,
-124.792782511734,-124.692406586735,-124.591982021321,-124.491376970956,
-124.399939813089,-124.299503686858,-124.199212133855,-124.099036003752,
-123.998922538952,-123.898840194359,-123.798757464703,-123.698574952104,
-123.598342156662,-123.497932620793,-123.415953817054),.UNSPECIFIED.);
#1370=B_SPLINE_CURVE_WITH_KNOTS('',3,(#54820,#54821,#54822,#54823,#54824,
#54825,#54826,#54827,#54828,#54829,#54830,#54831,#54832,#54833,#54834,#54835,
#54836,#54837,#54838,#54839,#54840,#54841,#54842,#54843,#54844,#54845,#54846,
#54847,#54848,#54849,#54850,#54851,#54852,#54853,#54854,#54855,#54856,#54857,
#54858,#54859,#54860,#54861,#54862,#54863,#54864,#54865,#54866,#54867,#54868,
#54869,#54870,#54871,#54872,#54873,#54874,#54875,#54876,#54877,#54878,#54879,
#54880,#54881,#54882,#54883,#54884,#54885,#54886,#54887,#54888,#54889,#54890,
#54891,#54892,#54893,#54894,#54895,#54896,#54897,#54898,#54899,#54900,#54901,
#54902,#54903,#54904,#54905,#54906,#54907,#54908,#54909,#54910,#54911,#54912,
#54913,#54914,#54915,#54916,#54917,#54918,#54919,#54920,#54921,#54922,#54923,
#54924,#54925,#54926,#54927,#54928,#54929,#54930,#54931,#54932,#54933,#54934,
#54935,#54936,#54937,#54938,#54939,#54940,#54941,#54942,#54943,#54944,#54945,
#54946,#54947,#54948,#54949,#54950,#54951,#54952,#54953,#54954,#54955,#54956,
#54957,#54958,#54959,#54960,#54961,#54962,#54963,#54964,#54965,#54966,#54967,
#54968,#54969,#54970,#54971,#54972,#54973,#54974,#54975,#54976,#54977,#54978,
#54979,#54980,#54981,#54982,#54983,#54984,#54985,#54986,#54987,#54988,#54989,
#54990,#54991,#54992,#54993,#54994,#54995,#54996,#54997,#54998,#54999,#55000,
#55001,#55002,#55003,#55004,#55005,#55006,#55007,#55008,#55009,#55010,#55011,
#55012),.UNSPECIFIED.,.F.,.F.,(4,3,3,3,3,3,3,3,3,3,3,3,3,3,3,3,3,3,3,3,
3,3,3,3,3,3,3,3,3,3,3,3,3,3,3,3,3,3,3,3,3,3,3,3,3,3,3,3,3,3,3,3,3,3,3,3,
3,3,3,3,3,3,3,3,4),(-123.415953816697,-123.404740294584,-123.304107000763,
-123.203618421569,-123.103245909458,-123.002936755605,-122.9026596879,-122.802383474724,
-122.702007549724,-122.60158298431,-122.500977933945,-122.409540776079,
-122.308907482258,-122.208418903063,-122.108046390952,-122.007737237099,
-121.907460169394,-121.807183956218,-121.706808031218,-121.606383465803,
-121.505778415438,-121.414341257574,-121.313707963754,-121.213219384559,
-121.112846872449,-121.012537718596,-120.912260650891,-120.811984437715,
-120.711608512716,-120.611183947302,-120.510578896937,-120.41914173907,
-120.318508445249,-120.218019866055,-120.117647353944,-120.01733820009,
-119.917061132386,-119.81678491921,-119.71640899421,-119.615984428796,-119.515379378431,
-119.423942220565,-119.323308926744,-119.222820347549,-119.122447835438,
-119.022138681584,-118.921861613879,-118.821585400703,-118.721209475703,
-118.620784910289,-118.520179859923,-118.42874270206,-118.32810940824,-118.227620829045,
-118.127248316935,-118.026939163082,-117.926662095377,-117.826385882202,
-117.726009957202,-117.625585391788,-117.524980341423,-117.433543183556,
-117.31144553275,-117.190918574851,-117.132768509857),.UNSPECIFIED.);
#1371=B_SPLINE_CURVE_WITH_KNOTS('',3,(#55014,#55015,#55016,#55017,#55018,
#55019,#55020,#55021,#55022,#55023,#55024,#55025,#55026,#55027,#55028,#55029,
#55030,#55031,#55032,#55033,#55034,#55035,#55036,#55037,#55038,#55039,#55040,
#55041,#55042,#55043,#55044,#55045,#55046,#55047,#55048,#55049,#55050,#55051,
#55052,#55053,#55054,#55055,#55056,#55057,#55058,#55059,#55060,#55061,#55062,
#55063,#55064,#55065,#55066,#55067,#55068,#55069,#55070,#55071,#55072,#55073,
#55074,#55075,#55076,#55077,#55078,#55079,#55080,#55081,#55082,#55083,#55084,
#55085,#55086,#55087,#55088,#55089,#55090,#55091,#55092,#55093,#55094,#55095,
#55096,#55097,#55098,#55099,#55100,#55101,#55102,#55103,#55104,#55105,#55106,
#55107,#55108,#55109,#55110,#55111,#55112,#55113,#55114,#55115,#55116,#55117,
#55118,#55119,#55120,#55121,#55122,#55123,#55124,#55125,#55126,#55127,#55128,
#55129,#55130,#55131,#55132,#55133,#55134,#55135,#55136,#55137,#55138,#55139,
#55140,#55141,#55142,#55143,#55144,#55145,#55146,#55147,#55148,#55149,#55150,
#55151,#55152,#55153,#55154,#55155,#55156,#55157,#55158,#55159,#55160,#55161,
#55162,#55163,#55164,#55165,#55166,#55167,#55168,#55169,#55170,#55171,#55172,
#55173,#55174,#55175,#55176,#55177,#55178,#55179,#55180,#55181,#55182,#55183,
#55184,#55185,#55186,#55187,#55188,#55189,#55190,#55191,#55192,#55193,#55194,
#55195,#55196,#55197,#55198,#55199,#55200,#55201,#55202,#55203),
 .UNSPECIFIED.,.F.,.F.,(4,3,3,3,3,3,3,3,3,3,3,3,3,3,3,3,3,3,3,3,3,3,3,3,
3,3,3,3,3,3,3,3,3,3,3,3,3,3,3,3,3,3,3,3,3,3,3,3,3,3,3,3,3,3,3,3,3,3,3,3,
3,3,3,4),(-117.132768509517,-117.033015063478,-116.933296664845,-116.833581387141,
-116.733766480766,-116.633903776678,-116.533856241353,-116.438343665051,
-116.337710371231,-116.237221792036,-116.136849279925,-116.036540126071,
-115.936263058367,-115.835986845191,-115.735610920191,-115.635186354777,
-115.534581304412,-115.443144146546,-115.342510852725,-115.24202227353,
-115.141649761419,-115.041340607566,-114.941063539861,-114.840787326685,
-114.740411401685,-114.63998683627,-114.539381785905,-114.447944628041,
-114.347311334221,-114.246822755026,-114.146450242915,-114.046141089062,
-113.945864021358,-113.845587808182,-113.745211883183,-113.644787317769,
-113.544182267404,-113.452745109537,-113.352111815717,-113.251623236522,
-113.151250724411,-113.050941570557,-112.950664502853,-112.850388289677,
-112.750012364677,-112.649587799263,-112.548982748898,-112.457545591032,
-112.356912297211,-112.256423718016,-112.156051205905,-112.055742052052,
-111.955464984347,-111.855188771171,-111.754812846171,-111.654388280757,
-111.553783230392,-111.462346072527,-111.360662607761,-111.259132552871,
-111.156745215238,-111.055443771602,-110.95251348697,-110.849583202337),
 .UNSPECIFIED.);
#1372=B_SPLINE_CURVE_WITH_KNOTS('',3,(#55205,#55206,#55207,#55208,#55209,
#55210,#55211,#55212,#55213,#55214),.UNSPECIFIED.,.F.,.F.,(4,1,1,1,1,1,
1,4),(-110.849576038581,-110.467146554023,-109.471947035518,-108.476747517013,
-107.481547998509,-106.486348480004,-105.491148961499,-104.566397895158),
 .UNSPECIFIED.);
#1373=B_SPLINE_CURVE_WITH_KNOTS('',3,(#55216,#55217,#55218,#55219,#55220,
#55221,#55222,#55223,#55224,#55225,#55226),.UNSPECIFIED.,.F.,.F.,(4,1,1,
1,1,1,1,1,4),(-104.566397895158,-104.495949442994,-103.50074992449,-102.505550405985,
-101.51035088748,-100.515151368976,-99.5199518504709,-98.5247523319661,
-98.2832125879783),.UNSPECIFIED.);
#1374=B_SPLINE_CURVE_WITH_KNOTS('',3,(#55228,#55229,#55230,#55231,#55232,
#55233,#55234,#55235,#55236,#55237),.UNSPECIFIED.,.F.,.F.,(4,1,1,1,1,1,
1,4),(-98.2832125879783,-97.5295528134614,-96.5343532949567,-95.539153776452,
-94.5439542579473,-93.5487547394426,-92.5535552209379,-92.0000272807987),
 .UNSPECIFIED.);
#1375=B_SPLINE_CURVE_WITH_KNOTS('',3,(#55239,#55240,#55241,#55242,#55243,
#55244,#55245,#55246,#55247,#55248),.UNSPECIFIED.,.F.,.F.,(4,1,1,1,1,1,
1,4),(-92.0000272807987,-91.5583557024332,-90.5631561839285,-89.5679566654238,
-88.5727571469191,-87.5775576284143,-86.5823581099096,-85.7168419736191),
 .UNSPECIFIED.);
#1376=B_SPLINE_CURVE_WITH_KNOTS('',3,(#55250,#55251,#55252,#55253,#55254,
#55255,#55256,#55257,#55258,#55259,#55260),.UNSPECIFIED.,.F.,.F.,(4,1,1,
1,1,1,1,1,4),(-85.7168419736191,-85.5871585914049,-84.5919590729002,-83.5967595543955,
-82.6015600358908,-81.6063605173861,-80.6111609988814,-79.6159614803767,
-79.4336566664395),.UNSPECIFIED.);
#1377=B_SPLINE_CURVE_WITH_KNOTS('',3,(#55262,#55263,#55264,#55265,#55266,
#55267,#55268,#55269,#55270,#55271),.UNSPECIFIED.,.F.,.F.,(4,1,1,1,1,1,
1,4),(-79.4336566664395,-78.620761961872,-77.6255624433673,-76.6303629248626,
-75.6351634063578,-74.6399638878531,-73.6447643693484,-73.1504713592599),
 .UNSPECIFIED.);
#1378=B_SPLINE_CURVE_WITH_KNOTS('',3,(#55273,#55274,#55275,#55276,#55277,
#55278,#55279,#55280,#55281,#55282),.UNSPECIFIED.,.F.,.F.,(4,1,1,1,1,1,
1,4),(-73.1504713592599,-72.6495648508437,-71.654365332339,-70.6591658138343,
-69.6639662953296,-68.6687667768249,-67.6735672583202,-66.8672860520803),
 .UNSPECIFIED.);
#1379=B_SPLINE_CURVE_WITH_KNOTS('',3,(#55284,#55285,#55286,#55287,#55288,
#55289,#55290,#55291,#55292,#55293,#55294),.UNSPECIFIED.,.F.,.F.,(4,1,1,
1,1,1,1,1,4),(-66.8672860520803,-66.6783677398155,-65.6831682213108,-64.6879687028061,
-63.6927691843014,-62.6975696657967,-61.7023701472919,-60.7071706287872,
-60.5841007449007),.UNSPECIFIED.);
#1380=B_SPLINE_CURVE_WITH_KNOTS('',3,(#55296,#55297,#55298,#55299,#55300,
#55301,#55302,#55303,#55304,#55305),.UNSPECIFIED.,.F.,.F.,(4,1,1,1,1,1,
1,4),(-60.5841007449007,-59.7119711102825,-58.7167715917778,-57.7215720732731,
-56.7263725547684,-55.7311730362637,-54.735973517759,-54.3009201196733),
 .UNSPECIFIED.);
#1381=B_SPLINE_CURVE_WITH_KNOTS('',3,(#55307,#55308,#55309,#55310,#55311,
#55312,#55313,#55314,#55315,#55316,#55317,#55318,#55319,#55320,#55321,#55322,
#55323,#55324,#55325,#55326,#55327,#55328,#55329,#55330,#55331,#55332,#55333,
#55334,#55335,#55336,#55337,#55338,#55339,#55340,#55341,#55342,#55343,#55344,
#55345,#55346,#55347,#55348,#55349,#55350,#55351,#55352,#55353,#55354,#55355,
#55356,#55357,#55358,#55359,#55360,#55361,#55362,#55363,#55364,#55365,#55366,
#55367,#55368,#55369,#55370,#55371,#55372,#55373,#55374,#55375,#55376,#55377,
#55378,#55379,#55380,#55381,#55382,#55383,#55384,#55385,#55386,#55387,#55388,
#55389,#55390,#55391,#55392,#55393,#55394,#55395,#55396,#55397,#55398,#55399,
#55400,#55401,#55402,#55403,#55404,#55405,#55406,#55407,#55408,#55409,#55410,
#55411,#55412,#55413,#55414,#55415,#55416,#55417,#55418,#55419,#55420,#55421,
#55422,#55423,#55424,#55425,#55426,#55427,#55428,#55429,#55430,#55431,#55432,
#55433,#55434,#55435,#55436,#55437,#55438,#55439,#55440,#55441,#55442,#55443,
#55444,#55445,#55446,#55447,#55448,#55449,#55450,#55451,#55452,#55453,#55454,
#55455,#55456,#55457,#55458,#55459,#55460,#55461,#55462,#55463,#55464,#55465,
#55466,#55467,#55468,#55469,#55470,#55471,#55472,#55473,#55474,#55475,#55476,
#55477,#55478,#55479,#55480,#55481,#55482,#55483,#55484,#55485,#55486,#55487,
#55488,#55489,#55490,#55491,#55492,#55493,#55494,#55495,#55496,#55497,#55498,
#55499),.UNSPECIFIED.,.F.,.F.,(4,3,3,3,3,3,3,3,3,3,3,3,3,3,3,3,3,3,3,3,
3,3,3,3,3,3,3,3,3,3,3,3,3,3,3,3,3,3,3,3,3,3,3,3,3,3,3,3,3,3,3,3,3,3,3,3,
3,3,3,3,3,3,3,3,4),(-54.3009154377211,-54.1982387367601,-54.095489715743,
-53.9925596038351,-53.8895284587086,-53.7862850394966,-53.7407739992543,
-53.6401407054337,-53.5396521262388,-53.4392796141279,-53.3389704602745,
-53.2386933925698,-53.1384171793937,-53.0380412543939,-52.9376166889798,
-52.8370116386147,-52.7455744807496,-52.6449411869291,-52.5444526077341,
-52.4440800956232,-52.3437709417699,-52.2434938740655,-52.1432176608895,
-52.0428417358898,-51.9424171704756,-51.8418121201105,-51.7503749622449,
-51.6497416684244,-51.5492530892298,-51.4488805771189,-51.3485714232656,
-51.248294355561,-51.1480181423849,-51.0476422173853,-50.9472176519712,
-50.8466126016061,-50.7551754437401,-50.6545421499194,-50.5540535707246,
-50.4536810586138,-50.3533719047605,-50.2530948370559,-50.1528186238798,
-50.05244269888,-49.9520181334659,-49.8514130831007,-49.7599759252354,-49.6593426314148,
-49.5588540522202,-49.4584815401094,-49.358172386256,-49.2578953185515,
-49.1576191053754,-49.0572431803758,-48.9568186149618,-48.8562135645966,
-48.7647764067307,-48.665331690439,-48.5660176090869,-48.4668013028627,
-48.3676500354695,-48.268502398764,-48.1693583936258,-48.0701377857838,
-48.0177301305415),.UNSPECIFIED.);
#1382=B_SPLINE_CURVE_WITH_KNOTS('',3,(#55501,#55502,#55503,#55504,#55505,
#55506,#55507,#55508,#55509,#55510,#55511,#55512,#55513,#55514,#55515,#55516,
#55517,#55518,#55519,#55520,#55521,#55522,#55523,#55524,#55525,#55526,#55527,
#55528,#55529,#55530,#55531,#55532,#55533,#55534,#55535,#55536,#55537,#55538,
#55539,#55540,#55541,#55542,#55543,#55544,#55545,#55546,#55547,#55548,#55549,
#55550,#55551,#55552,#55553,#55554,#55555,#55556,#55557,#55558,#55559,#55560,
#55561,#55562,#55563,#55564,#55565,#55566,#55567,#55568,#55569,#55570,#55571,
#55572,#55573,#55574,#55575,#55576,#55577,#55578,#55579,#55580,#55581,#55582,
#55583,#55584,#55585,#55586,#55587,#55588,#55589,#55590,#55591,#55592,#55593,
#55594,#55595,#55596,#55597,#55598,#55599,#55600,#55601,#55602,#55603,#55604,
#55605,#55606,#55607,#55608,#55609,#55610,#55611,#55612,#55613,#55614,#55615,
#55616,#55617,#55618,#55619,#55620,#55621,#55622,#55623,#55624,#55625,#55626,
#55627,#55628,#55629,#55630,#55631,#55632,#55633,#55634,#55635,#55636,#55637,
#55638,#55639,#55640,#55641,#55642,#55643,#55644,#55645,#55646,#55647,#55648,
#55649,#55650,#55651,#55652,#55653,#55654,#55655,#55656,#55657,#55658,#55659,
#55660,#55661,#55662,#55663,#55664,#55665,#55666,#55667,#55668,#55669,#55670,
#55671,#55672,#55673,#55674,#55675,#55676,#55677,#55678,#55679,#55680,#55681,
#55682,#55683,#55684,#55685,#55686,#55687,#55688,#55689,#55690),
 .UNSPECIFIED.,.F.,.F.,(4,3,3,3,3,3,3,3,3,3,3,3,3,3,3,3,3,3,3,3,3,3,3,3,
3,3,3,3,3,3,3,3,3,3,3,3,3,3,3,3,3,3,3,3,3,3,3,3,3,3,3,3,3,3,3,3,3,3,3,3,
3,3,3,4),(-48.0177301301753,-47.8875166216952,-47.769576888226,-47.6689435944054,
-47.5684550152104,-47.4680825030995,-47.367773349246,-47.2674962815413,
-47.1672200683651,-47.0668441433653,-46.966419577951,-46.8658145275858,
-46.7743773697213,-46.6737440759008,-46.5732554967061,-46.4728829845953,
-46.372573830742,-46.2722967630375,-46.1720205498615,-46.0716446248619,
-45.9712200594479,-45.8706150090829,-45.7791778512166,-45.678544557396,
-45.5780559782012,-45.4776834660903,-45.3773743122369,-45.2770972445323,
-45.1768210313562,-45.0764451063565,-44.9760205409424,-44.8754154905773,
-44.7839783327119,-44.6833450388914,-44.5828564596966,-44.4824839475857,
-44.3821747937323,-44.2818977260278,-44.1816215128516,-44.081245587852,
-43.9808210224379,-43.8802159720727,-43.7887788142072,-43.6881455203867,
-43.5876569411918,-43.487284429081,-43.3869752752276,-43.286698207523,-43.1864219943469,
-43.0860460693472,-42.985621503933,-42.8850164535679,-42.7935792957025,
-42.6929460018821,-42.5924574226874,-42.4920849105766,-42.3917757567232,
-42.2914986890187,-42.1912224758426,-42.090846550843,-41.9904219854289,
-41.8898169350638,-41.7983797771978,-41.7345448233619),.UNSPECIFIED.);
#1383=B_SPLINE_CURVE_WITH_KNOTS('',3,(#55692,#55693,#55694,#55695,#55696,
#55697,#55698,#55699,#55700,#55701,#55702,#55703,#55704,#55705,#55706,#55707,
#55708,#55709,#55710,#55711,#55712,#55713,#55714,#55715,#55716,#55717,#55718,
#55719,#55720,#55721,#55722,#55723,#55724,#55725,#55726,#55727,#55728,#55729,
#55730,#55731,#55732,#55733,#55734,#55735,#55736,#55737,#55738,#55739,#55740,
#55741,#55742,#55743,#55744,#55745,#55746,#55747,#55748,#55749,#55750,#55751,
#55752,#55753,#55754,#55755,#55756,#55757,#55758,#55759,#55760,#55761,#55762,
#55763,#55764,#55765,#55766,#55767,#55768,#55769,#55770,#55771,#55772,#55773,
#55774,#55775,#55776,#55777,#55778,#55779,#55780,#55781,#55782,#55783,#55784,
#55785,#55786,#55787,#55788,#55789,#55790,#55791,#55792,#55793,#55794,#55795,
#55796,#55797,#55798,#55799,#55800,#55801,#55802,#55803,#55804,#55805,#55806,
#55807,#55808,#55809,#55810,#55811,#55812,#55813,#55814,#55815,#55816,#55817,
#55818,#55819,#55820,#55821,#55822,#55823,#55824,#55825,#55826,#55827,#55828,
#55829,#55830,#55831,#55832,#55833,#55834,#55835,#55836,#55837,#55838,#55839,
#55840,#55841,#55842,#55843,#55844,#55845,#55846,#55847,#55848,#55849,#55850,
#55851,#55852,#55853,#55854,#55855,#55856,#55857,#55858,#55859,#55860,#55861,
#55862,#55863,#55864,#55865,#55866,#55867,#55868,#55869,#55870,#55871,#55872,
#55873,#55874,#55875,#55876,#55877,#55878,#55879,#55880,#55881,#55882,#55883,
#55884),.UNSPECIFIED.,.F.,.F.,(4,3,3,3,3,3,3,3,3,3,3,3,3,3,3,3,3,3,3,3,
3,3,3,3,3,3,3,3,3,3,3,3,3,3,3,3,3,3,3,3,3,3,3,3,3,3,3,3,3,3,3,3,3,3,3,3,
3,3,3,3,3,3,3,3,4),(-41.7345448229899,-41.6348663122446,-41.5309055555507,
-41.4314723515032,-41.3320923789549,-41.2327332315475,-41.1333625337808,
-41.0338869682092,-40.934349449426,-40.8346519333653,-40.8031802586931,
-40.7025469648726,-40.6020583856776,-40.5016858735667,-40.4013767197132,
-40.3010996520086,-40.2008234388324,-40.1004475138327,-40.0000229484186,
-39.8994178980534,-39.8079807401883,-39.7073474463679,-39.6068588671731,
-39.5064863550622,-39.4061772012088,-39.3059001335042,-39.2056239203282,
-39.1052479953285,-39.0048234299144,-38.9042183795492,-38.8127812216836,
-38.7121479278631,-38.6116593486681,-38.5112868365573,-38.4109776827039,
-38.3107006149993,-38.2104244018232,-38.1100484768235,-38.0096239114096,
-37.9090188610445,-37.8175817031789,-37.7169484093583,-37.6164598301635,
-37.5160873180526,-37.4157781641993,-37.3155010964947,-37.2152248833183,
-37.1148489583186,-37.0144243929046,-36.9138193425394,-36.8223821846742,
-36.7217488908536,-36.6212603116586,-36.5208877995478,-36.4205786456944,
-36.3203015779899,-36.2200253648136,-36.1196494398139,-36.0192248743999,
-35.9186198240348,-35.8271826661695,-35.7136072223652,-35.600451639753,
-35.4880062437431,-35.4513595164066),.UNSPECIFIED.);
#1384=B_SPLINE_CURVE_WITH_KNOTS('',3,(#55886,#55887,#55888,#55889,#55890,
#55891,#55892,#55893,#55894,#55895,#55896,#55897,#55898,#55899,#55900,#55901,
#55902,#55903,#55904,#55905,#55906,#55907,#55908,#55909,#55910,#55911,#55912,
#55913,#55914,#55915,#55916,#55917,#55918,#55919,#55920,#55921,#55922,#55923,
#55924,#55925,#55926,#55927,#55928,#55929,#55930,#55931,#55932,#55933,#55934,
#55935,#55936,#55937,#55938,#55939,#55940,#55941,#55942,#55943,#55944,#55945,
#55946,#55947,#55948,#55949,#55950,#55951,#55952,#55953,#55954,#55955,#55956,
#55957,#55958,#55959,#55960,#55961,#55962,#55963,#55964,#55965,#55966,#55967,
#55968,#55969,#55970,#55971,#55972,#55973,#55974,#55975,#55976,#55977,#55978,
#55979,#55980,#55981,#55982,#55983,#55984,#55985,#55986,#55987,#55988,#55989,
#55990,#55991,#55992,#55993,#55994,#55995,#55996,#55997,#55998,#55999,#56000,
#56001,#56002,#56003,#56004,#56005,#56006,#56007,#56008,#56009,#56010,#56011,
#56012,#56013,#56014,#56015,#56016,#56017,#56018,#56019,#56020,#56021,#56022,
#56023,#56024,#56025,#56026,#56027,#56028,#56029,#56030,#56031,#56032,#56033,
#56034,#56035,#56036,#56037,#56038,#56039,#56040,#56041,#56042,#56043,#56044,
#56045,#56046,#56047,#56048,#56049,#56050,#56051,#56052,#56053,#56054,#56055,
#56056,#56057,#56058,#56059,#56060,#56061,#56062,#56063,#56064,#56065,#56066,
#56067,#56068,#56069,#56070,#56071,#56072,#56073,#56074,#56075),
 .UNSPECIFIED.,.F.,.F.,(4,3,3,3,3,3,3,3,3,3,3,3,3,3,3,3,3,3,3,3,3,3,3,3,
3,3,3,3,3,3,3,3,3,3,3,3,3,3,3,3,3,3,3,3,3,3,3,3,3,3,3,3,3,3,3,3,3,3,3,3,
3,3,3,4),(-35.4513595161824,-35.3502780910073,-35.2491815897649,-35.1448819792399,
-35.0435980657394,-34.9377906067021,-34.8319831476648,-34.7313498538444,
-34.6308612746499,-34.5304887625391,-34.4301796086858,-34.3299025409813,
-34.2296263278054,-34.1292504028059,-34.0288258373918,-33.9282207870267,
-33.8367836291601,-33.7361503353399,-33.6356617561455,-33.5352892440351,
-33.4349800901822,-33.3347030224781,-33.2344268093024,-33.1340508843032,
-33.0336263188895,-32.9330212685249,-32.8415841106554,-32.7409508168336,
-32.6404622376377,-32.5400897255256,-32.4397805716711,-32.3395035039652,
-32.239227290788,-32.1388513657872,-32.0384268003719,-31.9378217500056,
-31.8463845921507,-31.745751298331,-31.6452627191372,-31.5448902070272,
-31.4445810531747,-31.3443039854709,-31.2440277722955,-31.1436518472967,
-31.0432272818834,-30.9426222315191,-30.851185073646,-30.750551779828,-30.6500632006356,
-30.5496906885274,-30.4493815346766,-30.3491044669747,-30.2488282538009,
-30.1484523288039,-30.0480277633924,-29.9474227130299,-29.8559855551413,
-29.7558310335539,-29.6558138224566,-29.555901863842,-29.4560514758558,
-29.3562408059202,-29.2563942120037,-29.1681742090028),.UNSPECIFIED.);
#1385=B_SPLINE_CURVE_WITH_KNOTS('',3,(#56077,#56078,#56079,#56080,#56081,
#56082,#56083,#56084,#56085,#56086,#56087,#56088,#56089,#56090,#56091,#56092,
#56093,#56094,#56095,#56096,#56097,#56098,#56099,#56100,#56101,#56102,#56103,
#56104,#56105,#56106,#56107,#56108,#56109,#56110,#56111,#56112,#56113,#56114,
#56115,#56116,#56117,#56118,#56119,#56120,#56121,#56122,#56123,#56124,#56125,
#56126,#56127,#56128,#56129,#56130,#56131,#56132,#56133,#56134,#56135,#56136,
#56137,#56138,#56139,#56140,#56141,#56142,#56143,#56144,#56145,#56146,#56147,
#56148,#56149,#56150,#56151,#56152,#56153,#56154,#56155,#56156,#56157,#56158,
#56159,#56160,#56161,#56162,#56163,#56164,#56165,#56166,#56167,#56168,#56169,
#56170,#56171,#56172,#56173,#56174,#56175,#56176,#56177,#56178,#56179,#56180,
#56181,#56182,#56183,#56184,#56185,#56186,#56187,#56188,#56189,#56190,#56191,
#56192,#56193,#56194,#56195,#56196,#56197,#56198,#56199,#56200,#56201,#56202,
#56203,#56204,#56205,#56206,#56207,#56208,#56209,#56210,#56211,#56212,#56213,
#56214,#56215,#56216,#56217,#56218,#56219,#56220,#56221,#56222,#56223,#56224,
#56225,#56226,#56227,#56228,#56229,#56230,#56231,#56232,#56233,#56234,#56235,
#56236,#56237,#56238,#56239,#56240,#56241,#56242,#56243,#56244,#56245,#56246,
#56247,#56248,#56249,#56250,#56251,#56252,#56253,#56254,#56255,#56256,#56257,
#56258,#56259,#56260,#56261,#56262,#56263,#56264,#56265,#56266,#56267,#56268,
#56269),.UNSPECIFIED.,.F.,.F.,(4,3,3,3,3,3,3,3,3,3,3,3,3,3,3,3,3,3,3,3,
3,3,3,3,3,3,3,3,3,3,3,3,3,3,3,3,3,3,3,3,3,3,3,3,3,3,3,3,3,3,3,3,3,3,3,3,
3,3,3,3,3,3,3,3,4),(-29.1681742086401,-29.048677086425,-28.9276740828448,
-28.8607860366366,-28.7601527428248,-28.6596641636387,-28.5592916515365,
-28.4589824976917,-28.3587054299956,-28.2584292168279,-28.1580532918364,
-28.0576287264303,-27.957023676073,-27.8655865181318,-27.7649532243258,
-27.6644646451456,-27.5640921330496,-27.4637829792112,-27.3635059115216,
-27.2632296983605,-27.1628537733758,-27.0624292079767,-26.9618241576264,
-26.8703869996271,-26.7697537057427,-26.6692651264839,-26.5688926143092,
-26.468583460392,-26.3683063926239,-26.2680301793844,-26.1676542543223,
-26.0672296888461,-25.9666246384202,-25.8751874811224,-25.7745541873821,
-25.6740656082671,-25.5736930962353,-25.4733839424605,-25.3731068748338,
-25.2728306617349,-25.1724547368107,-25.0720301714713,-24.9714251211786,
-24.8799879626177,-24.7793546688679,-24.6788660897448,-24.5784935777071,
-24.4781844239276,-24.3779073562977,-24.2776311431967,-24.1772552182725,
-24.0768306529341,-23.9762256026443,-23.884788444113,-23.7841551498422,
-23.6836665701958,-23.5832940576337,-23.4829849033294,-23.382707835175,
-23.2824316215506,-23.1820556961083,-23.0816311302539,-22.9810260794576,
-22.8895889256083,-22.8849889018232),.UNSPECIFIED.);
#1386=B_SPLINE_CURVE_WITH_KNOTS('',3,(#56271,#56272,#56273,#56274,#56275,
#56276,#56277,#56278,#56279,#56280,#56281,#56282,#56283,#56284,#56285,#56286,
#56287,#56288,#56289,#56290,#56291,#56292,#56293,#56294,#56295,#56296,#56297,
#56298,#56299,#56300,#56301,#56302,#56303,#56304,#56305,#56306,#56307,#56308,
#56309,#56310,#56311,#56312,#56313,#56314,#56315,#56316,#56317,#56318,#56319,
#56320,#56321,#56322,#56323,#56324,#56325,#56326,#56327,#56328,#56329,#56330,
#56331,#56332,#56333,#56334,#56335,#56336,#56337,#56338,#56339,#56340,#56341,
#56342,#56343,#56344,#56345,#56346,#56347,#56348,#56349,#56350,#56351,#56352,
#56353,#56354,#56355,#56356,#56357,#56358,#56359,#56360,#56361,#56362,#56363,
#56364,#56365,#56366,#56367,#56368,#56369,#56370,#56371,#56372,#56373,#56374,
#56375,#56376,#56377,#56378,#56379,#56380,#56381,#56382,#56383,#56384,#56385,
#56386,#56387,#56388,#56389,#56390,#56391,#56392,#56393,#56394,#56395,#56396,
#56397,#56398,#56399,#56400,#56401,#56402,#56403,#56404,#56405,#56406,#56407,
#56408,#56409,#56410,#56411,#56412,#56413,#56414,#56415,#56416,#56417,#56418,
#56419,#56420,#56421,#56422,#56423,#56424,#56425,#56426,#56427,#56428,#56429,
#56430,#56431,#56432,#56433,#56434,#56435,#56436,#56437,#56438,#56439,#56440,
#56441,#56442,#56443,#56444,#56445,#56446,#56447,#56448,#56449,#56450,#56451,
#56452,#56453,#56454,#56455,#56456,#56457,#56458,#56459,#56460),
 .UNSPECIFIED.,.F.,.F.,(4,3,3,3,3,3,3,3,3,3,3,3,3,3,3,3,3,3,3,3,3,3,3,3,
3,3,3,3,3,3,3,3,3,3,3,3,3,3,3,3,3,3,3,3,3,3,3,3,3,3,3,3,3,3,3,3,3,3,3,3,
3,3,3,4),(-22.8849889015675,-22.7844384795331,-22.6840326799569,-22.5837426163004,
-22.4835155834612,-22.383320192787,-22.2831250957898,-22.182830154689,-22.0824858463468,
-21.9819624781745,-21.8943894071036,-21.7937561135299,-21.69326753459,-21.5928950227447,
-21.4925858691631,-21.3923088017363,-21.2920325888435,-21.1916566641336,
-21.0912320990133,-20.9906270489452,-20.8991898885989,-20.7985565916873,
-20.6980680093904,-20.5976954941759,-20.4973863372192,-20.3971092664161,
-20.2968330501503,-20.1964571220964,-20.0960325536427,-19.995427500298,
-19.9039903700942,-19.8033570818677,-19.7028685082599,-19.6024960016997,
-19.5021868533724,-19.4019097911618,-19.3016335834403,-19.2012576637958,
-19.100833103691,-19.0002280584961,-18.9087908515895,-18.808157557575,-18.7076689782416,
-18.6072964660754,-18.5069873122171,-18.4067102445576,-18.3064340314764,
-18.2060581066479,-18.1056335414471,-18.0050284913629,-17.9135913330848,
-17.8129580186678,-17.7124694187854,-17.6120968859483,-17.5117877113545,
-17.4115106229241,-17.3112343890657,-17.2108584435958,-17.1104338577948,
-17.0098287874223,-16.91839181458,-16.798461421715,-16.6798620946292,-16.6018035950335),
 .UNSPECIFIED.);
#1387=B_SPLINE_CURVE_WITH_KNOTS('',3,(#56462,#56463,#56464,#56465,#56466,
#56467,#56468,#56469,#56470,#56471,#56472,#56473,#56474,#56475,#56476,#56477,
#56478,#56479,#56480,#56481,#56482,#56483,#56484,#56485,#56486,#56487,#56488,
#56489,#56490,#56491,#56492,#56493,#56494,#56495,#56496,#56497,#56498,#56499,
#56500,#56501,#56502,#56503,#56504,#56505,#56506,#56507,#56508,#56509,#56510,
#56511,#56512,#56513,#56514,#56515,#56516,#56517,#56518,#56519,#56520,#56521,
#56522,#56523,#56524,#56525,#56526,#56527,#56528,#56529,#56530,#56531,#56532,
#56533,#56534,#56535,#56536,#56537,#56538,#56539,#56540,#56541,#56542,#56543,
#56544,#56545,#56546,#56547,#56548,#56549,#56550,#56551,#56552,#56553,#56554,
#56555,#56556,#56557,#56558,#56559,#56560,#56561,#56562,#56563,#56564,#56565,
#56566,#56567,#56568,#56569,#56570,#56571,#56572,#56573,#56574,#56575,#56576,
#56577,#56578,#56579,#56580,#56581,#56582,#56583,#56584,#56585,#56586,#56587,
#56588,#56589,#56590,#56591,#56592,#56593,#56594,#56595,#56596,#56597,#56598,
#56599,#56600,#56601,#56602,#56603,#56604,#56605,#56606,#56607,#56608,#56609,
#56610,#56611,#56612,#56613,#56614,#56615,#56616,#56617,#56618,#56619,#56620,
#56621,#56622,#56623,#56624,#56625,#56626,#56627,#56628,#56629,#56630,#56631,
#56632,#56633,#56634,#56635,#56636,#56637,#56638,#56639,#56640,#56641,#56642,
#56643,#56644,#56645,#56646,#56647,#56648,#56649,#56650,#56651,#56652,#56653,
#56654),.UNSPECIFIED.,.F.,.F.,(4,3,3,3,3,3,3,3,3,3,3,3,3,3,3,3,3,3,3,3,
3,3,3,3,3,3,3,3,3,3,3,3,3,3,3,3,3,3,3,3,3,3,3,3,3,3,3,3,3,3,3,3,3,3,3,3,
3,3,3,3,3,3,3,3,4),(-16.6018035946436,-16.5018286166216,-16.4018795570295,
-16.3019248208445,-16.2018628992254,-16.1017459451112,-16.0014471696866,
-15.9231922960753,-15.8225589863926,-15.7220703917125,-15.6216978647484,
-15.5213886964323,-15.421111614672,-15.320835387864,-15.2204594499848,-15.1200348720827,
-15.0194298100292,-14.9279927775706,-14.8273593513153,-14.7268706389542,
-14.6264979932084,-14.5261887054969,-14.4259115038978,-14.3256351569767,
-14.2252590994022,-14.1248344018427,-14.0242292216037,-13.9327932590659,
-13.8321603041925,-13.7316720640727,-13.6312998896521,-13.5309910724934,
-13.4307143400328,-13.3304384601937,-13.2300628632367,-13.1296386234898,
-13.0290338909971,-12.9375937405612,-12.8369602289812,-12.7364714345042,
-12.6360987117923,-12.5357893502765,-12.4355120781078,-12.3352356639284,
-12.2348595447007,-12.1344347884583,-12.0338295551795,-11.9423942220565,
-11.8417601148349,-11.7412707165318,-11.6408973806369,-11.5405874005388,
-11.44030950529,-11.3400324644301,-11.2396557173348,-11.1392303315746,-11.0386244734383,
-10.9471947035518,-10.845900037974,-10.7447544119353,-10.6437275255628,
-10.5427944091178,-10.4419147704534,-10.34104881343,-10.318618287464),
 .UNSPECIFIED.);
#1388=B_SPLINE_CURVE_WITH_KNOTS('',3,(#56655,#56656,#56657,#56658,#56659,
#56660,#56661,#56662,#56663,#56664,#56665,#56666,#56667,#56668,#56669,#56670,
#56671,#56672,#56673,#56674,#56675,#56676,#56677,#56678,#56679,#56680,#56681,
#56682,#56683,#56684,#56685,#56686,#56687,#56688,#56689,#56690,#56691,#56692,
#56693,#56694,#56695,#56696,#56697,#56698,#56699,#56700,#56701,#56702,#56703,
#56704,#56705,#56706,#56707,#56708,#56709,#56710,#56711,#56712,#56713,#56714,
#56715,#56716,#56717,#56718,#56719,#56720,#56721,#56722,#56723,#56724,#56725,
#56726,#56727,#56728,#56729,#56730,#56731,#56732,#56733,#56734,#56735,#56736,
#56737,#56738,#56739,#56740,#56741,#56742,#56743,#56744,#56745,#56746,#56747,
#56748,#56749,#56750,#56751,#56752,#56753,#56754,#56755,#56756,#56757,#56758,
#56759,#56760,#56761,#56762,#56763,#56764,#56765,#56766,#56767,#56768,#56769,
#56770,#56771,#56772,#56773,#56774,#56775,#56776,#56777,#56778,#56779,#56780,
#56781,#56782,#56783,#56784,#56785,#56786,#56787,#56788,#56789,#56790,#56791,
#56792,#56793,#56794,#56795,#56796,#56797,#56798,#56799,#56800,#56801,#56802,
#56803,#56804,#56805,#56806,#56807,#56808,#56809,#56810,#56811,#56812,#56813,
#56814,#56815,#56816,#56817,#56818,#56819,#56820,#56821,#56822,#56823,#56824,
#56825,#56826,#56827,#56828,#56829,#56830,#56831,#56832,#56833,#56834,#56835,
#56836,#56837,#56838,#56839,#56840,#56841,#56842,#56843,#56844,#56845,#56846,
#56847),.UNSPECIFIED.,.F.,.F.,(4,3,3,3,3,3,3,3,3,3,3,3,3,3,3,3,3,3,3,3,
3,3,3,3,3,3,3,3,3,3,3,3,3,3,3,3,3,3,3,3,3,3,3,3,3,3,3,3,3,3,3,3,3,3,3,3,
3,3,3,3,3,3,3,3,4),(-10.3186182872368,-10.2052774276635,-10.0913956938805,
-9.97687885509846,-9.95199518504708,-9.85135960040161,-9.75086874603975,
-9.65049399259817,-9.55018261898653,-9.44990335596195,-9.34962497479173,
-9.24924693936844,-9.14882029168565,-9.04821323050691,-8.95679566654237,
-8.85615769082409,-8.75566438639974,-8.65528710663062,-8.55497316155205,
-8.45469128587806,-8.35441025479137,-8.2540295302673,-8.15360016775222,
-8.0529903808043,-7.96159614803767,-7.86098132409402,-7.76051124718896,
-7.66015719974532,-7.55986647932878,-7.45960778877813,-7.35934987137945,
-7.25899198778301,-7.15858535335808,-7.05799783872295,-6.96639662953296,
-6.8657419231591,-6.76523202542015,-6.66483843365732,-6.56450835497409,
-6.46421054479971,-6.36391379921318,-6.26351781155996,-6.16307340882067,
-6.06244913021843,-5.97119711102825,-5.87053955275317,-5.77002638776563,
-5.66962892692334,-5.56929461557409,-5.46899221832587,-5.36869054009127,
-5.26828911882982,-5.16783899958796,-5.06720860033739,-4.97599759252354,
-4.87631117852719,-4.7767689836149,-4.67734052968798,-4.57797267530372,
-4.47863299114264,-4.37928908656279,-4.27984729266011,-4.18035000264988,
-4.08069243412998,-4.03543298063145),.UNSPECIFIED.);
#1389=B_SPLINE_CURVE_WITH_KNOTS('',3,(#56850,#56851,#56852,#56853,#56854,
#56855,#56856,#56857,#56858,#56859,#56860,#56861,#56862,#56863,#56864,#56865,
#56866,#56867,#56868,#56869,#56870,#56871,#56872,#56873,#56874,#56875,#56876,
#56877,#56878,#56879,#56880,#56881,#56882,#56883,#56884,#56885,#56886,#56887,
#56888,#56889),.UNSPECIFIED.,.F.,.F.,(4,3,3,3,3,3,3,3,3,3,3,3,3,4),(177.819192458502,
177.870849877951,177.976746287652,178.087909176253,178.193518105667,178.299063112442,
178.404580569928,178.510106809205,178.615746262861,178.721451484676,178.827334848772,
178.866049396456,179.014820834809,179.070781254618),.UNSPECIFIED.);
#1390=B_SPLINE_CURVE_WITH_KNOTS('',3,(#56891,#56892,#56893,#56894,#56895,
#56896,#56897,#56898,#56899,#56900,#56901,#56902,#56903,#56904,#56905,#56906,
#56907,#56908,#56909,#56910,#56911,#56912,#56913,#56914,#56915,#56916,#56917,
#56918,#56919,#56920,#56921,#56922,#56923,#56924,#56925,#56926,#56927,#56928,
#56929,#56930,#56931,#56932,#56933,#56934,#56935,#56936,#56937,#56938,#56939,
#56940,#56941,#56942,#56943,#56944,#56945,#56946,#56947,#56948,#56949,#56950,
#56951,#56952,#56953,#56954,#56955,#56956,#56957,#56958,#56959,#56960,#56961,
#56962,#56963,#56964,#56965,#56966,#56967,#56968,#56969,#56970,#56971,#56972,
#56973,#56974,#56975,#56976,#56977,#56978,#56979,#56980,#56981,#56982,#56983,
#56984,#56985,#56986,#56987,#56988,#56989,#56990,#56991,#56992,#56993,#56994,
#56995,#56996,#56997,#56998,#56999,#57000,#57001,#57002,#57003,#57004,#57005,
#57006,#57007,#57008),.UNSPECIFIED.,.F.,.F.,(4,3,3,3,3,3,3,3,3,3,3,3,3,
3,3,3,3,3,3,3,3,3,3,3,3,3,3,3,3,3,3,3,3,3,3,3,3,3,3,4),(179.07078125494,
179.174995091213,179.279122198882,179.383200887903,179.487269395697,179.591434908581,
179.695652687092,179.800050733087,179.86124891496,179.966984731998,180.072561027452,
180.178013820682,180.283401178045,180.388759713088,180.49412599568,180.59960664732,
180.705152489819,180.810881328432,180.856448433465,180.962518989792,181.073660110064,
181.179441227978,181.285157249995,181.39084428965,181.496538416766,181.602342168825,
181.708209802484,181.814251277373,181.85164795197,181.957645557193,182.068795796353,
182.174511996658,182.280166179011,182.385794524185,182.491433172546,182.597186535568,
182.703006662787,182.809005320892,182.846847470474,182.852224483266),
 .UNSPECIFIED.);
#1391=B_SPLINE_CURVE_WITH_KNOTS('',3,(#57012,#57013,#57014,#57015,#57016,
#57017,#57018,#57019,#57020,#57021,#57022,#57023,#57024,#57025,#57026,#57027,
#57028,#57029,#57030,#57031,#57032,#57033,#57034,#57035,#57036,#57037,#57038,
#57039,#57040,#57041,#57042,#57043,#57044,#57045,#57046,#57047,#57048,#57049,
#57050,#57051,#57052,#57053,#57054,#57055,#57056,#57057,#57058,#57059,#57060,
#57061,#57062,#57063,#57064,#57065,#57066,#57067,#57068,#57069,#57070,#57071,
#57072,#57073,#57074,#57075,#57076,#57077,#57078,#57079,#57080,#57081,#57082,
#57083,#57084),.UNSPECIFIED.,.F.,.F.,(4,3,3,3,3,3,3,3,3,3,3,3,3,3,3,3,3,
3,3,3,3,3,3,3,4),(179.070781255096,179.185620068578,179.300780012931,179.416435972135,
179.507913446056,179.612695797115,179.717318404753,179.821821446474,179.926261807326,
180.030677319518,180.135105774966,180.239662568643,180.34429093876,180.44912182172,
180.503112964561,180.611895504391,180.722697626725,180.831119906092,180.939439767263,
181.047686885078,181.160343284574,181.268563069598,181.376793276413,181.485096017127,
181.498312483065),.UNSPECIFIED.);
#1392=B_SPLINE_CURVE_WITH_KNOTS('',3,(#57085,#57086,#57087,#57088,#57089,
#57090,#57091,#57092,#57093,#57094,#57095,#57096,#57097,#57098,#57099,#57100,
#57101,#57102,#57103,#57104,#57105,#57106,#57107,#57108,#57109,#57110,#57111,
#57112,#57113,#57114,#57115,#57116,#57117,#57118,#57119,#57120,#57121,#57122,
#57123,#57124,#57125,#57126,#57127,#57128,#57129,#57130,#57131,#57132,#57133,
#57134,#57135,#57136,#57137,#57138),.UNSPECIFIED.,.F.,.F.,(4,2,2,2,2,2,
2,2,2,2,2,2,2,2,2,2,2,2,2,2,2,2,2,2,2,2,4),(-2.43068563765362,-2.42265074372402,
-2.42024534622642,-2.41836210929473,-2.41647245656861,-2.414316274935,-2.41077045154461,
-2.39913112758483,-2.3524461932698,-2.3299497556685,-2.32572060496249,-2.32408420621342,
-2.32294866987872,-2.32192931846328,-2.32025802836276,-2.31602250759433,
-2.27620058838792,-2.24816465604659,-2.23858750987126,-2.23396094982001,
-2.23119225346768,-2.22870741324186,-2.22680052548476,-2.22497300025956,
-2.22243828418116,-2.21585189577543,-2.18872254859161),.UNSPECIFIED.);
#1393=B_SPLINE_CURVE_WITH_KNOTS('',3,(#57142,#57143,#57144,#57145,#57146,
#57147,#57148,#57149,#57150,#57151,#57152,#57153,#57154,#57155,#57156,#57157,
#57158,#57159,#57160,#57161,#57162,#57163,#57164,#57165,#57166,#57167,#57168,
#57169,#57170,#57171,#57172,#57173,#57174,#57175,#57176,#57177,#57178,#57179,
#57180,#57181,#57182,#57183,#57184,#57185,#57186,#57187,#57188,#57189,#57190,
#57191,#57192,#57193,#57194,#57195,#57196,#57197,#57198,#57199,#57200,#57201,
#57202,#57203,#57204,#57205,#57206,#57207,#57208,#57209,#57210,#57211,#57212,
#57213,#57214,#57215,#57216,#57217,#57218,#57219,#57220,#57221,#57222,#57223),
 .UNSPECIFIED.,.F.,.F.,(4,3,3,3,3,3,3,3,3,3,3,3,3,3,3,3,3,3,3,3,3,3,3,3,
3,3,3,4),(-0.423947533719778,-0.398852588470169,-0.377228555616947,-0.372439199709838,
-0.34764842283439,-0.329741977315031,-0.325329288343292,-0.321149784672366,
-0.296981160184881,-0.273087580671514,-0.249893960726593,-0.243157362702744,
-0.239407499053117,-0.235386549537422,-0.212468228537641,-0.204405790338345,
-0.180908491206444,-0.158373335170994,-0.153625676807497,-0.130854845993313,
-0.108177017216731,-0.0856898081540444,-0.0774429266195629,-0.0739031774787725,
-0.0519698695588112,-0.0306589296986993,-0.0096285538345829,0.),
 .UNSPECIFIED.);
#1394=B_SPLINE_CURVE_WITH_KNOTS('',3,(#57224,#57225,#57226,#57227,#57228,
#57229,#57230,#57231,#57232,#57233,#57234,#57235,#57236,#57237,#57238,#57239,
#57240,#57241,#57242,#57243,#57244,#57245,#57246,#57247,#57248,#57249,#57250,
#57251,#57252,#57253,#57254,#57255,#57256,#57257,#57258,#57259,#57260,#57261,
#57262,#57263,#57264,#57265,#57266,#57267,#57268,#57269,#57270,#57271,#57272,
#57273,#57274,#57275,#57276,#57277,#57278,#57279,#57280,#57281,#57282,#57283,
#57284,#57285,#57286,#57287,#57288,#57289,#57290,#57291,#57292,#57293,#57294,
#57295,#57296,#57297,#57298,#57299,#57300,#57301,#57302),.UNSPECIFIED.,
 .F.,.F.,(4,3,3,3,3,3,3,3,3,3,3,3,3,3,3,3,3,3,3,3,3,3,3,3,3,3,4),(-0.430289127733703,
-0.409131203295475,-0.391054495122007,-0.386034754015406,-0.363993110999897,
-0.346793254452062,-0.34223698527339,-0.337890536404446,-0.315048607800531,
-0.292209214405036,-0.269344703384665,-0.26200185233298,-0.25827143431592,
-0.234557662948815,-0.226394258617215,-0.203257661985663,-0.180121065354112,
-0.174814354906448,-0.151194220490317,-0.126840078836855,-0.102485937183392,
-0.0922144100858579,-0.0875882430594912,-0.0625337202221519,-0.0374931773906202,
-0.0129486697203148,0.),.UNSPECIFIED.);
#1395=B_SPLINE_CURVE_WITH_KNOTS('',3,(#58011,#58012,#58013,#58014),
 .UNSPECIFIED.,.F.,.F.,(4,4),(-0.0445064912682737,0.),.UNSPECIFIED.);
#1396=B_SPLINE_CURVE_WITH_KNOTS('',3,(#58015,#58016,#58017,#58018,#58019,
#58020,#58021,#58022,#58023,#58024,#58025,#58026,#58027,#58028,#58029,#58030,
#58031,#58032,#58033,#58034,#58035,#58036,#58037,#58038,#58039,#58040,#58041,
#58042,#58043,#58044,#58045,#58046,#58047,#58048,#58049,#58050,#58051,#58052,
#58053,#58054,#58055,#58056,#58057,#58058,#58059,#58060,#58061,#58062,#58063,
#58064,#58065,#58066,#58067,#58068,#58069,#58070,#58071,#58072,#58073,#58074,
#58075,#58076,#58077,#58078,#58079,#58080,#58081,#58082,#58083,#58084,#58085,
#58086,#58087,#58088,#58089,#58090,#58091,#58092,#58093),.UNSPECIFIED.,
 .F.,.F.,(4,3,3,3,3,3,3,3,3,3,3,3,3,3,3,3,3,3,3,3,3,3,3,3,3,3,4),(-0.430289127733828,
-0.409131192513218,-0.391054556741682,-0.386034835281542,-0.364002044843779,
-0.346793321163048,-0.342237084883542,-0.337890550896376,-0.315216893040039,
-0.292164481757858,-0.275755482800676,-0.262001866763717,-0.25827145905283,
-0.234557688497016,-0.226394258617259,-0.203257656753551,-0.180121054889843,
-0.174814354294875,-0.15112100411559,-0.126993562280297,-0.102598702378716,
-0.0922144183311342,-0.0875882464310277,-0.0626034767801118,-0.0376323704312253,
-0.0129486879091254,0.),.UNSPECIFIED.);
#1397=B_SPLINE_CURVE_WITH_KNOTS('',3,(#58098,#58099,#58100,#58101,#58102,
#58103,#58104,#58105,#58106,#58107,#58108,#58109,#58110,#58111,#58112,#58113,
#58114,#58115,#58116,#58117,#58118,#58119,#58120,#58121,#58122,#58123,#58124,
#58125,#58126,#58127,#58128,#58129,#58130,#58131,#58132,#58133,#58134,#58135,
#58136,#58137,#58138,#58139,#58140,#58141,#58142,#58143,#58144,#58145,#58146,
#58147,#58148,#58149,#58150,#58151,#58152,#58153,#58154,#58155,#58156,#58157,
#58158,#58159,#58160,#58161,#58162,#58163,#58164,#58165,#58166,#58167,#58168,
#58169,#58170,#58171,#58172,#58173,#58174,#58175,#58176,#58177,#58178,#58179),
 .UNSPECIFIED.,.F.,.F.,(4,3,3,3,3,3,3,3,3,3,3,3,3,3,3,3,3,3,3,3,3,3,3,3,
3,3,3,4),(-0.423947483310156,-0.39885253768024,-0.377228574786393,-0.37243923473487,
-0.347648458633374,-0.329742008624217,-0.325329264085242,-0.32114978023783,
-0.297024106120711,-0.273297481373415,-0.256074558614657,-0.24315736654559,
-0.239407516802922,-0.235386554398844,-0.212468243691861,-0.204405790338385,
-0.180908493451503,-0.158373340852528,-0.153625676577744,-0.130854850040819,
-0.108177012449888,-0.0856897908532072,-0.077442917873118,-0.073903169216813,
-0.051969851848939,-0.0306588946937463,-0.00962849885639309,-7.64403705571099E-15),
 .UNSPECIFIED.);
#1398=B_SPLINE_CURVE_WITH_KNOTS('',3,(#58889,#58890,#58891,#58892),
 .UNSPECIFIED.,.F.,.F.,(4,4),(-0.0446329464765972,0.),.UNSPECIFIED.);
#1399=B_SPLINE_CURVE_WITH_KNOTS('',3,(#59763,#59764,#59765,#59766,#59767,
#59768,#59769,#59770,#59771,#59772,#59773,#59774,#59775,#59776,#59777,#59778,
#59779,#59780,#59781,#59782,#59783,#59784,#59785,#59786,#59787,#59788,#59789,
#59790,#59791,#59792,#59793,#59794,#59795,#59796,#59797,#59798,#59799,#59800,
#59801,#59802,#59803,#59804,#59805,#59806,#59807,#59808,#59809,#59810,#59811,
#59812,#59813,#59814,#59815,#59816,#59817,#59818,#59819,#59820,#59821,#59822,
#59823,#59824,#59825,#59826,#59827,#59828,#59829,#59830,#59831,#59832,#59833,
#59834,#59835,#59836,#59837,#59838,#59839,#59840,#59841,#59842,#59843,#59844,
#59845,#59846,#59847,#59848,#59849,#59850,#59851,#59852,#59853,#59854,#59855,
#59856,#59857,#59858,#59859,#59860,#59861,#59862,#59863,#59864,#59865,#59866,
#59867,#59868,#59869,#59870,#59871,#59872,#59873,#59874,#59875,#59876,#59877,
#59878,#59879,#59880,#59881,#59882,#59883,#59884,#59885,#59886,#59887,#59888,
#59889,#59890,#59891,#59892,#59893,#59894,#59895,#59896,#59897,#59898,#59899,
#59900,#59901,#59902,#59903,#59904,#59905,#59906,#59907,#59908,#59909,#59910,
#59911,#59912,#59913,#59914,#59915,#59916),.UNSPECIFIED.,.F.,.F.,(4,3,3,
3,3,3,3,3,3,3,3,3,3,3,3,3,3,3,3,3,3,3,3,3,3,3,3,3,3,3,3,3,3,3,3,3,3,3,3,
3,3,3,3,3,3,3,3,3,3,3,3,4),(10.3390665670415,10.4389102386922,10.5386120657231,
10.6382011799414,10.7377295317413,10.8372284404688,10.9367291874285,11.0363271732773,
11.1359765274803,11.2357929021649,11.3030409577009,11.4034304911592,11.5036806043933,
11.6038203870021,11.7039000735038,11.8039502250711,11.9040013654047,12.0041527633794,
12.1043532357862,12.2047323921906,12.29551609492,12.3956256070617,12.495590671401,
12.5954391831491,12.6952239510319,12.7949759540912,12.8947261306514,12.9945742327021,
13.0944696581655,13.1945443542051,13.2879912321392,13.3882408851107,13.4883478478747,
13.5883402367819,13.6882700202373,13.788167975337,13.8880648394668,13.9880597667956,
14.0881023267245,14.1883229634351,14.2804663693584,14.3807107513822,14.4808127485467,
14.5808006601333,14.6807262662731,14.7806203507897,14.880513658085,14.9805055515609,
15.0805453590138,15.1807637564913,15.2729415065776,15.3376015162611),
 .UNSPECIFIED.);
#1400=B_SPLINE_CURVE_WITH_KNOTS('',3,(#59919,#59920,#59921,#59922,#59923,
#59924,#59925,#59926,#59927,#59928,#59929,#59930,#59931,#59932,#59933,#59934,
#59935,#59936,#59937,#59938,#59939,#59940,#59941,#59942,#59943,#59944,#59945,
#59946,#59947,#59948,#59949,#59950,#59951,#59952,#59953,#59954,#59955,#59956,
#59957,#59958,#59959,#59960,#59961,#59962,#59963,#59964,#59965,#59966,#59967,
#59968,#59969,#59970,#59971,#59972,#59973,#59974,#59975,#59976,#59977,#59978,
#59979,#59980,#59981,#59982,#59983,#59984,#59985,#59986,#59987,#59988,#59989,
#59990,#59991,#59992,#59993,#59994,#59995,#59996,#59997,#59998,#59999,#60000,
#60001,#60002,#60003,#60004,#60005,#60006,#60007,#60008,#60009,#60010,#60011,
#60012,#60013,#60014,#60015,#60016,#60017,#60018,#60019,#60020,#60021,#60022,
#60023,#60024,#60025,#60026,#60027,#60028,#60029,#60030),.UNSPECIFIED.,
 .F.,.F.,(4,3,3,3,3,3,3,3,3,3,3,3,3,3,3,3,3,3,3,3,3,3,3,3,3,3,3,3,3,3,3,
3,3,3,3,3,3,4),(11.652215734785,11.7547070075903,11.8571355266317,11.9595527584582,
12.0619674638986,12.1644046457875,12.2668893252805,12.3695249047339,12.4722399736612,
12.5751521582194,12.6446908720042,12.7439827386589,12.8431176847019,12.9423737252671,
13.0413040056414,13.1401936380512,13.239074595373,13.3385974488356,13.437614586494,
13.5373902978587,13.6371660092234,13.7375076850693,13.8377063835552,13.9377896041002,
14.0378096181711,14.1377970659549,14.2377825472796,14.3378640637924,14.4379922357335,
14.5382958050033,14.6296411464425,14.7300085256656,14.8302468999216,14.9303870192367,
15.0319699674751,15.132021670872,15.2343702415311,15.3367188121902),
 .UNSPECIFIED.);
#1401=B_SPLINE_CURVE_WITH_KNOTS('',3,(#60036,#60037,#60038,#60039,#60040,
#60041,#60042,#60043,#60044,#60045,#60046,#60047,#60048,#60049,#60050,#60051,
#60052,#60053,#60054,#60055,#60056,#60057,#60058,#60059,#60060,#60061,#60062,
#60063,#60064,#60065,#60066,#60067,#60068,#60069,#60070,#60071,#60072,#60073,
#60074,#60075,#60076,#60077,#60078,#60079,#60080,#60081,#60082,#60083,#60084,
#60085,#60086,#60087,#60088,#60089,#60090,#60091,#60092,#60093,#60094,#60095,
#60096,#60097,#60098,#60099,#60100,#60101,#60102,#60103,#60104,#60105,#60106,
#60107,#60108,#60109,#60110,#60111,#60112,#60113,#60114,#60115,#60116,#60117,
#60118,#60119,#60120,#60121,#60122,#60123,#60124,#60125,#60126,#60127,#60128,
#60129,#60130,#60131,#60132,#60133,#60134,#60135,#60136,#60137,#60138,#60139,
#60140,#60141,#60142,#60143,#60144,#60145,#60146,#60147,#60148,#60149,#60150,
#60151,#60152,#60153,#60154,#60155,#60156,#60157,#60158,#60159,#60160,#60161,
#60162,#60163,#60164,#60165,#60166,#60167,#60168,#60169,#60170,#60171,#60172,
#60173,#60174,#60175,#60176,#60177,#60178,#60179,#60180,#60181,#60182,#60183,
#60184,#60185,#60186,#60187,#60188,#60189,#60190,#60191,#60192,#60193,#60194,
#60195,#60196,#60197,#60198,#60199,#60200,#60201,#60202,#60203,#60204,#60205,
#60206,#60207,#60208,#60209,#60210,#60211,#60212,#60213,#60214,#60215,#60216,
#60217,#60218,#60219),.UNSPECIFIED.,.F.,.F.,(4,2,2,2,2,2,2,2,2,2,2,2,2,
2,2,2,2,2,2,2,2,2,2,2,2,2,2,2,2,2,2,2,2,2,2,2,2,2,2,2,2,2,2,2,2,2,2,2,2,
2,2,2,2,2,2,2,2,2,2,2,2,2,2,2,2,2,2,2,2,2,2,2,2,2,2,2,2,2,2,2,2,2,2,2,2,
2,2,2,2,2,2,4),(-1.42848528216476,-1.42739208805283,-1.40622437849851,-1.37846524486598,
-1.34657535696718,-1.33883007564381,-1.33489574589015,-1.33162098640515,
-1.32724990685484,-1.31707848245199,-1.30184135568175,-1.2440054143437,
-1.22640650465069,-1.21930244668961,-1.21340903375455,-1.20728796914555,
-1.19797336948744,-1.16486381749814,-1.13832634160604,-1.10687028411865,
-1.09914870424514,-1.09521904201124,-1.0919435878892,-1.0875655697369,-1.07735263012905,
-1.06202631501776,-1.02701163633883,-0.99072024806915,-0.981091898523054,
-0.974907304539464,-0.968985415790711,-0.960729553647196,-0.93895219195785,
-0.902576709035968,-0.867259014621424,-0.859527123122242,-0.85559532311957,
-0.852649105374209,-0.848472133247894,-0.839432498748516,-0.82652740309081,
-0.781966379937639,-0.750621313112192,-0.74121096101936,-0.735070976584003,
-0.72912287543821,-0.720713336379773,-0.697669608872822,-0.655842253620788,
-0.624860267805108,-0.618726418991694,-0.615124692485654,-0.611749712508817,
-0.606697270805978,-0.59153848349238,-0.526698428947319,-0.507822294607592,
-0.500570464141505,-0.495179109831771,-0.489204942127855,-0.480653259324066,
-0.45636568118876,-0.409544142972789,-0.384772235321615,-0.378832639248688,
-0.37527212144002,-0.371868856187233,-0.366677083966318,-0.350238001381969,
-0.313600705714356,-0.275411889141533,-0.263978910450126,-0.257359804474307,
-0.251621122789868,-0.244348652964047,-0.229148024112924,-0.208004865655459,
-0.180208760771186,-0.148302160491255,-0.140555510837425,-0.136620566999789,
-0.133347468785993,-0.128980844388615,-0.118823328013448,-0.0841312902037792,
-0.0601569568124256,-0.0311100578728027,-0.0219411437467501,-0.0164602522482374,
-0.0109348595217452,-0.00583149434787779,-0.000697598800115113),
 .UNSPECIFIED.);
#1402=B_SPLINE_CURVE_WITH_KNOTS('',3,(#60220,#60221,#60222,#60223,#60224,
#60225,#60226,#60227,#60228,#60229,#60230,#60231,#60232),.UNSPECIFIED.,
 .F.,.F.,(4,3,3,3,4),(15.3376015162611,15.4459524370878,15.5540381009166,
15.6617322199476,15.7079632677065),.UNSPECIFIED.);
#1403=B_SPLINE_CURVE_WITH_KNOTS('',3,(#60234,#60235,#60236,#60237,#60238,
#60239,#60240,#60241,#60242,#60243,#60244,#60245,#60246),.UNSPECIFIED.,
 .F.,.F.,(4,3,3,3,4),(15.3367188121902,15.4369232050171,15.5373043800419,
15.6221162836617,15.7079632679489),.UNSPECIFIED.);
#1404=B_SPLINE_CURVE_WITH_KNOTS('',3,(#60247,#60248,#60249,#60250,#60251,
#60252,#60253,#60254,#60255,#60256,#60257,#60258,#60259,#60260,#60261,#60262,
#60263,#60264,#60265,#60266,#60267,#60268,#60269,#60270,#60271,#60272,#60273,
#60274,#60275,#60276,#60277,#60278,#60279,#60280,#60281,#60282,#60283,#60284,
#60285,#60286,#60287,#60288,#60289,#60290,#60291,#60292,#60293,#60294,#60295,
#60296,#60297,#60298,#60299,#60300,#60301,#60302,#60303,#60304,#60305,#60306,
#60307,#60308,#60309,#60310,#60311,#60312,#60313,#60314,#60315,#60316,#60317,
#60318,#60319,#60320,#60321,#60322,#60323,#60324,#60325,#60326,#60327,#60328,
#60329,#60330,#60331,#60332,#60333,#60334,#60335,#60336,#60337,#60338,#60339,
#60340,#60341,#60342,#60343,#60344,#60345,#60346,#60347,#60348,#60349,#60350,
#60351,#60352,#60353,#60354,#60355,#60356,#60357,#60358,#60359,#60360,#60361,
#60362,#60363,#60364,#60365,#60366,#60367,#60368,#60369,#60370,#60371,#60372,
#60373,#60374,#60375,#60376,#60377,#60378,#60379,#60380,#60381,#60382,#60383,
#60384,#60385,#60386,#60387,#60388,#60389,#60390,#60391,#60392,#60393,#60394,
#60395,#60396,#60397,#60398,#60399,#60400,#60401,#60402,#60403,#60404,#60405,
#60406,#60407,#60408,#60409,#60410,#60411,#60412,#60413,#60414,#60415,#60416,
#60417,#60418,#60419,#60420,#60421,#60422,#60423,#60424,#60425,#60426,#60427,
#60428,#60429,#60430),.UNSPECIFIED.,.F.,.F.,(4,3,3,3,3,3,3,3,3,3,3,3,3,
3,3,3,3,3,3,3,3,3,3,3,3,3,3,3,3,3,3,3,3,3,3,3,3,3,3,3,3,3,3,3,3,3,3,3,3,
3,3,3,3,3,3,3,3,3,3,3,3,4),(15.7079632682029,15.8069001649058,15.9078615719027,
16.0065672226263,16.105223531544,16.2038627572048,16.3065449231238,16.4053067134902,
16.504134708423,16.6031149328184,16.6145914208809,16.7148412113139,16.814948312949,
16.9149408421862,17.0148707667914,17.1147688636603,17.2146658699796,17.3146609391629,
17.4147036409847,17.5149244179969,17.6070665581,17.7073109691657,17.8074129962093,
17.9074009388044,18.0073265766264,18.1072206934565,18.2071140336548,18.3071059607411,
18.4071458022442,18.5073642341291,18.5995416953192,18.6997523138288,18.7998199110768,
18.8997726256092,18.9996625659994,19.0995205661086,19.1993774199548,19.2993325318716,
19.3993353204137,19.4995167269311,19.5920168325384,19.6922477331165,19.7923358882727,
19.8923094785937,19.9922204783603,20.0920996917434,20.1919778832322,20.2919543795833,
20.3919786118565,20.4921813122795,20.5844919697575,20.684720363369,20.7848060235463,
20.8847771493862,20.984685704486,21.0845624965693,21.1844382936973,21.2844124553515,
21.3844343818922,21.4846348531285,21.5769671069767,21.6206806328394),
 .UNSPECIFIED.);
#1405=B_SPLINE_CURVE_WITH_KNOTS('',3,(#60435,#60436,#60437,#60438,#60439,
#60440,#60441,#60442,#60443,#60444,#60445,#60446,#60447,#60448,#60449,#60450,
#60451,#60452,#60453,#60454,#60455,#60456,#60457,#60458,#60459,#60460,#60461,
#60462,#60463,#60464,#60465,#60466,#60467,#60468,#60469,#60470,#60471,#60472,
#60473,#60474,#60475,#60476,#60477,#60478,#60479,#60480,#60481,#60482,#60483,
#60484,#60485,#60486,#60487,#60488,#60489,#60490,#60491,#60492,#60493,#60494,
#60495,#60496,#60497,#60498,#60499,#60500,#60501,#60502,#60503,#60504,#60505,
#60506,#60507,#60508,#60509,#60510,#60511,#60512,#60513,#60514,#60515,#60516,
#60517,#60518,#60519,#60520,#60521,#60522,#60523,#60524,#60525,#60526,#60527,
#60528,#60529,#60530,#60531,#60532,#60533,#60534,#60535,#60536,#60537,#60538,
#60539,#60540,#60541,#60542,#60543,#60544,#60545,#60546,#60547,#60548,#60549,
#60550,#60551,#60552,#60553,#60554,#60555,#60556,#60557,#60558,#60559,#60560,
#60561,#60562,#60563,#60564,#60565,#60566,#60567,#60568,#60569,#60570,#60571,
#60572,#60573,#60574,#60575,#60576,#60577,#60578,#60579,#60580,#60581,#60582,
#60583,#60584,#60585,#60586,#60587,#60588,#60589,#60590,#60591,#60592,#60593,
#60594,#60595,#60596,#60597,#60598,#60599,#60600,#60601,#60602,#60603,#60604,
#60605,#60606,#60607,#60608,#60609,#60610,#60611,#60612,#60613,#60614,#60615,
#60616,#60617,#60618,#60619,#60620,#60621,#60622),.UNSPECIFIED.,.F.,.F.,
(4,2,2,2,2,2,2,2,2,2,2,2,2,2,2,2,2,2,2,2,2,2,2,2,2,2,2,2,2,2,2,2,2,2,2,
2,2,2,2,2,2,2,2,2,2,2,2,2,2,2,2,2,2,2,2,2,2,2,2,2,2,2,2,2,2,2,2,2,2,2,2,
2,2,2,2,2,2,2,2,2,2,2,2,2,2,2,2,2,2,2,2,2,2,4),(-2.94547660919547,-2.92715951863759,
-2.90491281398846,-2.89658309479856,-2.89065023542024,-2.88449051745253,
-2.87497678642284,-2.84188205597475,-2.79891063631364,-2.78017752241277,
-2.77477174139842,-2.77132673082468,-2.76782588801094,-2.76215869957292,
-2.74216853520164,-2.69697053561332,-2.66704132024668,-2.65795951456132,
-2.6518859347408,-2.64596039778645,-2.63734050048888,-2.61435597554483,
-2.5557181451002,-2.53996704981601,-2.53485000233545,-2.53146327982842,
-2.52833043434775,-2.52277723967755,-2.50397545608757,-2.4576406988326,
-2.42746780756053,-2.41836637106877,-2.41228870741671,-2.40636589255893,
-2.39913762629131,-2.38057510656985,-2.32369276554082,-2.30865138491331,
-2.29857321265352,-2.29421807217505,-2.2909749043216,-2.28704487873791,
-2.27931864954599,-2.24397780354891,-2.20761978748256,-2.18591629316678,
-2.17767160516265,-2.17175292792489,-2.16556747572321,-2.15592902911769,
-2.11919719196462,-2.08438688513021,-2.06918249298325,-2.05902805959242,
-2.05466039020284,-2.05138665475765,-2.04745158870617,-2.03969957014487,
-2.00767291423227,-1.97966500619704,-1.94845983158126,-1.93927952133529,
-1.93318607931048,-1.92727499095709,-1.92009479439843,-1.90198554166627,
-1.84450148839802,-1.82946409779941,-1.81938762936905,-1.81503261857501,
-1.81178928627479,-1.80785872123584,-1.80013056578035,-1.7648674211659,
-1.72853639704151,-1.71373626053258,-1.70200281033097,-1.69538864939144,
-1.68959791623671,-1.68229926328989,-1.66693457796284,-1.59028407420276,
-1.57982636048455,-1.57540866172712,-1.57215880505185,-1.56826987461383,
-1.56097542836035,-1.51819938272134,-1.47364490395837,-1.46222720235396,
-1.45561289864828,-1.44987621721666,-1.44260354589539,-1.42848528216476),
 .UNSPECIFIED.);
#1406=B_SPLINE_CURVE_WITH_KNOTS('',3,(#60624,#60625,#60626,#60627,#60628,
#60629,#60630,#60631,#60632,#60633,#60634,#60635,#60636),.UNSPECIFIED.,
 .F.,.F.,(4,3,3,3,4),(21.6206806328394,21.7304850229789,21.8399813708388,
21.9490014055409,21.9911485751285),.UNSPECIFIED.);
#1407=B_SPLINE_CURVE_WITH_KNOTS('',3,(#60637,#60638,#60639,#60640,#60641,
#60642,#60643,#60644,#60645,#60646),.UNSPECIFIED.,.F.,.F.,(4,1,1,1,1,1,
1,4),(21.9911485751285,22.5694422441959,23.5619173814151,24.5543925186342,
25.5468676558534,26.5393427930726,27.5318179302917,27.9042171936241),
 .UNSPECIFIED.);
#1408=B_SPLINE_CURVE_WITH_KNOTS('',3,(#60652,#60653,#60654,#60655,#60656,
#60657,#60658,#60659,#60660,#60661),.UNSPECIFIED.,.F.,.F.,(4,1,1,1,1,1,
1,4),(28.2743423585487,29.1675934276459,30.1600685648651,31.1525437020842,
32.1450188393034,33.1374939765226,34.1299691137418,34.1871485763958),
 .UNSPECIFIED.);
#1409=B_SPLINE_CURVE_WITH_KNOTS('',3,(#60662,#60663,#60664,#60665,#60666,
#60667,#60668,#60669,#60670,#60671,#60672,#60673,#60674,#60675,#60676,#60677,
#60678,#60679),.UNSPECIFIED.,.F.,.F.,(4,2,2,2,2,2,2,2,4),(-3.03482422073094,
-3.02093589767063,-3.01648477335601,-3.01320992380041,-3.01000493469182,
-3.0061869062627,-2.99921991151881,-2.96963288453497,-2.94547660919547),
 .UNSPECIFIED.);
#1410=B_SPLINE_CURVE_WITH_KNOTS('',3,(#60681,#60682,#60683,#60684),
 .UNSPECIFIED.,.F.,.F.,(4,4),(27.9042171936241,28.2743338823081),
 .UNSPECIFIED.);
#1411=B_SPLINE_CURVE_WITH_KNOTS('',3,(#60685,#60686,#60687,#60688,#60689,
#60690,#60691,#60692,#60693,#60694,#60695,#60696,#60697,#60698,#60699,#60700,
#60701,#60702,#60703,#60704,#60705,#60706,#60707,#60708,#60709,#60710,#60711,
#60712,#60713,#60714,#60715,#60716,#60717,#60718,#60719,#60720,#60721,#60722,
#60723,#60724,#60725,#60726,#60727,#60728,#60729,#60730,#60731,#60732,#60733,
#60734,#60735,#60736,#60737,#60738,#60739,#60740,#60741,#60742,#60743,#60744,
#60745,#60746,#60747,#60748,#60749,#60750,#60751,#60752,#60753,#60754,#60755,
#60756,#60757,#60758,#60759,#60760,#60761,#60762,#60763,#60764,#60765,#60766,
#60767,#60768,#60769,#60770,#60771,#60772,#60773,#60774,#60775,#60776,#60777,
#60778,#60779,#60780,#60781,#60782,#60783,#60784,#60785,#60786,#60787,#60788,
#60789,#60790,#60791,#60792,#60793,#60794,#60795,#60796,#60797,#60798,#60799,
#60800,#60801,#60802,#60803,#60804,#60805,#60806,#60807,#60808,#60809,#60810,
#60811,#60812,#60813,#60814,#60815,#60816,#60817,#60818,#60819,#60820,#60821,
#60822,#60823,#60824,#60825,#60826,#60827,#60828,#60829,#60830,#60831,#60832,
#60833,#60834,#60835,#60836,#60837,#60838,#60839,#60840,#60841,#60842,#60843,
#60844,#60845,#60846,#60847,#60848,#60849,#60850,#60851,#60852,#60853,#60854,
#60855,#60856,#60857,#60858,#60859,#60860,#60861,#60862,#60863,#60864,#60865,
#60866,#60867,#60868),.UNSPECIFIED.,.F.,.F.,(4,2,2,2,2,2,2,2,2,2,2,2,2,
2,2,2,2,2,2,2,2,2,2,2,2,2,2,2,2,2,2,2,2,2,2,2,2,2,2,2,2,2,2,2,2,2,2,2,2,
2,2,2,2,2,2,2,2,2,2,2,2,2,2,2,2,2,2,2,2,2,2,2,2,2,2,2,2,2,2,2,2,2,2,2,2,
2,2,2,2,2,2,4),(-3.03525809594091,-2.99530510455854,-2.98648465697967,-2.98153112966352,
-2.97715190408744,-2.97387772211438,-2.96995227776847,-2.96224708361332,
-2.92617184921776,-2.8900353978971,-2.87551811930468,-2.86416755335944,
-2.86355662129243,-2.86297158538743,-2.86240273472369,-2.86184056032287,
-2.8557304818867,-2.8498335138595,-2.84270782976043,-2.82495866459474,-2.76759922190144,
-2.75217560558485,-2.74191930528804,-2.7375352662932,-2.73426049483457,
-2.73033801647843,-2.72288007573829,-2.67560075104725,-2.64679427291659,
-2.62812637763949,-2.62029788425523,-2.61444593320707,-2.6081142940785,
-2.59775935510852,-2.53896765011272,-2.50862575543308,-2.50095197670286,
-2.49703243920211,-2.4937570172262,-2.48944373613989,-2.47973881677227,
-2.4288368497774,-2.40442990828462,-2.38766264458717,-2.3801286386934,-2.374314951281,
-2.36784332257269,-2.35680862029876,-2.28743411801071,-2.2724777429273,
-2.26243907974251,-2.25809030174714,-2.25481791905695,-2.25086890059642,
-2.24328603372607,-2.2069682738424,-2.17025447330345,-2.14947286402478,
-2.14134712036435,-2.13544814062835,-2.12922483550164,-2.1194017489489,
-2.0790861103925,-2.04081829647575,-2.02466899008175,-2.01950918265168,
-2.01611389187263,-2.0125466334586,-2.00657231114134,-1.98087515647114,
-1.9348634158103,-1.91076585898542,-1.9022365321442,-1.89626734347457,-1.89015886705032,
-1.88090381567415,-1.85098553563016,-1.80491683310782,-1.78561302608664,
-1.7801580636809,-1.77670231403423,-1.77363404125072,-1.7684249814729,-1.75308146713379,
-1.70813827133112,-1.68471288182818,-1.66840178175483,-1.66094215067751,
-1.6551360838361,-1.648621777786,-1.63738098762808,-1.60771239371903),
 .UNSPECIFIED.);
#1412=B_SPLINE_CURVE_WITH_KNOTS('',3,(#60874,#60875,#60876,#60877,#60878,
#60879,#60880,#60881,#60882,#60883,#60884,#60885,#60886,#60887,#60888,#60889,
#60890,#60891,#60892,#60893,#60894,#60895,#60896,#60897,#60898,#60899,#60900,
#60901,#60902,#60903,#60904,#60905,#60906,#60907,#60908,#60909,#60910,#60911,
#60912,#60913,#60914,#60915,#60916,#60917,#60918,#60919,#60920,#60921,#60922,
#60923,#60924,#60925,#60926,#60927,#60928,#60929,#60930,#60931,#60932,#60933,
#60934,#60935,#60936,#60937,#60938,#60939,#60940,#60941,#60942,#60943,#60944,
#60945,#60946,#60947,#60948,#60949,#60950,#60951,#60952,#60953,#60954,#60955,
#60956,#60957,#60958,#60959,#60960,#60961,#60962,#60963,#60964,#60965,#60966,
#60967,#60968,#60969,#60970,#60971,#60972,#60973,#60974,#60975,#60976,#60977,
#60978,#60979,#60980,#60981,#60982,#60983,#60984,#60985,#60986,#60987,#60988,
#60989,#60990,#60991,#60992,#60993,#60994,#60995,#60996,#60997,#60998,#60999,
#61000,#61001,#61002,#61003,#61004,#61005,#61006,#61007,#61008,#61009,#61010,
#61011,#61012,#61013,#61014,#61015,#61016,#61017,#61018,#61019,#61020,#61021,
#61022,#61023,#61024,#61025,#61026,#61027,#61028,#61029,#61030,#61031,#61032,
#61033,#61034,#61035,#61036,#61037,#61038,#61039,#61040,#61041,#61042,#61043,
#61044,#61045,#61046,#61047,#61048,#61049),.UNSPECIFIED.,.F.,.F.,(4,2,2,
2,2,2,2,2,2,2,2,2,2,2,2,2,2,2,2,2,2,2,2,2,2,2,2,2,2,2,2,2,2,2,2,2,2,2,2,
2,2,2,2,2,2,2,2,2,2,2,2,2,2,2,2,2,2,2,2,2,2,2,2,2,2,2,2,2,2,2,2,2,2,2,2,
2,2,2,2,2,2,2,2,2,2,2,2,4),(-1.42901813234523,-1.40868918639051,-1.38082821385019,
-1.34889189041069,-1.341142083987,-1.33720611739261,-1.33393038528493,-1.32955850340953,
-1.31938728428427,-1.30415255338032,-1.24562145912397,-1.22847768934837,
-1.22144371224105,-1.21556573631506,-1.20941650070952,-1.19996771526432,
-1.16466995722726,-1.1189272236897,-1.10434979953971,-1.09923082955223,
-1.09617765291173,-1.09269654495528,-1.08712798846818,-1.06640069741722,
-1.01073415151283,-0.99002340742071,-0.981689381315718,-0.975811935944632,
-0.969661929679125,-0.960209201978839,-0.924839737117272,-0.878821125394451,
-0.86452435312988,-0.859440316816066,-0.856092115270448,-0.852509918715487,
-0.846470918604121,-0.816991460743075,-0.756380869664702,-0.745158785979234,
-0.738585376845186,-0.733366636134898,-0.726290996277387,-0.71218053347784,
-0.693147610310051,-0.663078028557834,-0.627038852563289,-0.620813755110829,
-0.617191859349139,-0.61382648714436,-0.608828812233951,-0.594153733754266,
-0.523948374676302,-0.5080485897618,-0.500656679893208,-0.494855961053586,
-0.488298055215494,-0.47684927032268,-0.439193070240063,-0.39611072986621,
-0.384253838712058,-0.379505126310676,-0.376182750311603,-0.372462110122931,
-0.365769912031505,-0.357166039822251,-0.336462832183888,-0.284363510761708,
-0.268386507001057,-0.260981645092294,-0.255179790536097,-0.248630064165351,
-0.237220994085274,-0.199872769812796,-0.157423527947901,-0.144826906813248,
-0.13996128996307,-0.136652652997935,-0.132993966334978,-0.126595094124896,
-0.118483480024856,-0.0613115477139129,-0.0328598753366852,-0.0237337666203509,
-0.0182573289756244,-0.012733045052215,-0.00686466933992766,-0.000717267781909915),
 .UNSPECIFIED.);
#1413=B_SPLINE_CURVE_WITH_KNOTS('',3,(#61050,#61051,#61052,#61053),
 .UNSPECIFIED.,.F.,.F.,(4,4),(34.1871485763958,34.5575142542),
 .UNSPECIFIED.);
#1414=B_SPLINE_CURVE_WITH_KNOTS('',3,(#61054,#61055,#61056,#61057,#61058,
#61059,#61060,#61061,#61062,#61063,#61064,#61065,#61066,#61067,#61068,#61069,
#61070,#61071,#61072,#61073,#61074,#61075,#61076,#61077,#61078,#61079,#61080,
#61081,#61082,#61083,#61084,#61085,#61086,#61087,#61088,#61089,#61090,#61091,
#61092,#61093,#61094,#61095,#61096,#61097,#61098,#61099,#61100,#61101,#61102,
#61103,#61104,#61105,#61106,#61107,#61108,#61109,#61110,#61111,#61112,#61113,
#61114,#61115,#61116,#61117,#61118,#61119,#61120,#61121,#61122,#61123,#61124,
#61125,#61126,#61127,#61128,#61129,#61130,#61131,#61132,#61133,#61134,#61135,
#61136,#61137,#61138,#61139,#61140,#61141,#61142,#61143,#61144,#61145,#61146,
#61147,#61148,#61149,#61150,#61151,#61152,#61153,#61154,#61155,#61156,#61157,
#61158,#61159,#61160,#61161,#61162,#61163,#61164,#61165,#61166,#61167,#61168,
#61169,#61170,#61171,#61172,#61173,#61174,#61175,#61176,#61177,#61178,#61179,
#61180,#61181,#61182,#61183,#61184,#61185,#61186,#61187,#61188,#61189,#61190,
#61191,#61192,#61193,#61194,#61195,#61196,#61197,#61198,#61199,#61200,#61201,
#61202,#61203,#61204,#61205,#61206,#61207,#61208,#61209,#61210,#61211,#61212,
#61213,#61214,#61215,#61216,#61217,#61218,#61219,#61220,#61221,#61222,#61223,
#61224,#61225,#61226,#61227,#61228,#61229,#61230,#61231,#61232,#61233,#61234,
#61235,#61236,#61237,#61238,#61239,#61240,#61241,#61242,#61243,#61244,#61245,
#61246,#61247,#61248,#61249,#61250,#61251),.UNSPECIFIED.,.F.,.F.,(4,2,2,
2,2,2,2,2,2,2,2,2,2,2,2,2,2,2,2,2,2,2,2,2,2,2,2,2,2,2,2,2,2,2,2,2,2,2,2,
2,2,2,2,2,2,2,2,2,2,2,2,2,2,2,2,2,2,2,2,2,2,2,2,2,2,2,2,2,2,2,2,2,2,2,2,
2,2,2,2,2,2,2,2,2,2,2,2,2,2,2,2,2,2,2,2,2,2,2,4),(-1.60771239371903,-1.58563232463443,
-1.54840195198594,-1.54161572852876,-1.53787602866725,-1.5345611530345,
-1.52985711170048,-1.51828242587957,-1.49938915117538,-1.43588506213879,
-1.42514860532117,-1.41873759394151,-1.4129082316278,-1.40525211849731,
-1.38772508560634,-1.36162369375314,-1.32186689920125,-1.30585903271183,
-1.30057415911958,-1.29749198579621,-1.29405362894285,-1.28868192036419,
-1.27034209092257,-1.22935250564103,-1.19401513014059,-1.18441277683645,
-1.17823426950886,-1.17231077052991,-1.1640403669311,-1.14214020236068,
-1.10581254455995,-1.07059933557428,-1.0628655918787,-1.05893380673687,
-1.05565923122297,-1.05128599563974,-1.0410996057581,-1.0258301172431,-0.971066521313685,
-0.951219963718141,-0.943021165674417,-0.937168388556777,-0.930982541490285,
-0.921344042240624,-0.881994264506287,-0.841803736747118,-0.826361613906376,
-0.821140750775315,-0.818070249532416,-0.814617069181905,-0.809174946846298,
-0.790022969790914,-0.74479562126903,-0.714154249915272,-0.70478946959568,
-0.69865879577729,-0.692704804882873,-0.684261284134163,-0.660925791722852,
-0.618006043352791,-0.588440109606404,-0.582325987843649,-0.578728568103269,
-0.575351456241607,-0.570286861002946,-0.555017707422506,-0.491431433983151,
-0.471733119521139,-0.463564449598397,-0.457658213014066,-0.451448529497508,
-0.441692850745728,-0.398778972855953,-0.352020667522152,-0.343940377447059,
-0.339941187063523,-0.337000583153999,-0.332903517818516,-0.324303506431401,
-0.31225617506193,-0.274048395568041,-0.235500715995794,-0.225757784064002,
-0.219550477930858,-0.214058167563003,-0.213409934812446,-0.212873479311974,
-0.212390648398338,-0.211928280322896,-0.211462625087586,-0.205030353579788,
-0.19554681253086,-0.167410218601886,-0.121909949769982,-0.107091260004682,
-0.101943963336318,-0.0988865612075943,-0.0954147961160319,-0.0901927161961946),
 .UNSPECIFIED.);
#1415=B_SPLINE_CURVE_WITH_KNOTS('',3,(#61256,#61257,#61258,#61259,#61260,
#61261,#61262,#61263,#61264,#61265,#61266,#61267,#61268,#61269,#61270,#61271,
#61272,#61273,#61274,#61275,#61276,#61277,#61278,#61279,#61280,#61281,#61282,
#61283,#61284,#61285,#61286,#61287,#61288,#61289,#61290,#61291,#61292,#61293,
#61294,#61295,#61296,#61297,#61298,#61299,#61300,#61301,#61302,#61303,#61304,
#61305,#61306,#61307,#61308,#61309,#61310,#61311,#61312,#61313,#61314,#61315,
#61316,#61317,#61318,#61319,#61320,#61321,#61322,#61323,#61324,#61325,#61326,
#61327,#61328,#61329,#61330,#61331,#61332,#61333,#61334,#61335,#61336,#61337,
#61338,#61339,#61340,#61341,#61342,#61343,#61344,#61345,#61346,#61347,#61348,
#61349,#61350,#61351,#61352,#61353,#61354,#61355,#61356,#61357,#61358,#61359,
#61360,#61361,#61362,#61363,#61364,#61365,#61366,#61367,#61368,#61369,#61370,
#61371,#61372,#61373,#61374,#61375,#61376,#61377,#61378,#61379,#61380,#61381,
#61382,#61383,#61384,#61385,#61386,#61387,#61388,#61389,#61390,#61391,#61392,
#61393,#61394,#61395,#61396,#61397,#61398,#61399,#61400,#61401,#61402,#61403,
#61404,#61405,#61406,#61407,#61408,#61409,#61410,#61411,#61412,#61413,#61414,
#61415,#61416,#61417,#61418,#61419,#61420,#61421,#61422,#61423,#61424,#61425,
#61426,#61427,#61428,#61429,#61430,#61431,#61432,#61433,#61434,#61435,#61436,
#61437,#61438,#61439,#61440,#61441,#61442,#61443,#61444,#61445,#61446,#61447,
#61448,#61449),.UNSPECIFIED.,.F.,.F.,(4,2,2,2,2,2,2,2,2,2,2,2,2,2,2,2,2,
2,2,2,2,2,2,2,2,2,2,2,2,2,2,2,2,2,2,2,2,2,2,2,2,2,2,2,2,2,2,2,2,2,2,2,2,
2,2,2,2,2,2,2,2,2,2,2,2,2,2,2,2,2,2,2,2,2,2,2,2,2,2,2,2,2,2,2,2,2,2,2,2,
2,2,2,2,2,2,2,4),(-2.94656220223364,-2.93107157250197,-2.90797912015355,
-2.89956315218436,-2.89361301984311,-2.88747302235605,-2.87806691297442,
-2.84680988552935,-2.80210780122725,-2.78918075954208,-2.78013051841647,
-2.77595108272143,-2.77300427068659,-2.769073291396,-2.76134674760497,-2.72586603616624,
-2.68944658537902,-2.66786572504297,-2.65963455908693,-2.65371651274769,
-2.64826260731479,-2.63926585838981,-2.61243376898799,-2.56330187262677,
-2.54348931356536,-2.53799166875045,-2.53452607891713,-2.53146302746631,
-2.52628695963156,-2.51123270060586,-2.46600501977972,-2.43085657052876,
-2.42141802421395,-2.41527132918213,-2.4093928232568,-2.40235459270603,
-2.38486164014381,-2.32665822285386,-2.31141090628959,-2.30123502262828,
-2.29686257175623,-2.29358707646706,-2.28965212164009,-2.28190641247196,
-2.25002586350779,-2.22226666793862,-2.19066748122149,-2.1814552974564,
-2.17535354957512,-2.16944379043507,-2.16227684142528,-2.14427713905496,
-2.08659909619292,-2.07155602553697,-2.06147548744532,-2.05711855501576,
-2.05387373706919,-2.04994131688916,-2.04220931722343,-2.00694322932635,
-1.97060118404076,-1.94879031191285,-1.94052920568066,-1.93460536335289,
-1.92842030129443,-1.91879467064947,-1.88279554603591,-1.84737247307824,
-1.83204383725341,-1.82182992023604,-1.8174510865857,-1.81417488392062,
-1.81024405432679,-1.80252001829571,-1.77103674633988,-1.74439987043636,
-1.71143818871409,-1.70213193664404,-1.69601123128642,-1.69011443012222,
-1.68166983281236,-1.66016213402194,-1.60536671541315,-1.59139282959725,
-1.58182324519615,-1.57755228477352,-1.57459623208069,-1.57073230872319,
-1.56355882476752,-1.51875550452783,-1.47603426478969,-1.46459152267197,
-1.45797059449349,-1.45223271153204,-1.44496454922729,-1.42978686594534,
-1.42901813234523),.UNSPECIFIED.);
#1416=B_SPLINE_CURVE_WITH_KNOTS('',3,(#61451,#61452,#61453,#61454,#61455,
#61456,#61457,#61458),.UNSPECIFIED.,.F.,.F.,(4,2,2,4),(-0.0901927161961946,
-0.0898859350082424,-0.0696626742519121,-0.00069517407964766),
 .UNSPECIFIED.);
#1417=B_SPLINE_CURVE_WITH_KNOTS('',3,(#61459,#61460,#61461,#61462,#61463,
#61464,#61465,#61466,#61467,#61468,#61469,#61470,#61471,#61472,#61473,#61474,
#61475,#61476,#61477,#61478,#61479,#61480,#61481,#61482,#61483,#61484,#61485,
#61486,#61487,#61488,#61489,#61490,#61491,#61492,#61493,#61494,#61495,#61496,
#61497,#61498,#61499,#61500,#61501,#61502,#61503,#61504,#61505,#61506,#61507,
#61508,#61509,#61510,#61511,#61512,#61513,#61514,#61515,#61516,#61517,#61518,
#61519,#61520,#61521,#61522,#61523,#61524,#61525,#61526,#61527,#61528,#61529,
#61530,#61531,#61532,#61533,#61534,#61535,#61536,#61537,#61538,#61539,#61540,
#61541,#61542,#61543,#61544,#61545,#61546,#61547,#61548,#61549,#61550,#61551,
#61552,#61553,#61554,#61555,#61556,#61557,#61558,#61559,#61560,#61561,#61562,
#61563,#61564,#61565,#61566,#61567,#61568,#61569,#61570,#61571,#61572,#61573,
#61574,#61575,#61576,#61577,#61578,#61579,#61580,#61581,#61582,#61583,#61584,
#61585,#61586,#61587,#61588,#61589,#61590,#61591,#61592,#61593,#61594,#61595,
#61596,#61597,#61598,#61599,#61600,#61601,#61602,#61603,#61604,#61605,#61606,
#61607,#61608,#61609,#61610,#61611,#61612,#61613,#61614,#61615,#61616,#61617,
#61618,#61619,#61620,#61621,#61622,#61623,#61624,#61625,#61626,#61627,#61628,
#61629,#61630,#61631,#61632,#61633,#61634,#61635,#61636),.UNSPECIFIED.,
 .F.,.F.,(4,2,2,2,2,2,2,2,2,2,2,2,2,2,2,2,2,2,2,2,2,2,2,2,2,2,2,2,2,2,2,
2,2,2,2,2,2,2,2,2,2,2,2,2,2,2,2,2,2,2,2,2,2,2,2,2,2,2,2,2,2,2,2,2,2,2,2,
2,2,2,2,2,2,2,2,2,2,2,2,2,2,2,2,2,2,2,2,2,4),(-3.03528425599135,-3.02396005249311,
-3.01821358683809,-3.01268720184321,-3.00720482041017,-2.9980336783293,
-2.96896968647659,-2.91266369537032,-2.90953754827863,-2.89989664775877,
-2.89561540810208,-2.89266009869233,-2.88880857383738,-2.88168501434852,
-2.83631742787498,-2.79315532775536,-2.7821219362015,-2.77565119907522,
-2.76983832760626,-2.76243075545287,-2.74594381814187,-2.69436048568999,
-2.66411404658158,-2.65805087440207,-2.65446504640402,-2.65112268622414,
-2.64606135836705,-2.63192637368942,-2.5907630621108,-2.55335300487471,
-2.54241432349103,-2.53596270165716,-2.53014505464891,-2.52270124197044,
-2.50599231645271,-2.44587343122491,-2.43085503741057,-2.42078758064652,
-2.41643436596033,-2.41316199265588,-2.40921708739238,-2.40165258090245,
-2.36512766873907,-2.32834068630927,-2.30775772511052,-2.29965912861901,
-2.293765156788,-2.28753392246816,-2.27766950112804,-2.23660984209929,-2.20052138600566,
-2.18326929602024,-2.17799890007728,-2.17458178139168,-2.17148161467711,
-2.1660987422454,-2.14916956010022,-2.10573551548009,-2.07107094692933,
-2.0616631535585,-2.05552465527732,-2.04964565738719,-2.04259683073055,
-2.02501647593209,-1.96660132232056,-1.95156915718805,-1.94149507868237,
-1.93714063149586,-1.93389759071763,-1.92996737037985,-1.92224003247172,
-1.89064639072072,-1.86367457468669,-1.83113425382627,-1.82185942249268,
-1.81574723687957,-1.80984992834648,-1.8027259133918,-1.78499279174484,
-1.72694380532815,-1.71190772053385,-1.7018315967207,-1.69747662867949,
-1.69420376659426,-1.69025928797621,-1.68269818608245,-1.64605070440242,
-1.60921153310692,-1.60751603659748),.UNSPECIFIED.);
#1418=B_SPLINE_CURVE_WITH_KNOTS('',3,(#61642,#61643,#61644,#61645,#61646,
#61647,#61648,#61649,#61650,#61651,#61652,#61653,#61654,#61655,#61656,#61657,
#61658,#61659,#61660,#61661,#61662,#61663,#61664,#61665,#61666,#61667,#61668,
#61669,#61670,#61671,#61672,#61673,#61674,#61675,#61676,#61677,#61678,#61679,
#61680,#61681,#61682,#61683,#61684,#61685,#61686,#61687,#61688,#61689,#61690,
#61691,#61692,#61693,#61694,#61695,#61696,#61697,#61698,#61699,#61700,#61701,
#61702,#61703,#61704,#61705,#61706,#61707,#61708,#61709,#61710,#61711,#61712,
#61713,#61714,#61715,#61716,#61717,#61718,#61719,#61720,#61721,#61722,#61723,
#61724,#61725,#61726,#61727,#61728,#61729,#61730,#61731,#61732,#61733,#61734,
#61735,#61736,#61737,#61738,#61739,#61740,#61741,#61742,#61743,#61744,#61745,
#61746,#61747,#61748,#61749,#61750,#61751,#61752,#61753,#61754,#61755,#61756,
#61757,#61758,#61759,#61760,#61761,#61762,#61763,#61764,#61765,#61766,#61767,
#61768,#61769,#61770,#61771,#61772,#61773,#61774,#61775,#61776,#61777,#61778,
#61779,#61780,#61781,#61782,#61783,#61784,#61785,#61786,#61787,#61788,#61789,
#61790,#61791,#61792,#61793,#61794,#61795,#61796,#61797,#61798,#61799,#61800,
#61801,#61802,#61803,#61804,#61805,#61806,#61807,#61808,#61809,#61810,#61811,
#61812,#61813,#61814,#61815,#61816,#61817,#61818,#61819,#61820,#61821,#61822,
#61823,#61824,#61825,#61826,#61827,#61828,#61829,#61830,#61831,#61832,#61833,
#61834,#61835,#61836,#61837,#61838,#61839,#61840,#61841,#61842,#61843,#61844,
#61845,#61846,#61847,#61848,#61849,#61850,#61851,#61852,#61853,#61854,#61855,
#61856,#61857,#61858,#61859,#61860,#61861,#61862,#61863,#61864,#61865,#61866,
#61867,#61868,#61869,#61870,#61871,#61872,#61873,#61874,#61875,#61876,#61877,
#61878,#61879,#61880,#61881,#61882,#61883,#61884,#61885),.UNSPECIFIED.,
 .F.,.F.,(4,2,2,2,2,2,2,2,2,2,2,2,2,2,2,2,2,2,2,2,2,2,2,2,2,2,2,2,2,2,2,
2,2,2,2,2,2,2,2,2,2,2,2,2,2,2,2,2,2,2,2,2,2,2,2,2,2,2,2,2,2,2,2,2,2,2,2,
2,2,2,2,2,2,2,2,2,2,2,2,2,2,2,2,2,2,2,2,2,2,2,2,2,2,2,2,2,2,2,2,2,2,2,2,
2,2,2,2,2,2,2,2,2,2,2,2,2,2,2,2,2,2,4),(-1.42845108479066,-1.42143216311403,
-1.41758627357992,-1.41462899073518,-1.41033661236475,-1.40063413152217,
-1.38638506044704,-1.32809077973996,-1.30963254464462,-1.30241329235493,
-1.29649229261596,-1.29041096578148,-1.28129322476405,-1.25092988990403,
-1.20375959232591,-1.18578806005888,-1.18030639936041,-1.17718711163717,
-1.17378764847098,-1.16860727252622,-1.1522584519666,-1.11493846960333,
-1.07414430063867,-1.0642556710435,-1.05801878957064,-1.05212596392673,
-1.0440393376434,-1.02355317112203,-0.986690161992489,-0.950047148183531,
-0.942483440886864,-0.938538274846616,-0.93526514916804,-0.930910167126929,
-0.920834734191991,-0.905801979162551,-0.848912044381502,-0.830386547693013,
-0.823161212722347,-0.81723851696378,-0.811158738900404,-0.802049809877046,
-0.77180323958155,-0.72518152112645,-0.706622602390665,-0.701090568418409,
-0.697961487151243,-0.694570508182388,-0.689433808381316,-0.673502902656044,
-0.63446189318228,-0.59460958159339,-0.584851694904917,-0.578641341993393,
-0.572734876945046,-0.564566503029301,-0.543465588412021,-0.506842146047196,
-0.470918783349053,-0.463173005355096,-0.459238741253637,-0.455964220132156,
-0.451593684452382,-0.441424450938279,-0.426191495766157,-0.368087255942739,
-0.350576365455206,-0.343536975728104,-0.337659312475759,-0.331515422549332,
-0.322085271345438,-0.287068915929982,-0.242361170518768,-0.226738444819332,
-0.221496770065138,-0.218422374284001,-0.215084828686073,-0.215047741239131,
-0.215011024064946,-0.214974615849982,-0.214938457914119,-0.214902493739294,
-0.214866668611279,-0.214830929268752,-0.214795223557888,-0.21475950011054,
-0.2147237079959,-0.214687796485903,-0.214651714799997,-0.21461541177425,
-0.214578835577679,-0.214541933469283,-0.214504651522058,-0.214466934257536,
-0.214428724394927,-0.214389962543958,-0.214350586853511,-0.214310532635308,
-0.214269731962686,-0.214228113321684,-0.214185601096374,-0.214142115101583,
-0.214097570059814,-0.214051874961794,-0.214004932461522,-0.2139566381116,
-0.213906879592602,-0.213855535806203,-0.21380247587604,-0.213747558012905,
-0.213690628277317,-0.209633536400428,-0.203161230754096,-0.18992986547316,
-0.142565256877873,-0.114263719858855,-0.10501542840349,-0.0989078195222654,
-0.0929367070542661,-0.08439970750449,-0.0602410135355151,-0.000695333887311579),
 .UNSPECIFIED.);
#1419=B_SPLINE_CURVE_WITH_KNOTS('',3,(#61886,#61887,#61888,#61889,#61890,
#61891,#61892,#61893,#61894,#61895,#61896,#61897,#61898,#61899,#61900,#61901,
#61902,#61903),.UNSPECIFIED.,.F.,.F.,(4,2,2,2,2,2,2,2,4),(-3.03596232598265,
-3.02651077198456,-3.0199354130703,-3.01655933429411,-3.0134607107987,-3.00984676424624,
-3.00365792931449,-2.97487168403078,-2.94656220223364),.UNSPECIFIED.);
#1420=B_SPLINE_CURVE_WITH_KNOTS('',3,(#61904,#61905,#61906,#61907,#61908,
#61909,#61910,#61911,#61912,#61913,#61914,#61915,#61916,#61917,#61918,#61919,
#61920,#61921,#61922,#61923,#61924,#61925,#61926,#61927,#61928,#61929,#61930,
#61931,#61932,#61933,#61934,#61935,#61936,#61937,#61938,#61939,#61940,#61941,
#61942,#61943,#61944,#61945,#61946,#61947,#61948,#61949,#61950,#61951,#61952,
#61953,#61954,#61955,#61956,#61957,#61958,#61959,#61960,#61961,#61962,#61963,
#61964,#61965,#61966,#61967,#61968,#61969,#61970,#61971,#61972,#61973,#61974,
#61975,#61976,#61977,#61978,#61979,#61980,#61981,#61982,#61983,#61984,#61985,
#61986,#61987,#61988,#61989,#61990,#61991,#61992,#61993,#61994,#61995,#61996,
#61997,#61998,#61999,#62000,#62001,#62002,#62003,#62004,#62005,#62006,#62007,
#62008,#62009,#62010,#62011,#62012,#62013,#62014,#62015,#62016,#62017,#62018,
#62019,#62020,#62021,#62022,#62023,#62024,#62025,#62026,#62027,#62028,#62029,
#62030,#62031,#62032,#62033,#62034,#62035,#62036,#62037,#62038,#62039,#62040,
#62041,#62042,#62043,#62044,#62045,#62046,#62047,#62048,#62049,#62050,#62051,
#62052,#62053,#62054,#62055,#62056,#62057,#62058,#62059,#62060,#62061,#62062,
#62063,#62064,#62065,#62066,#62067,#62068,#62069,#62070,#62071,#62072,#62073,
#62074,#62075,#62076,#62077,#62078,#62079,#62080,#62081,#62082,#62083,#62084,
#62085,#62086,#62087,#62088,#62089,#62090,#62091,#62092,#62093),
 .UNSPECIFIED.,.F.,.F.,(4,2,2,2,2,2,2,2,2,2,2,2,2,2,2,2,2,2,2,2,2,2,2,2,
2,2,2,2,2,2,2,2,2,2,2,2,2,2,2,2,2,2,2,2,2,2,2,2,2,2,2,2,2,2,2,2,2,2,2,2,
2,2,2,2,2,2,2,2,2,2,2,2,2,2,2,2,2,2,2,2,2,2,2,2,2,2,2,2,2,2,2,2,2,2,4),
(-1.60751603659748,-1.58874532652916,-1.58066179055868,-1.57476972114249,
-1.56853232732708,-1.55864024971192,-1.51777931087869,-1.47422828083003,
-1.46293308922925,-1.45872534371252,-1.45538855481355,-1.4517907796266,
-1.44567437905709,-1.41366240458484,-1.35715132647057,-1.3451507595116,
-1.33841407579451,-1.332635186044,-1.325505690886,-1.31109072274315,-1.30042488523193,
-1.26413623461994,-1.22902332242951,-1.22128859974243,-1.21735681476033,
-1.21408253849505,-1.20971009489354,-1.19952721966985,-1.18426474873691,
-1.12895382027006,-1.10947073894241,-1.10215417084762,-1.09674867171552,
-1.09079194128018,-1.08233060087535,-1.05883566297541,-1.01529488135641,
-0.986525026668314,-0.980431659506431,-0.976838923648086,-0.973459632044182,
-0.968382285070097,-0.952995474299193,-0.890659216879083,-0.870185227995624,
-0.861887667860104,-0.856018736833323,-0.849862886221126,-0.840370460046385,
-0.804199345277004,-0.754971655366581,-0.743821264141982,-0.739626202596394,
-0.736292707079823,-0.732689325679836,-0.726546268582389,-0.693476016035368,
-0.634875141860273,-0.624498461368961,-0.618161942184082,-0.612310847809796,
-0.604491688982575,-0.585891656639177,-0.557251531090971,-0.51053376052804,
-0.502422381453692,-0.498417586841131,-0.495477764859172,-0.491388083729115,
-0.482826022098898,-0.470850881481872,-0.433118132058109,-0.393905080040855,
-0.384200422285627,-0.378001527108626,-0.372090363869801,-0.363889938682951,
-0.342536814621959,-0.306012053221888,-0.270412825170174,-0.262603496706861,
-0.258657115929539,-0.255384558852583,-0.251032545615987,-0.240973516492402,
-0.22597559994144,-0.16429582581797,-0.148658257254241,-0.141312948541282,
-0.135518707487021,-0.128936309828955,-0.117358294392849,-0.112633652509009,
-0.0992878568064811,-0.0901262604413663),.UNSPECIFIED.);
#1421=B_SPLINE_CURVE_WITH_KNOTS('',3,(#62098,#62099,#62100,#62101,#62102,
#62103,#62104,#62105,#62106,#62107,#62108,#62109,#62110,#62111,#62112,#62113,
#62114,#62115,#62116,#62117,#62118,#62119,#62120,#62121,#62122,#62123,#62124,
#62125,#62126,#62127,#62128,#62129,#62130,#62131,#62132,#62133,#62134,#62135,
#62136,#62137,#62138,#62139,#62140,#62141,#62142,#62143,#62144,#62145,#62146,
#62147,#62148,#62149,#62150,#62151,#62152,#62153,#62154,#62155,#62156,#62157,
#62158,#62159,#62160,#62161,#62162,#62163,#62164,#62165,#62166,#62167,#62168,
#62169,#62170,#62171,#62172,#62173,#62174,#62175,#62176,#62177,#62178,#62179,
#62180,#62181,#62182,#62183,#62184,#62185,#62186,#62187,#62188,#62189,#62190,
#62191,#62192,#62193,#62194,#62195,#62196,#62197,#62198,#62199,#62200,#62201,
#62202,#62203,#62204,#62205,#62206,#62207,#62208,#62209,#62210,#62211,#62212,
#62213,#62214,#62215,#62216,#62217,#62218,#62219,#62220,#62221,#62222,#62223,
#62224,#62225,#62226,#62227,#62228,#62229,#62230,#62231,#62232,#62233,#62234,
#62235,#62236,#62237,#62238,#62239,#62240,#62241,#62242,#62243,#62244,#62245,
#62246,#62247,#62248,#62249,#62250,#62251,#62252,#62253,#62254,#62255,#62256,
#62257,#62258,#62259,#62260,#62261,#62262,#62263,#62264,#62265,#62266,#62267,
#62268,#62269,#62270,#62271,#62272,#62273,#62274,#62275,#62276,#62277,#62278,
#62279,#62280,#62281,#62282,#62283,#62284,#62285,#62286,#62287,#62288,#62289,
#62290,#62291,#62292,#62293,#62294,#62295,#62296,#62297,#62298,#62299,#62300,
#62301,#62302,#62303,#62304,#62305,#62306,#62307,#62308,#62309,#62310,#62311,
#62312,#62313,#62314,#62315,#62316,#62317,#62318,#62319,#62320,#62321,#62322,
#62323,#62324,#62325,#62326,#62327,#62328,#62329,#62330,#62331,#62332,#62333,
#62334,#62335,#62336,#62337,#62338,#62339,#62340,#62341,#62342,#62343,#62344,
#62345,#62346,#62347,#62348,#62349,#62350,#62351,#62352,#62353,#62354,#62355,
#62356,#62357,#62358,#62359,#62360,#62361,#62362,#62363,#62364,#62365,#62366,
#62367,#62368,#62369),.UNSPECIFIED.,.F.,.F.,(4,2,2,2,2,2,2,2,2,2,2,2,2,
2,2,2,2,2,2,2,2,2,2,2,2,2,2,2,2,2,2,2,2,2,2,2,2,2,2,2,2,2,2,2,2,2,2,2,2,
2,2,2,2,2,2,2,2,2,2,2,2,2,2,2,2,2,2,2,2,2,2,2,2,2,2,2,2,2,2,2,2,2,2,2,2,
2,2,2,2,2,2,2,2,2,2,2,2,2,2,2,2,2,2,2,2,2,2,2,2,2,2,2,2,2,2,2,2,2,2,2,2,
2,2,2,2,2,2,2,2,2,2,2,2,2,2,4),(-2.94522627611978,-2.9278260567548,-2.88209537165937,
-2.86904939939296,-2.86022824290779,-2.86012762899294,-2.86003321938999,
-2.85994447229088,-2.85986090262605,-2.85978207532565,-2.85970759940869,
-2.85963712287195,-2.85957032823019,-2.85950692860159,-2.85944666427833,
-2.85938929973542,-2.85933462101949,-2.85928243343705,-2.85923255950263,
-2.85918483717171,-2.85913911825154,-2.85909526696991,-2.85905315881138,
-2.85901267931485,-2.85897372316421,-2.85893619334639,-2.85890000029291,
-2.85886506119732,-2.85883129945282,-2.85879864407773,-2.8587670291803,
-2.85873639351689,-2.85870668014095,-2.85867783597254,-2.85858012111323,
-2.85848407999915,-2.85838959708076,-2.85829656093362,-2.85820486387315,
-2.85811440161406,-2.85802507290806,-2.85793677919645,-2.85784942430879,
-2.85776291410638,-2.85767715617137,-2.85759205950617,-2.85750753421965,
-2.85742349117799,-2.85733984171817,-2.85725649731425,-2.85383273884977,
-2.85073935320882,-2.84539135417927,-2.82879005941319,-2.78506671315378,
-2.7503379832641,-2.74092770273516,-2.73478915674464,-2.72891117263452,
-2.72055647766217,-2.69967501603011,-2.64635493763055,-2.63106082520032,
-2.62086499746477,-2.61649090726033,-2.61321702191833,-2.60928746787096,
-2.60156184225795,-2.56625414439879,-2.52991195498661,-2.50818290104245,
-2.49993578941481,-2.49401735709842,-2.48783389766611,-2.47820222356469,
-2.44171333151579,-2.40688756654073,-2.39154852184529,-2.38133183481815,
-2.37695436121585,-2.37368021593805,-2.36975312446663,-2.36203988399547,
-2.3260237310847,-2.28940604106807,-2.26841192383277,-2.26025943828437,
-2.25435699980941,-2.24814421656735,-2.23836824285325,-2.19833688616145,
-2.15956242226595,-2.14356056535607,-2.1384171183554,-2.13502554231489,
-2.13145433008986,-2.12545931626638,-2.0992411852945,-2.05369650959472,
-2.02971447160205,-2.02119947198221,-2.015233819974,-2.00983895352222,-2.00256536460833,
-1.98340947856826,-1.91892515319589,-1.90375492269643,-1.89870201804694,
-1.89532764781893,-1.89172731317724,-1.8855974912203,-1.85473878782276,
-1.81289030001618,-1.79728601394542,-1.78508095864178,-1.77837300077994,
-1.77259256650636,-1.76542740239465,-1.7540931702843,-1.6980986404642,-1.66626321796789,
-1.66015138432425,-1.65655478368268,-1.65321763512158,-1.64818631853087,
-1.63428879976942,-1.59294087438025,-1.56624837414105,-1.54846438275313,
-1.54076878823646,-1.53493448118191,-1.52854257305925,-1.51789811129468,
-1.47428171580287,-1.42852668002049,-1.42845108479066),.UNSPECIFIED.);
#1422=B_SPLINE_CURVE_WITH_KNOTS('',3,(#62371,#62372,#62373,#62374,#62375,
#62376,#62377,#62378,#62379,#62380,#62381,#62382,#62383,#62384,#62385,#62386,
#62387,#62388),.UNSPECIFIED.,.F.,.F.,(4,2,2,2,2,2,2,2,4),(-0.0901262604413663,
-0.050740347091941,-0.0273583609058817,-0.0214867594294149,-0.0179417442508245,
-0.0148777648982165,-0.0114578850196497,-0.00665285670582603,-0.000694003661653763),
 .UNSPECIFIED.);
#1423=B_SPLINE_CURVE_WITH_KNOTS('',3,(#62389,#62390,#62391,#62392,#62393,
#62394,#62395,#62396,#62397,#62398,#62399,#62400,#62401,#62402,#62403,#62404,
#62405,#62406,#62407,#62408,#62409,#62410,#62411,#62412,#62413,#62414,#62415,
#62416,#62417,#62418,#62419,#62420,#62421,#62422,#62423,#62424,#62425,#62426,
#62427,#62428,#62429,#62430,#62431,#62432,#62433,#62434,#62435,#62436,#62437,
#62438,#62439,#62440,#62441,#62442,#62443,#62444,#62445,#62446,#62447,#62448,
#62449,#62450,#62451,#62452,#62453,#62454,#62455,#62456,#62457,#62458,#62459,
#62460,#62461,#62462,#62463,#62464,#62465,#62466,#62467,#62468,#62469,#62470,
#62471,#62472,#62473,#62474,#62475,#62476,#62477,#62478,#62479,#62480,#62481,
#62482,#62483,#62484,#62485,#62486,#62487,#62488,#62489,#62490,#62491,#62492,
#62493,#62494,#62495,#62496,#62497,#62498,#62499,#62500,#62501,#62502,#62503,
#62504,#62505,#62506,#62507,#62508,#62509,#62510,#62511,#62512,#62513,#62514,
#62515,#62516,#62517,#62518,#62519,#62520,#62521,#62522,#62523,#62524,#62525,
#62526,#62527,#62528,#62529,#62530,#62531,#62532,#62533,#62534,#62535,#62536,
#62537,#62538,#62539,#62540,#62541,#62542,#62543,#62544,#62545,#62546,#62547,
#62548,#62549,#62550,#62551,#62552,#62553,#62554,#62555,#62556,#62557,#62558,
#62559,#62560,#62561,#62562,#62563,#62564,#62565,#62566,#62567,#62568,#62569,
#62570,#62571,#62572,#62573,#62574,#62575,#62576),.UNSPECIFIED.,.F.,.F.,
(4,2,2,2,2,2,2,2,2,2,2,2,2,2,2,2,2,2,2,2,2,2,2,2,2,2,2,2,2,2,2,2,2,2,2,
2,2,2,2,2,2,2,2,2,2,2,2,2,2,2,2,2,2,2,2,2,2,2,2,2,2,2,2,2,2,2,2,2,2,2,2,
2,2,2,2,2,2,2,2,2,2,2,2,2,2,2,2,2,2,2,2,2,2,4),(-3.03589799970467,-2.96791287576106,
-2.94642853128536,-2.93821240019877,-2.9322992873552,-2.92610657953658,
-2.91642922553783,-2.87792590980494,-2.83954868038511,-2.82747534841312,
-2.82138142172164,-2.81663901184802,-2.81658441314679,-2.81652992760057,
-2.81647543426394,-2.81642080975002,-2.81636592706931,-2.81631065435479,
-2.81625485339372,-2.81619837807209,-2.81614107252712,-2.81285634926421,
-2.80972862790769,-2.80420060556432,-2.78567240527661,-2.73906801988853,
-2.70883636433632,-2.69973082199681,-2.69365288502093,-2.68773168954697,
-2.67913387965057,-2.65635436189848,-2.59742774031163,-2.58168715932836,
-2.57657140156469,-2.57318509837418,-2.56960525170644,-2.56357058263477,
-2.53641413385352,-2.49162411804925,-2.46782118015233,-2.45932583692511,
-2.45336353629828,-2.44796493891926,-2.43927785077053,-2.41560691348531,
-2.3579385945619,-2.3420625666281,-2.33693207651549,-2.33354278861617,-2.33041318804702,
-2.32487656379686,-2.30625418978656,-2.25973167709141,-2.22951546843293,
-2.22041043080765,-2.21433214480538,-2.20841010130841,-2.19981013459804,
-2.17701671024055,-2.11810053533784,-2.10235656187319,-2.0972400808126,
-2.09385338721421,-2.09027322517966,-2.08423819901111,-2.057085677852,-2.01228541589481,
-1.98847862929008,-1.97998224450321,-1.97401929301848,-1.96862015868814,
-1.96133062537079,-1.94203652545307,-1.87774036954437,-1.86252795889626,
-1.85746971663518,-1.85409396628481,-1.850494706891,-1.84437158094169,-1.81423392915018,
-1.771808614623,-1.74860644240584,-1.74017899290998,-1.73422803031838,-1.72881577049308,
-1.72005282703135,-1.6955874318218,-1.64400095612153,-1.62381968244339,
-1.61829389179362,-1.61482292791769,-1.61176524667919,-1.60794378585001),
 .UNSPECIFIED.);
#1424=B_SPLINE_CURVE_WITH_KNOTS('',3,(#62582,#62583,#62584,#62585,#62586,
#62587,#62588,#62589,#62590,#62591,#62592,#62593,#62594,#62595,#62596,#62597,
#62598,#62599,#62600,#62601,#62602,#62603,#62604,#62605,#62606,#62607,#62608,
#62609,#62610,#62611,#62612,#62613,#62614,#62615,#62616,#62617,#62618,#62619,
#62620,#62621,#62622,#62623,#62624,#62625,#62626,#62627,#62628,#62629,#62630,
#62631,#62632,#62633,#62634,#62635,#62636,#62637,#62638,#62639,#62640,#62641,
#62642,#62643,#62644,#62645,#62646,#62647,#62648,#62649,#62650,#62651,#62652,
#62653,#62654,#62655,#62656,#62657,#62658,#62659,#62660,#62661,#62662,#62663,
#62664,#62665,#62666,#62667,#62668,#62669,#62670,#62671,#62672,#62673,#62674,
#62675,#62676,#62677,#62678,#62679,#62680,#62681,#62682,#62683,#62684,#62685,
#62686,#62687,#62688,#62689,#62690,#62691,#62692,#62693,#62694,#62695,#62696,
#62697,#62698,#62699,#62700,#62701,#62702,#62703,#62704,#62705,#62706,#62707,
#62708,#62709,#62710,#62711,#62712,#62713,#62714,#62715,#62716,#62717,#62718,
#62719,#62720,#62721,#62722,#62723,#62724,#62725,#62726,#62727,#62728,#62729,
#62730,#62731,#62732,#62733,#62734,#62735,#62736,#62737,#62738,#62739,#62740,
#62741,#62742,#62743,#62744,#62745,#62746,#62747,#62748,#62749,#62750,#62751,
#62752,#62753,#62754,#62755,#62756,#62757,#62758,#62759,#62760,#62761,#62762,
#62763,#62764,#62765,#62766,#62767,#62768,#62769,#62770,#62771,#62772,#62773,
#62774,#62775),.UNSPECIFIED.,.F.,.F.,(4,2,2,2,2,2,2,2,2,2,2,2,2,2,2,2,2,
2,2,2,2,2,2,2,2,2,2,2,2,2,2,2,2,2,2,2,2,2,2,2,2,2,2,2,2,2,2,2,2,2,2,2,2,
2,2,2,2,2,2,2,2,2,2,2,2,2,2,2,2,2,2,2,2,2,2,2,2,2,2,2,2,2,2,2,2,2,2,2,2,
2,2,2,2,2,2,2,4),(-1.42841089888011,-1.39743125910206,-1.38627017924954,
-1.37971024003408,-1.37449024409628,-1.36739713881939,-1.35318936919051,
-1.33397199569542,-1.30425467612233,-1.26821184225344,-1.26198698498176,
-1.25836536333979,-1.25500035935803,-1.25000339313463,-1.23533164811459,
-1.16510950920946,-1.14922548606105,-1.14183670814692,-1.1360367879022,
-1.12947804076786,-1.11802308202274,-1.08031352273074,-1.03711764803795,
-1.02539796242703,-1.02067181999798,-1.0173532107127,-1.01362279311818,
-1.00688280537667,-0.964307626410539,-0.918424412513452,-0.907028676291929,
-0.900418977923977,-0.895205902154449,-0.888182772956108,-0.874350769863942,
-0.831502867027447,-0.791039008700119,-0.78358331499852,-0.77966032431973,
-0.77638392736607,-0.771996082351945,-0.761723097388814,-0.746267710548788,
-0.691148415155324,-0.671753967625412,-0.664450734642208,-0.659047360334772,
-0.653085412857472,-0.644601701715289,-0.620923025878264,-0.576659721088888,
-0.548788350275378,-0.542723754773779,-0.539136586917193,-0.535752407258442,
-0.530652911746744,-0.515072306329791,-0.454838251416227,-0.432962182639879,
-0.424470552686589,-0.41856654163639,-0.412459729485191,-0.403217872933108,
-0.371192462615528,-0.343752583386746,-0.311981018327415,-0.304242367226241,
-0.30030924760718,-0.297034193176301,-0.292660996599385,-0.282477285733853,
-0.267213970295811,-0.211933234788478,-0.1924315678338,-0.18511089400292,
-0.179703543397623,-0.173745873371159,-0.173512973598671,-0.173333278919473,
-0.173190533760916,-0.173074616792294,-0.172510806331846,-0.171945837720901,
-0.171370056799897,-0.170773913773818,-0.170147435910445,-0.158407839669011,
-0.143238213392588,-0.103825627830268,-0.0722918285290809,-0.0645660267556695,
-0.0606354498802551,-0.0573601138789549,-0.054120789610304,-0.0497727212624637,
-0.0394267764559731,-0.000694732967017225),.UNSPECIFIED.);
#1425=B_SPLINE_CURVE_WITH_KNOTS('',3,(#62776,#62777,#62778,#62779,#62780,
#62781,#62782,#62783,#62784,#62785,#62786,#62787,#62788,#62789,#62790,#62791),
 .UNSPECIFIED.,.F.,.F.,(4,2,2,2,2,2,2,4),(-3.03489967675623,-2.99347372483665,
-2.98529204977498,-2.97935572956225,-2.97339855375462,-2.96727673357796,
-2.95794991026736,-2.94522627611978),.UNSPECIFIED.);
#1426=B_SPLINE_CURVE_WITH_KNOTS('',3,(#62792,#62793,#62794,#62795,#62796,
#62797,#62798,#62799,#62800,#62801,#62802,#62803,#62804,#62805,#62806,#62807,
#62808,#62809,#62810,#62811,#62812,#62813,#62814,#62815,#62816,#62817,#62818,
#62819,#62820,#62821,#62822,#62823,#62824,#62825,#62826,#62827,#62828,#62829,
#62830,#62831,#62832,#62833,#62834,#62835,#62836,#62837,#62838,#62839,#62840,
#62841,#62842,#62843,#62844,#62845,#62846,#62847,#62848,#62849,#62850,#62851,
#62852,#62853,#62854,#62855,#62856,#62857,#62858,#62859,#62860,#62861,#62862,
#62863,#62864,#62865,#62866,#62867,#62868,#62869,#62870,#62871,#62872,#62873,
#62874,#62875,#62876,#62877,#62878,#62879,#62880,#62881,#62882,#62883,#62884,
#62885,#62886,#62887,#62888,#62889,#62890,#62891,#62892,#62893,#62894,#62895,
#62896,#62897,#62898,#62899,#62900,#62901,#62902,#62903,#62904,#62905,#62906,
#62907,#62908,#62909,#62910,#62911,#62912,#62913,#62914,#62915,#62916,#62917,
#62918,#62919,#62920,#62921,#62922,#62923,#62924,#62925,#62926,#62927,#62928,
#62929,#62930,#62931,#62932,#62933,#62934,#62935,#62936,#62937,#62938,#62939,
#62940,#62941,#62942,#62943,#62944,#62945,#62946,#62947,#62948,#62949,#62950,
#62951,#62952,#62953,#62954,#62955,#62956,#62957,#62958,#62959,#62960,#62961,
#62962,#62963,#62964,#62965,#62966,#62967,#62968,#62969,#62970,#62971,#62972,
#62973,#62974,#62975,#62976,#62977,#62978,#62979,#62980,#62981,#62982,#62983,
#62984,#62985,#62986,#62987,#62988,#62989,#62990,#62991,#62992,#62993,#62994,
#62995,#62996,#62997,#62998,#62999,#63000,#63001,#63002,#63003,#63004,#63005,
#63006,#63007,#63008,#63009,#63010,#63011,#63012,#63013,#63014,#63015,#63016,
#63017,#63018,#63019,#63020,#63021,#63022,#63023,#63024,#63025,#63026,#63027,
#63028,#63029,#63030,#63031,#63032,#63033,#63034,#63035,#63036,#63037,#63038,
#63039,#63040,#63041,#63042,#63043,#63044,#63045,#63046,#63047,#63048,#63049,
#63050,#63051,#63052,#63053,#63054,#63055,#63056,#63057,#63058,#63059,#63060,
#63061,#63062,#63063,#63064,#63065,#63066,#63067,#63068,#63069,#63070,#63071),
 .UNSPECIFIED.,.F.,.F.,(4,2,2,2,2,2,2,2,2,2,2,2,2,2,2,2,2,2,2,2,2,2,2,2,
2,2,2,2,2,2,2,2,2,2,2,2,2,2,2,2,2,2,2,2,2,2,2,2,2,2,2,2,2,2,2,2,2,2,2,2,
2,2,2,2,2,2,2,2,2,2,2,2,2,2,2,2,2,2,2,2,2,2,2,2,2,2,2,2,2,2,2,2,2,2,2,2,
2,2,2,2,2,2,2,2,2,2,2,2,2,2,2,2,2,2,2,2,2,2,2,2,2,2,2,2,2,2,2,2,2,2,2,2,
2,2,2,2,2,2,2,4),(-1.60794378585001,-1.6066158861157,-1.59177736166794,
-1.55115553904906,-1.51854628348446,-1.50515840438898,-1.49813701178107,
-1.49236179629711,-1.48553263022734,-1.47271585801169,-1.43471963056368,
-1.38671505427769,-1.37986218412915,-1.37606821381087,-1.37276843159126,
-1.36817105785611,-1.35654148085098,-1.33800316922406,-1.27611797947543,
-1.26431251812801,-1.25761632678228,-1.25183359864333,-1.24464955941393,
-1.22993588235711,-1.21895620905585,-1.17872466213274,-1.14822555055159,
-1.14063653824262,-1.13668599883945,-1.13341335235904,-1.12906561020843,
-1.11903472094206,-1.10409753113472,-1.0349630755503,-1.0238058074265,-1.01730858573358,
-1.0114992411048,-1.00400944532224,-0.987516967753724,-0.963702091217662,
-0.916548228951036,-0.903395688130634,-0.898462383622608,-0.895142748715777,
-0.891511492739865,-0.885238612798559,-0.845741050902313,-0.795650688148293,
-0.784415561519985,-0.777841032989775,-0.772624942467169,-0.76555760157846,
-0.751482548225762,-0.732513896729955,-0.702416609605827,-0.666308545371244,
-0.66008156541868,-0.656460189012472,-0.653096750673222,-0.648104178589684,
-0.633461975544626,-0.562683402235284,-0.547150149963822,-0.539822810700446,
-0.534030182942953,-0.527436227594513,-0.515801029922933,-0.476642174124733,
-0.430305207357967,-0.421823393302142,-0.417748593392565,-0.41448461020491,
-0.410290227558175,-0.401150876899449,-0.388047103570359,-0.341808185496286,
-0.312128198316772,-0.302890352388055,-0.296785467201068,-0.290813964774743,
-0.2822711366414,-0.258053633019459,-0.211540007429808,-0.186386526791709,
-0.180434128460067,-0.176871650713859,-0.173473262210404,-0.173390655692988,
-0.173307892005637,-0.173224882450212,-0.173141538753151,-0.173057772752981,
-0.172973496037839,-0.172888619640973,-0.172803053745737,-0.172716707327175,
-0.172629487850089,-0.172541300975064,-0.172452050235491,-0.172361636691484,
-0.172269958605175,-0.172176911106818,-0.172082385857964,-0.17198627066799,
-0.171888449104264,-0.171788800128309,-0.171757287849786,-0.171724692046217,
-0.171690944169791,-0.171655970274543,-0.171619690469221,-0.171582018348421,
-0.17154286030542,-0.171502114816463,-0.171459671566905,-0.171415410575822,
-0.171369201107853,-0.171320900520313,-0.171270352934051,-0.171217387689528,
-0.171161817655816,-0.171103437331629,-0.171042020665314,-0.170977318504732,
-0.170909055815295,-0.170836928430975,-0.170760599338807,-0.170679694477294,
-0.170593797887025,-0.170502446143018,-0.170405121993403,-0.170301247048615,
-0.1701901733403,-0.17007117363754,-0.169943430328354,-0.169806022636715,
-0.158945166949799,-0.152234720465392,-0.120589434598602,-0.0904170319211295),
 .UNSPECIFIED.);
#1427=B_SPLINE_CURVE_WITH_KNOTS('',3,(#63076,#63077,#63078,#63079,#63080,
#63081,#63082,#63083,#63084,#63085,#63086,#63087,#63088,#63089,#63090,#63091,
#63092,#63093,#63094,#63095,#63096,#63097,#63098,#63099,#63100,#63101,#63102,
#63103,#63104,#63105,#63106,#63107,#63108,#63109,#63110,#63111,#63112,#63113,
#63114,#63115,#63116,#63117,#63118,#63119,#63120,#63121,#63122,#63123,#63124,
#63125,#63126,#63127,#63128,#63129,#63130,#63131,#63132,#63133,#63134,#63135,
#63136,#63137,#63138,#63139,#63140,#63141,#63142,#63143,#63144,#63145,#63146,
#63147,#63148,#63149,#63150,#63151,#63152,#63153,#63154,#63155,#63156,#63157,
#63158,#63159,#63160,#63161,#63162,#63163,#63164,#63165,#63166,#63167,#63168,
#63169,#63170,#63171,#63172,#63173,#63174,#63175,#63176,#63177,#63178,#63179,
#63180,#63181,#63182,#63183,#63184,#63185,#63186,#63187,#63188,#63189,#63190,
#63191,#63192,#63193,#63194,#63195,#63196,#63197,#63198,#63199,#63200,#63201,
#63202,#63203,#63204,#63205,#63206,#63207,#63208,#63209,#63210,#63211,#63212,
#63213,#63214,#63215,#63216,#63217,#63218,#63219,#63220,#63221,#63222,#63223,
#63224,#63225,#63226,#63227,#63228,#63229,#63230,#63231,#63232,#63233,#63234,
#63235,#63236,#63237,#63238,#63239,#63240,#63241,#63242,#63243,#63244,#63245,
#63246,#63247,#63248,#63249,#63250,#63251,#63252,#63253,#63254,#63255,#63256,
#63257,#63258,#63259,#63260,#63261,#63262,#63263,#63264,#63265,#63266,#63267,
#63268,#63269,#63270,#63271,#63272,#63273),.UNSPECIFIED.,.F.,.F.,(4,2,2,
2,2,2,2,2,2,2,2,2,2,2,2,2,2,2,2,2,2,2,2,2,2,2,2,2,2,2,2,2,2,2,2,2,2,2,2,
2,2,2,2,2,2,2,2,2,2,2,2,2,2,2,2,2,2,2,2,2,2,2,2,2,2,2,2,2,2,2,2,2,2,2,2,
2,2,2,2,2,2,2,2,2,2,2,2,2,2,2,2,2,2,2,2,2,2,2,4),(-2.94574554020504,-2.94263391637022,
-2.9380216451502,-2.93471991858296,-2.93093378306239,-2.92411683916993,
-2.87587854893091,-2.83876665948301,-2.82939216056483,-2.82300227906537,
-2.82247231816296,-2.8219405544679,-2.82137344699033,-2.82071838771216,
-2.81521747057133,-2.80905172400534,-2.79951378668693,-2.76579916297151,
-2.72335017003197,-2.70471569839339,-2.69931749059466,-2.69587344932726,
-2.6923695082861,-2.68669074246475,-2.66655554382784,-2.62147346205144,
-2.59156339601923,-2.58248133282319,-2.57640655770994,-2.57047909404194,
-2.56323577358459,-2.54448605555577,-2.48848806087467,-2.47303865797311,
-2.46276964812287,-2.45838264349705,-2.45510660362791,-2.45118362243595,
-2.44349572581563,-2.40611489576622,-2.36891202207806,-2.35550335480519,
-2.34460979159622,-2.33816598007048,-2.33234391117117,-2.3248785233301,
-2.30804491450854,-2.24810253692434,-2.23308072341452,-2.22301090488542,
-2.21865640254579,-2.21538289749203,-2.21143628845636,-2.20386745340013,
-2.16738806668926,-2.1306054782168,-2.10998194231242,-2.1018762054719,-2.09597947889058,
-2.08974746991473,-2.07988635061938,-2.03879731401897,-2.00172771303634,
-1.98529435238335,-1.98010439757153,-1.97670262553101,-1.97314300588603,
-1.96720654572637,-1.94248942485543,-1.89566384939458,-1.871377981766,-1.86282671637233,
-1.8568525433889,-1.8514609315774,-1.84420838736942,-1.8253348945646,-1.76041744827706,
-1.74527800153628,-1.74022711806984,-1.73685207904848,-1.73324878561934,
-1.72710978478299,-1.69487596940296,-1.65402552840008,-1.63859364088875,
-1.62648759868956,-1.61979748071452,-1.61401281901431,-1.60681697911757,
-1.59538032841674,-1.53949392164539,-1.51782831778016,-1.50518352924775,
-1.50031119422111,-1.49700132260882,-1.49334506109092,-1.48695803363345,
-1.44853616035284,-1.42841089888011),.UNSPECIFIED.);
#1428=B_SPLINE_CURVE_WITH_KNOTS('',3,(#63275,#63276,#63277,#63278,#63279,
#63280,#63281,#63282,#63283,#63284,#63285,#63286,#63287,#63288,#63289,#63290,
#63291,#63292),.UNSPECIFIED.,.F.,.F.,(4,2,2,2,2,2,2,2,4),(-0.0904170319211295,
-0.077397385079546,-0.0657139835705077,-0.0590439735663556,-0.0532594854266007,
-0.0476886497618599,-0.0406051108281494,-0.0267866391532106,-0.000694393962764245),
 .UNSPECIFIED.);
#1429=B_SPLINE_CURVE_WITH_KNOTS('',3,(#63293,#63294,#63295,#63296,#63297,
#63298,#63299,#63300,#63301,#63302),.UNSPECIFIED.,.F.,.F.,(4,1,1,1,1,1,
1,4),(65.9734485846553,66.2383482818393,67.2308234190585,68.2232985562776,
69.2157736934968,70.208248830716,71.2007239679351,71.8851149398144),
 .UNSPECIFIED.);
#1430=B_SPLINE_CURVE_WITH_KNOTS('',3,(#63308,#63309,#63310,#63311,#63312,
#63313,#63314,#63315,#63316,#63317),.UNSPECIFIED.,.F.,.F.,(4,1,1,1,1,1,
1,4),(72.2566310325652,72.8364994652893,73.8289746025085,74.8214497397277,
75.8139248769468,76.806400014166,77.7988751513852,78.1697058192857),
 .UNSPECIFIED.);
#1431=B_SPLINE_CURVE_WITH_KNOTS('',3,(#63318,#63319,#63320,#63321,#63322,
#63323,#63324,#63325),.UNSPECIFIED.,.F.,.F.,(4,2,2,4),(-3.035220816981,
-2.97315166642837,-2.95436542165648,-2.94574554020504),.UNSPECIFIED.);
#1432=B_SPLINE_CURVE_WITH_KNOTS('',3,(#63327,#63328,#63329,#63330,#63331),
 .UNSPECIFIED.,.F.,.F.,(4,1,4),(71.8851149398144,72.1931991051543,72.2566310325652),
 .UNSPECIFIED.);
#1433=B_SPLINE_CURVE_WITH_KNOTS('',3,(#63332,#63333,#63334,#63335,#63336,
#63337,#63338,#63339,#63340,#63341,#63342,#63343,#63344,#63345,#63346,#63347,
#63348,#63349,#63350,#63351,#63352,#63353,#63354,#63355,#63356,#63357,#63358,
#63359,#63360,#63361,#63362,#63363,#63364,#63365,#63366,#63367,#63368,#63369,
#63370,#63371,#63372,#63373,#63374,#63375,#63376,#63377,#63378,#63379,#63380,
#63381,#63382,#63383,#63384,#63385,#63386,#63387,#63388,#63389,#63390,#63391,
#63392,#63393,#63394,#63395,#63396,#63397,#63398,#63399,#63400,#63401,#63402,
#63403,#63404,#63405,#63406,#63407,#63408,#63409,#63410,#63411,#63412,#63413,
#63414,#63415,#63416,#63417,#63418,#63419,#63420,#63421,#63422,#63423,#63424,
#63425,#63426,#63427,#63428,#63429,#63430,#63431,#63432,#63433,#63434,#63435,
#63436,#63437,#63438,#63439,#63440,#63441,#63442,#63443,#63444,#63445,#63446,
#63447,#63448,#63449,#63450,#63451,#63452,#63453,#63454,#63455,#63456,#63457,
#63458,#63459,#63460,#63461,#63462,#63463,#63464,#63465,#63466,#63467,#63468,
#63469,#63470,#63471,#63472,#63473,#63474,#63475,#63476,#63477,#63478,#63479,
#63480,#63481,#63482,#63483,#63484,#63485,#63486,#63487,#63488,#63489,#63490,
#63491,#63492,#63493,#63494,#63495,#63496,#63497,#63498,#63499,#63500,#63501,
#63502,#63503,#63504,#63505,#63506,#63507,#63508,#63509,#63510,#63511,#63512,
#63513,#63514,#63515,#63516,#63517,#63518,#63519,#63520,#63521,#63522,#63523,
#63524,#63525,#63526,#63527,#63528,#63529,#63530,#63531,#63532,#63533,#63534,
#63535,#63536,#63537,#63538,#63539),.UNSPECIFIED.,.F.,.F.,(4,2,2,2,2,2,
2,2,2,2,2,2,2,2,2,2,2,2,2,2,2,2,2,2,2,2,2,2,2,2,2,2,2,2,2,2,2,2,2,2,2,2,
2,2,2,2,2,2,2,2,2,2,2,2,2,2,2,2,2,2,2,2,2,2,2,2,2,2,2,2,2,2,2,2,2,2,2,2,
2,2,2,2,2,2,2,2,2,2,2,2,2,2,2,2,2,2,2,2,2,2,2,2,2,4),(-7.40692637570555,
-7.33746437258257,-7.31576929720708,-7.30752912445337,-7.30161418438117,
-7.29543312973761,-7.28580270729364,-7.24920865613869,-7.2092814225013,
-7.19698698858259,-7.19082090059144,-7.18601372586172,-7.18595005520301,
-7.18588678551918,-7.18582375706269,-7.18576080878017,-7.18569777663025,
-7.18563449182612,-7.18557077886074,-7.18550645330422,-7.18544131927868,
-7.18537516657691,-7.1853077672651,-7.18523887163769,-7.18516820337284,
-7.18509545360177,-7.18502027361203,-7.18494226570937,-7.18486097167816,
-7.18477585804234,-7.18468629686798,-7.18459154048083,-7.1813183202842,
-7.17739909707478,-7.1697198043893,-7.1336669077005,-7.09707122502135,-7.07606809000857,
-7.06791695842809,-7.06201701247935,-7.05580825745978,-7.04604178956603,
-7.00467080220601,-6.9678474721791,-6.95135440212621,-6.94616150449742,
-6.94276135379914,-6.93920741626362,-6.93328752935679,-6.90892501571539,
-6.86184884812638,-6.83751650816176,-6.82896540451994,-6.82299537267477,
-6.81761015113748,-6.81037028795483,-6.79160161740801,-6.72662567342674,
-6.71148979386952,-6.70644234475273,-6.70307020960615,-6.69947081496129,
-6.69334010803431,-6.66185240968146,-6.62048937879845,-6.59758206117575,
-6.5891930023695,-6.58325176049818,-6.57711236280072,-6.56768977963242,
-6.53610458464198,-6.49175978595594,-6.47277125115529,-6.46734515395923,
-6.4638969215758,-6.46082644294791,-6.45559802315712,-6.44006871812096,
-6.4000178007572,-6.37381748163223,-6.35624973341649,-6.34859045612672,
-6.34276368012452,-6.33636042015771,-6.32564917113136,-6.26942833940005,
-6.23467507315847,-6.22849792247837,-6.22488840217855,-6.22156072941251,
-6.21738466586562,-6.20645904983877,-6.12907604803193,-6.11490518625184,
-6.10782319040023,-6.10260860717325,-6.09605201193141,-6.084888117701,-6.0338921044371,
-5.9950992869525,-5.98886992452876,-5.98524941537587,-5.98192771141387,
-5.97968578406166),.UNSPECIFIED.);
#1434=B_SPLINE_CURVE_WITH_KNOTS('',3,(#63545,#63546,#63547,#63548,#63549,
#63550,#63551,#63552,#63553,#63554,#63555,#63556,#63557,#63558,#63559,#63560,
#63561,#63562,#63563,#63564,#63565,#63566,#63567,#63568,#63569,#63570,#63571,
#63572,#63573,#63574,#63575,#63576,#63577,#63578,#63579,#63580,#63581,#63582,
#63583,#63584,#63585,#63586,#63587,#63588,#63589,#63590,#63591,#63592,#63593,
#63594,#63595,#63596,#63597,#63598,#63599,#63600,#63601,#63602,#63603,#63604,
#63605,#63606,#63607,#63608,#63609,#63610,#63611,#63612,#63613,#63614,#63615,
#63616,#63617,#63618,#63619,#63620,#63621,#63622,#63623,#63624,#63625,#63626,
#63627,#63628,#63629,#63630,#63631,#63632,#63633,#63634,#63635,#63636,#63637,
#63638,#63639,#63640,#63641,#63642,#63643,#63644,#63645,#63646,#63647,#63648,
#63649,#63650,#63651,#63652,#63653,#63654,#63655,#63656,#63657,#63658,#63659,
#63660,#63661,#63662,#63663,#63664,#63665,#63666,#63667,#63668,#63669,#63670,
#63671,#63672,#63673,#63674,#63675,#63676,#63677,#63678,#63679,#63680,#63681,
#63682,#63683,#63684,#63685,#63686,#63687,#63688,#63689,#63690,#63691,#63692,
#63693,#63694,#63695,#63696,#63697,#63698,#63699,#63700,#63701,#63702,#63703,
#63704,#63705,#63706,#63707,#63708,#63709,#63710,#63711,#63712,#63713,#63714,
#63715,#63716,#63717,#63718,#63719,#63720,#63721,#63722),.UNSPECIFIED.,
 .F.,.F.,(4,3,3,3,3,3,3,3,3,3,3,3,3,3,3,3,3,3,3,3,3,3,3,3,3,3,3,3,3,3,3,
3,3,3,3,3,3,3,3,3,3,3,3,3,3,3,3,3,3,3,3,3,3,3,3,3,3,3,3,4),(78.5398163397448,
78.6684221201328,78.7913502886043,78.8915768985185,78.9916607299099,79.0916299674899,
79.1915365989967,79.2914114348292,79.3912852456916,79.4912573874797,79.5912772725973,
79.691475689468,79.7838254258235,79.8840520360163,79.9841358676786,80.0841051055166,
80.1840117372737,80.2838865733481,80.3837603844441,80.4837325264511,80.5837524117798,
80.6839508288464,80.7763005630427,80.8765271760024,80.9766110104464,81.0765802510749,
81.1764868856266,81.2763617244957,81.3762355383828,81.4762076831553,81.5762275712401,
81.6764259910143,81.7687757002619,81.8690023062344,81.9690861336894,82.069055367359,
82.1689619949731,82.2688368269357,82.3687106339565,82.4686827719735,82.5687026533527,
82.6689010665837,82.761250837481,82.861477447805,82.9615612795589,83.0615305174294,
83.1614371491829,83.2613119852182,83.3611857962398,83.4611579381179,83.5611778232878,
83.6613762401475,83.7537259747002,83.8539302864532,83.9540022423295,84.0539728511632,
84.1538861754786,84.2537613122279,84.353676596689,84.4517779076862),
 .UNSPECIFIED.);
#1435=B_SPLINE_CURVE_WITH_KNOTS('',3,(#63723,#63724,#63725,#63726),
 .UNSPECIFIED.,.F.,.F.,(4,4),(78.1697058192857,78.5398163397448),
 .UNSPECIFIED.);
#1436=B_SPLINE_CURVE_WITH_KNOTS('',3,(#63727,#63728,#63729,#63730,#63731,
#63732,#63733,#63734,#63735,#63736,#63737,#63738,#63739,#63740,#63741,#63742,
#63743,#63744,#63745,#63746,#63747,#63748,#63749,#63750,#63751,#63752,#63753,
#63754,#63755,#63756,#63757,#63758,#63759,#63760,#63761,#63762,#63763,#63764,
#63765,#63766,#63767,#63768,#63769,#63770,#63771,#63772,#63773,#63774,#63775,
#63776,#63777,#63778,#63779,#63780,#63781,#63782,#63783,#63784,#63785,#63786,
#63787,#63788,#63789,#63790,#63791,#63792,#63793,#63794,#63795,#63796,#63797,
#63798,#63799,#63800,#63801,#63802,#63803,#63804,#63805,#63806,#63807,#63808,
#63809,#63810,#63811,#63812,#63813,#63814,#63815,#63816,#63817,#63818,#63819,
#63820,#63821,#63822,#63823,#63824,#63825,#63826,#63827,#63828,#63829,#63830,
#63831,#63832,#63833,#63834,#63835,#63836,#63837,#63838,#63839,#63840,#63841,
#63842,#63843,#63844,#63845,#63846,#63847,#63848,#63849,#63850,#63851,#63852,
#63853,#63854,#63855,#63856,#63857,#63858,#63859,#63860,#63861,#63862,#63863,
#63864,#63865,#63866,#63867,#63868,#63869,#63870,#63871,#63872,#63873,#63874,
#63875,#63876,#63877,#63878,#63879,#63880,#63881,#63882,#63883,#63884,#63885,
#63886,#63887,#63888,#63889,#63890,#63891,#63892,#63893,#63894,#63895,#63896,
#63897,#63898,#63899,#63900,#63901,#63902,#63903,#63904,#63905,#63906,#63907,
#63908,#63909,#63910),.UNSPECIFIED.,.F.,.F.,(4,2,2,2,2,2,2,2,2,2,2,2,2,
2,2,2,2,2,2,2,2,2,2,2,2,2,2,2,2,2,2,2,2,2,2,2,2,2,2,2,2,2,2,2,2,2,2,2,2,
2,2,2,2,2,2,2,2,2,2,2,2,2,2,2,2,2,2,2,2,2,2,2,2,2,2,2,2,2,2,2,2,2,2,2,2,
2,2,2,2,2,2,4),(-5.97968578406166,-5.97777524899889,-5.96707634600142,-5.91748140018603,
-5.89328770447047,-5.87662121589563,-5.86910587326657,-5.86329664062136,
-5.85681985478997,-5.84575034987089,-5.78380545876526,-5.75510400534421,
-5.74909749852156,-5.7455244880415,-5.74217609187747,-5.73707910099528,
-5.72265289987859,-5.67684586465858,-5.64155872287236,-5.63211814690166,
-5.62597455986409,-5.62010221364698,-5.61307526092356,-5.59563511192601,
-5.53704783298034,-5.52202247801489,-5.51195266290995,-5.50759987078933,
-5.50432841498464,-5.5003853507009,-5.49282624576918,-5.45623640489311,
-5.41943012074704,-5.39892935702118,-5.39084341047394,-5.38495287984466,
-5.37872008773172,-5.36884182474448,-5.32789109469462,-5.29074715594446,
-5.27432912047089,-5.26914291396222,-5.26574342111177,-5.26218611071873,
-5.25625354543958,-5.23156433738646,-5.18474060543174,-5.16046146113616,
-5.15191453724468,-5.14594401978716,-5.14055615412961,-5.13330938979103,
-5.11446582208134,-5.04956544469465,-5.0344166596197,-5.02936680749083,
-5.0259935326858,-5.02239343949439,-5.01626249761823,-4.98509416183607,
-4.94347411652509,-4.92049309607189,-4.91209370836017,-4.90614937295933,
-4.90001037365684,-4.89059574826412,-4.85915774427427,-4.81465357471461,
-4.80175423360786,-4.79271937558736,-4.78854430074904,-4.78559952472588,
-4.7816698806427,-4.77394237969323,-4.73872282011194,-4.70242150679562,
-4.68058501867143,-4.67232490112911,-4.66640480152499,-4.66022635419281,
-4.65061685025712,-4.6149944689493,-4.57918774502019,-4.56388220746901,
-4.55368117402625,-4.54930655534362,-4.5460330239758,-4.54210494808226,
-4.53438530686615,-4.50290763004632,-4.47625482696426,-4.46296054289888),
 .UNSPECIFIED.);
#1437=B_SPLINE_CURVE_WITH_KNOTS('',3,(#63916,#63917,#63918,#63919,#63920,
#63921,#63922,#63923,#63924,#63925,#63926,#63927,#63928,#63929,#63930,#63931,
#63932,#63933,#63934,#63935,#63936,#63937,#63938,#63939,#63940,#63941,#63942,
#63943,#63944,#63945,#63946,#63947,#63948,#63949,#63950,#63951,#63952,#63953,
#63954,#63955,#63956,#63957,#63958,#63959,#63960,#63961,#63962,#63963,#63964,
#63965,#63966,#63967,#63968,#63969,#63970,#63971,#63972,#63973,#63974,#63975,
#63976,#63977,#63978,#63979,#63980,#63981,#63982,#63983,#63984,#63985,#63986,
#63987,#63988,#63989,#63990,#63991,#63992,#63993,#63994,#63995,#63996,#63997,
#63998,#63999,#64000,#64001,#64002,#64003,#64004,#64005,#64006,#64007,#64008,
#64009,#64010,#64011,#64012,#64013,#64014,#64015,#64016,#64017,#64018,#64019,
#64020,#64021,#64022,#64023,#64024,#64025,#64026,#64027,#64028,#64029,#64030,
#64031,#64032,#64033,#64034,#64035,#64036,#64037,#64038,#64039,#64040,#64041,
#64042,#64043,#64044,#64045,#64046,#64047,#64048,#64049,#64050,#64051,#64052,
#64053,#64054,#64055,#64056,#64057,#64058,#64059,#64060,#64061,#64062,#64063,
#64064,#64065,#64066,#64067,#64068,#64069,#64070,#64071,#64072,#64073,#64074,
#64075,#64076,#64077,#64078,#64079,#64080,#64081,#64082,#64083,#64084,#64085,
#64086,#64087,#64088,#64089,#64090,#64091,#64092,#64093,#64094,#64095,#64096,
#64097,#64098,#64099,#64100,#64101,#64102,#64103,#64104,#64105,#64106,#64107,
#64108,#64109,#64110,#64111,#64112,#64113,#64114,#64115,#64116,#64117,#64118,
#64119,#64120,#64121,#64122,#64123,#64124,#64125,#64126,#64127,#64128,#64129,
#64130,#64131,#64132,#64133,#64134,#64135,#64136,#64137,#64138,#64139,#64140,
#64141,#64142,#64143,#64144,#64145,#64146,#64147,#64148,#64149,#64150,#64151,
#64152,#64153,#64154,#64155,#64156,#64157,#64158,#64159,#64160,#64161,#64162,
#64163,#64164,#64165,#64166,#64167,#64168,#64169,#64170,#64171,#64172,#64173),
 .UNSPECIFIED.,.F.,.F.,(4,2,2,2,2,2,2,2,2,2,2,2,2,2,2,2,2,2,2,2,2,2,2,2,
2,2,2,2,2,2,2,2,2,2,2,2,2,2,2,2,2,2,2,2,2,2,2,2,2,2,2,2,2,2,2,2,2,2,2,2,
2,2,2,2,2,2,2,2,2,2,2,2,2,2,2,2,2,2,2,2,2,2,2,2,2,2,2,2,2,2,2,2,2,2,2,2,
2,2,2,2,2,2,2,2,2,2,2,2,2,2,2,2,2,2,2,2,2,2,2,2,2,2,2,2,2,2,2,2,4),(-1.42837807589884,
-1.42524134414718,-1.42130813240249,-1.4180338660253,-1.41366302047601,
-1.40349121065487,-1.38825241851016,-1.33081896982025,-1.31295448713341,
-1.30580980368273,-1.29990690633567,-1.29380061282707,-1.28455822691273,
-1.25250836612072,-1.22510254701366,-1.19334907132251,-1.18561256150371,
-1.18168016668658,-1.17840559590932,-1.1740327817962,-1.16384836766296,
-1.14858228631447,-1.09386815109252,-1.07400654788409,-1.06580502126933,
-1.0599519619398,-1.05376722256114,-1.04413333325148,-1.00487797354269,
-0.964842987353306,-0.949216328408684,-0.943974538163219,-0.940900334670229,
-0.937452237205509,-0.9320336659137,-0.913155522800388,-0.869411685162678,
-0.837208113905973,-0.827743078855024,-0.82159245586301,-0.815652141982764,
-0.807284453152251,-0.784587988878946,-0.74400716229303,-0.711368328351309,
-0.705227638905959,-0.701624644024069,-0.698250872939404,-0.693203493137969,
-0.678085781538767,-0.613110999641547,-0.594332994057977,-0.587089214396346,
-0.581700420395482,-0.575725715152555,-0.567166528349918,-0.542801010319937,
-0.495627918297755,-0.471287683708212,-0.465364240543545,-0.461807880295868,
-0.458404978616514,-0.453207183529864,-0.436688279963417,-0.400032391087145,
-0.361885768785443,-0.35047887588711,-0.343867454283116,-0.338131314186896,
-0.330856719093743,-0.315630638434211,-0.294432454928553,-0.266719019019359,
-0.23483058153165,-0.227099407511814,-0.22316818432982,-0.220012930508764,
-0.219915748223137,-0.219825304576007,-0.21974064895348,-0.219660996951698,
-0.219585694081227,-0.219514188689558,-0.219446011404488,-0.219380759368339,
-0.219318083946978,-0.219257681068282,-0.219199283527306,-0.219142654786388,
-0.219087583953101,-0.219033881682199,-0.218981376761157,-0.218929913270291,
-0.218879348220789,-0.218829549545364,-0.218780394341606,-0.218731767403464,
-0.218683559903509,-0.218635668294907,-0.218587993259698,-0.218540438778011,
-0.218492911321806,-0.218445319092736,-0.218397571275159,-0.218349577330781,
-0.218301246341939,-0.218252486377718,-0.218203203830066,-0.218153302741946,
-0.218102684134915,-0.218051245310653,-0.217998879108618,-0.217945473125218,
-0.217890908873052,-0.217835060861853,-0.217777795598811,-0.21771897052681,
-0.217658432817669,-0.213752607898776,-0.207664338282858,-0.195609598126315,
-0.157343946092611,-0.118770999978118,-0.109091642139302,-0.102897455692032,
-0.0969826916772131,-0.0887638153535705,-0.0672701948442808,-0.000695735724638068),
 .UNSPECIFIED.);
#1438=B_SPLINE_CURVE_WITH_KNOTS('',3,(#64174,#64175,#64176,#64177,#64178,
#64179,#64180,#64181,#64182,#64183,#64184,#64185,#64186),.UNSPECIFIED.,
 .F.,.F.,(4,3,3,3,4),(84.4517779076862,84.5517966727696,84.6519945647983,
84.7462011119194,84.8230016469244),.UNSPECIFIED.);
#1439=B_SPLINE_CURVE_WITH_KNOTS('',3,(#64187,#64188,#64189,#64190,#64191,
#64192,#64193,#64194,#64195,#64196,#64197,#64198,#64199,#64200,#64201,#64202,
#64203,#64204,#64205,#64206,#64207,#64208,#64209,#64210,#64211,#64212,#64213,
#64214,#64215,#64216,#64217,#64218,#64219,#64220,#64221,#64222,#64223,#64224,
#64225,#64226,#64227,#64228,#64229,#64230,#64231,#64232,#64233,#64234,#64235,
#64236,#64237,#64238,#64239,#64240,#64241,#64242,#64243,#64244,#64245,#64246,
#64247,#64248,#64249,#64250,#64251,#64252,#64253,#64254,#64255,#64256,#64257,
#64258,#64259,#64260,#64261,#64262,#64263,#64264,#64265,#64266,#64267,#64268,
#64269,#64270,#64271,#64272,#64273,#64274,#64275,#64276,#64277,#64278,#64279,
#64280,#64281,#64282,#64283,#64284,#64285,#64286,#64287,#64288,#64289,#64290,
#64291,#64292,#64293,#64294,#64295,#64296,#64297,#64298,#64299,#64300,#64301,
#64302,#64303,#64304,#64305,#64306,#64307,#64308,#64309,#64310,#64311,#64312,
#64313,#64314,#64315,#64316,#64317,#64318,#64319,#64320,#64321,#64322,#64323,
#64324,#64325,#64326,#64327,#64328,#64329,#64330,#64331,#64332,#64333,#64334,
#64335,#64336,#64337,#64338,#64339,#64340,#64341,#64342,#64343,#64344,#64345,
#64346,#64347,#64348,#64349,#64350,#64351,#64352,#64353,#64354,#64355,#64356,
#64357,#64358,#64359,#64360,#64361,#64362,#64363,#64364,#64365,#64366,#64367,
#64368,#64369,#64370,#64371,#64372,#64373,#64374,#64375,#64376,#64377,#64378),
 .UNSPECIFIED.,.F.,.F.,(4,2,2,2,2,2,2,2,2,2,2,2,2,2,2,2,2,2,2,2,2,2,2,2,
2,2,2,2,2,2,2,2,2,2,2,2,2,2,2,2,2,2,2,2,2,2,2,2,2,2,2,2,2,2,2,2,2,2,2,2,
2,2,2,2,2,2,2,2,2,2,2,2,2,2,2,2,2,2,2,2,2,2,2,2,2,2,2,2,2,2,2,2,2,2,2,4),
(-4.46296054289888,-4.44334705562705,-4.43404958348456,-4.4279339977854,
-4.4220417148616,-4.41360295271457,-4.39210733336086,-4.33129100598783,
-4.31574691641167,-4.31065281438645,-4.30727088869646,-4.30368466750205,
-4.29761940742059,-4.26965358527184,-4.22553039061928,-4.20189355904667,
-4.19341755216622,-4.18745911162837,-4.1820576493129,-4.17475514689521,
-4.15535293696579,-4.09969282609683,-4.08454065386224,-4.07441075898397,
-4.07004747387351,-4.06677453186116,-4.06283750502988,-4.05507384244125,
-4.02286684187405,-3.99444982727113,-3.9637589638796,-3.95461776879782,
-3.94853266601384,-3.94261675738436,-3.93541467699021,-3.91712302935526,
-3.86004411962012,-3.84490421262699,-3.83477986048366,-3.83041731575201,
-3.82714424698754,-3.82320623065312,-3.81567453892662,-3.77796710796068,
-3.7406733280058,-3.727412380208,-3.71661043407204,-3.71018666307565,-3.70436187545414,
-3.69673534282109,-3.67939117588751,-3.65370241978786,-3.60144741373858,
-3.59393639821687,-3.59000256049281,-3.58672873562954,-3.5823597260441,
-3.57219686335738,-3.55697695049393,-3.52313994985118,-3.48554327900528,
-3.47588776628478,-3.46969888990834,-3.4637822578494,-3.45554938069427,
-3.4339423864121,-3.39751237417951,-3.36202029706523,-3.35429261997151,
-3.35036226778842,-3.34741659053971,-3.34323984950171,-3.33419959664806,
-3.32129278327236,-3.27671388122,-3.245388391687,-3.23598020646377,-3.22984124494449,
-3.22389387981815,-3.21548499296537,-3.19244091168747,-3.15061029285033,
-3.11963174995708,-3.11349842670924,-3.10989711780091,-3.1065227494267,
-3.10147147976953,-3.08631828945336,-3.02152848276922,-3.00261668519787,
-2.99536362704613,-2.98997293614038,-2.98400108874955,-2.97545597721663,
-2.95121688859845,-2.94580181291742),.UNSPECIFIED.);
#1440=B_SPLINE_CURVE_WITH_KNOTS('',3,(#64383,#64384,#64385,#64386,#64387,
#64388,#64389,#64390,#64391,#64392,#64393,#64394,#64395,#64396,#64397,#64398,
#64399,#64400,#64401,#64402,#64403,#64404,#64405,#64406,#64407,#64408,#64409,
#64410,#64411,#64412,#64413,#64414,#64415,#64416,#64417,#64418,#64419,#64420,
#64421,#64422,#64423,#64424,#64425,#64426,#64427,#64428,#64429,#64430,#64431,
#64432,#64433,#64434,#64435,#64436,#64437,#64438,#64439,#64440,#64441,#64442,
#64443,#64444,#64445,#64446,#64447,#64448,#64449,#64450,#64451,#64452,#64453,
#64454,#64455,#64456,#64457,#64458,#64459,#64460,#64461,#64462,#64463,#64464,
#64465,#64466,#64467,#64468,#64469,#64470,#64471,#64472,#64473,#64474,#64475,
#64476,#64477,#64478,#64479,#64480,#64481,#64482,#64483,#64484,#64485,#64486,
#64487,#64488,#64489,#64490,#64491,#64492,#64493,#64494,#64495,#64496,#64497,
#64498,#64499,#64500,#64501,#64502,#64503,#64504,#64505,#64506,#64507,#64508,
#64509,#64510,#64511,#64512,#64513,#64514,#64515,#64516,#64517,#64518,#64519,
#64520,#64521,#64522,#64523,#64524,#64525,#64526,#64527,#64528,#64529,#64530,
#64531,#64532,#64533,#64534,#64535,#64536,#64537,#64538,#64539,#64540,#64541,
#64542,#64543,#64544,#64545,#64546,#64547,#64548,#64549,#64550,#64551,#64552,
#64553,#64554,#64555,#64556,#64557,#64558,#64559,#64560,#64561,#64562,#64563,
#64564,#64565,#64566,#64567,#64568,#64569,#64570,#64571,#64572),
 .UNSPECIFIED.,.F.,.F.,(4,2,2,2,2,2,2,2,2,2,2,2,2,2,2,2,2,2,2,2,2,2,2,2,
2,2,2,2,2,2,2,2,2,2,2,2,2,2,2,2,2,2,2,2,2,2,2,2,2,2,2,2,2,2,2,2,2,2,2,2,
2,2,2,2,2,2,2,2,2,2,2,2,2,2,2,2,2,2,2,2,2,2,2,2,2,2,2,2,2,2,2,2,2,2,4),
(-2.94523236784797,-2.89412897057835,-2.87585892680347,-2.87199687465583,
-2.86442055324781,-2.86427548969014,-2.86414119233107,-2.8640166129821,
-2.86390082307732,-2.86379299865036,-2.85946083256039,-2.85620259674313,
-2.85227043674791,-2.84453338318664,-2.80990801160753,-2.77348898574701,
-2.75124899808426,-2.7429277620191,-2.73698705154369,-2.73080646540264,
-2.72123196771318,-2.68678242039236,-2.64530585489749,-2.6268780382423,
-2.62148894264644,-2.61803956528082,-2.61495270216126,-2.60965455558554,
-2.59354306914457,-2.54939496425623,-2.51456920830108,-2.50515264440698,
-2.49901148643024,-2.49313194344047,-2.48608479983668,-2.46852256403455,
-2.40160359846132,-2.38652379516422,-2.38148159343967,-2.37811005343167,
-2.37451002517544,-2.36837267859651,-2.33537605226832,-2.30873130461617,
-2.27476673196577,-2.26540624945676,-2.2592811113331,-2.25340260469101,
-2.24502423249094,-2.22394696151315,-2.16259905988378,-2.14701373847534,
-2.14191748829202,-2.13853666780573,-2.1349518515119,-2.12889534515261,
-2.10118564852403,-2.05686040946996,-2.03317154616355,-2.02468740468876,
-2.01872546561648,-2.01332215921277,-2.00461593107362,-1.98074941512188,
-1.92327105220116,-1.90749275391143,-1.90237124624896,-1.89898250999011,
-1.89584940771864,-1.89029635207755,-1.87150069347068,-1.82516514819071,
-1.79499290309654,-1.78589146527955,-1.77981369910301,-1.77389070552113,
-1.7666621346104,-1.74809801522878,-1.68280577363384,-1.66768216522862,
-1.66263425357083,-1.65926069278246,-1.65565859713215,-1.64952080810449,
-1.61707659581354,-1.57640063968567,-1.56100285568651,-1.54891789362754,
-1.542233720371,-1.53645116631866,-1.52925403651798,-1.51780712372874,-1.46891882869467,
-1.4329837807736,-1.42837807589884),.UNSPECIFIED.);
#1441=B_SPLINE_CURVE_WITH_KNOTS('',3,(#64573,#64574,#64575,#64576,#64577,
#64578,#64579,#64580,#64581,#64582,#64583,#64584,#64585,#64586,#64587,#64588,
#64589,#64590,#64591,#64592,#64593,#64594,#64595,#64596,#64597,#64598,#64599,
#64600,#64601,#64602,#64603,#64604,#64605,#64606,#64607,#64608,#64609,#64610,
#64611,#64612,#64613,#64614,#64615,#64616,#64617,#64618,#64619,#64620,#64621,
#64622,#64623,#64624,#64625,#64626,#64627,#64628,#64629,#64630,#64631,#64632,
#64633,#64634,#64635,#64636,#64637,#64638,#64639,#64640,#64641,#64642,#64643,
#64644,#64645,#64646,#64647,#64648,#64649,#64650,#64651,#64652,#64653,#64654,
#64655,#64656,#64657,#64658,#64659,#64660,#64661,#64662,#64663,#64664,#64665,
#64666,#64667,#64668,#64669,#64670,#64671,#64672,#64673,#64674,#64675,#64676,
#64677,#64678,#64679,#64680,#64681,#64682,#64683,#64684,#64685,#64686,#64687,
#64688,#64689,#64690,#64691,#64692,#64693,#64694,#64695,#64696,#64697,#64698,
#64699,#64700,#64701,#64702,#64703,#64704,#64705,#64706,#64707,#64708,#64709,
#64710,#64711,#64712,#64713,#64714,#64715,#64716,#64717,#64718,#64719,#64720,
#64721,#64722,#64723,#64724,#64725,#64726,#64727,#64728,#64729,#64730,#64731,
#64732,#64733,#64734,#64735,#64736,#64737,#64738,#64739,#64740,#64741,#64742,
#64743,#64744,#64745,#64746,#64747,#64748,#64749,#64750,#64751,#64752,#64753,
#64754,#64755,#64756,#64757,#64758,#64759,#64760),.UNSPECIFIED.,.F.,.F.,
(4,2,2,2,2,2,2,2,2,2,2,2,2,2,2,2,2,2,2,2,2,2,2,2,2,2,2,2,2,2,2,2,2,2,2,
2,2,2,2,2,2,2,2,2,2,2,2,2,2,2,2,2,2,2,2,2,2,2,2,2,2,2,2,2,2,2,2,2,2,2,2,
2,2,2,2,2,2,2,2,2,2,2,2,2,2,2,2,2,2,2,2,2,2,4),(-2.94580181291742,-2.90460817499543,
-2.87957057982993,-2.87362279539053,-2.87006135467304,-2.86666243233881,
-2.86148378575859,-2.84514975103675,-2.80769388954017,-2.76699648150796,
-2.75710869117688,-2.75087233969347,-2.74498008002403,-2.73689442948782,
-2.71641315089111,-2.67954814378088,-2.64288082941598,-2.63531715777725,
-2.63137219105095,-2.62809941468957,-2.62374530387194,-2.61367391329442,
-2.59864989086835,-2.54036867173092,-2.52282693656846,-2.51573252499838,
-2.50984227131804,-2.50371957771023,-2.49439260272701,-2.46107579791063,
-2.4347056638658,-2.40330639069313,-2.39558813285142,-2.39165958686182,
-2.38838478073055,-2.38400740923458,-2.37379534298358,-2.35847022784197,
-2.32342084827458,-2.28715451827096,-2.27752768260669,-2.27134423055541,
-2.2654236152994,-2.25716992115575,-2.23540234331792,-2.19902855419543,
-2.16368967106783,-2.15595854697814,-2.1520273602556,-2.14908177966834,
-2.14490607103522,-2.1358707893209,-2.1229737375826,-2.07847633986276,-2.04705775273901,
-2.03764330338641,-2.031503338738,-2.02555727575551,-2.01715417805907,-1.99415698908484,
-1.95249960551774,-1.92128425609789,-1.91514975410334,-1.91154833581123,
-1.90817433469293,-1.90312451294921,-1.88798375021566,-1.82275564409671,
-1.80417786895916,-1.79694843026936,-1.79102493033042,-1.78494694635427,
-1.77584597289201,-1.74569901618576,-1.69954658479955,-1.68050149940176,
-1.67491384650807,-1.67142947861358,-1.66796604998943,-1.66248058532875,
-1.64281917099795,-1.59458126778472,-1.56697662497112,-1.55790248733235,
-1.55243492120172,-1.54652696657721,-1.53835637895877,-1.51724841161208,
-1.48062542995621,-1.44468151589752,-1.43693716097271,-1.43300316341903,
-1.4297307922503,-1.42845765518849),.UNSPECIFIED.);
#1442=B_SPLINE_CURVE_WITH_KNOTS('',3,(#64764,#64765,#64766,#64767,#64768,
#64769,#64770,#64771,#64772,#64773,#64774,#64775,#64776,#64777,#64778,#64779,
#64780,#64781,#64782,#64783,#64784,#64785,#64786,#64787,#64788,#64789,#64790,
#64791,#64792,#64793,#64794,#64795,#64796,#64797,#64798,#64799,#64800,#64801,
#64802,#64803,#64804,#64805,#64806,#64807,#64808,#64809,#64810,#64811,#64812,
#64813,#64814,#64815,#64816,#64817,#64818,#64819,#64820,#64821,#64822,#64823,
#64824,#64825,#64826,#64827,#64828,#64829,#64830,#64831,#64832,#64833),
 .UNSPECIFIED.,.F.,.F.,(4,3,3,3,3,3,3,3,3,3,3,3,3,3,3,3,3,3,3,3,3,3,3,4),
(-4.05574753316386,-3.96990054887667,-3.87574120014698,-3.78170877927821,
-3.68777526208839,-3.59390997284874,-3.50007964416114,-3.4062590961083,
-3.3124231640359,-3.21849032913891,-3.1245041690831,-3.03037165160513,-2.9774254116575,
-2.88380029281574,-2.79029953948074,-2.69318460824238,-2.59984389426094,
-2.50653282197543,-2.41322559184539,-2.31989641457199,-2.22646577718421,
-2.1329748240063,-2.03934284451356,-2.01338008957384),.UNSPECIFIED.);
#1443=B_SPLINE_CURVE_WITH_KNOTS('',3,(#64837,#64838,#64839,#64840,#64841),
 .UNSPECIFIED.,.F.,.F.,(4,1,4),(0.,0.992475137219176,1.09916241472585),
 .UNSPECIFIED.);
#1444=B_SPLINE_CURVE_WITH_KNOTS('',3,(#64843,#64844,#64845,#64846,#64847,
#64848,#64849,#64850,#64851,#64852,#64853,#64854,#64855,#64856,#64857,#64858,
#64859,#64860,#64861,#64862,#64863,#64864,#64865,#64866,#64867,#64868,#64869,
#64870,#64871,#64872,#64873,#64874,#64875,#64876,#64877,#64878,#64879,#64880,
#64881,#64882,#64883,#64884,#64885,#64886,#64887,#64888,#64889,#64890,#64891,
#64892,#64893,#64894,#64895,#64896,#64897,#64898,#64899,#64900,#64901,#64902,
#64903,#64904,#64905,#64906,#64907,#64908,#64909,#64910,#64911,#64912,#64913,
#64914,#64915,#64916,#64917,#64918,#64919,#64920,#64921,#64922,#64923,#64924,
#64925,#64926,#64927,#64928,#64929,#64930,#64931,#64932,#64933,#64934,#64935,
#64936,#64937,#64938,#64939,#64940,#64941,#64942,#64943,#64944,#64945,#64946,
#64947,#64948,#64949,#64950,#64951,#64952,#64953,#64954,#64955,#64956,#64957,
#64958,#64959,#64960,#64961,#64962,#64963,#64964,#64965,#64966,#64967,#64968,
#64969,#64970,#64971,#64972,#64973,#64974,#64975,#64976,#64977,#64978,#64979,
#64980,#64981,#64982,#64983,#64984,#64985,#64986,#64987,#64988,#64989,#64990,
#64991,#64992,#64993,#64994,#64995,#64996,#64997,#64998,#64999,#65000,#65001,
#65002,#65003,#65004,#65005,#65006,#65007,#65008,#65009,#65010,#65011,#65012,
#65013,#65014,#65015,#65016,#65017,#65018,#65019,#65020,#65021,#65022,#65023,
#65024,#65025,#65026,#65027,#65028,#65029,#65030,#65031,#65032,#65033,#65034,
#65035,#65036,#65037,#65038,#65039,#65040,#65041,#65042,#65043,#65044,#65045,
#65046,#65047,#65048,#65049,#65050,#65051,#65052,#65053),.UNSPECIFIED.,
 .F.,.F.,(4,3,3,3,3,3,3,3,3,3,3,3,3,3,3,3,3,3,3,3,3,3,3,3,3,3,3,3,3,3,3,
3,3,3,3,3,3,3,3,3,3,3,3,3,3,3,3,3,3,3,3,3,3,3,3,3,3,3,3,3,3,3,3,3,3,3,3,
3,3,3,4),(1.09916241472585,1.19108189997564,1.28288257485515,1.37459207473264,
1.46625293783966,1.55789236719196,1.64953753678025,1.74127307032638,1.83305681701207,
1.92499004688988,1.98495027443835,2.07904726479922,2.17301758138154,2.26688931662874,
2.36069352084906,2.45446321554417,2.54822364236444,2.64200002812979,2.73587451626984,
2.82980292430621,2.92387915370253,2.97742541165751,3.07156802140755,3.16558709693299,
3.25951064804815,3.3533710377344,3.44719960305778,3.54102152138864,3.63486195742961,
3.72880403951816,3.82280214187751,3.91695071813298,3.96990054887668,4.06378056215249,
4.15753260692621,4.25118509216546,4.34476952351686,4.43831921063563,4.531859673343,
4.62541641671787,4.71907310930614,4.81278444856287,4.9066469062787,4.96237568609585,
5.05638711968008,5.15027213667652,5.24405895441764,5.3377791926669,5.43146554874222,
5.52514337660817,5.61883801603108,5.71263258107009,5.80648198314815,5.90048144632545,
5.95485082331501,6.04885731394597,6.14273765631534,6.23652007325052,6.3302363411792,
6.42391899533065,6.51759339540272,6.61128488712475,6.70507675502254,6.7989237106116,
6.89292115016949,6.94732596053418,7.0492143061606,7.15073816485904,7.25202703522367,
7.35297873667727,7.38234742361043),.UNSPECIFIED.);
#1445=B_SPLINE_CURVE_WITH_KNOTS('',3,(#65055,#65056,#65057,#65058,#65059,
#65060,#65061,#65062,#65063,#65064),.UNSPECIFIED.,.F.,.F.,(4,1,1,1,1,1,
1,4),(7.38234772190543,7.93980109775335,8.93227623497251,9.92475137219169,
10.9172265094109,11.90970164663,12.9021767838492,13.6655327805175),
 .UNSPECIFIED.);
#1446=B_SPLINE_CURVE_WITH_KNOTS('',3,(#65066,#65067,#65068,#65069,#65070,
#65071,#65072,#65073,#65074,#65075,#65076,#65077,#65078,#65079,#65080,#65081,
#65082,#65083,#65084,#65085,#65086,#65087,#65088,#65089,#65090,#65091,#65092,
#65093,#65094,#65095,#65096,#65097,#65098,#65099,#65100,#65101,#65102,#65103,
#65104,#65105,#65106,#65107,#65108,#65109,#65110,#65111,#65112,#65113,#65114,
#65115,#65116,#65117,#65118,#65119,#65120,#65121,#65122,#65123,#65124,#65125,
#65126,#65127,#65128,#65129,#65130,#65131,#65132,#65133,#65134,#65135,#65136,
#65137,#65138,#65139,#65140,#65141,#65142,#65143,#65144,#65145,#65146,#65147,
#65148,#65149,#65150,#65151,#65152,#65153,#65154,#65155,#65156,#65157,#65158,
#65159,#65160,#65161,#65162,#65163,#65164,#65165,#65166,#65167,#65168,#65169,
#65170,#65171,#65172,#65173,#65174,#65175,#65176,#65177,#65178,#65179,#65180,
#65181,#65182,#65183,#65184,#65185,#65186,#65187,#65188,#65189,#65190,#65191,
#65192,#65193,#65194,#65195,#65196,#65197,#65198,#65199,#65200,#65201,#65202,
#65203,#65204,#65205,#65206,#65207,#65208,#65209,#65210,#65211,#65212,#65213,
#65214,#65215,#65216,#65217,#65218,#65219,#65220,#65221,#65222,#65223,#65224,
#65225,#65226,#65227,#65228,#65229,#65230,#65231,#65232,#65233,#65234,#65235,
#65236,#65237,#65238,#65239,#65240,#65241,#65242,#65243,#65244,#65245,#65246,
#65247,#65248,#65249,#65250,#65251,#65252,#65253,#65254,#65255,#65256,#65257,
#65258,#65259,#65260,#65261,#65262,#65263,#65264,#65265,#65266,#65267,#65268,
#65269,#65270,#65271,#65272,#65273),.UNSPECIFIED.,.F.,.F.,(4,3,3,3,3,3,
3,3,3,3,3,3,3,3,3,3,3,3,3,3,3,3,3,3,3,3,3,3,3,3,3,3,3,3,3,3,3,3,3,3,3,3,
3,3,3,3,3,3,3,3,3,3,3,3,3,3,3,3,3,3,3,3,3,3,3,3,3,3,3,4),(13.665533029085,
13.7908310334317,13.8946519210684,13.988641850667,14.0825052861128,14.1762704756524,
14.2699691086556,14.363633882415,14.4572901782299,14.5509633632484,14.6447367251609,
14.7385650352236,14.8325437909839,14.8871270582875,14.9811168910591,15.0749802289659,
15.1687453203954,15.2624438548513,15.3561085298316,15.4497647267587,15.5434378129045,
15.6372110765735,15.7310392886046,15.8250179476368,15.8796021955067,15.9735919886998,
16.0674552860834,16.1612203361062,16.2549188280051,16.3485834597327,16.442239612763,
16.5359126544189,16.6296858729579,16.7235140394316,16.8174926526751,16.8720773327259,
16.966067173307,17.0599305187923,17.1536956175594,17.2473941589593,17.341058840637,
17.4347150440056,17.5283881363271,17.6221614057251,17.7159896232411,17.8099682873159,
17.864552469945,17.9585422943882,18.0524056235837,18.1461707059327,18.2398692307921,
18.33353389586,18.4271900825701,18.5208631582051,18.6146364109757,18.7084646118734,
18.8024432595083,18.8570276071642,18.9510174282501,19.0448807539868,19.1386458327808,
19.232344353956,19.3260090152612,19.4196651981345,19.5133382698629,19.6071115186433,
19.700939715498,19.7949183590452,19.8495027443834,19.9487183362646),
 .UNSPECIFIED.);
#1447=B_SPLINE_CURVE_WITH_KNOTS('',3,(#65275,#65276,#65277,#65278,#65279,
#65280,#65281,#65282,#65283,#65284,#65285,#65286,#65287,#65288,#65289,#65290,
#65291,#65292,#65293,#65294,#65295,#65296,#65297,#65298,#65299,#65300,#65301,
#65302,#65303,#65304,#65305,#65306,#65307,#65308,#65309,#65310,#65311,#65312,
#65313,#65314,#65315,#65316,#65317,#65318,#65319,#65320,#65321,#65322,#65323,
#65324,#65325,#65326,#65327,#65328,#65329,#65330,#65331,#65332,#65333,#65334,
#65335,#65336,#65337,#65338,#65339,#65340,#65341,#65342,#65343,#65344,#65345,
#65346,#65347,#65348,#65349,#65350,#65351,#65352,#65353,#65354,#65355,#65356,
#65357,#65358,#65359,#65360,#65361,#65362,#65363,#65364,#65365,#65366,#65367,
#65368,#65369,#65370,#65371,#65372,#65373,#65374,#65375,#65376,#65377,#65378,
#65379,#65380,#65381,#65382,#65383,#65384,#65385,#65386,#65387,#65388,#65389,
#65390,#65391,#65392,#65393,#65394,#65395,#65396,#65397,#65398,#65399,#65400,
#65401,#65402,#65403,#65404,#65405,#65406,#65407,#65408,#65409,#65410,#65411,
#65412,#65413,#65414,#65415,#65416,#65417,#65418,#65419,#65420,#65421,#65422,
#65423,#65424,#65425,#65426,#65427,#65428,#65429,#65430,#65431,#65432,#65433,
#65434,#65435,#65436,#65437,#65438,#65439,#65440,#65441,#65442,#65443,#65444,
#65445,#65446,#65447,#65448,#65449,#65450,#65451,#65452,#65453,#65454,#65455,
#65456,#65457,#65458,#65459,#65460,#65461,#65462,#65463,#65464,#65465,#65466,
#65467,#65468,#65469,#65470,#65471,#65472,#65473,#65474,#65475,#65476,#65477,
#65478,#65479,#65480,#65481,#65482,#65483,#65484,#65485),.UNSPECIFIED.,
 .F.,.F.,(4,3,3,3,3,3,3,3,3,3,3,3,3,3,3,3,3,3,3,3,3,3,3,3,3,3,3,3,3,3,3,
3,3,3,3,3,3,3,3,3,3,3,3,3,3,3,3,3,3,3,3,3,3,3,3,3,3,3,3,3,3,3,3,3,3,3,3,
3,3,3,4),(19.9487183364793,20.0414927127207,20.1341536551306,20.2267293285119,
20.3192599426483,20.4117721022213,20.5042923885719,20.5969045224113,20.6895660174233,
20.7823763144016,20.8419778816025,20.9359677062525,21.0298310356222,21.1235961181127,
21.2172946430643,21.3109593081937,21.4046154949344,21.4982885705689,21.5920618232911,
21.6858900241134,21.7798686716303,21.8344530188217,21.9284428432923,22.0223061724728,
22.1160712547648,22.209769779504,22.3034344444127,22.3970906309247,22.4907637063224,
22.5845369587974,22.678365159366,22.7723438066217,22.8269281560409,22.9209179812708,
23.0147813112232,23.1085463942984,23.2022449198351,23.2959095855495,23.3895657728746,
23.4832388490922,23.5770121023914,23.6708403037884,23.7648189518703,23.8194032932601,
23.9133931181127,24.0072564476835,24.1010215303731,24.1947200555196,24.2883847208415,
24.3820409077721,24.4757139835937,24.569487236497,24.6633154374973,24.7572940851858,
24.8118784304792,24.9058682553442,24.9997315849265,25.0934966676268,25.1871951927831,
25.2808598581141,25.374516045053,25.4681891208814,25.5619623737908,25.6557905747963,
25.7497692224888,25.8043535676984,25.9112410865558,26.0132189365589,26.1149468961578,
26.216320556494,26.2319036431278),.UNSPECIFIED.);
#1448=B_SPLINE_CURVE_WITH_KNOTS('',3,(#65487,#65488,#65489,#65490,#65491,
#65492,#65493,#65494,#65495,#65496,#65497,#65498,#65499,#65500,#65501,#65502,
#65503,#65504,#65505,#65506,#65507,#65508,#65509,#65510,#65511,#65512,#65513,
#65514,#65515,#65516,#65517,#65518,#65519,#65520,#65521,#65522,#65523,#65524,
#65525,#65526,#65527,#65528,#65529,#65530,#65531,#65532,#65533,#65534,#65535,
#65536,#65537,#65538,#65539,#65540,#65541,#65542,#65543,#65544,#65545,#65546,
#65547,#65548,#65549,#65550,#65551,#65552,#65553,#65554,#65555,#65556,#65557,
#65558,#65559,#65560,#65561,#65562,#65563,#65564,#65565,#65566,#65567,#65568,
#65569,#65570,#65571,#65572,#65573,#65574,#65575,#65576,#65577,#65578,#65579,
#65580,#65581,#65582,#65583,#65584,#65585,#65586,#65587,#65588,#65589,#65590,
#65591,#65592,#65593,#65594,#65595,#65596,#65597,#65598,#65599,#65600,#65601,
#65602,#65603,#65604,#65605,#65606,#65607,#65608,#65609,#65610,#65611,#65612,
#65613,#65614,#65615,#65616,#65617,#65618,#65619,#65620,#65621,#65622,#65623,
#65624,#65625,#65626,#65627,#65628,#65629,#65630,#65631,#65632,#65633,#65634,
#65635,#65636,#65637,#65638,#65639,#65640,#65641,#65642,#65643,#65644,#65645,
#65646,#65647,#65648,#65649,#65650,#65651,#65652,#65653,#65654,#65655,#65656,
#65657,#65658,#65659,#65660,#65661,#65662,#65663,#65664,#65665,#65666,#65667,
#65668,#65669,#65670,#65671,#65672,#65673,#65674,#65675,#65676,#65677,#65678,
#65679,#65680,#65681,#65682,#65683,#65684,#65685,#65686,#65687,#65688,#65689,
#65690,#65691,#65692,#65693,#65694,#65695,#65696,#65697),.UNSPECIFIED.,
 .F.,.F.,(4,3,3,3,3,3,3,3,3,3,3,3,3,3,3,3,3,3,3,3,3,3,3,3,3,3,3,3,3,3,3,
3,3,3,3,3,3,3,3,3,3,3,3,3,3,3,3,3,3,3,3,3,3,3,3,3,3,3,3,3,3,3,3,3,3,3,3,
3,3,3,4),(26.2319036434442,26.3276115682817,26.423375181536,26.519294850849,
26.6152944080368,26.7114937996171,26.7968287049176,26.8908185298198,26.9846818594401,
27.0784469421796,27.1721454673759,27.2658101327474,27.3594663197274,27.4531393955981,
27.54691264855,27.6407408495986,27.7347194973344,27.7893038421367,27.8832936670454,
27.9771569966723,28.0709220794184,28.164620604621,28.2582852699989,28.3519414569851,
28.4456145328617,28.5393877858197,28.6332159868743,28.7271946346159,28.7817789793559,
28.8757688042752,28.9696321339128,29.0633972166698,29.1570957418837,29.2507604072728,
29.3444165942707,29.4380896701591,29.5318629231286,29.625691124195,29.7196697719483,
29.7742541165751,29.8682439414868,29.9621072711167,30.0558723538656,30.1495708790716,
30.2432355444527,30.3368917314425,30.4305648073228,30.5243380602843,30.6181662613425,
30.7121449090877,30.7667292537942,30.8607190787074,30.954582408339,31.0483474910895,
31.142046016297,31.2357106816797,31.3293668686707,31.4230399445526,31.5168131975156,
31.6106413985755,31.7046200463222,31.7592043910134,31.8536899609647,31.9463790432336,
32.0389818453475,32.1315250528619,32.2274160273024,32.3199469364277,32.4124932923736,
32.5051109026203,32.5150889506238),.UNSPECIFIED.);
#1449=B_SPLINE_CURVE_WITH_KNOTS('',3,(#65699,#65700,#65701,#65702,#65703,
#65704,#65705,#65706,#65707,#65708,#65709),.UNSPECIFIED.,.F.,.F.,(4,1,1,
1,1,1,1,1,4),(32.5150893692119,32.7516795282326,33.7441546654517,34.7366298026709,
35.7291049398901,36.7215800771092,37.7140552143284,38.7065303515476,38.7982742578034),
 .UNSPECIFIED.);
#1450=B_SPLINE_CURVE_WITH_KNOTS('',3,(#65711,#65712,#65713,#65714,#65715,
#65716,#65717,#65718,#65719,#65720,#65721,#65722,#65723,#65724,#65725,#65726,
#65727,#65728,#65729,#65730,#65731,#65732,#65733,#65734,#65735,#65736,#65737,
#65738,#65739,#65740,#65741,#65742,#65743,#65744,#65745,#65746,#65747,#65748,
#65749,#65750,#65751,#65752,#65753,#65754,#65755,#65756,#65757,#65758,#65759,
#65760,#65761,#65762,#65763,#65764,#65765,#65766,#65767,#65768,#65769,#65770,
#65771,#65772,#65773,#65774,#65775,#65776,#65777,#65778,#65779,#65780,#65781,
#65782,#65783,#65784,#65785,#65786,#65787,#65788,#65789,#65790,#65791,#65792,
#65793,#65794,#65795,#65796,#65797,#65798,#65799,#65800,#65801,#65802,#65803,
#65804,#65805,#65806,#65807,#65808,#65809,#65810,#65811,#65812,#65813,#65814,
#65815,#65816,#65817,#65818,#65819,#65820,#65821,#65822,#65823,#65824,#65825,
#65826,#65827,#65828,#65829,#65830,#65831,#65832,#65833,#65834,#65835,#65836,
#65837,#65838,#65839,#65840,#65841,#65842,#65843,#65844,#65845,#65846,#65847,
#65848,#65849,#65850,#65851,#65852,#65853,#65854,#65855,#65856,#65857,#65858,
#65859,#65860,#65861,#65862,#65863,#65864,#65865,#65866,#65867,#65868,#65869,
#65870,#65871,#65872,#65873,#65874,#65875,#65876,#65877,#65878,#65879,#65880,
#65881,#65882,#65883,#65884,#65885,#65886,#65887,#65888,#65889,#65890,#65891,
#65892,#65893,#65894,#65895,#65896,#65897,#65898,#65899,#65900,#65901,#65902,
#65903,#65904,#65905,#65906,#65907,#65908,#65909,#65910,#65911,#65912,#65913,
#65914,#65915,#65916,#65917,#65918),.UNSPECIFIED.,.F.,.F.,(4,3,3,3,3,3,
3,3,3,3,3,3,3,3,3,3,3,3,3,3,3,3,3,3,3,3,3,3,3,3,3,3,3,3,3,3,3,3,3,3,3,3,
3,3,3,3,3,3,3,3,3,3,3,3,3,3,3,3,3,3,3,3,3,3,3,3,3,3,3,4),(38.7982742578034,
38.8911077810691,38.9838262178453,39.0764570669745,39.1690412837208,39.2616054304404,
39.3541760447021,39.4468376766205,39.5395470952447,39.632407528133,39.6990054887667,
39.7929953136803,39.8868586433119,39.9806237260628,40.0743222512708,40.1679869166541,
40.2616431036457,40.355316179528,40.4490894324914,40.5429176335517,40.636896281299,
40.6914806259859,40.7854704508995,40.8793337805316,40.9730988632824,41.0667973884904,
41.1604620538735,41.2541182408653,41.3477913167472,41.4415645697106,41.5353927707708,
41.6293714185179,41.6839557632051,41.7779455881187,41.8718089177506,41.9655740005019,
42.0592725257098,42.152937191093,42.2465933780846,42.340266453967,42.4340397069304,
42.5278679079905,42.6218465557376,42.6764309004243,42.770420725338,42.8642840549696,
42.9580491377205,43.0517476629285,43.1454123283117,43.2390685153034,43.3327415911854,
43.4265148441489,43.5203430452093,43.6143216929564,43.6689060376434,43.762895862557,
43.8567591921892,43.9505242749404,44.0442228001483,44.1378874655315,44.2315436525232,
44.3252167284053,44.4189899813687,44.5128181824287,44.6067968301759,44.6613811748626,
44.7664007723502,44.8688416746821,44.9751506197477,45.0814595648132),
 .UNSPECIFIED.);
#1451=B_SPLINE_CURVE_WITH_KNOTS('',3,(#65920,#65921,#65922,#65923,#65924,
#65925,#65926,#65927,#65928,#65929,#65930,#65931,#65932,#65933,#65934,#65935,
#65936,#65937,#65938,#65939,#65940,#65941,#65942,#65943,#65944,#65945,#65946,
#65947,#65948,#65949,#65950,#65951,#65952,#65953,#65954,#65955,#65956,#65957,
#65958,#65959,#65960,#65961,#65962,#65963,#65964,#65965,#65966,#65967,#65968,
#65969,#65970,#65971,#65972,#65973,#65974,#65975,#65976,#65977,#65978,#65979,
#65980,#65981,#65982,#65983,#65984,#65985,#65986,#65987,#65988,#65989,#65990,
#65991,#65992,#65993,#65994,#65995,#65996,#65997,#65998,#65999,#66000,#66001,
#66002,#66003,#66004,#66005,#66006,#66007,#66008,#66009,#66010,#66011,#66012,
#66013,#66014,#66015,#66016,#66017,#66018,#66019,#66020,#66021,#66022,#66023,
#66024,#66025,#66026,#66027,#66028,#66029,#66030,#66031,#66032,#66033,#66034,
#66035,#66036,#66037,#66038,#66039,#66040,#66041,#66042,#66043,#66044,#66045,
#66046,#66047,#66048,#66049,#66050,#66051,#66052,#66053,#66054,#66055,#66056,
#66057,#66058,#66059,#66060,#66061,#66062,#66063,#66064,#66065,#66066,#66067,
#66068,#66069,#66070,#66071,#66072,#66073,#66074,#66075,#66076,#66077,#66078,
#66079,#66080,#66081,#66082,#66083,#66084,#66085,#66086,#66087,#66088,#66089,
#66090,#66091,#66092,#66093,#66094,#66095,#66096,#66097,#66098,#66099,#66100,
#66101,#66102,#66103,#66104,#66105,#66106,#66107,#66108,#66109,#66110,#66111,
#66112,#66113,#66114,#66115,#66116,#66117,#66118,#66119,#66120,#66121,#66122,
#66123,#66124,#66125,#66126,#66127),.UNSPECIFIED.,.F.,.F.,(4,3,3,3,3,3,
3,3,3,3,3,3,3,3,3,3,3,3,3,3,3,3,3,3,3,3,3,3,3,3,3,3,3,3,3,3,3,3,3,3,3,3,
3,3,3,3,3,3,3,3,3,3,3,3,3,3,3,3,3,3,3,3,3,3,3,3,3,3,3,4),(45.081459564983,
45.1769592542972,45.2725075662283,45.3682050177821,45.4639772739664,45.5599488925284,
45.6538563120818,45.7478461369954,45.8417094666272,45.9354745493782,46.0291730745861,
46.1228377399692,46.2164939269609,46.310167002843,46.4039402558063,46.4977684568664,
46.5917471046135,46.6463314493009,46.7403212742146,46.8341846038464,46.9279496865972,
47.0216482118051,47.1153128771883,47.2089690641801,47.3026421400624,47.3964153930259,
47.4902435940862,47.5842222418335,47.6388065865201,47.7327964114337,47.8266597410655,
47.9204248238163,48.0141233490243,48.1077880144075,48.2014442013991,48.2951172772811,
48.3888905302445,48.4827187313046,48.5766973790517,48.6312817237393,48.7252715486528,
48.8191348782849,48.9128999610356,49.0065984862435,49.1002631516265,49.1939193386183,
49.2875924145003,49.3813656674637,49.4751938685238,49.569172516271,49.6237568609584,
49.717746685872,49.811610015504,49.9053750982546,49.9990736234626,50.0927382888457,
50.1863944758373,50.28006755172,50.3738408046834,50.4676690057437,50.5616476534909,
50.6162319981776,50.7097836074257,50.8025276215215,50.8951845324334,50.9877809804665,
51.0819969533905,51.1745774864197,51.2696111792911,51.3646448721626),
 .UNSPECIFIED.);
#1452=B_SPLINE_CURVE_WITH_KNOTS('',3,(#66129,#66130,#66131,#66132,#66133,
#66134,#66135,#66136,#66137,#66138,#66139),.UNSPECIFIED.,.F.,.F.,(4,1,1,
1,1,1,1,1,4),(51.3646459623497,51.6087071353968,52.601182272616,53.5936574098351,
54.5861325470543,55.5786076842735,56.5710828214926,57.5635579587118,57.6478301793422),
 .UNSPECIFIED.);
#1453=B_SPLINE_CURVE_WITH_KNOTS('',3,(#66141,#66142,#66143,#66144,#66145,
#66146,#66147,#66148,#66149,#66150,#66151,#66152,#66153,#66154,#66155,#66156,
#66157,#66158,#66159,#66160,#66161,#66162,#66163,#66164,#66165,#66166,#66167,
#66168,#66169,#66170,#66171,#66172,#66173,#66174,#66175,#66176,#66177,#66178,
#66179,#66180,#66181,#66182,#66183,#66184,#66185,#66186,#66187,#66188,#66189,
#66190,#66191,#66192,#66193,#66194,#66195,#66196,#66197,#66198,#66199,#66200,
#66201,#66202,#66203,#66204,#66205,#66206,#66207,#66208,#66209,#66210,#66211,
#66212,#66213,#66214,#66215,#66216,#66217,#66218,#66219,#66220,#66221,#66222,
#66223,#66224,#66225,#66226,#66227,#66228,#66229,#66230,#66231,#66232,#66233,
#66234,#66235,#66236,#66237,#66238,#66239,#66240,#66241,#66242,#66243,#66244,
#66245,#66246,#66247,#66248,#66249,#66250,#66251,#66252,#66253,#66254,#66255,
#66256,#66257,#66258,#66259,#66260,#66261,#66262,#66263,#66264,#66265,#66266,
#66267,#66268,#66269,#66270,#66271,#66272,#66273,#66274,#66275,#66276,#66277,
#66278,#66279,#66280,#66281,#66282,#66283,#66284,#66285,#66286,#66287,#66288,
#66289,#66290,#66291,#66292,#66293,#66294,#66295,#66296,#66297,#66298,#66299,
#66300,#66301,#66302,#66303,#66304,#66305,#66306,#66307,#66308,#66309,#66310,
#66311,#66312,#66313,#66314,#66315,#66316,#66317,#66318,#66319,#66320,#66321,
#66322,#66323,#66324,#66325,#66326,#66327,#66328,#66329,#66330,#66331,#66332,
#66333,#66334,#66335,#66336,#66337,#66338,#66339,#66340,#66341,#66342,#66343,
#66344,#66345,#66346,#66347,#66348),.UNSPECIFIED.,.F.,.F.,(4,3,3,3,3,3,
3,3,3,3,3,3,3,3,3,3,3,3,3,3,3,3,3,3,3,3,3,3,3,3,3,3,3,3,3,3,3,3,3,3,3,3,
3,3,3,3,3,3,3,3,3,3,3,3,3,3,3,3,3,3,3,3,3,3,3,3,3,3,3,4),(57.6478301793422,
57.7407280669645,57.8335093047544,57.9262007371352,58.0188440325848,58.1114657054143,
58.2040922438032,58.2968090105251,58.3895720306128,58.4824883121618,58.556033095931,
58.6500229208446,58.7438862504766,58.8376513332274,58.9313498584353,59.0250145238185,
59.1186707108101,59.2123437866921,59.3061170396555,59.3999452407157,59.4939238884629,
59.5485082331501,59.6424980580633,59.7363613876947,59.8301264704455,59.9238249956531,
60.017489661036,60.1111458480273,60.2048189239094,60.2985921768725,60.3924203779325,
60.4863990256793,60.5409833703693,60.6349731952839,60.7288365249167,60.8226016076682,
60.9163001328769,61.0099647982609,61.1036209852534,61.1972940611366,61.2910673141008,
61.3848955151621,61.4788741629101,61.5334585075885,61.6274483325016,61.7213116621329,
61.8150767448828,61.9087752700902,62.0024399354729,62.0960961224641,62.1897691983459,
62.2835424513088,62.3773706523686,62.4713493001154,62.5259336448076,62.6199234697194,
62.713786799349,62.8075518820985,62.9012504073045,62.9949150726858,63.0885712596754,
63.1822443355558,63.2760175885173,63.3698457895758,63.4638244373211,63.5184087820268,
63.6215975387392,63.7245199877336,63.8277677370369,63.9310154863402),
 .UNSPECIFIED.);
#1454=B_SPLINE_CURVE_WITH_KNOTS('',3,(#66350,#66351,#66352,#66353,#66354,
#66355,#66356,#66357,#66358,#66359,#66360,#66361,#66362,#66363,#66364,#66365,
#66366,#66367,#66368,#66369,#66370,#66371,#66372,#66373,#66374,#66375,#66376,
#66377,#66378,#66379,#66380,#66381,#66382,#66383,#66384,#66385,#66386,#66387,
#66388,#66389,#66390,#66391,#66392,#66393,#66394,#66395,#66396,#66397,#66398,
#66399,#66400,#66401,#66402,#66403,#66404,#66405,#66406,#66407,#66408,#66409,
#66410,#66411,#66412,#66413,#66414,#66415,#66416,#66417,#66418,#66419,#66420,
#66421,#66422,#66423,#66424,#66425,#66426,#66427,#66428,#66429,#66430,#66431,
#66432,#66433,#66434,#66435,#66436,#66437,#66438,#66439,#66440,#66441,#66442,
#66443,#66444,#66445,#66446,#66447,#66448,#66449,#66450,#66451,#66452,#66453,
#66454,#66455,#66456,#66457,#66458,#66459,#66460,#66461,#66462,#66463,#66464,
#66465,#66466,#66467,#66468,#66469,#66470,#66471,#66472,#66473,#66474,#66475,
#66476,#66477,#66478,#66479,#66480,#66481,#66482,#66483,#66484,#66485,#66486,
#66487,#66488,#66489,#66490,#66491,#66492,#66493,#66494,#66495,#66496,#66497,
#66498,#66499,#66500,#66501,#66502,#66503,#66504,#66505,#66506,#66507,#66508,
#66509,#66510,#66511,#66512,#66513,#66514,#66515,#66516,#66517,#66518,#66519,
#66520,#66521,#66522,#66523,#66524,#66525,#66526,#66527,#66528,#66529,#66530,
#66531,#66532,#66533,#66534,#66535,#66536,#66537,#66538,#66539,#66540,#66541,
#66542,#66543,#66544,#66545,#66546,#66547,#66548,#66549,#66550,#66551,#66552,
#66553,#66554,#66555,#66556,#66557),.UNSPECIFIED.,.F.,.F.,(4,3,3,3,3,3,
3,3,3,3,3,3,3,3,3,3,3,3,3,3,3,3,3,3,3,3,3,3,3,3,3,3,3,3,3,3,3,3,3,3,3,3,
3,3,3,3,3,3,3,3,3,3,3,3,3,3,3,3,3,3,3,3,3,3,3,3,3,3,3,4),(63.9310154865217,
64.0263152239147,64.1216568579874,64.2189636233021,64.3145192288704,64.4127015740582,
64.510883919246,64.6048737441539,64.6987370737801,64.7925021565253,64.8862006817278,
64.9798653471056,65.0735215340919,65.1671946099688,65.260967862927,65.3547960639822,
65.4487747117244,65.5033590564651,65.5973488813674,65.6912122109878,65.7849772937273,
65.8786758189237,65.9723404842952,66.0659966712754,66.1596697471461,66.2534430000979,
66.3472712011466,66.4412498488823,66.4958341936843,66.5898240186435,66.6836873483209,
66.7774524311176,66.8711509563712,66.9648156217999,67.058471808837,67.1521448847643,
67.2459181377723,67.3397463388767,67.4337249866672,67.4883093309035,67.5822991557625,
67.6761624853401,67.7699275680371,67.8636260931917,67.9572907585219,68.0509469454611,
68.1446200212909,68.2383932742035,68.3322214752134,68.4262001229117,68.4807844681226,
68.5747742929777,68.6686376225504,68.7624027052413,68.8561012303887,68.9497658957111,
69.0434220826416,69.1370951584623,69.2308684113642,69.324696612363,69.4186752600488,
69.4732596053418,69.5661785353861,69.65898289471,69.751699366492,69.8443545393512,
69.9370009516695,70.0296366765961,70.1223440423424,70.2142007937013),
 .UNSPECIFIED.);
#1455=B_SPLINE_CURVE_WITH_KNOTS('',3,(#66559,#66560,#66561,#66562,#66563,
#66564,#66565,#66566,#66567,#66568,#66569,#66570,#66571,#66572,#66573,#66574,
#66575,#66576,#66577,#66578,#66579,#66580,#66581,#66582,#66583,#66584,#66585,
#66586,#66587,#66588,#66589,#66590,#66591,#66592,#66593,#66594,#66595,#66596,
#66597,#66598,#66599,#66600,#66601,#66602,#66603,#66604,#66605,#66606,#66607,
#66608,#66609,#66610,#66611,#66612,#66613,#66614,#66615,#66616,#66617,#66618,
#66619,#66620,#66621,#66622,#66623,#66624,#66625,#66626,#66627,#66628,#66629,
#66630,#66631,#66632,#66633,#66634,#66635,#66636,#66637,#66638,#66639,#66640,
#66641,#66642,#66643,#66644,#66645,#66646,#66647,#66648,#66649,#66650,#66651,
#66652,#66653,#66654,#66655,#66656,#66657,#66658,#66659,#66660,#66661,#66662,
#66663,#66664,#66665,#66666,#66667,#66668,#66669,#66670,#66671,#66672,#66673,
#66674,#66675,#66676,#66677,#66678,#66679,#66680,#66681,#66682,#66683,#66684,
#66685,#66686,#66687,#66688,#66689,#66690,#66691,#66692,#66693,#66694,#66695,
#66696,#66697,#66698,#66699,#66700,#66701,#66702,#66703,#66704,#66705,#66706,
#66707,#66708,#66709,#66710,#66711,#66712,#66713,#66714,#66715,#66716,#66717,
#66718,#66719,#66720,#66721,#66722,#66723,#66724,#66725,#66726,#66727,#66728,
#66729,#66730,#66731,#66732,#66733,#66734,#66735,#66736,#66737,#66738,#66739,
#66740,#66741,#66742,#66743,#66744,#66745,#66746,#66747,#66748,#66749,#66750,
#66751,#66752,#66753,#66754,#66755,#66756,#66757,#66758,#66759,#66760,#66761,
#66762,#66763,#66764,#66765,#66766,#66767,#66768,#66769),.UNSPECIFIED.,
 .F.,.F.,(4,3,3,3,3,3,3,3,3,3,3,3,3,3,3,3,3,3,3,3,3,3,3,3,3,3,3,3,3,3,3,
3,3,3,3,3,3,3,3,3,3,3,3,3,3,3,3,3,3,3,3,3,3,3,3,3,3,3,3,3,3,3,3,3,3,3,3,
3,3,3,4),(70.2142007939207,70.3334640590779,70.4552451164889,70.465734742561,
70.5597245669846,70.6535878961274,70.7473529783913,70.8410515031168,70.9347161680207,
71.0283723545367,71.1220454299474,71.2158186824487,71.3096468830513,71.4036255303524,
71.4582098797801,71.552199704465,71.6460630338625,71.7398281163739,71.8335266413357,
71.9271913064686,72.0208474932064,72.1145205688314,72.2082938215339,72.302122022331,
72.3961006698139,72.4506850169993,72.544674844279,72.6385381762844,72.732303261413,
72.826001788995,72.919666456749,73.0133226461056,73.1069957243438,73.2007689796352,
73.2945971830111,73.3885758330317,73.4431601542185,73.5371499749457,73.6310133003967,
73.724778378978,73.8184769000496,73.9121415613188,74.0057977442235,74.0994708160508,
74.1932440650325,74.2870722621464,74.3810509060418,74.4356352914376,74.5296251162456,
74.6234884457315,74.7172535282968,74.8109520532614,74.9046167183659,74.9982729050441,
75.0919459805785,75.1857192331444,75.2795474337786,75.3735260810593,75.4281104286568,
75.5221002698313,75.6159636157889,75.709728714908,75.8034272564792,75.8970919382164,
75.9907481415329,76.0844212336906,76.1781945027555,76.2720227198425,76.366001383341,
76.420585565876,76.4973861008809),.UNSPECIFIED.);
#1456=B_SPLINE_CURVE_WITH_KNOTS('',3,(#66771,#66772,#66773,#66774,#66775,
#66776,#66777,#66778,#66779,#66780),.UNSPECIFIED.,.F.,.F.,(4,1,1,1,1,1,
1,4),(76.4973940480353,77.4130607030951,78.4055358403143,79.3980109775335,
80.3904861147527,81.3829612519718,82.375436389191,82.780565175451),
 .UNSPECIFIED.);
#1457=B_SPLINE_CURVE_WITH_KNOTS('',3,(#66782,#66783,#66784,#66785,#66786,
#66787,#66788,#66789,#66790,#66791,#66792,#66793,#66794,#66795,#66796,#66797,
#66798,#66799,#66800,#66801,#66802,#66803,#66804,#66805,#66806,#66807,#66808,
#66809,#66810,#66811,#66812,#66813,#66814,#66815,#66816,#66817,#66818,#66819,
#66820,#66821,#66822,#66823,#66824,#66825,#66826,#66827,#66828,#66829,#66830,
#66831,#66832,#66833,#66834,#66835,#66836,#66837,#66838,#66839,#66840,#66841,
#66842,#66843,#66844,#66845,#66846,#66847,#66848,#66849,#66850,#66851,#66852,
#66853,#66854,#66855,#66856,#66857,#66858,#66859,#66860,#66861,#66862,#66863,
#66864,#66865,#66866,#66867,#66868,#66869,#66870,#66871,#66872,#66873,#66874,
#66875,#66876,#66877,#66878,#66879,#66880,#66881,#66882,#66883,#66884,#66885,
#66886,#66887,#66888,#66889,#66890,#66891,#66892,#66893,#66894,#66895,#66896,
#66897,#66898,#66899,#66900,#66901,#66902,#66903,#66904,#66905,#66906,#66907,
#66908,#66909,#66910,#66911,#66912,#66913,#66914,#66915,#66916,#66917,#66918,
#66919,#66920,#66921,#66922,#66923,#66924,#66925,#66926,#66927,#66928,#66929,
#66930,#66931,#66932,#66933,#66934,#66935,#66936,#66937,#66938,#66939,#66940,
#66941,#66942,#66943,#66944,#66945,#66946,#66947,#66948,#66949,#66950,#66951,
#66952,#66953,#66954,#66955,#66956,#66957,#66958,#66959,#66960,#66961,#66962,
#66963,#66964,#66965,#66966,#66967,#66968,#66969,#66970,#66971,#66972,#66973,
#66974,#66975,#66976,#66977,#66978,#66979,#66980,#66981,#66982,#66983,#66984,
#66985,#66986,#66987,#66988,#66989,#66990,#66991,#66992),.UNSPECIFIED.,
 .F.,.F.,(4,3,3,3,3,3,3,3,3,3,3,3,3,3,3,3,3,3,3,3,3,3,3,3,3,3,3,3,3,3,3,
3,3,3,3,3,3,3,3,3,3,3,3,3,3,3,3,3,3,3,3,3,3,3,3,3,3,3,3,3,3,3,3,3,3,3,3,
3,3,3,4),(82.7805714080605,82.8756769963287,82.9708180774348,83.0700914396786,
83.165437152978,83.2608693513861,83.3564641921791,83.3679115264102,83.461903274698,
83.5557685153425,83.6495354943892,83.7432358864185,83.8369023997384,83.9305604136443,
84.0242352932622,84.1180103039131,84.211840239249,84.3058205675134,84.3603866636293,
84.4543804594747,84.5482477945329,84.6420169113679,84.7357194963243,84.8293882357292,
84.9230485059173,85.0167256690785,85.110502990458,85.2043352552119,85.2983179190271,
85.3528618008485,85.4468357700119,85.5406832175902,85.6344324134189,85.7281151096413,
85.8217639877295,85.9154044481434,86.0090618772467,86.1028196996842,86.1966325696502,
86.2905961935937,86.3453369380677,86.4393455013607,86.5332274937779,86.6270111399809,
86.720728005926,86.8144108676545,86.9080850852006,87.0017760043043,87.0955667082914,
87.1894121644862,87.28340759052,87.3378120752868,87.4318226025838,87.5257068980905,
87.6194931783374,87.7132131551182,87.806899420454,87.900577328163,87.9942722180067,
88.0880672920136,88.1819173497577,88.2759176933972,88.330287212506,88.4231787283098,
88.515954847165,88.6086422726807,88.701267612456,88.7938817763749,88.8864846860942,
88.9791544786862,89.0637567152401),.UNSPECIFIED.);
#1458=B_SPLINE_CURVE_WITH_KNOTS('',3,(#66994,#66995,#66996,#66997,#66998,
#66999,#67000,#67001,#67002,#67003,#67004,#67005,#67006,#67007,#67008,#67009,
#67010,#67011,#67012,#67013,#67014,#67015,#67016,#67017,#67018,#67019,#67020,
#67021,#67022,#67023,#67024,#67025,#67026,#67027,#67028,#67029,#67030,#67031,
#67032,#67033,#67034,#67035,#67036,#67037,#67038,#67039,#67040,#67041,#67042,
#67043,#67044,#67045,#67046,#67047,#67048,#67049,#67050,#67051,#67052,#67053,
#67054,#67055,#67056,#67057,#67058,#67059,#67060,#67061,#67062,#67063,#67064,
#67065,#67066,#67067,#67068,#67069),.UNSPECIFIED.,.F.,.F.,(4,3,3,3,3,3,
3,3,3,3,3,3,3,3,3,3,3,3,3,3,3,3,3,3,3,4),(89.063756715403,89.1813412978231,
89.3011841336904,89.3227623497252,89.4169215726789,89.5109538690648,89.6048872632074,
89.6987524320014,89.7925826418988,89.8864030729481,89.9802388899363,90.074171613325,
90.1681576637385,90.262290075529,90.3152374869443,90.4088618846611,90.5023619137458,
90.5994770169613,90.6928170034203,90.7861273482923,90.8794338519026,90.9727623043365,
91.0661922230418,91.159682460239,91.253313733231,91.2792827394697),
 .UNSPECIFIED.);
#1459=B_SPLINE_CURVE_WITH_KNOTS('',3,(#67073,#67074,#67075,#67076,#67077),
 .UNSPECIFIED.,.F.,.F.,(4,1,4),(-93.2926628986018,-92.3001877613827,-92.0203418336781),
 .UNSPECIFIED.);
#1460=B_SPLINE_CURVE_WITH_KNOTS('',3,(#67079,#67080,#67081,#67082,#67083,
#67084,#67085,#67086,#67087,#67088),.UNSPECIFIED.,.F.,.F.,(4,1,1,1,1,1,
1,4),(-92.0203418336781,-91.3077126241635,-90.3152374869444,-89.3227623497252,
-88.330287212506,-87.3378120752868,-86.3453369380677,-85.7371565264985),
 .UNSPECIFIED.);
#1461=B_SPLINE_CURVE_WITH_KNOTS('',3,(#67090,#67091,#67092,#67093,#67094,
#67095,#67096,#67097,#67098,#67099,#67100,#67101,#67102,#67103,#67104,#67105,
#67106,#67107,#67108,#67109,#67110,#67111,#67112,#67113,#67114,#67115,#67116,
#67117,#67118,#67119,#67120,#67121,#67122,#67123,#67124,#67125,#67126,#67127,
#67128,#67129,#67130,#67131,#67132,#67133,#67134,#67135,#67136,#67137,#67138,
#67139,#67140,#67141,#67142,#67143,#67144,#67145,#67146,#67147,#67148,#67149,
#67150,#67151,#67152,#67153,#67154,#67155,#67156,#67157,#67158,#67159,#67160,
#67161,#67162,#67163,#67164,#67165,#67166,#67167,#67168,#67169,#67170,#67171,
#67172,#67173,#67174,#67175,#67176,#67177,#67178,#67179,#67180,#67181,#67182,
#67183,#67184,#67185,#67186,#67187,#67188,#67189,#67190,#67191,#67192,#67193,
#67194,#67195,#67196,#67197,#67198,#67199,#67200,#67201,#67202,#67203,#67204,
#67205,#67206,#67207,#67208,#67209,#67210,#67211,#67212,#67213,#67214,#67215,
#67216,#67217,#67218,#67219,#67220,#67221,#67222,#67223,#67224,#67225,#67226,
#67227,#67228,#67229,#67230,#67231,#67232,#67233,#67234,#67235,#67236,#67237,
#67238,#67239,#67240,#67241,#67242,#67243,#67244,#67245,#67246,#67247,#67248,
#67249,#67250,#67251,#67252,#67253,#67254,#67255,#67256,#67257,#67258,#67259,
#67260,#67261,#67262,#67263,#67264,#67265,#67266,#67267,#67268,#67269,#67270,
#67271,#67272,#67273,#67274,#67275,#67276,#67277,#67278,#67279,#67280,#67281,
#67282,#67283,#67284,#67285,#67286,#67287,#67288,#67289,#67290,#67291,#67292,
#67293,#67294,#67295,#67296,#67297),.UNSPECIFIED.,.F.,.F.,(4,3,3,3,3,3,
3,3,3,3,3,3,3,3,3,3,3,3,3,3,3,3,3,3,3,3,3,3,3,3,3,3,3,3,3,3,3,3,3,3,3,3,
3,3,3,3,3,3,3,3,3,3,3,3,3,3,3,3,3,3,3,3,3,3,3,3,3,3,3,4),(-85.7371563039944,
-85.632809300152,-85.5280804819151,-85.4228292623581,-85.3528618008485,
-85.2588679527554,-85.1650005706409,-85.0712314119546,-84.9775287930657,
-84.8838600246363,-84.7901997303596,-84.6965225480777,-84.6027452152697,
-84.5089129434122,-84.4149302793837,-84.3603866636294,-84.2663951665026,
-84.1725301249216,-84.0787632930732,-83.9850629704441,-83.8913964784107,
-83.7977384377239,-83.704063483264,-83.6102883249328,-83.5164582005907,
-83.4224776200041,-83.3679115264102,-83.273923687219,-83.1800623731564,
-83.0862993328493,-82.9926028817128,-82.8989403091757,-82.8052862312469,
-82.7116152780994,-82.6178441559045,-82.5240180932625,-82.430041575035,
-82.375436389191,-82.2814458914497,-82.1875818826862,-82.0938161154856,
-82.0001169007732,-81.9064515430276,-81.8127946616749,-81.7191208902913,
-81.6253469443368,-81.5315180506916,-81.4375387178315,-81.3829612519718,
-81.2889712841214,-81.1951078072733,-81.1013425732528,-81.0076438913324,
-80.9139790659265,-80.8203227157901,-80.7266494738271,-80.6328760512805,
-80.5390476784111,-80.4450688570051,-80.3904861147527,-80.2972774958163,
-80.2041947611772,-80.1104168184663,-80.0174951058634,-79.9246039336365,
-79.8317170561381,-79.7372805969761,-79.6442735644754,-79.5491223919828,
-79.4539712194903),.UNSPECIFIED.);
#1462=B_SPLINE_CURVE_WITH_KNOTS('',3,(#67299,#67300,#67301,#67302,#67303,
#67304,#67305,#67306,#67307,#67308,#67309,#67310,#67311,#67312,#67313,#67314,
#67315,#67316,#67317,#67318,#67319,#67320,#67321,#67322,#67323,#67324,#67325,
#67326,#67327,#67328,#67329,#67330,#67331,#67332,#67333,#67334,#67335,#67336,
#67337,#67338,#67339,#67340,#67341,#67342,#67343,#67344,#67345,#67346,#67347,
#67348,#67349,#67350,#67351,#67352,#67353,#67354,#67355,#67356,#67357,#67358,
#67359,#67360,#67361,#67362,#67363,#67364,#67365,#67366,#67367,#67368,#67369,
#67370,#67371,#67372,#67373,#67374,#67375,#67376,#67377,#67378,#67379,#67380,
#67381,#67382,#67383,#67384,#67385,#67386,#67387,#67388,#67389,#67390,#67391,
#67392,#67393,#67394,#67395,#67396,#67397,#67398,#67399,#67400,#67401,#67402,
#67403,#67404,#67405,#67406,#67407,#67408,#67409,#67410,#67411,#67412,#67413,
#67414,#67415,#67416,#67417,#67418,#67419,#67420,#67421,#67422,#67423,#67424,
#67425,#67426,#67427,#67428,#67429,#67430,#67431,#67432,#67433,#67434,#67435,
#67436,#67437,#67438,#67439,#67440,#67441,#67442,#67443,#67444,#67445,#67446,
#67447,#67448,#67449,#67450,#67451,#67452,#67453,#67454,#67455,#67456,#67457,
#67458,#67459,#67460,#67461,#67462,#67463,#67464,#67465,#67466,#67467,#67468,
#67469,#67470,#67471,#67472,#67473,#67474,#67475,#67476,#67477,#67478,#67479,
#67480,#67481,#67482,#67483,#67484,#67485,#67486,#67487,#67488,#67489,#67490,
#67491,#67492,#67493,#67494,#67495,#67496,#67497,#67498,#67499,#67500,#67501,
#67502,#67503,#67504,#67505,#67506,#67507,#67508,#67509),.UNSPECIFIED.,
 .F.,.F.,(4,3,3,3,3,3,3,3,3,3,3,3,3,3,3,3,3,3,3,3,3,3,3,3,3,3,3,3,3,3,3,
3,3,3,3,3,3,3,3,3,3,3,3,3,3,3,3,3,3,3,3,3,3,3,3,3,3,3,3,3,3,3,3,3,3,3,3,
3,3,3,4),(-79.4539712193189,-79.3980109775335,-79.3040210470638,-79.2101576107371,
-79.1163924203078,-79.0226937864058,-78.9290290117422,-78.835372715019,
-78.7416995290889,-78.6479261662656,-78.5540978552912,-78.4601190986269,
-78.4055358403143,-78.3115460075673,-78.2176826696829,-78.123917578274,
-78.0302190438356,-77.936554368871,-77.8428981719575,-77.7492250858235,
-77.6554518221633,-77.5616236101392,-77.4676449511111,-77.4130607030952,
-77.3190709101445,-77.2252076130074,-77.1314425632348,-77.0377440715906,
-76.9440794401205,-76.85042328735,-76.756750245956,-76.6629770276805,-76.5691488614716,
-76.4751702484923,-76.420585565876,-76.3265957251464,-76.2327323795108,
-76.1389672805919,-76.0452687390383,-75.9516040572061,-75.857947853682,
-75.7642747612044,-75.6705014916504,-75.576673273978,-75.4826946097481,
-75.4281104286568,-75.3341206042293,-75.2402572750495,-75.1464921927161,
-75.0527936678719,-74.959129002819,-74.8654728161236,-74.7717997405032,
-74.6780264877467,-74.5841982868627,-74.4902196392412,-74.4356352914376,
-74.3416454703856,-74.2477821446834,-74.1540170659243,-74.0603185447847,
-73.9666538835156,-73.8729977006788,-73.7793246289871,-73.6855513802437,
-73.5917231834264,-73.4977445399164,-73.4431601542185,-73.325149510274,
-73.2090479125567,-73.1707860257054),.UNSPECIFIED.);
#1463=B_SPLINE_CURVE_WITH_KNOTS('',3,(#67511,#67512,#67513,#67514,#67515,
#67516,#67517,#67518,#67519,#67520),.UNSPECIFIED.,.F.,.F.,(4,1,1,1,1,1,
1,4),(-73.1707859121394,-72.4506850169993,-71.4582098797801,-70.465734742561,
-69.4732596053418,-68.4807844681226,-67.4883093309035,-66.8876006049598),
 .UNSPECIFIED.);
#1464=B_SPLINE_CURVE_WITH_KNOTS('',3,(#67522,#67523,#67524,#67525,#67526,
#67527,#67528,#67529,#67530,#67531,#67532,#67533,#67534,#67535,#67536,#67537,
#67538,#67539,#67540,#67541,#67542,#67543,#67544,#67545,#67546,#67547,#67548,
#67549,#67550,#67551,#67552,#67553,#67554,#67555,#67556,#67557,#67558,#67559,
#67560,#67561,#67562,#67563,#67564,#67565,#67566,#67567,#67568,#67569,#67570,
#67571,#67572,#67573,#67574,#67575,#67576,#67577,#67578,#67579,#67580,#67581,
#67582,#67583,#67584,#67585,#67586,#67587,#67588,#67589,#67590,#67591,#67592,
#67593,#67594,#67595,#67596,#67597,#67598,#67599,#67600,#67601,#67602,#67603,
#67604,#67605,#67606,#67607,#67608,#67609,#67610,#67611,#67612,#67613,#67614,
#67615,#67616,#67617,#67618,#67619,#67620,#67621,#67622,#67623,#67624,#67625,
#67626,#67627,#67628,#67629,#67630,#67631,#67632,#67633,#67634,#67635,#67636,
#67637,#67638,#67639,#67640,#67641,#67642,#67643,#67644,#67645,#67646,#67647,
#67648,#67649,#67650,#67651,#67652,#67653,#67654,#67655,#67656,#67657,#67658,
#67659,#67660,#67661,#67662,#67663,#67664,#67665,#67666,#67667,#67668,#67669,
#67670,#67671,#67672,#67673,#67674,#67675,#67676,#67677,#67678,#67679,#67680,
#67681,#67682,#67683,#67684,#67685,#67686,#67687,#67688,#67689,#67690,#67691,
#67692,#67693,#67694,#67695,#67696,#67697,#67698,#67699,#67700,#67701,#67702,
#67703,#67704,#67705,#67706,#67707,#67708,#67709,#67710,#67711,#67712,#67713,
#67714,#67715,#67716,#67717,#67718,#67719,#67720,#67721,#67722,#67723,#67724,
#67725,#67726,#67727,#67728,#67729),.UNSPECIFIED.,.F.,.F.,(4,3,3,3,3,3,
3,3,3,3,3,3,3,3,3,3,3,3,3,3,3,3,3,3,3,3,3,3,3,3,3,3,3,3,3,3,3,3,3,3,3,3,
3,3,3,3,3,3,3,3,3,3,3,3,3,3,3,3,3,3,3,3,3,3,3,3,3,3,3,4),(-66.8876003895016,
-66.7837700712268,-66.6795867770187,-66.5749020761923,-66.4958341936843,
-66.4018443687823,-66.3079810391619,-66.2142159564225,-66.1205174312264,
-66.0268527658549,-65.933196578875,-65.8395235030045,-65.7457502500528,
-65.6519220490043,-65.5579434012686,-65.5033590564651,-65.4093692315565,
-65.3155059019297,-65.221740819184,-65.1280422939814,-65.0343776286037,
-64.9407214416174,-64.8470483657408,-64.753275112783,-64.6594469117285,
-64.565468263987,-64.510883919246,-64.4168940943267,-64.3230307646889,-64.229265681932,
-64.1355671567181,-64.0419024913288,-63.9482463043309,-63.8545732284425,
-63.7607999754729,-63.6669717744064,-63.572993126653,-63.5184087820268,
-63.4244189571151,-63.3305556274852,-63.2367905447362,-63.1430920195302,
-63.049427354149,-62.9557711671592,-62.862098091279,-62.7683248383175,-62.6744966372593,
-62.580517989514,-62.5259336448076,-62.4319438198945,-62.3380804902631,
-62.2443154075127,-62.1506168823053,-62.0569522169226,-61.9632960299315,
-61.8696229540498,-61.7758497010869,-61.6820215000272,-61.5880428522806,
-61.5334585075885,-61.4403288883763,-61.3473250707808,-61.2544247374575,
-61.1615812526724,-61.0687682618145,-60.9759594442223,-60.8830700660323,
-60.7901426869388,-60.6970626347649,-60.6044152979652),.UNSPECIFIED.);
#1465=B_SPLINE_CURVE_WITH_KNOTS('',3,(#67731,#67732,#67733,#67734,#67735,
#67736,#67737,#67738,#67739,#67740,#67741,#67742,#67743,#67744,#67745,#67746,
#67747,#67748,#67749,#67750,#67751,#67752,#67753,#67754,#67755,#67756,#67757,
#67758,#67759,#67760,#67761,#67762,#67763,#67764,#67765,#67766,#67767,#67768,
#67769,#67770,#67771,#67772,#67773,#67774,#67775,#67776,#67777,#67778,#67779,
#67780,#67781,#67782,#67783,#67784,#67785,#67786,#67787,#67788,#67789,#67790,
#67791,#67792,#67793,#67794,#67795,#67796,#67797,#67798,#67799,#67800,#67801,
#67802,#67803,#67804,#67805,#67806,#67807,#67808,#67809,#67810,#67811,#67812,
#67813,#67814,#67815,#67816,#67817,#67818,#67819,#67820,#67821,#67822,#67823,
#67824,#67825,#67826,#67827,#67828,#67829,#67830,#67831,#67832,#67833,#67834,
#67835,#67836,#67837,#67838,#67839,#67840,#67841,#67842,#67843,#67844,#67845,
#67846,#67847,#67848,#67849,#67850,#67851,#67852,#67853,#67854,#67855,#67856,
#67857,#67858,#67859,#67860,#67861,#67862,#67863,#67864,#67865,#67866,#67867,
#67868,#67869,#67870,#67871,#67872,#67873,#67874,#67875,#67876,#67877,#67878,
#67879,#67880,#67881,#67882,#67883,#67884,#67885,#67886,#67887,#67888,#67889,
#67890,#67891,#67892,#67893,#67894,#67895,#67896,#67897,#67898,#67899,#67900,
#67901,#67902,#67903,#67904,#67905,#67906,#67907,#67908,#67909,#67910,#67911,
#67912,#67913,#67914,#67915,#67916,#67917,#67918,#67919,#67920,#67921,#67922,
#67923,#67924,#67925,#67926,#67927,#67928,#67929,#67930,#67931,#67932,#67933,
#67934,#67935,#67936,#67937,#67938,#67939,#67940,#67941),.UNSPECIFIED.,
 .F.,.F.,(4,3,3,3,3,3,3,3,3,3,3,3,3,3,3,3,3,3,3,3,3,3,3,3,3,3,3,3,3,3,3,
3,3,3,3,3,3,3,3,3,3,3,3,3,3,3,3,3,3,3,3,3,3,3,3,3,3,3,3,3,3,3,3,3,3,3,3,
3,3,3,4),(-60.6044152977802,-60.5409833703693,-60.4469935454563,-60.3531302158249,
-60.2593651330745,-60.1656666078671,-60.0720019424845,-59.9783457554934,
-59.8846726796118,-59.7908994266489,-59.6970712255893,-59.6030925778426,
-59.5485082331501,-59.4545184082364,-59.3606550786044,-59.2668899958533,
-59.1731914706452,-59.0795268052619,-58.98587061827,-58.8921975423876,-58.7984242894241,
-58.7045960883637,-58.6106174406164,-58.556033095931,-58.4620432710174,
-58.3681799413855,-58.2744148586345,-58.1807163334265,-58.0870516680433,
-57.9933954810515,-57.8997224051692,-57.8059491522057,-57.7121209511454,
-57.6181423033982,-57.5635579587118,-57.4695681337982,-57.3757048041664,
-57.2819397214155,-57.1882411962076,-57.0945765308244,-57.0009203438327,
-56.9072472679505,-56.8134740149871,-56.7196458139269,-56.6256671661798,
-56.5710828214926,-56.477092996579,-56.3832296669472,-56.2894645841962,
-56.1957660589883,-56.1021013936051,-56.0084452066135,-55.9147721307313,
-55.8209988777679,-55.7271706767077,-55.6331920289605,-55.5786076842735,
-55.4846178593599,-55.390754529728,-55.2969894469769,-55.203290921769,-55.1096262563858,
-55.0159700693942,-54.9222969935119,-54.8285237405484,-54.7346955394881,
-54.6407168917409,-54.5861325470543,-54.4668321488865,-54.3496326388445,
-54.3212299907803),.UNSPECIFIED.);
#1466=B_SPLINE_CURVE_WITH_KNOTS('',3,(#67943,#67944,#67945,#67946,#67947,
#67948,#67949,#67950,#67951,#67952,#67953,#67954,#67955,#67956,#67957,#67958,
#67959,#67960,#67961,#67962,#67963,#67964,#67965,#67966,#67967,#67968,#67969,
#67970,#67971,#67972,#67973,#67974,#67975,#67976,#67977,#67978,#67979,#67980,
#67981,#67982,#67983,#67984,#67985,#67986,#67987,#67988,#67989,#67990,#67991,
#67992,#67993,#67994,#67995,#67996,#67997,#67998,#67999,#68000,#68001,#68002,
#68003,#68004,#68005,#68006,#68007,#68008,#68009,#68010,#68011,#68012,#68013,
#68014,#68015,#68016,#68017,#68018,#68019,#68020,#68021,#68022,#68023,#68024,
#68025,#68026,#68027,#68028,#68029,#68030,#68031,#68032,#68033,#68034,#68035,
#68036,#68037,#68038,#68039,#68040,#68041,#68042,#68043,#68044,#68045,#68046,
#68047,#68048,#68049,#68050,#68051,#68052,#68053,#68054,#68055,#68056,#68057,
#68058,#68059,#68060,#68061,#68062,#68063,#68064,#68065,#68066,#68067,#68068,
#68069,#68070,#68071,#68072,#68073,#68074,#68075,#68076,#68077,#68078,#68079,
#68080,#68081,#68082,#68083,#68084,#68085,#68086,#68087,#68088,#68089,#68090,
#68091,#68092,#68093,#68094,#68095,#68096,#68097,#68098,#68099,#68100,#68101,
#68102,#68103,#68104,#68105,#68106,#68107,#68108,#68109,#68110,#68111,#68112,
#68113,#68114,#68115,#68116,#68117,#68118,#68119,#68120,#68121,#68122,#68123,
#68124,#68125,#68126,#68127,#68128,#68129,#68130,#68131,#68132,#68133,#68134,
#68135,#68136,#68137,#68138,#68139,#68140,#68141,#68142,#68143,#68144,#68145,
#68146,#68147,#68148,#68149,#68150,#68151,#68152,#68153),.UNSPECIFIED.,
 .F.,.F.,(4,3,3,3,3,3,3,3,3,3,3,3,3,3,3,3,3,3,3,3,3,3,3,3,3,3,3,3,3,3,3,
3,3,3,3,3,3,3,3,3,3,3,3,3,3,3,3,3,3,3,3,3,3,3,3,3,3,3,3,3,3,3,3,3,3,3,3,
3,3,3,4),(-54.3212299906006,-54.2284183110393,-54.1356537708416,-54.0429099834603,
-53.950160587367,-53.8573191213051,-53.7644310102756,-53.6713864992433,
-53.5936574098351,-53.4996675849215,-53.4058042552895,-53.3120391725386,
-53.2183406473307,-53.1246759819475,-53.0310197949558,-52.9373467190735,
-52.8435734661101,-52.7497452650498,-52.6557666173027,-52.601182272616,
-52.5071924477025,-52.4133291180705,-52.3195640353194,-52.2258655101115,
-52.1322008447283,-52.0385446577366,-51.9448715818547,-51.8510983288913,
-51.757270127831,-51.6632914800839,-51.6087071353968,-51.5147173104833,
-51.4208539808515,-51.3270888981007,-51.2333903728928,-51.1397257075096,
-51.0460695205179,-50.9523964446358,-50.8586231916724,-50.764794990612,
-50.6708163428648,-50.6162319981776,-50.522242173264,-50.4283788436319,
-50.334613760881,-50.240915235673,-50.1472505702897,-50.0535943832979,-49.9599213074159,
-49.8661480544523,-49.772319853392,-49.6783412056449,-49.6237568609584,
-49.5297670360449,-49.4359037064131,-49.3421386236626,-49.2484400984547,
-49.1547754330715,-49.0611192460799,-48.9674461701977,-48.8736729172343,
-48.7798447161742,-48.6858660684269,-48.6312817237393,-48.5358676688867,
-48.4405923974443,-48.3454327805398,-48.2503808034438,-48.1553913922474,
-48.060442494842,-48.038044683421),.UNSPECIFIED.);
#1467=B_SPLINE_CURVE_WITH_KNOTS('',3,(#68155,#68156,#68157,#68158,#68159,
#68160,#68161,#68162,#68163,#68164),.UNSPECIFIED.,.F.,.F.,(4,1,1,1,1,1,
1,4),(-48.0380382192525,-47.6388065865201,-46.6463314493009,-45.6538563120818,
-44.6613811748626,-43.6689060376434,-42.6764309004243,-41.7548670354255),
 .UNSPECIFIED.);
#1468=B_SPLINE_CURVE_WITH_KNOTS('',3,(#68166,#68167,#68168,#68169,#68170,
#68171,#68172,#68173,#68174,#68175,#68176,#68177,#68178,#68179,#68180,#68181,
#68182,#68183,#68184,#68185,#68186,#68187,#68188,#68189,#68190,#68191,#68192,
#68193,#68194,#68195,#68196,#68197,#68198,#68199,#68200,#68201,#68202,#68203,
#68204,#68205,#68206,#68207,#68208,#68209,#68210,#68211,#68212,#68213,#68214,
#68215,#68216,#68217,#68218,#68219,#68220,#68221,#68222,#68223,#68224,#68225,
#68226,#68227,#68228,#68229,#68230,#68231,#68232,#68233,#68234,#68235,#68236,
#68237,#68238,#68239,#68240,#68241,#68242,#68243,#68244,#68245,#68246,#68247,
#68248,#68249,#68250,#68251,#68252,#68253,#68254,#68255,#68256,#68257,#68258,
#68259,#68260,#68261,#68262,#68263,#68264,#68265,#68266,#68267,#68268,#68269,
#68270,#68271,#68272,#68273,#68274,#68275,#68276,#68277,#68278,#68279,#68280,
#68281,#68282,#68283,#68284,#68285,#68286,#68287,#68288,#68289,#68290,#68291,
#68292,#68293,#68294,#68295,#68296,#68297,#68298,#68299,#68300,#68301,#68302,
#68303,#68304,#68305,#68306,#68307,#68308,#68309,#68310,#68311,#68312,#68313,
#68314,#68315,#68316,#68317,#68318,#68319,#68320,#68321,#68322,#68323,#68324,
#68325,#68326,#68327,#68328,#68329,#68330,#68331,#68332,#68333,#68334,#68335,
#68336,#68337,#68338,#68339,#68340,#68341,#68342,#68343,#68344,#68345,#68346,
#68347,#68348,#68349,#68350,#68351,#68352,#68353,#68354,#68355,#68356,#68357,
#68358,#68359,#68360,#68361,#68362,#68363,#68364,#68365,#68366,#68367,#68368,
#68369,#68370,#68371,#68372,#68373,#68374,#68375,#68376),.UNSPECIFIED.,
 .F.,.F.,(4,3,3,3,3,3,3,3,3,3,3,3,3,3,3,3,3,3,3,3,3,3,3,3,3,3,3,3,3,3,3,
3,3,3,3,3,3,3,3,3,3,3,3,3,3,3,3,3,3,3,3,3,3,3,3,3,3,3,3,3,3,3,3,3,3,3,3,
3,3,3,4),(-41.7548593762414,-41.6839557632051,-41.5899659382915,-41.4961026086598,
-41.4023375259089,-41.308639000701,-41.2149743353178,-41.1213181483262,
-41.0276450724441,-40.9338718194807,-40.8400436184206,-40.7460649706734,
-40.6914806259859,-40.5974908010722,-40.5036274714403,-40.4098623886892,
-40.3161638634812,-40.222499198098,-40.1288430111062,-40.0351699352239,
-39.9413966822604,-39.8475684812001,-39.7535898334529,-39.6990054887667,
-39.6050156638532,-39.5111523342213,-39.4173872514704,-39.3236887262625,
-39.2300240608794,-39.1363678738877,-39.0426947980056,-38.9489215450422,
-38.855093343982,-38.7611146962348,-38.7065303515476,-38.612540526634,-38.5186771970021,
-38.4249121142512,-38.3312135890432,-38.2375489236601,-38.1438927366683,
-38.0502196607861,-37.9564464078227,-37.8626182067624,-37.7686395590152,
-37.7140552143284,-37.6200653894147,-37.5262020597829,-37.4324369770319,
-37.3387384518239,-37.2450737864407,-37.151417599449,-37.0577445235668,
-36.9639712706034,-36.8701430695431,-36.7761644217959,-36.7215800771092,
-36.6275902521957,-36.5337269225639,-36.439961839813,-36.3462633146052,
-36.2525986492221,-36.1589424622304,-36.0652693863482,-35.9714961333848,
-35.8776679323247,-35.7836892845776,-35.7291049398901,-35.6084268596164,
-35.4900717265883,-35.4716740693444),.UNSPECIFIED.);
#1469=B_SPLINE_CURVE_WITH_KNOTS('',3,(#68378,#68379,#68380,#68381,#68382,
#68383,#68384,#68385,#68386,#68387,#68388,#68389,#68390,#68391,#68392,#68393,
#68394,#68395,#68396,#68397,#68398,#68399,#68400,#68401,#68402,#68403,#68404,
#68405,#68406,#68407,#68408,#68409,#68410,#68411,#68412,#68413,#68414,#68415,
#68416,#68417,#68418,#68419,#68420,#68421,#68422,#68423,#68424,#68425,#68426,
#68427,#68428,#68429,#68430,#68431,#68432,#68433,#68434,#68435,#68436,#68437,
#68438,#68439,#68440,#68441,#68442,#68443,#68444,#68445,#68446,#68447,#68448,
#68449,#68450,#68451,#68452,#68453,#68454,#68455,#68456,#68457,#68458,#68459,
#68460,#68461,#68462,#68463,#68464,#68465,#68466,#68467,#68468,#68469,#68470,
#68471,#68472,#68473,#68474,#68475,#68476,#68477,#68478,#68479,#68480,#68481,
#68482,#68483,#68484,#68485,#68486,#68487,#68488,#68489,#68490,#68491,#68492,
#68493,#68494,#68495,#68496,#68497,#68498,#68499,#68500,#68501,#68502,#68503,
#68504,#68505,#68506,#68507,#68508,#68509,#68510,#68511,#68512,#68513,#68514,
#68515,#68516,#68517,#68518,#68519,#68520,#68521,#68522,#68523,#68524,#68525,
#68526,#68527,#68528,#68529,#68530,#68531,#68532,#68533,#68534,#68535,#68536,
#68537,#68538,#68539,#68540,#68541,#68542,#68543,#68544,#68545,#68546,#68547,
#68548,#68549,#68550,#68551,#68552,#68553,#68554,#68555,#68556,#68557,#68558,
#68559,#68560,#68561,#68562,#68563,#68564,#68565,#68566,#68567,#68568,#68569,
#68570,#68571,#68572,#68573,#68574,#68575,#68576,#68577,#68578,#68579,#68580,
#68581,#68582,#68583,#68584,#68585,#68586,#68587,#68588),.UNSPECIFIED.,
 .F.,.F.,(4,3,3,3,3,3,3,3,3,3,3,3,3,3,3,3,3,3,3,3,3,3,3,3,3,3,3,3,3,3,3,
3,3,3,3,3,3,3,3,3,3,3,3,3,3,3,3,3,3,3,3,3,3,3,3,3,3,3,3,3,3,3,3,3,3,3,3,
3,3,3,4),(-35.4716740690618,-35.3789228982328,-35.2862219687801,-35.1935448239753,
-35.1008650350535,-35.0080954319963,-34.9152817146125,-34.8223097482569,
-34.7366298026709,-34.6426399777574,-34.5487766481253,-34.4550115653746,
-34.3613130401666,-34.2676483747836,-34.173992187792,-34.08031911191,-33.9865458589465,
-33.8927176578865,-33.7987390101393,-33.7441546654517,-33.6501648405385,
-33.556301510907,-33.4625364281562,-33.3688379029486,-33.2751732375657,
-33.1815170505743,-33.0878439746921,-32.994070721729,-32.9002425206692,
-32.8062638729223,-32.7516795282326,-32.6576897033182,-32.5638263736856,
-32.4700612909339,-32.376362765725,-32.2826981003411,-32.1890419133485,
-32.0953688374656,-32.0015955845014,-31.9077673834402,-31.8137887356923,
-31.7592043910134,-31.6652145661003,-31.571351236469,-31.4775861537182,
-31.3838876285108,-31.290222963128,-31.1965667761368,-31.1028937002547,
-31.0091204472917,-30.915292246232,-30.8213135984851,-30.7667292537942,
-30.6727394288825,-30.5788760992527,-30.4851110165036,-30.3914124912977,
-30.2977478259166,-30.2040916389268,-30.110418563047,-30.0166453100855,
-29.9228171090273,-29.8288384612821,-29.7742541165751,-29.6786386681049,
-29.5831643289439,-29.4844954371785,-29.3892549266595,-29.294079326632,
-29.198949630498,-29.1884887618822),.UNSPECIFIED.);
#1470=B_SPLINE_CURVE_WITH_KNOTS('',3,(#68590,#68591,#68592,#68593,#68594,
#68595,#68596,#68597,#68598,#68599),.UNSPECIFIED.,.F.,.F.,(4,1,1,1,1,1,
1,4),(-29.1884825968197,-28.7817789793559,-27.7893038421367,-26.7968287049176,
-25.8043535676984,-24.8118784304792,-23.81940329326,-22.9053114674703),
 .UNSPECIFIED.);
#1471=B_SPLINE_CURVE_WITH_KNOTS('',3,(#68601,#68602,#68603,#68604,#68605,
#68606,#68607,#68608,#68609,#68610,#68611,#68612,#68613,#68614,#68615,#68616,
#68617,#68618,#68619,#68620,#68621,#68622,#68623,#68624,#68625,#68626,#68627,
#68628,#68629,#68630,#68631,#68632,#68633,#68634,#68635,#68636,#68637,#68638,
#68639,#68640,#68641,#68642,#68643,#68644,#68645,#68646,#68647,#68648,#68649,
#68650,#68651,#68652,#68653,#68654,#68655,#68656,#68657,#68658,#68659,#68660,
#68661,#68662,#68663,#68664,#68665,#68666,#68667,#68668,#68669,#68670,#68671,
#68672,#68673,#68674,#68675,#68676,#68677,#68678,#68679,#68680,#68681,#68682,
#68683,#68684,#68685,#68686,#68687,#68688,#68689,#68690,#68691,#68692,#68693,
#68694,#68695,#68696,#68697,#68698,#68699,#68700,#68701,#68702,#68703,#68704,
#68705,#68706,#68707,#68708,#68709,#68710,#68711,#68712,#68713,#68714,#68715,
#68716,#68717,#68718,#68719,#68720,#68721,#68722,#68723,#68724,#68725,#68726,
#68727,#68728,#68729,#68730,#68731,#68732,#68733,#68734,#68735,#68736,#68737,
#68738,#68739,#68740,#68741,#68742,#68743,#68744,#68745,#68746,#68747,#68748,
#68749,#68750,#68751,#68752,#68753,#68754,#68755,#68756,#68757,#68758,#68759,
#68760,#68761,#68762,#68763,#68764,#68765,#68766,#68767,#68768,#68769,#68770,
#68771,#68772,#68773,#68774,#68775,#68776,#68777,#68778,#68779,#68780,#68781,
#68782,#68783,#68784,#68785,#68786,#68787,#68788,#68789,#68790,#68791,#68792,
#68793,#68794,#68795,#68796,#68797,#68798,#68799,#68800,#68801,#68802,#68803,
#68804,#68805,#68806,#68807,#68808),.UNSPECIFIED.,.F.,.F.,(4,3,3,3,3,3,
3,3,3,3,3,3,3,3,3,3,3,3,3,3,3,3,3,3,3,3,3,3,3,3,3,3,3,3,3,3,3,3,3,3,3,3,
3,3,3,3,3,3,3,3,3,3,3,3,3,3,3,3,3,3,3,3,3,3,3,3,3,3,3,4),(-22.9053034547026,
-22.8269281560409,-22.732938331622,-22.6390750024836,-22.5453099202241,
-22.451611395503,-22.3579467306036,-22.2642905440919,-22.1706174686853,
-22.0768442161883,-21.9830160155899,-21.8890373682928,-21.8344530188217,
-21.7404631941409,-21.6465998647475,-21.5528347822404,-21.4591362572829,
-21.3654715921543,-21.2718154054209,-21.1781423298004,-21.0843690771022,
-20.9905408763096,-20.8965622288311,-20.8419778816025,-20.7479880542975,
-20.6541247222668,-20.5603596371129,-20.4666611095056,-20.3729964417263,
-20.2793402523445,-20.1856671740813,-20.0918939187651,-19.9980657153645,
-19.9040870653197,-19.8495027443834,-19.7555129236932,-19.661649598279,
-19.5678845197346,-19.4741859986994,-19.3805213374666,-19.2868651545979,
-19.1931920828063,-19.0994188338597,-19.0055906367805,-18.911611992919,
-18.8570276071642,-18.7630377823695,-18.6691744528973,-18.575409370346,
-18.4817108453957,-18.388046180306,-18.2943899936429,-18.2007169181238,
-18.1069436655733,-18.0131154649549,-17.9191368176901,-17.864552469945,
-17.7705626286161,-17.6766992825034,-17.5829341832289,-17.4892356415025,
-17.3955709596102,-17.3019147561389,-17.2082416638269,-17.1144683946094,
-17.0206401773705,-16.9266615137229,-16.8720773327259,-16.7470977402257,
-16.6221181477255),.UNSPECIFIED.);
#1472=B_SPLINE_CURVE_WITH_KNOTS('',3,(#68810,#68811,#68812,#68813,#68814,
#68815,#68816,#68817,#68818,#68819,#68820,#68821,#68822,#68823,#68824,#68825,
#68826,#68827,#68828,#68829,#68830,#68831,#68832,#68833,#68834,#68835,#68836,
#68837,#68838,#68839,#68840,#68841,#68842,#68843,#68844,#68845,#68846,#68847,
#68848,#68849,#68850,#68851,#68852,#68853,#68854,#68855,#68856,#68857,#68858,
#68859,#68860,#68861,#68862,#68863,#68864,#68865,#68866,#68867,#68868,#68869,
#68870,#68871,#68872,#68873,#68874,#68875,#68876,#68877,#68878,#68879,#68880,
#68881,#68882,#68883,#68884,#68885,#68886,#68887,#68888,#68889,#68890,#68891,
#68892,#68893,#68894,#68895,#68896,#68897,#68898,#68899,#68900,#68901,#68902,
#68903,#68904,#68905,#68906,#68907,#68908,#68909,#68910,#68911,#68912,#68913,
#68914,#68915,#68916,#68917,#68918,#68919,#68920,#68921,#68922,#68923,#68924,
#68925,#68926,#68927,#68928,#68929,#68930,#68931,#68932,#68933,#68934,#68935,
#68936,#68937,#68938,#68939,#68940,#68941,#68942,#68943,#68944,#68945,#68946,
#68947,#68948,#68949,#68950,#68951,#68952,#68953,#68954,#68955,#68956,#68957,
#68958,#68959,#68960,#68961,#68962,#68963,#68964,#68965,#68966,#68967,#68968,
#68969,#68970,#68971,#68972,#68973,#68974,#68975,#68976,#68977,#68978,#68979,
#68980,#68981,#68982,#68983,#68984,#68985,#68986,#68987,#68988,#68989,#68990,
#68991,#68992,#68993,#68994,#68995,#68996,#68997,#68998,#68999,#69000,#69001,
#69002,#69003,#69004,#69005,#69006,#69007,#69008,#69009,#69010,#69011,#69012,
#69013,#69014,#69015,#69016,#69017),.UNSPECIFIED.,.F.,.F.,(4,3,3,3,3,3,
3,3,3,3,3,3,3,3,3,3,3,3,3,3,3,3,3,3,3,3,3,3,3,3,3,3,3,3,3,3,3,3,3,3,3,3,
3,3,3,3,3,3,3,3,3,3,3,3,3,3,3,3,3,3,3,3,3,3,3,3,3,3,3,4),(-16.622118147523,
-16.529303653521,-16.4366606337733,-16.3440443155275,-16.2514282096388,
-16.1584717061058,-16.0657261490512,-15.972664172279,-15.8796021955067,
-15.7856123593066,-15.6917490186731,-15.5979839252156,-15.5042853897803,
-15.4106207144692,-15.3169645178588,-15.2232914326779,-15.1295181709556,
-15.0356899614281,-14.9417113057535,-14.8871270582875,-14.7931371249199,
-14.6992736862861,-14.6055084941381,-14.5118098593999,-14.418145084446,
-14.324488787978,-14.2308156028486,-14.1370422416525,-14.0432139327744,
-13.9492351789253,-13.8946519210684,-13.8006623712746,-13.7067993168445,
-13.6130345090102,-13.5193362571705,-13.4256718640968,-13.3320159480289,
-13.238343141357,-13.1445701533681,-13.0507422152792,-12.9567638247687,
-12.9021767838492,-12.8081867855782,-12.7143232845114,-12.6205580324466,
-12.526859341746,-12.433194513289,-12.3395381658261,-12.2458649322607,-12.1520915267901,
-12.0582631759197,-11.9642843840604,-11.90970164663,-11.8157111396676,-11.7218471235632,
-11.6280813508929,-11.5343821335191,-11.4407167748487,-11.3470598943064,
-11.2533861254682,-11.1596121846898,-11.0657832977134,-10.9718039738099,
-10.9172265094109,-10.8214033407368,-10.7257237751919,-10.6290260414798,
-10.5335869751275,-10.4362599077354,-10.3389328403434),.UNSPECIFIED.);
#1473=B_SPLINE_CURVE_WITH_KNOTS('',3,(#69018,#69019,#69020,#69021,#69022,
#69023,#69024,#69025,#69026,#69027,#69028,#69029,#69030,#69031,#69032,#69033,
#69034,#69035,#69036,#69037,#69038,#69039,#69040,#69041,#69042,#69043,#69044,
#69045,#69046,#69047,#69048,#69049,#69050,#69051,#69052,#69053,#69054,#69055,
#69056,#69057,#69058,#69059,#69060,#69061,#69062,#69063,#69064,#69065,#69066,
#69067,#69068,#69069,#69070,#69071,#69072,#69073,#69074,#69075,#69076,#69077,
#69078,#69079,#69080,#69081,#69082,#69083,#69084,#69085,#69086,#69087,#69088,
#69089,#69090,#69091,#69092,#69093,#69094,#69095,#69096,#69097,#69098,#69099,
#69100,#69101,#69102,#69103,#69104,#69105,#69106,#69107,#69108,#69109,#69110,
#69111,#69112,#69113,#69114,#69115,#69116,#69117,#69118,#69119,#69120,#69121,
#69122,#69123,#69124,#69125,#69126,#69127,#69128,#69129,#69130,#69131,#69132,
#69133,#69134,#69135,#69136,#69137,#69138,#69139,#69140,#69141,#69142,#69143,
#69144,#69145,#69146,#69147,#69148,#69149,#69150,#69151,#69152,#69153,#69154,
#69155,#69156,#69157,#69158,#69159,#69160,#69161,#69162,#69163,#69164,#69165,
#69166,#69167,#69168,#69169,#69170,#69171,#69172,#69173,#69174,#69175,#69176,
#69177,#69178,#69179,#69180,#69181,#69182,#69183,#69184,#69185,#69186,#69187,
#69188,#69189,#69190,#69191,#69192,#69193,#69194,#69195,#69196,#69197,#69198,
#69199,#69200,#69201,#69202,#69203,#69204,#69205,#69206,#69207,#69208,#69209,
#69210,#69211,#69212,#69213,#69214,#69215,#69216,#69217,#69218,#69219,#69220,
#69221,#69222,#69223,#69224,#69225),.UNSPECIFIED.,.F.,.F.,(4,3,3,3,3,3,
3,3,3,3,3,3,3,3,3,3,3,3,3,3,3,3,3,3,3,3,3,3,3,3,3,3,3,3,3,3,3,3,3,3,3,3,
3,3,3,3,3,3,3,3,3,3,3,3,3,3,3,3,3,3,3,3,3,3,3,3,3,3,3,4),(-10.3389328401642,
-10.2353874731711,-10.1327533663568,-10.0287523692743,-9.92475137219169,
-9.83075961919574,-9.73689437390884,-9.64312739029071,-9.54942699381244,
-9.45576047612084,-9.36210245792533,-9.26842757410462,-9.17465255940701,
-9.08082262010667,-8.98684228804526,-8.93227623497251,-8.83828241309624,
-8.74441505185367,-8.6506459087176,-8.55694329739515,-8.46327453159424,
-8.36961423501245,-8.2759370454921,-8.18215969796653,-8.0883274071486,-7.99434471765517,
-7.93980109775335,-7.84582719101489,-7.75197980594718,-7.65823067263216,
-7.56454803867557,-7.47089922267758,-7.37725882410477,-7.28360145651992,
-7.18984369474053,-7.09603088503644,-7.00206732014101,-6.94732596053418,
-6.85331736490599,-6.75943534045618,-6.66565166255936,-6.57193476554713,
-6.47825187314932,-6.38457762536547,-6.29088667648968,-6.19709594361215,
-6.10325045898227,-6.0092550055028,-5.95485082331501,-5.86084016495999,
-5.76695573758775,-5.6731693248544,-5.57944921521557,-5.48576281684318,
-5.39208477608375,-5.29838975334033,-5.2045945474717,-5.11074435826087,
-5.01674388507031,-4.96237568609584,-4.86955617493606,-4.77686249766569,
-4.68427218947732,-4.59173829152433,-4.49923418079547,-4.40673326888904,
-4.31415439096147,-4.22153603551285,-4.12877526983171,-4.05574753337591),
 .UNSPECIFIED.);
#1474=B_SPLINE_CURVE_WITH_KNOTS('',3,(#69228,#69229,#69230,#69231,#69232,
#69233,#69234,#69235,#69236,#69237,#69238,#69239,#69240,#69241,#69242,#69243,
#69244,#69245,#69246,#69247,#69248,#69249,#69250,#69251,#69252,#69253,#69254,
#69255,#69256,#69257,#69258,#69259,#69260,#69261,#69262,#69263,#69264,#69265,
#69266,#69267,#69268,#69269,#69270,#69271,#69272,#69273,#69274,#69275,#69276,
#69277,#69278,#69279,#69280,#69281,#69282,#69283,#69284,#69285,#69286,#69287,
#69288,#69289,#69290,#69291,#69292,#69293,#69294,#69295,#69296,#69297,#69298,
#69299,#69300,#69301,#69302,#69303,#69304,#69305,#69306,#69307,#69308,#69309,
#69310,#69311,#69312,#69313,#69314,#69315,#69316,#69317,#69318,#69319,#69320,
#69321,#69322,#69323,#69324,#69325,#69326,#69327,#69328,#69329,#69330,#69331,
#69332,#69333,#69334,#69335,#69336,#69337,#69338,#69339,#69340,#69341,#69342,
#69343,#69344,#69345,#69346,#69347,#69348,#69349,#69350,#69351,#69352,#69353,
#69354,#69355,#69356,#69357,#69358,#69359,#69360,#69361,#69362,#69363,#69364,
#69365,#69366,#69367,#69368,#69369,#69370,#69371,#69372,#69373,#69374,#69375,
#69376,#69377,#69378,#69379,#69380,#69381,#69382,#69383,#69384,#69385,#69386,
#69387,#69388,#69389,#69390,#69391,#69392,#69393,#69394,#69395,#69396,#69397,
#69398,#69399,#69400,#69401,#69402,#69403,#69404,#69405),.UNSPECIFIED.,
 .F.,.F.,(4,2,2,2,2,2,2,2,2,2,2,2,2,2,2,2,2,2,2,2,2,2,2,2,2,2,2,2,2,2,2,
2,2,2,2,2,2,2,2,2,2,2,2,2,2,2,2,2,2,2,2,2,2,2,2,2,2,2,2,2,2,2,2,2,2,2,2,
2,2,2,2,2,2,2,2,2,2,2,2,2,2,2,2,2,2,2,2,2,4),(-1.42845765518849,-1.42536520723414,
-1.4152106799514,-1.40000645349711,-1.36537780576554,-1.32846426919925,
-1.31882578618782,-1.31264347562592,-1.30673031714364,-1.29849799497411,
-1.27686787775135,-1.24046462295499,-1.20495917778271,-1.19723313512881,
-1.19330464947426,-1.19003138756434,-1.1856591932015,-1.17547759035392,
-1.16021971512157,-1.10340153745338,-1.08502637211127,-1.07781251877794,
-1.07189100828158,-1.06580425026859,-1.05666856388179,-1.02610026476917,
-0.997564570479381,-0.965304109106234,-0.95753238642215,-0.953590449435717,
-0.950306827488488,-0.945920862623889,-0.935712633518282,-0.920403351779626,
-0.885711427188332,-0.849406801774189,-0.839776414519515,-0.833582840866373,
-0.827646045497534,-0.819357871285679,-0.797406078607802,-0.761087574562804,
-0.725841905691213,-0.718105712749734,-0.71417271863651,-0.710913120996444,
-0.706578428912307,-0.696512562638217,-0.68147964072391,-0.620541456282429,
-0.604153436769905,-0.5967882038272,-0.591011115083337,-0.584584856189687,
-0.573644959721232,-0.534751712525508,-0.49107109487792,-0.479935020943087,
-0.475754502458658,-0.472432773967653,-0.468828132279145,-0.462698685853784,
-0.43064954985613,-0.374149053004026,-0.36295465566877,-0.355808816948442,
-0.350000995585055,-0.343211633245007,-0.330703313246897,-0.314581297100423,
-0.280498153286423,-0.245926707479042,-0.238162651384305,-0.234201926234243,
-0.231189491043961,-0.226862069247317,-0.217320989971945,-0.203451483169819,
-0.148879497062157,-0.129098959834247,-0.121687509624381,-0.11620466799479,
-0.110150587183573,-0.101518505191228,-0.0772017292500017,-0.0430984593012172,
-0.0101131422229349,-0.00412518396300005,-0.00334863135138759),
 .UNSPECIFIED.);
#1475=B_SPLINE_CURVE_WITH_KNOTS('',3,(#69409,#69410,#69411,#69412,#69413,
#69414,#69415,#69416,#69417,#69418,#69419,#69420,#69421,#69422,#69423,#69424,
#69425,#69426,#69427,#69428,#69429,#69430,#69431,#69432,#69433,#69434,#69435,
#69436,#69437,#69438,#69439,#69440,#69441,#69442,#69443,#69444,#69445,#69446,
#69447,#69448,#69449,#69450,#69451,#69452,#69453,#69454,#69455,#69456,#69457,
#69458,#69459,#69460,#69461,#69462,#69463,#69464,#69465,#69466,#69467,#69468,
#69469,#69470,#69471,#69472,#69473,#69474,#69475,#69476,#69477,#69478,#69479,
#69480,#69481,#69482,#69483,#69484,#69485,#69486,#69487,#69488,#69489,#69490,
#69491,#69492,#69493,#69494,#69495,#69496,#69497,#69498,#69499,#69500,#69501,
#69502,#69503,#69504,#69505,#69506,#69507,#69508,#69509,#69510,#69511,#69512,
#69513,#69514,#69515,#69516,#69517,#69518,#69519,#69520,#69521,#69522,#69523,
#69524,#69525,#69526,#69527,#69528,#69529,#69530,#69531,#69532,#69533,#69534,
#69535),.UNSPECIFIED.,.F.,.F.,(4,3,3,3,3,3,3,3,3,3,3,3,3,3,3,3,3,3,3,3,
3,3,3,3,3,3,3,3,3,3,3,3,3,3,3,3,3,3,3,3,3,3,4),(97.3893722615554,97.518875078662,
97.6483778957685,97.7487851448158,97.8490491164149,97.9491968996414,98.0492810170443,
98.1493320356798,98.2493804817632,98.3495236236437,98.4497127805419,98.5500755985478,
98.6408530329877,98.7411830318357,98.8413724125209,98.9414499030046,99.0414663731791,
99.1414524608134,99.2414387653865,99.3415245228427,99.4416588133798,99.5419715975158,
99.6333281702069,99.7325582456431,99.8316450817934,99.9309148599975,100.029830533657,
100.128718182013,100.227609766748,100.327158151918,100.42621669172,100.526009999573,
100.625803307426,100.728742075655,100.831518076764,100.934132454852,101.036651773703,
101.139101194609,101.24150579755,101.343920147708,101.446334638376,101.548821984608,
101.618278444645),.UNSPECIFIED.);
#1476=B_SPLINE_CURVE_WITH_KNOTS('',3,(#69536,#69537,#69538,#69539,#69540,
#69541,#69542,#69543,#69544,#69545,#69546,#69547,#69548,#69549,#69550,#69551,
#69552,#69553),.UNSPECIFIED.,.F.,.F.,(4,2,2,2,2,2,2,2,4),(-3.03489337710244,
-2.99899587031306,-2.99021794071613,-2.98407651260254,-2.97800987248344,
-2.97215058911282,-2.96506738697773,-2.94742697701634,-2.94523236784797),
 .UNSPECIFIED.);
#1477=B_SPLINE_CURVE_WITH_KNOTS('',3,(#69558,#69559,#69560,#69561,#69562,
#69563,#69564,#69565,#69566,#69567,#69568,#69569,#69570,#69571,#69572,#69573,
#69574,#69575,#69576,#69577,#69578,#69579,#69580,#69581,#69582,#69583,#69584,
#69585,#69586,#69587,#69588,#69589,#69590,#69591,#69592,#69593,#69594,#69595,
#69596,#69597,#69598,#69599,#69600,#69601,#69602,#69603,#69604,#69605,#69606,
#69607,#69608,#69609,#69610,#69611,#69612,#69613,#69614,#69615,#69616,#69617,
#69618,#69619,#69620,#69621,#69622,#69623,#69624,#69625,#69626,#69627,#69628,
#69629,#69630,#69631,#69632,#69633,#69634,#69635,#69636,#69637,#69638,#69639,
#69640,#69641,#69642,#69643,#69644,#69645,#69646,#69647,#69648,#69649,#69650,
#69651),.UNSPECIFIED.,.F.,.F.,(4,3,3,3,3,3,3,3,3,3,3,3,3,3,3,3,3,3,3,3,
3,3,3,3,3,3,3,3,3,3,3,4),(-0.554646516726398,-0.550740972514746,-0.520307837848763,
-0.493932175372676,-0.486045706929786,-0.47859141274925,-0.448508884890132,
-0.418681489211896,-0.414805187944416,-0.409823971499447,-0.3807253319587,
-0.351958298846651,-0.324015927788516,-0.30764879626434,-0.30203888514984,
-0.297878709519076,-0.270514541794969,-0.258756835329769,-0.230309513510376,
-0.201862191690984,-0.196335053501894,-0.19215012140112,-0.165081508204436,
-0.138209907372373,-0.111603956434757,-0.103486289378542,-0.0966196945845564,
-0.0926311917683891,-0.066934469307677,-0.0416411581672595,-0.0171026713579872,
0.),.UNSPECIFIED.);
#1478=B_SPLINE_CURVE_WITH_KNOTS('',3,(#69653,#69654,#69655,#69656),
 .UNSPECIFIED.,.F.,.F.,(4,4),(0.,0.0117666873624648),.UNSPECIFIED.);
#1479=B_SPLINE_CURVE_WITH_KNOTS('',3,(#69657,#69658,#69659,#69660,#69661,
#69662,#69663,#69664,#69665,#69666,#69667,#69668,#69669,#69670,#69671,#69672,
#69673,#69674,#69675,#69676,#69677,#69678,#69679,#69680,#69681,#69682,#69683,
#69684,#69685,#69686,#69687,#69688,#69689,#69690,#69691,#69692,#69693,#69694,
#69695,#69696,#69697,#69698,#69699,#69700,#69701,#69702,#69703,#69704,#69705,
#69706,#69707,#69708,#69709,#69710,#69711,#69712,#69713,#69714,#69715,#69716,
#69717,#69718,#69719,#69720,#69721,#69722,#69723,#69724,#69725,#69726,#69727,
#69728,#69729,#69730,#69731,#69732,#69733,#69734,#69735,#69736,#69737,#69738,
#69739,#69740,#69741,#69742,#69743,#69744),.UNSPECIFIED.,.F.,.F.,(4,3,3,
3,3,3,3,3,3,3,3,3,3,3,3,3,3,3,3,3,3,3,3,3,3,3,3,3,3,4),(-0.562645757026855,
-0.555701473914062,-0.530900441032168,-0.515098938149575,-0.507065541704813,
-0.499621376006763,-0.473611873388524,-0.45123192600063,-0.444269138995806,
-0.438512576095804,-0.411585781389386,-0.384071987787232,-0.356846623787638,
-0.339848296888339,-0.335818611590039,-0.30730117792828,-0.29482500179958,
-0.2670444715065,-0.23926394121342,-0.231611467000139,-0.227138760951209,
-0.198500238527404,-0.169355291582403,-0.139789787243429,-0.122176108873976,
-0.117677873121744,-0.0872368492236495,-0.0566234034005496,-0.0264688552303108,
0.),.UNSPECIFIED.);
#1480=B_SPLINE_CURVE_WITH_KNOTS('',3,(#70134,#70135,#70136,#70137),
 .UNSPECIFIED.,.F.,.F.,(4,4),(-0.0490568531851087,0.),.UNSPECIFIED.);
#1481=B_SPLINE_CURVE_WITH_KNOTS('',3,(#70138,#70139,#70140,#70141,#70142,
#70143,#70144,#70145,#70146,#70147,#70148,#70149,#70150,#70151,#70152,#70153,
#70154,#70155,#70156,#70157,#70158,#70159,#70160,#70161,#70162,#70163,#70164,
#70165,#70166,#70167,#70168,#70169,#70170,#70171,#70172,#70173,#70174,#70175,
#70176,#70177,#70178,#70179,#70180,#70181,#70182,#70183,#70184,#70185,#70186,
#70187,#70188,#70189,#70190,#70191,#70192,#70193,#70194,#70195,#70196,#70197,
#70198,#70199,#70200,#70201,#70202,#70203,#70204,#70205,#70206,#70207,#70208,
#70209,#70210,#70211,#70212,#70213,#70214,#70215,#70216,#70217,#70218,#70219,
#70220,#70221,#70222,#70223,#70224,#70225),.UNSPECIFIED.,.F.,.F.,(4,3,3,
3,3,3,3,3,3,3,3,3,3,3,3,3,3,3,3,3,3,3,3,3,3,3,3,3,3,4),(-0.56264575702688,
-0.555701473914083,-0.531007418756454,-0.515098938720501,-0.507065529682846,
-0.499621375158853,-0.473611844527599,-0.451231901960729,-0.44426920356528,
-0.438512593706661,-0.411476852815532,-0.384052718111971,-0.356621494830653,
-0.339848281411137,-0.335818576668947,-0.307301144235682,-0.294825001799607,
-0.267044458395629,-0.23926391499165,-0.231611325020553,-0.227138740775428,
-0.198500204394852,-0.169355239834281,-0.139789729029255,-0.122176056932312,
-0.117677830115777,-0.0872367918330862,-0.0566233467844078,-0.0264688402299216,
-1.07255465021213E-14),.UNSPECIFIED.);
#1482=B_SPLINE_CURVE_WITH_KNOTS('',3,(#70230,#70231,#70232,#70233,#70234,
#70235,#70236,#70237,#70238,#70239,#70240,#70241,#70242,#70243,#70244,#70245,
#70246,#70247,#70248,#70249,#70250,#70251,#70252,#70253,#70254,#70255,#70256,
#70257,#70258,#70259,#70260,#70261,#70262,#70263,#70264,#70265,#70266,#70267,
#70268,#70269,#70270,#70271,#70272,#70273,#70274,#70275,#70276,#70277,#70278,
#70279,#70280,#70281,#70282,#70283,#70284,#70285,#70286,#70287,#70288,#70289,
#70290,#70291,#70292,#70293,#70294,#70295,#70296,#70297,#70298,#70299,#70300,
#70301,#70302,#70303,#70304,#70305,#70306,#70307,#70308,#70309,#70310,#70311,
#70312,#70313,#70314,#70315,#70316,#70317,#70318,#70319,#70320),
 .UNSPECIFIED.,.F.,.F.,(4,3,3,3,3,3,3,3,3,3,3,3,3,3,3,3,3,3,3,3,3,3,3,3,
3,3,3,3,3,3,4),(-0.554646384615711,-0.550740972514731,-0.520102356322042,
-0.489576564448263,-0.481306012005539,-0.451226840594297,-0.427170533611444,
-0.414805205120169,-0.409823976078728,-0.380725346809426,-0.351958339265775,
-0.32401601607743,-0.307648859480877,-0.302038780735922,-0.297878690081443,
-0.270514560405435,-0.258756835329743,-0.23030952069742,-0.201862206065096,
-0.196335035864416,-0.192150115673263,-0.165068640371989,-0.138040782233652,
-0.11155197104457,-0.103486161100401,-0.0966193329184451,-0.092630885380201,
-0.0669341287282739,-0.0416407713559216,-0.0171022276675499,0.),
 .UNSPECIFIED.);
#1483=B_SPLINE_CURVE_WITH_KNOTS('',3,(#70710,#70711,#70712,#70713),
 .UNSPECIFIED.,.F.,.F.,(4,4),(-0.0490579837509845,0.),.UNSPECIFIED.);
#1484=FACE_BOUND('',#2677,.T.);
#1485=FACE_BOUND('',#2681,.T.);
#1486=FACE_BOUND('',#2685,.T.);
#1487=FACE_BOUND('',#2689,.T.);
#1488=FACE_BOUND('',#2693,.T.);
#1489=FACE_BOUND('',#2697,.T.);
#1490=FACE_BOUND('',#2701,.T.);
#1491=FACE_BOUND('',#2702,.T.);
#1492=FACE_BOUND('',#2703,.T.);
#1493=FACE_BOUND('',#2704,.T.);
#1494=FACE_BOUND('',#2713,.T.);
#1495=FACE_BOUND('',#2715,.T.);
#1496=FACE_BOUND('',#2717,.T.);
#1497=FACE_BOUND('',#2719,.T.);
#1498=FACE_BOUND('',#2731,.T.);
#1499=FACE_BOUND('',#2732,.T.);
#1500=FACE_BOUND('',#2733,.T.);
#1501=FACE_BOUND('',#2734,.T.);
#1502=FACE_BOUND('',#2735,.T.);
#1503=FACE_BOUND('',#2736,.T.);
#1504=FACE_BOUND('',#2737,.T.);
#1505=FACE_BOUND('',#2738,.T.);
#1506=FACE_BOUND('',#2739,.T.);
#1507=FACE_BOUND('',#2740,.T.);
#1508=FACE_BOUND('',#2743,.T.);
#1509=FACE_BOUND('',#2744,.T.);
#1510=FACE_BOUND('',#2745,.T.);
#1511=FACE_BOUND('',#2751,.T.);
#1512=FACE_BOUND('',#2752,.T.);
#1513=FACE_BOUND('',#2753,.T.);
#1514=FACE_BOUND('',#2761,.T.);
#1515=FACE_BOUND('',#2762,.T.);
#1516=FACE_BOUND('',#2763,.T.);
#1517=FACE_BOUND('',#2764,.T.);
#1518=FACE_BOUND('',#2765,.T.);
#1519=FACE_BOUND('',#2766,.T.);
#1520=FACE_BOUND('',#2767,.T.);
#1521=FACE_BOUND('',#2768,.T.);
#1522=FACE_BOUND('',#2769,.T.);
#1523=FACE_BOUND('',#2770,.T.);
#1524=FACE_BOUND('',#2771,.T.);
#1525=FACE_BOUND('',#2772,.T.);
#1526=FACE_BOUND('',#2786,.T.);
#1527=FACE_BOUND('',#2788,.T.);
#1528=FACE_BOUND('',#2790,.T.);
#1529=FACE_BOUND('',#2793,.T.);
#1530=FACE_BOUND('',#2795,.T.);
#1531=FACE_BOUND('',#2798,.T.);
#1532=FACE_BOUND('',#2800,.T.);
#1533=FACE_BOUND('',#2803,.T.);
#1534=FACE_BOUND('',#2845,.T.);
#1535=FACE_BOUND('',#2846,.T.);
#1536=FACE_BOUND('',#2847,.T.);
#1537=FACE_BOUND('',#2848,.T.);
#1538=FACE_BOUND('',#2849,.T.);
#1539=FACE_BOUND('',#2850,.T.);
#1540=FACE_BOUND('',#2851,.T.);
#1541=FACE_BOUND('',#2852,.T.);
#1542=FACE_BOUND('',#2862,.T.);
#1543=FACE_BOUND('',#2863,.T.);
#1544=FACE_BOUND('',#2864,.T.);
#1545=FACE_BOUND('',#2869,.T.);
#1546=FACE_BOUND('',#2870,.T.);
#1547=FACE_BOUND('',#2876,.T.);
#1548=FACE_BOUND('',#2877,.T.);
#1549=FACE_BOUND('',#2923,.T.);
#1550=FACE_BOUND('',#2924,.T.);
#1551=FACE_BOUND('',#2925,.T.);
#1552=FACE_BOUND('',#2926,.T.);
#1553=FACE_BOUND('',#2927,.T.);
#1554=FACE_BOUND('',#2929,.T.);
#1555=FACE_BOUND('',#2930,.T.);
#1556=FACE_BOUND('',#2931,.T.);
#1557=FACE_BOUND('',#2932,.T.);
#1558=FACE_BOUND('',#2933,.T.);
#1559=FACE_BOUND('',#2963,.T.);
#1560=FACE_BOUND('',#3077,.T.);
#1561=FACE_BOUND('',#3126,.T.);
#1562=FACE_BOUND('',#3240,.T.);
#1563=FACE_BOUND('',#3276,.T.);
#1564=FACE_BOUND('',#3390,.T.);
#1565=PLANE('',#13761);
#1566=PLANE('',#13767);
#1567=PLANE('',#13773);
#1568=PLANE('',#13779);
#1569=PLANE('',#13785);
#1570=PLANE('',#13791);
#1571=PLANE('',#13797);
#1572=PLANE('',#13815);
#1573=PLANE('',#13817);
#1574=PLANE('',#13819);
#1575=PLANE('',#13821);
#1576=PLANE('',#13831);
#1577=PLANE('',#13832);
#1578=PLANE('',#13833);
#1579=PLANE('',#13836);
#1580=PLANE('',#13837);
#1581=PLANE('',#13838);
#1582=PLANE('',#13839);
#1583=PLANE('',#13840);
#1584=PLANE('',#13843);
#1585=PLANE('',#13844);
#1586=PLANE('',#13845);
#1587=PLANE('',#13846);
#1588=PLANE('',#13849);
#1589=PLANE('',#13850);
#1590=PLANE('',#13851);
#1591=PLANE('',#13852);
#1592=PLANE('',#13853);
#1593=PLANE('',#13858);
#1594=PLANE('',#13898);
#1595=PLANE('',#13901);
#1596=PLANE('',#13903);
#1597=PLANE('',#13907);
#1598=PLANE('',#13910);
#1599=PLANE('',#13914);
#1600=PLANE('',#13917);
#1601=PLANE('',#13921);
#1602=PLANE('',#13984);
#1603=PLANE('',#13985);
#1604=PLANE('',#13986);
#1605=PLANE('',#13987);
#1606=PLANE('',#13988);
#1607=PLANE('',#13989);
#1608=PLANE('',#13990);
#1609=PLANE('',#13991);
#1610=PLANE('',#13992);
#1611=PLANE('',#14003);
#1612=PLANE('',#14011);
#1613=PLANE('',#14016);
#1614=PLANE('',#14033);
#1615=PLANE('',#14034);
#1616=PLANE('',#14037);
#1617=PLANE('',#14038);
#1618=PLANE('',#14039);
#1619=PLANE('',#14040);
#1620=PLANE('',#14041);
#1621=PLANE('',#14042);
#1622=PLANE('',#14043);
#1623=PLANE('',#14044);
#1624=PLANE('',#14046);
#1625=PLANE('',#14047);
#1626=PLANE('',#14051);
#1627=PLANE('',#14055);
#1628=PLANE('',#14061);
#1629=PLANE('',#14062);
#1630=PLANE('',#14065);
#1631=PLANE('',#14066);
#1632=PLANE('',#14069);
#1633=PLANE('',#14070);
#1634=PLANE('',#14073);
#1635=PLANE('',#14074);
#1636=PLANE('',#14077);
#1637=PLANE('',#14078);
#1638=PLANE('',#14081);
#1639=PLANE('',#14082);
#1640=PLANE('',#14085);
#1641=PLANE('',#14086);
#1642=PLANE('',#14089);
#1643=PLANE('',#14090);
#1644=PLANE('',#14093);
#1645=PLANE('',#14094);
#1646=PLANE('',#14097);
#1647=PLANE('',#14098);
#1648=PLANE('',#14101);
#1649=PLANE('',#14102);
#1650=PLANE('',#14103);
#1651=PLANE('',#14110);
#1652=PLANE('',#14141);
#1653=PLANE('',#14143);
#1654=PLANE('',#14149);
#1655=PLANE('',#14153);
#1656=PLANE('',#14154);
#1657=PLANE('',#14155);
#1658=PLANE('',#14156);
#1659=PLANE('',#14196);
#1660=PLANE('',#14197);
#1661=PLANE('',#14198);
#1662=PLANE('',#14200);
#1663=PLANE('',#14201);
#1664=PLANE('',#14202);
#1665=PLANE('',#14204);
#1666=PLANE('',#14205);
#1667=PLANE('',#14206);
#1668=PLANE('',#14208);
#1669=PLANE('',#14209);
#1670=PLANE('',#14210);
#1671=PLANE('',#14212);
#1672=PLANE('',#14213);
#1673=PLANE('',#14214);
#1674=PLANE('',#14216);
#1675=PLANE('',#14217);
#1676=PLANE('',#14218);
#1677=PLANE('',#14220);
#1678=PLANE('',#14221);
#1679=PLANE('',#14222);
#1680=PLANE('',#14224);
#1681=PLANE('',#14225);
#1682=PLANE('',#14226);
#1683=PLANE('',#14228);
#1684=PLANE('',#14229);
#1685=PLANE('',#14230);
#1686=PLANE('',#14232);
#1687=PLANE('',#14233);
#1688=PLANE('',#14234);
#1689=PLANE('',#14236);
#1690=PLANE('',#14237);
#1691=PLANE('',#14238);
#1692=PLANE('',#14240);
#1693=PLANE('',#14241);
#1694=PLANE('',#14242);
#1695=PLANE('',#14244);
#1696=PLANE('',#14245);
#1697=PLANE('',#14246);
#1698=PLANE('',#14248);
#1699=PLANE('',#14249);
#1700=PLANE('',#14250);
#1701=PLANE('',#14252);
#1702=PLANE('',#14253);
#1703=PLANE('',#14254);
#1704=PLANE('',#14256);
#1705=PLANE('',#14257);
#1706=PLANE('',#14258);
#1707=PLANE('',#14260);
#1708=PLANE('',#14261);
#1709=PLANE('',#14262);
#1710=PLANE('',#14265);
#1711=PLANE('',#14266);
#1712=PLANE('',#14267);
#1713=PLANE('',#14269);
#1714=PLANE('',#14270);
#1715=PLANE('',#14271);
#1716=PLANE('',#14273);
#1717=PLANE('',#14274);
#1718=PLANE('',#14275);
#1719=PLANE('',#14277);
#1720=PLANE('',#14278);
#1721=PLANE('',#14279);
#1722=PLANE('',#14281);
#1723=PLANE('',#14282);
#1724=PLANE('',#14283);
#1725=PLANE('',#14285);
#1726=PLANE('',#14286);
#1727=PLANE('',#14287);
#1728=PLANE('',#14289);
#1729=PLANE('',#14290);
#1730=PLANE('',#14291);
#1731=PLANE('',#14293);
#1732=PLANE('',#14294);
#1733=PLANE('',#14295);
#1734=PLANE('',#14297);
#1735=PLANE('',#14298);
#1736=PLANE('',#14299);
#1737=PLANE('',#14301);
#1738=PLANE('',#14302);
#1739=PLANE('',#14303);
#1740=PLANE('',#14305);
#1741=PLANE('',#14306);
#1742=PLANE('',#14307);
#1743=PLANE('',#14309);
#1744=PLANE('',#14310);
#1745=PLANE('',#14311);
#1746=PLANE('',#14313);
#1747=PLANE('',#14314);
#1748=PLANE('',#14315);
#1749=PLANE('',#14317);
#1750=PLANE('',#14318);
#1751=PLANE('',#14319);
#1752=PLANE('',#14321);
#1753=PLANE('',#14322);
#1754=PLANE('',#14323);
#1755=PLANE('',#14325);
#1756=PLANE('',#14326);
#1757=PLANE('',#14327);
#1758=PLANE('',#14329);
#1759=PLANE('',#14330);
#1760=PLANE('',#14331);
#1761=PLANE('',#14333);
#1762=PLANE('',#14334);
#1763=PLANE('',#14335);
#1764=PLANE('',#14338);
#1765=PLANE('',#14339);
#1766=PLANE('',#14341);
#1767=PLANE('',#14343);
#1768=PLANE('',#14345);
#1769=PLANE('',#14347);
#1770=PLANE('',#14349);
#1771=PLANE('',#14352);
#1772=PLANE('',#14353);
#1773=PLANE('',#14354);
#1774=PLANE('',#14355);
#1775=PLANE('',#14356);
#1776=PLANE('',#14357);
#1777=PLANE('',#14393);
#1778=PLANE('',#14395);
#1779=PLANE('',#14401);
#1780=PLANE('',#14405);
#1781=PLANE('',#14406);
#1782=PLANE('',#14407);
#1783=PLANE('',#14408);
#1784=PLANE('',#14448);
#1785=PLANE('',#14450);
#1786=PLANE('',#14451);
#1787=PLANE('',#14488);
#1788=PLANE('',#14489);
#1789=PLANE('',#14490);
#1790=PLANE('',#14491);
#1791=PLANE('',#14492);
#1792=PLANE('',#14493);
#1793=PLANE('',#14494);
#1794=PLANE('',#14495);
#1795=PLANE('',#14496);
#1796=PLANE('',#14497);
#1797=PLANE('',#14498);
#1798=PLANE('',#14499);
#1799=PLANE('',#14500);
#1800=PLANE('',#14501);
#1801=PLANE('',#14502);
#1802=PLANE('',#14503);
#1803=PLANE('',#14504);
#1804=PLANE('',#14505);
#1805=PLANE('',#14506);
#1806=PLANE('',#14507);
#1807=PLANE('',#14508);
#1808=PLANE('',#14509);
#1809=PLANE('',#14510);
#1810=PLANE('',#14511);
#1811=PLANE('',#14512);
#1812=PLANE('',#14513);
#1813=PLANE('',#14514);
#1814=PLANE('',#14515);
#1815=PLANE('',#14516);
#1816=PLANE('',#14517);
#1817=PLANE('',#14518);
#1818=PLANE('',#14519);
#1819=PLANE('',#14520);
#1820=PLANE('',#14521);
#1821=PLANE('',#14522);
#1822=PLANE('',#14523);
#1823=PLANE('',#14524);
#1824=PLANE('',#14525);
#1825=PLANE('',#14526);
#1826=PLANE('',#14527);
#1827=PLANE('',#14528);
#1828=PLANE('',#14529);
#1829=PLANE('',#14530);
#1830=PLANE('',#14531);
#1831=PLANE('',#14532);
#1832=PLANE('',#14533);
#1833=PLANE('',#14534);
#1834=PLANE('',#14535);
#1835=PLANE('',#14536);
#1836=PLANE('',#14537);
#1837=PLANE('',#14538);
#1838=PLANE('',#14539);
#1839=PLANE('',#14540);
#1840=PLANE('',#14541);
#1841=PLANE('',#14542);
#1842=PLANE('',#14543);
#1843=PLANE('',#14544);
#1844=PLANE('',#14545);
#1845=PLANE('',#14546);
#1846=PLANE('',#14547);
#1847=PLANE('',#14548);
#1848=PLANE('',#14549);
#1849=PLANE('',#14550);
#1850=PLANE('',#14551);
#1851=PLANE('',#14552);
#1852=PLANE('',#14553);
#1853=PLANE('',#14554);
#1854=PLANE('',#14555);
#1855=PLANE('',#14556);
#1856=PLANE('',#14557);
#1857=PLANE('',#14558);
#1858=PLANE('',#14559);
#1859=PLANE('',#14560);
#1860=PLANE('',#14561);
#1861=PLANE('',#14562);
#1862=PLANE('',#14563);
#1863=PLANE('',#14564);
#1864=PLANE('',#14565);
#1865=PLANE('',#14566);
#1866=PLANE('',#14567);
#1867=PLANE('',#14568);
#1868=PLANE('',#14569);
#1869=PLANE('',#14570);
#1870=PLANE('',#14571);
#1871=PLANE('',#14572);
#1872=PLANE('',#14573);
#1873=PLANE('',#14574);
#1874=PLANE('',#14575);
#1875=PLANE('',#14576);
#1876=PLANE('',#14577);
#1877=PLANE('',#14578);
#1878=PLANE('',#14579);
#1879=PLANE('',#14580);
#1880=PLANE('',#14581);
#1881=PLANE('',#14582);
#1882=PLANE('',#14583);
#1883=PLANE('',#14584);
#1884=PLANE('',#14585);
#1885=PLANE('',#14586);
#1886=PLANE('',#14587);
#1887=PLANE('',#14588);
#1888=PLANE('',#14589);
#1889=PLANE('',#14590);
#1890=PLANE('',#14591);
#1891=PLANE('',#14593);
#1892=PLANE('',#14595);
#1893=PLANE('',#14597);
#1894=PLANE('',#14599);
#1895=PLANE('',#14601);
#1896=PLANE('',#14604);
#1897=PLANE('',#14605);
#1898=PLANE('',#14606);
#1899=PLANE('',#14607);
#1900=PLANE('',#14608);
#1901=PLANE('',#14609);
#1902=PLANE('',#14631);
#1903=PLANE('',#14634);
#1904=PLANE('',#14640);
#1905=PLANE('',#14644);
#1906=PLANE('',#14645);
#1907=PLANE('',#14646);
#1908=PLANE('',#14647);
#1909=PLANE('',#14687);
#1910=PLANE('',#14688);
#1911=PLANE('',#14689);
#1912=PLANE('',#14691);
#1913=PLANE('',#14692);
#1914=PLANE('',#14693);
#1915=PLANE('',#14695);
#1916=PLANE('',#14696);
#1917=PLANE('',#14697);
#1918=PLANE('',#14699);
#1919=PLANE('',#14700);
#1920=PLANE('',#14701);
#1921=PLANE('',#14703);
#1922=PLANE('',#14704);
#1923=PLANE('',#14705);
#1924=PLANE('',#14707);
#1925=PLANE('',#14708);
#1926=PLANE('',#14709);
#1927=PLANE('',#14711);
#1928=PLANE('',#14712);
#1929=PLANE('',#14713);
#1930=PLANE('',#14715);
#1931=PLANE('',#14716);
#1932=PLANE('',#14717);
#1933=PLANE('',#14719);
#1934=PLANE('',#14720);
#1935=PLANE('',#14721);
#1936=PLANE('',#14723);
#1937=PLANE('',#14724);
#1938=PLANE('',#14725);
#1939=PLANE('',#14727);
#1940=PLANE('',#14728);
#1941=PLANE('',#14729);
#1942=PLANE('',#14731);
#1943=PLANE('',#14732);
#1944=PLANE('',#14733);
#1945=PLANE('',#14735);
#1946=PLANE('',#14736);
#1947=PLANE('',#14737);
#1948=PLANE('',#14739);
#1949=PLANE('',#14740);
#1950=PLANE('',#14741);
#1951=PLANE('',#14743);
#1952=PLANE('',#14744);
#1953=PLANE('',#14745);
#1954=PLANE('',#14747);
#1955=PLANE('',#14748);
#1956=PLANE('',#14749);
#1957=PLANE('',#14751);
#1958=PLANE('',#14752);
#1959=PLANE('',#14753);
#1960=PLANE('',#14756);
#1961=PLANE('',#14757);
#1962=PLANE('',#14758);
#1963=PLANE('',#14760);
#1964=PLANE('',#14761);
#1965=PLANE('',#14762);
#1966=PLANE('',#14764);
#1967=PLANE('',#14765);
#1968=PLANE('',#14766);
#1969=PLANE('',#14768);
#1970=PLANE('',#14769);
#1971=PLANE('',#14770);
#1972=PLANE('',#14772);
#1973=PLANE('',#14773);
#1974=PLANE('',#14774);
#1975=PLANE('',#14776);
#1976=PLANE('',#14777);
#1977=PLANE('',#14778);
#1978=PLANE('',#14780);
#1979=PLANE('',#14781);
#1980=PLANE('',#14782);
#1981=PLANE('',#14784);
#1982=PLANE('',#14785);
#1983=PLANE('',#14786);
#1984=PLANE('',#14788);
#1985=PLANE('',#14789);
#1986=PLANE('',#14790);
#1987=PLANE('',#14792);
#1988=PLANE('',#14793);
#1989=PLANE('',#14794);
#1990=PLANE('',#14796);
#1991=PLANE('',#14797);
#1992=PLANE('',#14798);
#1993=PLANE('',#14800);
#1994=PLANE('',#14801);
#1995=PLANE('',#14802);
#1996=PLANE('',#14804);
#1997=PLANE('',#14805);
#1998=PLANE('',#14806);
#1999=PLANE('',#14808);
#2000=PLANE('',#14809);
#2001=PLANE('',#14810);
#2002=PLANE('',#14812);
#2003=PLANE('',#14813);
#2004=PLANE('',#14814);
#2005=PLANE('',#14816);
#2006=PLANE('',#14817);
#2007=PLANE('',#14818);
#2008=PLANE('',#14820);
#2009=PLANE('',#14821);
#2010=PLANE('',#14822);
#2011=PLANE('',#14824);
#2012=PLANE('',#14825);
#2013=PLANE('',#14826);
#2014=PLANE('',#14829);
#2015=PLANE('',#14830);
#2016=PLANE('',#14832);
#2017=PLANE('',#14834);
#2018=PLANE('',#14836);
#2019=PLANE('',#14838);
#2020=PLANE('',#14840);
#2021=PLANE('',#14843);
#2022=PLANE('',#14844);
#2023=PLANE('',#14845);
#2024=PLANE('',#14846);
#2025=PLANE('',#14847);
#2026=PLANE('',#14848);
#2027=FACE_OUTER_BOUND('',#2675,.T.);
#2028=FACE_OUTER_BOUND('',#2676,.T.);
#2029=FACE_OUTER_BOUND('',#2678,.T.);
#2030=FACE_OUTER_BOUND('',#2679,.T.);
#2031=FACE_OUTER_BOUND('',#2680,.T.);
#2032=FACE_OUTER_BOUND('',#2682,.T.);
#2033=FACE_OUTER_BOUND('',#2683,.T.);
#2034=FACE_OUTER_BOUND('',#2684,.T.);
#2035=FACE_OUTER_BOUND('',#2686,.T.);
#2036=FACE_OUTER_BOUND('',#2687,.T.);
#2037=FACE_OUTER_BOUND('',#2688,.T.);
#2038=FACE_OUTER_BOUND('',#2690,.T.);
#2039=FACE_OUTER_BOUND('',#2691,.T.);
#2040=FACE_OUTER_BOUND('',#2692,.T.);
#2041=FACE_OUTER_BOUND('',#2694,.T.);
#2042=FACE_OUTER_BOUND('',#2695,.T.);
#2043=FACE_OUTER_BOUND('',#2696,.T.);
#2044=FACE_OUTER_BOUND('',#2698,.T.);
#2045=FACE_OUTER_BOUND('',#2699,.T.);
#2046=FACE_OUTER_BOUND('',#2700,.T.);
#2047=FACE_OUTER_BOUND('',#2705,.T.);
#2048=FACE_OUTER_BOUND('',#2706,.T.);
#2049=FACE_OUTER_BOUND('',#2707,.T.);
#2050=FACE_OUTER_BOUND('',#2708,.T.);
#2051=FACE_OUTER_BOUND('',#2709,.T.);
#2052=FACE_OUTER_BOUND('',#2710,.T.);
#2053=FACE_OUTER_BOUND('',#2711,.T.);
#2054=FACE_OUTER_BOUND('',#2712,.T.);
#2055=FACE_OUTER_BOUND('',#2714,.T.);
#2056=FACE_OUTER_BOUND('',#2716,.T.);
#2057=FACE_OUTER_BOUND('',#2718,.T.);
#2058=FACE_OUTER_BOUND('',#2720,.T.);
#2059=FACE_OUTER_BOUND('',#2721,.T.);
#2060=FACE_OUTER_BOUND('',#2722,.T.);
#2061=FACE_OUTER_BOUND('',#2723,.T.);
#2062=FACE_OUTER_BOUND('',#2724,.T.);
#2063=FACE_OUTER_BOUND('',#2725,.T.);
#2064=FACE_OUTER_BOUND('',#2726,.T.);
#2065=FACE_OUTER_BOUND('',#2727,.T.);
#2066=FACE_OUTER_BOUND('',#2728,.T.);
#2067=FACE_OUTER_BOUND('',#2729,.T.);
#2068=FACE_OUTER_BOUND('',#2730,.T.);
#2069=FACE_OUTER_BOUND('',#2741,.T.);
#2070=FACE_OUTER_BOUND('',#2742,.T.);
#2071=FACE_OUTER_BOUND('',#2746,.T.);
#2072=FACE_OUTER_BOUND('',#2747,.T.);
#2073=FACE_OUTER_BOUND('',#2748,.T.);
#2074=FACE_OUTER_BOUND('',#2749,.T.);
#2075=FACE_OUTER_BOUND('',#2750,.T.);
#2076=FACE_OUTER_BOUND('',#2754,.T.);
#2077=FACE_OUTER_BOUND('',#2755,.T.);
#2078=FACE_OUTER_BOUND('',#2756,.T.);
#2079=FACE_OUTER_BOUND('',#2757,.T.);
#2080=FACE_OUTER_BOUND('',#2758,.T.);
#2081=FACE_OUTER_BOUND('',#2759,.T.);
#2082=FACE_OUTER_BOUND('',#2760,.T.);
#2083=FACE_OUTER_BOUND('',#2773,.T.);
#2084=FACE_OUTER_BOUND('',#2774,.T.);
#2085=FACE_OUTER_BOUND('',#2775,.T.);
#2086=FACE_OUTER_BOUND('',#2776,.T.);
#2087=FACE_OUTER_BOUND('',#2777,.T.);
#2088=FACE_OUTER_BOUND('',#2778,.T.);
#2089=FACE_OUTER_BOUND('',#2779,.T.);
#2090=FACE_OUTER_BOUND('',#2780,.T.);
#2091=FACE_OUTER_BOUND('',#2781,.T.);
#2092=FACE_OUTER_BOUND('',#2782,.T.);
#2093=FACE_OUTER_BOUND('',#2783,.T.);
#2094=FACE_OUTER_BOUND('',#2784,.T.);
#2095=FACE_OUTER_BOUND('',#2785,.T.);
#2096=FACE_OUTER_BOUND('',#2787,.T.);
#2097=FACE_OUTER_BOUND('',#2789,.T.);
#2098=FACE_OUTER_BOUND('',#2791,.T.);
#2099=FACE_OUTER_BOUND('',#2792,.T.);
#2100=FACE_OUTER_BOUND('',#2794,.T.);
#2101=FACE_OUTER_BOUND('',#2796,.T.);
#2102=FACE_OUTER_BOUND('',#2797,.T.);
#2103=FACE_OUTER_BOUND('',#2799,.T.);
#2104=FACE_OUTER_BOUND('',#2801,.T.);
#2105=FACE_OUTER_BOUND('',#2802,.T.);
#2106=FACE_OUTER_BOUND('',#2804,.T.);
#2107=FACE_OUTER_BOUND('',#2805,.T.);
#2108=FACE_OUTER_BOUND('',#2806,.T.);
#2109=FACE_OUTER_BOUND('',#2807,.T.);
#2110=FACE_OUTER_BOUND('',#2808,.T.);
#2111=FACE_OUTER_BOUND('',#2809,.T.);
#2112=FACE_OUTER_BOUND('',#2810,.T.);
#2113=FACE_OUTER_BOUND('',#2811,.T.);
#2114=FACE_OUTER_BOUND('',#2812,.T.);
#2115=FACE_OUTER_BOUND('',#2813,.T.);
#2116=FACE_OUTER_BOUND('',#2814,.T.);
#2117=FACE_OUTER_BOUND('',#2815,.T.);
#2118=FACE_OUTER_BOUND('',#2816,.T.);
#2119=FACE_OUTER_BOUND('',#2817,.T.);
#2120=FACE_OUTER_BOUND('',#2818,.T.);
#2121=FACE_OUTER_BOUND('',#2819,.T.);
#2122=FACE_OUTER_BOUND('',#2820,.T.);
#2123=FACE_OUTER_BOUND('',#2821,.T.);
#2124=FACE_OUTER_BOUND('',#2822,.T.);
#2125=FACE_OUTER_BOUND('',#2823,.T.);
#2126=FACE_OUTER_BOUND('',#2824,.T.);
#2127=FACE_OUTER_BOUND('',#2825,.T.);
#2128=FACE_OUTER_BOUND('',#2826,.T.);
#2129=FACE_OUTER_BOUND('',#2827,.T.);
#2130=FACE_OUTER_BOUND('',#2828,.T.);
#2131=FACE_OUTER_BOUND('',#2829,.T.);
#2132=FACE_OUTER_BOUND('',#2830,.T.);
#2133=FACE_OUTER_BOUND('',#2831,.T.);
#2134=FACE_OUTER_BOUND('',#2832,.T.);
#2135=FACE_OUTER_BOUND('',#2833,.T.);
#2136=FACE_OUTER_BOUND('',#2834,.T.);
#2137=FACE_OUTER_BOUND('',#2835,.T.);
#2138=FACE_OUTER_BOUND('',#2836,.T.);
#2139=FACE_OUTER_BOUND('',#2837,.T.);
#2140=FACE_OUTER_BOUND('',#2838,.T.);
#2141=FACE_OUTER_BOUND('',#2839,.T.);
#2142=FACE_OUTER_BOUND('',#2840,.T.);
#2143=FACE_OUTER_BOUND('',#2841,.T.);
#2144=FACE_OUTER_BOUND('',#2842,.T.);
#2145=FACE_OUTER_BOUND('',#2843,.T.);
#2146=FACE_OUTER_BOUND('',#2844,.T.);
#2147=FACE_OUTER_BOUND('',#2853,.T.);
#2148=FACE_OUTER_BOUND('',#2854,.T.);
#2149=FACE_OUTER_BOUND('',#2855,.T.);
#2150=FACE_OUTER_BOUND('',#2856,.T.);
#2151=FACE_OUTER_BOUND('',#2857,.T.);
#2152=FACE_OUTER_BOUND('',#2858,.T.);
#2153=FACE_OUTER_BOUND('',#2859,.T.);
#2154=FACE_OUTER_BOUND('',#2860,.T.);
#2155=FACE_OUTER_BOUND('',#2861,.T.);
#2156=FACE_OUTER_BOUND('',#2865,.T.);
#2157=FACE_OUTER_BOUND('',#2866,.T.);
#2158=FACE_OUTER_BOUND('',#2867,.T.);
#2159=FACE_OUTER_BOUND('',#2868,.T.);
#2160=FACE_OUTER_BOUND('',#2871,.T.);
#2161=FACE_OUTER_BOUND('',#2872,.T.);
#2162=FACE_OUTER_BOUND('',#2873,.T.);
#2163=FACE_OUTER_BOUND('',#2874,.T.);
#2164=FACE_OUTER_BOUND('',#2875,.T.);
#2165=FACE_OUTER_BOUND('',#2878,.T.);
#2166=FACE_OUTER_BOUND('',#2879,.T.);
#2167=FACE_OUTER_BOUND('',#2880,.T.);
#2168=FACE_OUTER_BOUND('',#2881,.T.);
#2169=FACE_OUTER_BOUND('',#2882,.T.);
#2170=FACE_OUTER_BOUND('',#2883,.T.);
#2171=FACE_OUTER_BOUND('',#2884,.T.);
#2172=FACE_OUTER_BOUND('',#2885,.T.);
#2173=FACE_OUTER_BOUND('',#2886,.T.);
#2174=FACE_OUTER_BOUND('',#2887,.T.);
#2175=FACE_OUTER_BOUND('',#2888,.T.);
#2176=FACE_OUTER_BOUND('',#2889,.T.);
#2177=FACE_OUTER_BOUND('',#2890,.T.);
#2178=FACE_OUTER_BOUND('',#2891,.T.);
#2179=FACE_OUTER_BOUND('',#2892,.T.);
#2180=FACE_OUTER_BOUND('',#2893,.T.);
#2181=FACE_OUTER_BOUND('',#2894,.T.);
#2182=FACE_OUTER_BOUND('',#2895,.T.);
#2183=FACE_OUTER_BOUND('',#2896,.T.);
#2184=FACE_OUTER_BOUND('',#2897,.T.);
#2185=FACE_OUTER_BOUND('',#2898,.T.);
#2186=FACE_OUTER_BOUND('',#2899,.T.);
#2187=FACE_OUTER_BOUND('',#2900,.T.);
#2188=FACE_OUTER_BOUND('',#2901,.T.);
#2189=FACE_OUTER_BOUND('',#2902,.T.);
#2190=FACE_OUTER_BOUND('',#2903,.T.);
#2191=FACE_OUTER_BOUND('',#2904,.T.);
#2192=FACE_OUTER_BOUND('',#2905,.T.);
#2193=FACE_OUTER_BOUND('',#2906,.T.);
#2194=FACE_OUTER_BOUND('',#2907,.T.);
#2195=FACE_OUTER_BOUND('',#2908,.T.);
#2196=FACE_OUTER_BOUND('',#2909,.T.);
#2197=FACE_OUTER_BOUND('',#2910,.T.);
#2198=FACE_OUTER_BOUND('',#2911,.T.);
#2199=FACE_OUTER_BOUND('',#2912,.T.);
#2200=FACE_OUTER_BOUND('',#2913,.T.);
#2201=FACE_OUTER_BOUND('',#2914,.T.);
#2202=FACE_OUTER_BOUND('',#2915,.T.);
#2203=FACE_OUTER_BOUND('',#2916,.T.);
#2204=FACE_OUTER_BOUND('',#2917,.T.);
#2205=FACE_OUTER_BOUND('',#2918,.T.);
#2206=FACE_OUTER_BOUND('',#2919,.T.);
#2207=FACE_OUTER_BOUND('',#2920,.T.);
#2208=FACE_OUTER_BOUND('',#2921,.T.);
#2209=FACE_OUTER_BOUND('',#2922,.T.);
#2210=FACE_OUTER_BOUND('',#2928,.T.);
#2211=FACE_OUTER_BOUND('',#2934,.T.);
#2212=FACE_OUTER_BOUND('',#2935,.T.);
#2213=FACE_OUTER_BOUND('',#2936,.T.);
#2214=FACE_OUTER_BOUND('',#2937,.T.);
#2215=FACE_OUTER_BOUND('',#2938,.T.);
#2216=FACE_OUTER_BOUND('',#2939,.T.);
#2217=FACE_OUTER_BOUND('',#2940,.T.);
#2218=FACE_OUTER_BOUND('',#2941,.T.);
#2219=FACE_OUTER_BOUND('',#2942,.T.);
#2220=FACE_OUTER_BOUND('',#2943,.T.);
#2221=FACE_OUTER_BOUND('',#2944,.T.);
#2222=FACE_OUTER_BOUND('',#2945,.T.);
#2223=FACE_OUTER_BOUND('',#2946,.T.);
#2224=FACE_OUTER_BOUND('',#2947,.T.);
#2225=FACE_OUTER_BOUND('',#2948,.T.);
#2226=FACE_OUTER_BOUND('',#2949,.T.);
#2227=FACE_OUTER_BOUND('',#2950,.T.);
#2228=FACE_OUTER_BOUND('',#2951,.T.);
#2229=FACE_OUTER_BOUND('',#2952,.T.);
#2230=FACE_OUTER_BOUND('',#2953,.T.);
#2231=FACE_OUTER_BOUND('',#2954,.T.);
#2232=FACE_OUTER_BOUND('',#2955,.T.);
#2233=FACE_OUTER_BOUND('',#2956,.T.);
#2234=FACE_OUTER_BOUND('',#2957,.T.);
#2235=FACE_OUTER_BOUND('',#2958,.T.);
#2236=FACE_OUTER_BOUND('',#2959,.T.);
#2237=FACE_OUTER_BOUND('',#2960,.T.);
#2238=FACE_OUTER_BOUND('',#2961,.T.);
#2239=FACE_OUTER_BOUND('',#2962,.T.);
#2240=FACE_OUTER_BOUND('',#2964,.T.);
#2241=FACE_OUTER_BOUND('',#2965,.T.);
#2242=FACE_OUTER_BOUND('',#2966,.T.);
#2243=FACE_OUTER_BOUND('',#2967,.T.);
#2244=FACE_OUTER_BOUND('',#2968,.T.);
#2245=FACE_OUTER_BOUND('',#2969,.T.);
#2246=FACE_OUTER_BOUND('',#2970,.T.);
#2247=FACE_OUTER_BOUND('',#2971,.T.);
#2248=FACE_OUTER_BOUND('',#2972,.T.);
#2249=FACE_OUTER_BOUND('',#2973,.T.);
#2250=FACE_OUTER_BOUND('',#2974,.T.);
#2251=FACE_OUTER_BOUND('',#2975,.T.);
#2252=FACE_OUTER_BOUND('',#2976,.T.);
#2253=FACE_OUTER_BOUND('',#2977,.T.);
#2254=FACE_OUTER_BOUND('',#2978,.T.);
#2255=FACE_OUTER_BOUND('',#2979,.T.);
#2256=FACE_OUTER_BOUND('',#2980,.T.);
#2257=FACE_OUTER_BOUND('',#2981,.T.);
#2258=FACE_OUTER_BOUND('',#2982,.T.);
#2259=FACE_OUTER_BOUND('',#2983,.T.);
#2260=FACE_OUTER_BOUND('',#2984,.T.);
#2261=FACE_OUTER_BOUND('',#2985,.T.);
#2262=FACE_OUTER_BOUND('',#2986,.T.);
#2263=FACE_OUTER_BOUND('',#2987,.T.);
#2264=FACE_OUTER_BOUND('',#2988,.T.);
#2265=FACE_OUTER_BOUND('',#2989,.T.);
#2266=FACE_OUTER_BOUND('',#2990,.T.);
#2267=FACE_OUTER_BOUND('',#2991,.T.);
#2268=FACE_OUTER_BOUND('',#2992,.T.);
#2269=FACE_OUTER_BOUND('',#2993,.T.);
#2270=FACE_OUTER_BOUND('',#2994,.T.);
#2271=FACE_OUTER_BOUND('',#2995,.T.);
#2272=FACE_OUTER_BOUND('',#2996,.T.);
#2273=FACE_OUTER_BOUND('',#2997,.T.);
#2274=FACE_OUTER_BOUND('',#2998,.T.);
#2275=FACE_OUTER_BOUND('',#2999,.T.);
#2276=FACE_OUTER_BOUND('',#3000,.T.);
#2277=FACE_OUTER_BOUND('',#3001,.T.);
#2278=FACE_OUTER_BOUND('',#3002,.T.);
#2279=FACE_OUTER_BOUND('',#3003,.T.);
#2280=FACE_OUTER_BOUND('',#3004,.T.);
#2281=FACE_OUTER_BOUND('',#3005,.T.);
#2282=FACE_OUTER_BOUND('',#3006,.T.);
#2283=FACE_OUTER_BOUND('',#3007,.T.);
#2284=FACE_OUTER_BOUND('',#3008,.T.);
#2285=FACE_OUTER_BOUND('',#3009,.T.);
#2286=FACE_OUTER_BOUND('',#3010,.T.);
#2287=FACE_OUTER_BOUND('',#3011,.T.);
#2288=FACE_OUTER_BOUND('',#3012,.T.);
#2289=FACE_OUTER_BOUND('',#3013,.T.);
#2290=FACE_OUTER_BOUND('',#3014,.T.);
#2291=FACE_OUTER_BOUND('',#3015,.T.);
#2292=FACE_OUTER_BOUND('',#3016,.T.);
#2293=FACE_OUTER_BOUND('',#3017,.T.);
#2294=FACE_OUTER_BOUND('',#3018,.T.);
#2295=FACE_OUTER_BOUND('',#3019,.T.);
#2296=FACE_OUTER_BOUND('',#3020,.T.);
#2297=FACE_OUTER_BOUND('',#3021,.T.);
#2298=FACE_OUTER_BOUND('',#3022,.T.);
#2299=FACE_OUTER_BOUND('',#3023,.T.);
#2300=FACE_OUTER_BOUND('',#3024,.T.);
#2301=FACE_OUTER_BOUND('',#3025,.T.);
#2302=FACE_OUTER_BOUND('',#3026,.T.);
#2303=FACE_OUTER_BOUND('',#3027,.T.);
#2304=FACE_OUTER_BOUND('',#3028,.T.);
#2305=FACE_OUTER_BOUND('',#3029,.T.);
#2306=FACE_OUTER_BOUND('',#3030,.T.);
#2307=FACE_OUTER_BOUND('',#3031,.T.);
#2308=FACE_OUTER_BOUND('',#3032,.T.);
#2309=FACE_OUTER_BOUND('',#3033,.T.);
#2310=FACE_OUTER_BOUND('',#3034,.T.);
#2311=FACE_OUTER_BOUND('',#3035,.T.);
#2312=FACE_OUTER_BOUND('',#3036,.T.);
#2313=FACE_OUTER_BOUND('',#3037,.T.);
#2314=FACE_OUTER_BOUND('',#3038,.T.);
#2315=FACE_OUTER_BOUND('',#3039,.T.);
#2316=FACE_OUTER_BOUND('',#3040,.T.);
#2317=FACE_OUTER_BOUND('',#3041,.T.);
#2318=FACE_OUTER_BOUND('',#3042,.T.);
#2319=FACE_OUTER_BOUND('',#3043,.T.);
#2320=FACE_OUTER_BOUND('',#3044,.T.);
#2321=FACE_OUTER_BOUND('',#3045,.T.);
#2322=FACE_OUTER_BOUND('',#3046,.T.);
#2323=FACE_OUTER_BOUND('',#3047,.T.);
#2324=FACE_OUTER_BOUND('',#3048,.T.);
#2325=FACE_OUTER_BOUND('',#3049,.T.);
#2326=FACE_OUTER_BOUND('',#3050,.T.);
#2327=FACE_OUTER_BOUND('',#3051,.T.);
#2328=FACE_OUTER_BOUND('',#3052,.T.);
#2329=FACE_OUTER_BOUND('',#3053,.T.);
#2330=FACE_OUTER_BOUND('',#3054,.T.);
#2331=FACE_OUTER_BOUND('',#3055,.T.);
#2332=FACE_OUTER_BOUND('',#3056,.T.);
#2333=FACE_OUTER_BOUND('',#3057,.T.);
#2334=FACE_OUTER_BOUND('',#3058,.T.);
#2335=FACE_OUTER_BOUND('',#3059,.T.);
#2336=FACE_OUTER_BOUND('',#3060,.T.);
#2337=FACE_OUTER_BOUND('',#3061,.T.);
#2338=FACE_OUTER_BOUND('',#3062,.T.);
#2339=FACE_OUTER_BOUND('',#3063,.T.);
#2340=FACE_OUTER_BOUND('',#3064,.T.);
#2341=FACE_OUTER_BOUND('',#3065,.T.);
#2342=FACE_OUTER_BOUND('',#3066,.T.);
#2343=FACE_OUTER_BOUND('',#3067,.T.);
#2344=FACE_OUTER_BOUND('',#3068,.T.);
#2345=FACE_OUTER_BOUND('',#3069,.T.);
#2346=FACE_OUTER_BOUND('',#3070,.T.);
#2347=FACE_OUTER_BOUND('',#3071,.T.);
#2348=FACE_OUTER_BOUND('',#3072,.T.);
#2349=FACE_OUTER_BOUND('',#3073,.T.);
#2350=FACE_OUTER_BOUND('',#3074,.T.);
#2351=FACE_OUTER_BOUND('',#3075,.T.);
#2352=FACE_OUTER_BOUND('',#3076,.T.);
#2353=FACE_OUTER_BOUND('',#3078,.T.);
#2354=FACE_OUTER_BOUND('',#3079,.T.);
#2355=FACE_OUTER_BOUND('',#3080,.T.);
#2356=FACE_OUTER_BOUND('',#3081,.T.);
#2357=FACE_OUTER_BOUND('',#3082,.T.);
#2358=FACE_OUTER_BOUND('',#3083,.T.);
#2359=FACE_OUTER_BOUND('',#3084,.T.);
#2360=FACE_OUTER_BOUND('',#3085,.T.);
#2361=FACE_OUTER_BOUND('',#3086,.T.);
#2362=FACE_OUTER_BOUND('',#3087,.T.);
#2363=FACE_OUTER_BOUND('',#3088,.T.);
#2364=FACE_OUTER_BOUND('',#3089,.T.);
#2365=FACE_OUTER_BOUND('',#3090,.T.);
#2366=FACE_OUTER_BOUND('',#3091,.T.);
#2367=FACE_OUTER_BOUND('',#3092,.T.);
#2368=FACE_OUTER_BOUND('',#3093,.T.);
#2369=FACE_OUTER_BOUND('',#3094,.T.);
#2370=FACE_OUTER_BOUND('',#3095,.T.);
#2371=FACE_OUTER_BOUND('',#3096,.T.);
#2372=FACE_OUTER_BOUND('',#3097,.T.);
#2373=FACE_OUTER_BOUND('',#3098,.T.);
#2374=FACE_OUTER_BOUND('',#3099,.T.);
#2375=FACE_OUTER_BOUND('',#3100,.T.);
#2376=FACE_OUTER_BOUND('',#3101,.T.);
#2377=FACE_OUTER_BOUND('',#3102,.T.);
#2378=FACE_OUTER_BOUND('',#3103,.T.);
#2379=FACE_OUTER_BOUND('',#3104,.T.);
#2380=FACE_OUTER_BOUND('',#3105,.T.);
#2381=FACE_OUTER_BOUND('',#3106,.T.);
#2382=FACE_OUTER_BOUND('',#3107,.T.);
#2383=FACE_OUTER_BOUND('',#3108,.T.);
#2384=FACE_OUTER_BOUND('',#3109,.T.);
#2385=FACE_OUTER_BOUND('',#3110,.T.);
#2386=FACE_OUTER_BOUND('',#3111,.T.);
#2387=FACE_OUTER_BOUND('',#3112,.T.);
#2388=FACE_OUTER_BOUND('',#3113,.T.);
#2389=FACE_OUTER_BOUND('',#3114,.T.);
#2390=FACE_OUTER_BOUND('',#3115,.T.);
#2391=FACE_OUTER_BOUND('',#3116,.T.);
#2392=FACE_OUTER_BOUND('',#3117,.T.);
#2393=FACE_OUTER_BOUND('',#3118,.T.);
#2394=FACE_OUTER_BOUND('',#3119,.T.);
#2395=FACE_OUTER_BOUND('',#3120,.T.);
#2396=FACE_OUTER_BOUND('',#3121,.T.);
#2397=FACE_OUTER_BOUND('',#3122,.T.);
#2398=FACE_OUTER_BOUND('',#3123,.T.);
#2399=FACE_OUTER_BOUND('',#3124,.T.);
#2400=FACE_OUTER_BOUND('',#3125,.T.);
#2401=FACE_OUTER_BOUND('',#3127,.T.);
#2402=FACE_OUTER_BOUND('',#3128,.T.);
#2403=FACE_OUTER_BOUND('',#3129,.T.);
#2404=FACE_OUTER_BOUND('',#3130,.T.);
#2405=FACE_OUTER_BOUND('',#3131,.T.);
#2406=FACE_OUTER_BOUND('',#3132,.T.);
#2407=FACE_OUTER_BOUND('',#3133,.T.);
#2408=FACE_OUTER_BOUND('',#3134,.T.);
#2409=FACE_OUTER_BOUND('',#3135,.T.);
#2410=FACE_OUTER_BOUND('',#3136,.T.);
#2411=FACE_OUTER_BOUND('',#3137,.T.);
#2412=FACE_OUTER_BOUND('',#3138,.T.);
#2413=FACE_OUTER_BOUND('',#3139,.T.);
#2414=FACE_OUTER_BOUND('',#3140,.T.);
#2415=FACE_OUTER_BOUND('',#3141,.T.);
#2416=FACE_OUTER_BOUND('',#3142,.T.);
#2417=FACE_OUTER_BOUND('',#3143,.T.);
#2418=FACE_OUTER_BOUND('',#3144,.T.);
#2419=FACE_OUTER_BOUND('',#3145,.T.);
#2420=FACE_OUTER_BOUND('',#3146,.T.);
#2421=FACE_OUTER_BOUND('',#3147,.T.);
#2422=FACE_OUTER_BOUND('',#3148,.T.);
#2423=FACE_OUTER_BOUND('',#3149,.T.);
#2424=FACE_OUTER_BOUND('',#3150,.T.);
#2425=FACE_OUTER_BOUND('',#3151,.T.);
#2426=FACE_OUTER_BOUND('',#3152,.T.);
#2427=FACE_OUTER_BOUND('',#3153,.T.);
#2428=FACE_OUTER_BOUND('',#3154,.T.);
#2429=FACE_OUTER_BOUND('',#3155,.T.);
#2430=FACE_OUTER_BOUND('',#3156,.T.);
#2431=FACE_OUTER_BOUND('',#3157,.T.);
#2432=FACE_OUTER_BOUND('',#3158,.T.);
#2433=FACE_OUTER_BOUND('',#3159,.T.);
#2434=FACE_OUTER_BOUND('',#3160,.T.);
#2435=FACE_OUTER_BOUND('',#3161,.T.);
#2436=FACE_OUTER_BOUND('',#3162,.T.);
#2437=FACE_OUTER_BOUND('',#3163,.T.);
#2438=FACE_OUTER_BOUND('',#3164,.T.);
#2439=FACE_OUTER_BOUND('',#3165,.T.);
#2440=FACE_OUTER_BOUND('',#3166,.T.);
#2441=FACE_OUTER_BOUND('',#3167,.T.);
#2442=FACE_OUTER_BOUND('',#3168,.T.);
#2443=FACE_OUTER_BOUND('',#3169,.T.);
#2444=FACE_OUTER_BOUND('',#3170,.T.);
#2445=FACE_OUTER_BOUND('',#3171,.T.);
#2446=FACE_OUTER_BOUND('',#3172,.T.);
#2447=FACE_OUTER_BOUND('',#3173,.T.);
#2448=FACE_OUTER_BOUND('',#3174,.T.);
#2449=FACE_OUTER_BOUND('',#3175,.T.);
#2450=FACE_OUTER_BOUND('',#3176,.T.);
#2451=FACE_OUTER_BOUND('',#3177,.T.);
#2452=FACE_OUTER_BOUND('',#3178,.T.);
#2453=FACE_OUTER_BOUND('',#3179,.T.);
#2454=FACE_OUTER_BOUND('',#3180,.T.);
#2455=FACE_OUTER_BOUND('',#3181,.T.);
#2456=FACE_OUTER_BOUND('',#3182,.T.);
#2457=FACE_OUTER_BOUND('',#3183,.T.);
#2458=FACE_OUTER_BOUND('',#3184,.T.);
#2459=FACE_OUTER_BOUND('',#3185,.T.);
#2460=FACE_OUTER_BOUND('',#3186,.T.);
#2461=FACE_OUTER_BOUND('',#3187,.T.);
#2462=FACE_OUTER_BOUND('',#3188,.T.);
#2463=FACE_OUTER_BOUND('',#3189,.T.);
#2464=FACE_OUTER_BOUND('',#3190,.T.);
#2465=FACE_OUTER_BOUND('',#3191,.T.);
#2466=FACE_OUTER_BOUND('',#3192,.T.);
#2467=FACE_OUTER_BOUND('',#3193,.T.);
#2468=FACE_OUTER_BOUND('',#3194,.T.);
#2469=FACE_OUTER_BOUND('',#3195,.T.);
#2470=FACE_OUTER_BOUND('',#3196,.T.);
#2471=FACE_OUTER_BOUND('',#3197,.T.);
#2472=FACE_OUTER_BOUND('',#3198,.T.);
#2473=FACE_OUTER_BOUND('',#3199,.T.);
#2474=FACE_OUTER_BOUND('',#3200,.T.);
#2475=FACE_OUTER_BOUND('',#3201,.T.);
#2476=FACE_OUTER_BOUND('',#3202,.T.);
#2477=FACE_OUTER_BOUND('',#3203,.T.);
#2478=FACE_OUTER_BOUND('',#3204,.T.);
#2479=FACE_OUTER_BOUND('',#3205,.T.);
#2480=FACE_OUTER_BOUND('',#3206,.T.);
#2481=FACE_OUTER_BOUND('',#3207,.T.);
#2482=FACE_OUTER_BOUND('',#3208,.T.);
#2483=FACE_OUTER_BOUND('',#3209,.T.);
#2484=FACE_OUTER_BOUND('',#3210,.T.);
#2485=FACE_OUTER_BOUND('',#3211,.T.);
#2486=FACE_OUTER_BOUND('',#3212,.T.);
#2487=FACE_OUTER_BOUND('',#3213,.T.);
#2488=FACE_OUTER_BOUND('',#3214,.T.);
#2489=FACE_OUTER_BOUND('',#3215,.T.);
#2490=FACE_OUTER_BOUND('',#3216,.T.);
#2491=FACE_OUTER_BOUND('',#3217,.T.);
#2492=FACE_OUTER_BOUND('',#3218,.T.);
#2493=FACE_OUTER_BOUND('',#3219,.T.);
#2494=FACE_OUTER_BOUND('',#3220,.T.);
#2495=FACE_OUTER_BOUND('',#3221,.T.);
#2496=FACE_OUTER_BOUND('',#3222,.T.);
#2497=FACE_OUTER_BOUND('',#3223,.T.);
#2498=FACE_OUTER_BOUND('',#3224,.T.);
#2499=FACE_OUTER_BOUND('',#3225,.T.);
#2500=FACE_OUTER_BOUND('',#3226,.T.);
#2501=FACE_OUTER_BOUND('',#3227,.T.);
#2502=FACE_OUTER_BOUND('',#3228,.T.);
#2503=FACE_OUTER_BOUND('',#3229,.T.);
#2504=FACE_OUTER_BOUND('',#3230,.T.);
#2505=FACE_OUTER_BOUND('',#3231,.T.);
#2506=FACE_OUTER_BOUND('',#3232,.T.);
#2507=FACE_OUTER_BOUND('',#3233,.T.);
#2508=FACE_OUTER_BOUND('',#3234,.T.);
#2509=FACE_OUTER_BOUND('',#3235,.T.);
#2510=FACE_OUTER_BOUND('',#3236,.T.);
#2511=FACE_OUTER_BOUND('',#3237,.T.);
#2512=FACE_OUTER_BOUND('',#3238,.T.);
#2513=FACE_OUTER_BOUND('',#3239,.T.);
#2514=FACE_OUTER_BOUND('',#3241,.T.);
#2515=FACE_OUTER_BOUND('',#3242,.T.);
#2516=FACE_OUTER_BOUND('',#3243,.T.);
#2517=FACE_OUTER_BOUND('',#3244,.T.);
#2518=FACE_OUTER_BOUND('',#3245,.T.);
#2519=FACE_OUTER_BOUND('',#3246,.T.);
#2520=FACE_OUTER_BOUND('',#3247,.T.);
#2521=FACE_OUTER_BOUND('',#3248,.T.);
#2522=FACE_OUTER_BOUND('',#3249,.T.);
#2523=FACE_OUTER_BOUND('',#3250,.T.);
#2524=FACE_OUTER_BOUND('',#3251,.T.);
#2525=FACE_OUTER_BOUND('',#3252,.T.);
#2526=FACE_OUTER_BOUND('',#3253,.T.);
#2527=FACE_OUTER_BOUND('',#3254,.T.);
#2528=FACE_OUTER_BOUND('',#3255,.T.);
#2529=FACE_OUTER_BOUND('',#3256,.T.);
#2530=FACE_OUTER_BOUND('',#3257,.T.);
#2531=FACE_OUTER_BOUND('',#3258,.T.);
#2532=FACE_OUTER_BOUND('',#3259,.T.);
#2533=FACE_OUTER_BOUND('',#3260,.T.);
#2534=FACE_OUTER_BOUND('',#3261,.T.);
#2535=FACE_OUTER_BOUND('',#3262,.T.);
#2536=FACE_OUTER_BOUND('',#3263,.T.);
#2537=FACE_OUTER_BOUND('',#3264,.T.);
#2538=FACE_OUTER_BOUND('',#3265,.T.);
#2539=FACE_OUTER_BOUND('',#3266,.T.);
#2540=FACE_OUTER_BOUND('',#3267,.T.);
#2541=FACE_OUTER_BOUND('',#3268,.T.);
#2542=FACE_OUTER_BOUND('',#3269,.T.);
#2543=FACE_OUTER_BOUND('',#3270,.T.);
#2544=FACE_OUTER_BOUND('',#3271,.T.);
#2545=FACE_OUTER_BOUND('',#3272,.T.);
#2546=FACE_OUTER_BOUND('',#3273,.T.);
#2547=FACE_OUTER_BOUND('',#3274,.T.);
#2548=FACE_OUTER_BOUND('',#3275,.T.);
#2549=FACE_OUTER_BOUND('',#3277,.T.);
#2550=FACE_OUTER_BOUND('',#3278,.T.);
#2551=FACE_OUTER_BOUND('',#3279,.T.);
#2552=FACE_OUTER_BOUND('',#3280,.T.);
#2553=FACE_OUTER_BOUND('',#3281,.T.);
#2554=FACE_OUTER_BOUND('',#3282,.T.);
#2555=FACE_OUTER_BOUND('',#3283,.T.);
#2556=FACE_OUTER_BOUND('',#3284,.T.);
#2557=FACE_OUTER_BOUND('',#3285,.T.);
#2558=FACE_OUTER_BOUND('',#3286,.T.);
#2559=FACE_OUTER_BOUND('',#3287,.T.);
#2560=FACE_OUTER_BOUND('',#3288,.T.);
#2561=FACE_OUTER_BOUND('',#3289,.T.);
#2562=FACE_OUTER_BOUND('',#3290,.T.);
#2563=FACE_OUTER_BOUND('',#3291,.T.);
#2564=FACE_OUTER_BOUND('',#3292,.T.);
#2565=FACE_OUTER_BOUND('',#3293,.T.);
#2566=FACE_OUTER_BOUND('',#3294,.T.);
#2567=FACE_OUTER_BOUND('',#3295,.T.);
#2568=FACE_OUTER_BOUND('',#3296,.T.);
#2569=FACE_OUTER_BOUND('',#3297,.T.);
#2570=FACE_OUTER_BOUND('',#3298,.T.);
#2571=FACE_OUTER_BOUND('',#3299,.T.);
#2572=FACE_OUTER_BOUND('',#3300,.T.);
#2573=FACE_OUTER_BOUND('',#3301,.T.);
#2574=FACE_OUTER_BOUND('',#3302,.T.);
#2575=FACE_OUTER_BOUND('',#3303,.T.);
#2576=FACE_OUTER_BOUND('',#3304,.T.);
#2577=FACE_OUTER_BOUND('',#3305,.T.);
#2578=FACE_OUTER_BOUND('',#3306,.T.);
#2579=FACE_OUTER_BOUND('',#3307,.T.);
#2580=FACE_OUTER_BOUND('',#3308,.T.);
#2581=FACE_OUTER_BOUND('',#3309,.T.);
#2582=FACE_OUTER_BOUND('',#3310,.T.);
#2583=FACE_OUTER_BOUND('',#3311,.T.);
#2584=FACE_OUTER_BOUND('',#3312,.T.);
#2585=FACE_OUTER_BOUND('',#3313,.T.);
#2586=FACE_OUTER_BOUND('',#3314,.T.);
#2587=FACE_OUTER_BOUND('',#3315,.T.);
#2588=FACE_OUTER_BOUND('',#3316,.T.);
#2589=FACE_OUTER_BOUND('',#3317,.T.);
#2590=FACE_OUTER_BOUND('',#3318,.T.);
#2591=FACE_OUTER_BOUND('',#3319,.T.);
#2592=FACE_OUTER_BOUND('',#3320,.T.);
#2593=FACE_OUTER_BOUND('',#3321,.T.);
#2594=FACE_OUTER_BOUND('',#3322,.T.);
#2595=FACE_OUTER_BOUND('',#3323,.T.);
#2596=FACE_OUTER_BOUND('',#3324,.T.);
#2597=FACE_OUTER_BOUND('',#3325,.T.);
#2598=FACE_OUTER_BOUND('',#3326,.T.);
#2599=FACE_OUTER_BOUND('',#3327,.T.);
#2600=FACE_OUTER_BOUND('',#3328,.T.);
#2601=FACE_OUTER_BOUND('',#3329,.T.);
#2602=FACE_OUTER_BOUND('',#3330,.T.);
#2603=FACE_OUTER_BOUND('',#3331,.T.);
#2604=FACE_OUTER_BOUND('',#3332,.T.);
#2605=FACE_OUTER_BOUND('',#3333,.T.);
#2606=FACE_OUTER_BOUND('',#3334,.T.);
#2607=FACE_OUTER_BOUND('',#3335,.T.);
#2608=FACE_OUTER_BOUND('',#3336,.T.);
#2609=FACE_OUTER_BOUND('',#3337,.T.);
#2610=FACE_OUTER_BOUND('',#3338,.T.);
#2611=FACE_OUTER_BOUND('',#3339,.T.);
#2612=FACE_OUTER_BOUND('',#3340,.T.);
#2613=FACE_OUTER_BOUND('',#3341,.T.);
#2614=FACE_OUTER_BOUND('',#3342,.T.);
#2615=FACE_OUTER_BOUND('',#3343,.T.);
#2616=FACE_OUTER_BOUND('',#3344,.T.);
#2617=FACE_OUTER_BOUND('',#3345,.T.);
#2618=FACE_OUTER_BOUND('',#3346,.T.);
#2619=FACE_OUTER_BOUND('',#3347,.T.);
#2620=FACE_OUTER_BOUND('',#3348,.T.);
#2621=FACE_OUTER_BOUND('',#3349,.T.);
#2622=FACE_OUTER_BOUND('',#3350,.T.);
#2623=FACE_OUTER_BOUND('',#3351,.T.);
#2624=FACE_OUTER_BOUND('',#3352,.T.);
#2625=FACE_OUTER_BOUND('',#3353,.T.);
#2626=FACE_OUTER_BOUND('',#3354,.T.);
#2627=FACE_OUTER_BOUND('',#3355,.T.);
#2628=FACE_OUTER_BOUND('',#3356,.T.);
#2629=FACE_OUTER_BOUND('',#3357,.T.);
#2630=FACE_OUTER_BOUND('',#3358,.T.);
#2631=FACE_OUTER_BOUND('',#3359,.T.);
#2632=FACE_OUTER_BOUND('',#3360,.T.);
#2633=FACE_OUTER_BOUND('',#3361,.T.);
#2634=FACE_OUTER_BOUND('',#3362,.T.);
#2635=FACE_OUTER_BOUND('',#3363,.T.);
#2636=FACE_OUTER_BOUND('',#3364,.T.);
#2637=FACE_OUTER_BOUND('',#3365,.T.);
#2638=FACE_OUTER_BOUND('',#3366,.T.);
#2639=FACE_OUTER_BOUND('',#3367,.T.);
#2640=FACE_OUTER_BOUND('',#3368,.T.);
#2641=FACE_OUTER_BOUND('',#3369,.T.);
#2642=FACE_OUTER_BOUND('',#3370,.T.);
#2643=FACE_OUTER_BOUND('',#3371,.T.);
#2644=FACE_OUTER_BOUND('',#3372,.T.);
#2645=FACE_OUTER_BOUND('',#3373,.T.);
#2646=FACE_OUTER_BOUND('',#3374,.T.);
#2647=FACE_OUTER_BOUND('',#3375,.T.);
#2648=FACE_OUTER_BOUND('',#3376,.T.);
#2649=FACE_OUTER_BOUND('',#3377,.T.);
#2650=FACE_OUTER_BOUND('',#3378,.T.);
#2651=FACE_OUTER_BOUND('',#3379,.T.);
#2652=FACE_OUTER_BOUND('',#3380,.T.);
#2653=FACE_OUTER_BOUND('',#3381,.T.);
#2654=FACE_OUTER_BOUND('',#3382,.T.);
#2655=FACE_OUTER_BOUND('',#3383,.T.);
#2656=FACE_OUTER_BOUND('',#3384,.T.);
#2657=FACE_OUTER_BOUND('',#3385,.T.);
#2658=FACE_OUTER_BOUND('',#3386,.T.);
#2659=FACE_OUTER_BOUND('',#3387,.T.);
#2660=FACE_OUTER_BOUND('',#3388,.T.);
#2661=FACE_OUTER_BOUND('',#3389,.T.);
#2662=FACE_OUTER_BOUND('',#3391,.T.);
#2663=FACE_OUTER_BOUND('',#3392,.T.);
#2664=FACE_OUTER_BOUND('',#3393,.T.);
#2665=FACE_OUTER_BOUND('',#3394,.T.);
#2666=FACE_OUTER_BOUND('',#3395,.T.);
#2667=FACE_OUTER_BOUND('',#3396,.T.);
#2668=FACE_OUTER_BOUND('',#3397,.T.);
#2669=FACE_OUTER_BOUND('',#3398,.T.);
#2670=FACE_OUTER_BOUND('',#3399,.T.);
#2671=FACE_OUTER_BOUND('',#3400,.T.);
#2672=FACE_OUTER_BOUND('',#3401,.T.);
#2673=FACE_OUTER_BOUND('',#3402,.T.);
#2674=FACE_OUTER_BOUND('',#3403,.T.);
#2675=EDGE_LOOP('',(#8965,#8966,#8967,#8968));
#2676=EDGE_LOOP('',(#8969));
#2677=EDGE_LOOP('',(#8970));
#2678=EDGE_LOOP('',(#8971,#8972,#8973,#8974,#8975));
#2679=EDGE_LOOP('',(#8976,#8977,#8978,#8979));
#2680=EDGE_LOOP('',(#8980));
#2681=EDGE_LOOP('',(#8981));
#2682=EDGE_LOOP('',(#8982,#8983,#8984,#8985,#8986));
#2683=EDGE_LOOP('',(#8987,#8988,#8989,#8990));
#2684=EDGE_LOOP('',(#8991));
#2685=EDGE_LOOP('',(#8992));
#2686=EDGE_LOOP('',(#8993,#8994,#8995,#8996,#8997));
#2687=EDGE_LOOP('',(#8998,#8999,#9000,#9001));
#2688=EDGE_LOOP('',(#9002));
#2689=EDGE_LOOP('',(#9003));
#2690=EDGE_LOOP('',(#9004,#9005,#9006,#9007,#9008));
#2691=EDGE_LOOP('',(#9009,#9010,#9011,#9012));
#2692=EDGE_LOOP('',(#9013));
#2693=EDGE_LOOP('',(#9014));
#2694=EDGE_LOOP('',(#9015,#9016,#9017,#9018,#9019));
#2695=EDGE_LOOP('',(#9020,#9021,#9022,#9023));
#2696=EDGE_LOOP('',(#9024));
#2697=EDGE_LOOP('',(#9025));
#2698=EDGE_LOOP('',(#9026,#9027,#9028,#9029,#9030));
#2699=EDGE_LOOP('',(#9031,#9032,#9033,#9034));
#2700=EDGE_LOOP('',(#9035,#9036,#9037,#9038));
#2701=EDGE_LOOP('',(#9039));
#2702=EDGE_LOOP('',(#9040));
#2703=EDGE_LOOP('',(#9041));
#2704=EDGE_LOOP('',(#9042));
#2705=EDGE_LOOP('',(#9043,#9044,#9045,#9046));
#2706=EDGE_LOOP('',(#9047,#9048,#9049,#9050));
#2707=EDGE_LOOP('',(#9051,#9052,#9053,#9054));
#2708=EDGE_LOOP('',(#9055,#9056,#9057,#9058));
#2709=EDGE_LOOP('',(#9059,#9060,#9061,#9062));
#2710=EDGE_LOOP('',(#9063,#9064,#9065,#9066));
#2711=EDGE_LOOP('',(#9067,#9068,#9069,#9070));
#2712=EDGE_LOOP('',(#9071));
#2713=EDGE_LOOP('',(#9072));
#2714=EDGE_LOOP('',(#9073));
#2715=EDGE_LOOP('',(#9074));
#2716=EDGE_LOOP('',(#9075));
#2717=EDGE_LOOP('',(#9076));
#2718=EDGE_LOOP('',(#9077));
#2719=EDGE_LOOP('',(#9078));
#2720=EDGE_LOOP('',(#9079,#9080,#9081,#9082));
#2721=EDGE_LOOP('',(#9083,#9084,#9085,#9086));
#2722=EDGE_LOOP('',(#9087,#9088,#9089,#9090));
#2723=EDGE_LOOP('',(#9091,#9092,#9093,#9094));
#2724=EDGE_LOOP('',(#9095,#9096,#9097,#9098));
#2725=EDGE_LOOP('',(#9099,#9100,#9101,#9102));
#2726=EDGE_LOOP('',(#9103,#9104,#9105,#9106,#9107,#9108,#9109,#9110,#9111,
#9112,#9113,#9114,#9115,#9116,#9117,#9118,#9119,#9120));
#2727=EDGE_LOOP('',(#9121,#9122,#9123,#9124));
#2728=EDGE_LOOP('',(#9125,#9126,#9127,#9128));
#2729=EDGE_LOOP('',(#9129,#9130,#9131,#9132));
#2730=EDGE_LOOP('',(#9133,#9134,#9135,#9136));
#2731=EDGE_LOOP('',(#9137));
#2732=EDGE_LOOP('',(#9138));
#2733=EDGE_LOOP('',(#9139));
#2734=EDGE_LOOP('',(#9140));
#2735=EDGE_LOOP('',(#9141));
#2736=EDGE_LOOP('',(#9142));
#2737=EDGE_LOOP('',(#9143));
#2738=EDGE_LOOP('',(#9144));
#2739=EDGE_LOOP('',(#9145));
#2740=EDGE_LOOP('',(#9146));
#2741=EDGE_LOOP('',(#9147,#9148,#9149,#9150));
#2742=EDGE_LOOP('',(#9151,#9152,#9153,#9154));
#2743=EDGE_LOOP('',(#9155,#9156));
#2744=EDGE_LOOP('',(#9157,#9158));
#2745=EDGE_LOOP('',(#9159,#9160));
#2746=EDGE_LOOP('',(#9161,#9162,#9163,#9164));
#2747=EDGE_LOOP('',(#9165,#9166,#9167,#9168));
#2748=EDGE_LOOP('',(#9169,#9170,#9171,#9172));
#2749=EDGE_LOOP('',(#9173,#9174,#9175,#9176));
#2750=EDGE_LOOP('',(#9177,#9178,#9179,#9180));
#2751=EDGE_LOOP('',(#9181,#9182));
#2752=EDGE_LOOP('',(#9183,#9184));
#2753=EDGE_LOOP('',(#9185,#9186));
#2754=EDGE_LOOP('',(#9187,#9188,#9189,#9190));
#2755=EDGE_LOOP('',(#9191,#9192,#9193,#9194));
#2756=EDGE_LOOP('',(#9195,#9196,#9197,#9198));
#2757=EDGE_LOOP('',(#9199,#9200,#9201,#9202));
#2758=EDGE_LOOP('',(#9203,#9204,#9205,#9206,#9207,#9208,#9209,#9210,#9211,
#9212,#9213,#9214,#9215,#9216,#9217,#9218,#9219,#9220));
#2759=EDGE_LOOP('',(#9221,#9222,#9223,#9224));
#2760=EDGE_LOOP('',(#9225,#9226,#9227,#9228));
#2761=EDGE_LOOP('',(#9229));
#2762=EDGE_LOOP('',(#9230));
#2763=EDGE_LOOP('',(#9231));
#2764=EDGE_LOOP('',(#9232));
#2765=EDGE_LOOP('',(#9233,#9234));
#2766=EDGE_LOOP('',(#9235,#9236));
#2767=EDGE_LOOP('',(#9237));
#2768=EDGE_LOOP('',(#9238));
#2769=EDGE_LOOP('',(#9239,#9240));
#2770=EDGE_LOOP('',(#9241,#9242));
#2771=EDGE_LOOP('',(#9243));
#2772=EDGE_LOOP('',(#9244));
#2773=EDGE_LOOP('',(#9245,#9246,#9247,#9248));
#2774=EDGE_LOOP('',(#9249,#9250,#9251,#9252));
#2775=EDGE_LOOP('',(#9253,#9254,#9255,#9256));
#2776=EDGE_LOOP('',(#9257,#9258,#9259,#9260));
#2777=EDGE_LOOP('',(#9261,#9262,#9263,#9264));
#2778=EDGE_LOOP('',(#9265,#9266,#9267,#9268));
#2779=EDGE_LOOP('',(#9269,#9270,#9271,#9272));
#2780=EDGE_LOOP('',(#9273,#9274,#9275,#9276));
#2781=EDGE_LOOP('',(#9277,#9278,#9279,#9280));
#2782=EDGE_LOOP('',(#9281,#9282,#9283,#9284));
#2783=EDGE_LOOP('',(#9285,#9286,#9287,#9288));
#2784=EDGE_LOOP('',(#9289,#9290,#9291,#9292,#9293,#9294));
#2785=EDGE_LOOP('',(#9295,#9296));
#2786=EDGE_LOOP('',(#9297));
#2787=EDGE_LOOP('',(#9298));
#2788=EDGE_LOOP('',(#9299));
#2789=EDGE_LOOP('',(#9300));
#2790=EDGE_LOOP('',(#9301));
#2791=EDGE_LOOP('',(#9302,#9303,#9304,#9305,#9306,#9307));
#2792=EDGE_LOOP('',(#9308,#9309));
#2793=EDGE_LOOP('',(#9310));
#2794=EDGE_LOOP('',(#9311));
#2795=EDGE_LOOP('',(#9312));
#2796=EDGE_LOOP('',(#9313,#9314,#9315,#9316,#9317,#9318));
#2797=EDGE_LOOP('',(#9319,#9320));
#2798=EDGE_LOOP('',(#9321));
#2799=EDGE_LOOP('',(#9322));
#2800=EDGE_LOOP('',(#9323));
#2801=EDGE_LOOP('',(#9324,#9325,#9326,#9327,#9328,#9329));
#2802=EDGE_LOOP('',(#9330,#9331));
#2803=EDGE_LOOP('',(#9332));
#2804=EDGE_LOOP('',(#9333,#9334,#9335,#9336,#9337,#9338,#9339));
#2805=EDGE_LOOP('',(#9340,#9341,#9342,#9343,#9344,#9345,#9346));
#2806=EDGE_LOOP('',(#9347,#9348,#9349,#9350,#9351,#9352,#9353));
#2807=EDGE_LOOP('',(#9354,#9355,#9356,#9357,#9358,#9359,#9360));
#2808=EDGE_LOOP('',(#9361,#9362,#9363,#9364));
#2809=EDGE_LOOP('',(#9365,#9366,#9367,#9368));
#2810=EDGE_LOOP('',(#9369,#9370,#9371,#9372));
#2811=EDGE_LOOP('',(#9373,#9374,#9375,#9376));
#2812=EDGE_LOOP('',(#9377,#9378,#9379,#9380));
#2813=EDGE_LOOP('',(#9381,#9382,#9383,#9384));
#2814=EDGE_LOOP('',(#9385,#9386,#9387,#9388));
#2815=EDGE_LOOP('',(#9389,#9390,#9391,#9392));
#2816=EDGE_LOOP('',(#9393,#9394,#9395,#9396));
#2817=EDGE_LOOP('',(#9397,#9398,#9399,#9400));
#2818=EDGE_LOOP('',(#9401,#9402,#9403,#9404));
#2819=EDGE_LOOP('',(#9405,#9406,#9407,#9408));
#2820=EDGE_LOOP('',(#9409,#9410,#9411,#9412,#9413,#9414,#9415,#9416));
#2821=EDGE_LOOP('',(#9417,#9418,#9419,#9420,#9421,#9422,#9423,#9424));
#2822=EDGE_LOOP('',(#9425,#9426,#9427,#9428,#9429,#9430,#9431,#9432));
#2823=EDGE_LOOP('',(#9433,#9434,#9435,#9436,#9437,#9438,#9439,#9440));
#2824=EDGE_LOOP('',(#9441,#9442,#9443,#9444));
#2825=EDGE_LOOP('',(#9445,#9446,#9447,#9448));
#2826=EDGE_LOOP('',(#9449,#9450,#9451,#9452));
#2827=EDGE_LOOP('',(#9453,#9454,#9455,#9456));
#2828=EDGE_LOOP('',(#9457,#9458,#9459));
#2829=EDGE_LOOP('',(#9460,#9461,#9462));
#2830=EDGE_LOOP('',(#9463,#9464,#9465));
#2831=EDGE_LOOP('',(#9466,#9467,#9468));
#2832=EDGE_LOOP('',(#9469,#9470,#9471));
#2833=EDGE_LOOP('',(#9472,#9473,#9474));
#2834=EDGE_LOOP('',(#9475,#9476,#9477));
#2835=EDGE_LOOP('',(#9478,#9479,#9480));
#2836=EDGE_LOOP('',(#9481,#9482,#9483,#9484));
#2837=EDGE_LOOP('',(#9485,#9486,#9487,#9488));
#2838=EDGE_LOOP('',(#9489,#9490,#9491,#9492));
#2839=EDGE_LOOP('',(#9493,#9494,#9495,#9496));
#2840=EDGE_LOOP('',(#9497,#9498,#9499,#9500));
#2841=EDGE_LOOP('',(#9501,#9502,#9503,#9504));
#2842=EDGE_LOOP('',(#9505,#9506,#9507,#9508));
#2843=EDGE_LOOP('',(#9509,#9510,#9511,#9512));
#2844=EDGE_LOOP('',(#9513,#9514,#9515,#9516));
#2845=EDGE_LOOP('',(#9517));
#2846=EDGE_LOOP('',(#9518));
#2847=EDGE_LOOP('',(#9519));
#2848=EDGE_LOOP('',(#9520));
#2849=EDGE_LOOP('',(#9521));
#2850=EDGE_LOOP('',(#9522));
#2851=EDGE_LOOP('',(#9523));
#2852=EDGE_LOOP('',(#9524));
#2853=EDGE_LOOP('',(#9525,#9526,#9527,#9528,#9529));
#2854=EDGE_LOOP('',(#9530,#9531,#9532));
#2855=EDGE_LOOP('',(#9533,#9534,#9535,#9536,#9537));
#2856=EDGE_LOOP('',(#9538,#9539,#9540));
#2857=EDGE_LOOP('',(#9541,#9542,#9543,#9544,#9545));
#2858=EDGE_LOOP('',(#9546,#9547,#9548));
#2859=EDGE_LOOP('',(#9549));
#2860=EDGE_LOOP('',(#9550,#9551,#9552,#9553));
#2861=EDGE_LOOP('',(#9554,#9555,#9556,#9557));
#2862=EDGE_LOOP('',(#9558,#9559));
#2863=EDGE_LOOP('',(#9560,#9561));
#2864=EDGE_LOOP('',(#9562,#9563));
#2865=EDGE_LOOP('',(#9564,#9565,#9566,#9567));
#2866=EDGE_LOOP('',(#9568));
#2867=EDGE_LOOP('',(#9569,#9570,#9571,#9572));
#2868=EDGE_LOOP('',(#9573,#9574,#9575,#9576));
#2869=EDGE_LOOP('',(#9577));
#2870=EDGE_LOOP('',(#9578));
#2871=EDGE_LOOP('',(#9579,#9580,#9581,#9582,#9583,#9584));
#2872=EDGE_LOOP('',(#9585,#9586,#9587,#9588));
#2873=EDGE_LOOP('',(#9589,#9590,#9591,#9592,#9593,#9594));
#2874=EDGE_LOOP('',(#9595,#9596,#9597,#9598,#9599));
#2875=EDGE_LOOP('',(#9600,#9601,#9602,#9603));
#2876=EDGE_LOOP('',(#9604,#9605));
#2877=EDGE_LOOP('',(#9606,#9607));
#2878=EDGE_LOOP('',(#9608,#9609,#9610,#9611,#9612));
#2879=EDGE_LOOP('',(#9613,#9614,#9615,#9616));
#2880=EDGE_LOOP('',(#9617,#9618,#9619,#9620,#9621,#9622,#9623,#9624,#9625,
#9626));
#2881=EDGE_LOOP('',(#9627,#9628,#9629,#9630,#9631,#9632));
#2882=EDGE_LOOP('',(#9633,#9634,#9635,#9636));
#2883=EDGE_LOOP('',(#9637,#9638,#9639,#9640,#9641,#9642,#9643,#9644,#9645,
#9646));
#2884=EDGE_LOOP('',(#9647,#9648,#9649,#9650,#9651,#9652));
#2885=EDGE_LOOP('',(#9653,#9654,#9655,#9656));
#2886=EDGE_LOOP('',(#9657,#9658,#9659,#9660));
#2887=EDGE_LOOP('',(#9661,#9662,#9663,#9664));
#2888=EDGE_LOOP('',(#9665,#9666,#9667,#9668));
#2889=EDGE_LOOP('',(#9669,#9670,#9671,#9672));
#2890=EDGE_LOOP('',(#9673,#9674,#9675,#9676));
#2891=EDGE_LOOP('',(#9677,#9678,#9679,#9680,#9681,#9682));
#2892=EDGE_LOOP('',(#9683,#9684,#9685,#9686,#9687,#9688));
#2893=EDGE_LOOP('',(#9689,#9690,#9691,#9692));
#2894=EDGE_LOOP('',(#9693,#9694,#9695,#9696));
#2895=EDGE_LOOP('',(#9697,#9698,#9699,#9700));
#2896=EDGE_LOOP('',(#9701,#9702,#9703,#9704));
#2897=EDGE_LOOP('',(#9705,#9706,#9707,#9708));
#2898=EDGE_LOOP('',(#9709,#9710,#9711,#9712));
#2899=EDGE_LOOP('',(#9713,#9714,#9715,#9716));
#2900=EDGE_LOOP('',(#9717,#9718,#9719,#9720));
#2901=EDGE_LOOP('',(#9721,#9722,#9723,#9724));
#2902=EDGE_LOOP('',(#9725,#9726,#9727,#9728));
#2903=EDGE_LOOP('',(#9729,#9730,#9731,#9732));
#2904=EDGE_LOOP('',(#9733,#9734,#9735,#9736));
#2905=EDGE_LOOP('',(#9737,#9738,#9739,#9740));
#2906=EDGE_LOOP('',(#9741,#9742,#9743,#9744));
#2907=EDGE_LOOP('',(#9745,#9746,#9747,#9748));
#2908=EDGE_LOOP('',(#9749,#9750,#9751,#9752));
#2909=EDGE_LOOP('',(#9753,#9754,#9755,#9756));
#2910=EDGE_LOOP('',(#9757,#9758,#9759,#9760));
#2911=EDGE_LOOP('',(#9761,#9762,#9763,#9764));
#2912=EDGE_LOOP('',(#9765,#9766,#9767,#9768));
#2913=EDGE_LOOP('',(#9769,#9770,#9771,#9772));
#2914=EDGE_LOOP('',(#9773,#9774,#9775,#9776));
#2915=EDGE_LOOP('',(#9777,#9778,#9779,#9780));
#2916=EDGE_LOOP('',(#9781,#9782,#9783,#9784));
#2917=EDGE_LOOP('',(#9785,#9786,#9787,#9788));
#2918=EDGE_LOOP('',(#9789,#9790,#9791,#9792));
#2919=EDGE_LOOP('',(#9793,#9794,#9795,#9796));
#2920=EDGE_LOOP('',(#9797,#9798,#9799,#9800));
#2921=EDGE_LOOP('',(#9801,#9802,#9803,#9804));
#2922=EDGE_LOOP('',(#9805,#9806,#9807,#9808));
#2923=EDGE_LOOP('',(#9809,#9810,#9811,#9812));
#2924=EDGE_LOOP('',(#9813,#9814,#9815,#9816));
#2925=EDGE_LOOP('',(#9817,#9818,#9819,#9820));
#2926=EDGE_LOOP('',(#9821,#9822,#9823,#9824));
#2927=EDGE_LOOP('',(#9825,#9826,#9827,#9828));
#2928=EDGE_LOOP('',(#9829,#9830,#9831,#9832));
#2929=EDGE_LOOP('',(#9833,#9834,#9835,#9836));
#2930=EDGE_LOOP('',(#9837,#9838,#9839,#9840));
#2931=EDGE_LOOP('',(#9841,#9842,#9843,#9844));
#2932=EDGE_LOOP('',(#9845,#9846,#9847,#9848));
#2933=EDGE_LOOP('',(#9849,#9850,#9851,#9852));
#2934=EDGE_LOOP('',(#9853,#9854,#9855,#9856));
#2935=EDGE_LOOP('',(#9857,#9858));
#2936=EDGE_LOOP('',(#9859,#9860,#9861,#9862));
#2937=EDGE_LOOP('',(#9863,#9864,#9865,#9866,#9867,#9868));
#2938=EDGE_LOOP('',(#9869,#9870,#9871,#9872));
#2939=EDGE_LOOP('',(#9873,#9874,#9875,#9876,#9877,#9878));
#2940=EDGE_LOOP('',(#9879,#9880,#9881,#9882));
#2941=EDGE_LOOP('',(#9883,#9884,#9885,#9886,#9887,#9888));
#2942=EDGE_LOOP('',(#9889,#9890,#9891,#9892));
#2943=EDGE_LOOP('',(#9893,#9894,#9895,#9896,#9897,#9898));
#2944=EDGE_LOOP('',(#9899,#9900,#9901,#9902,#9903));
#2945=EDGE_LOOP('',(#9904,#9905,#9906,#9907,#9908,#9909));
#2946=EDGE_LOOP('',(#9910,#9911,#9912,#9913,#9914));
#2947=EDGE_LOOP('',(#9915,#9916,#9917,#9918,#9919,#9920));
#2948=EDGE_LOOP('',(#9921,#9922,#9923,#9924));
#2949=EDGE_LOOP('',(#9925,#9926,#9927,#9928,#9929,#9930));
#2950=EDGE_LOOP('',(#9931,#9932,#9933,#9934));
#2951=EDGE_LOOP('',(#9935,#9936,#9937,#9938,#9939,#9940));
#2952=EDGE_LOOP('',(#9941,#9942,#9943,#9944));
#2953=EDGE_LOOP('',(#9945,#9946,#9947,#9948,#9949,#9950));
#2954=EDGE_LOOP('',(#9951,#9952,#9953,#9954));
#2955=EDGE_LOOP('',(#9955,#9956,#9957,#9958,#9959,#9960,#9961,#9962,#9963,
#9964,#9965,#9966,#9967,#9968,#9969,#9970,#9971,#9972,#9973,#9974,#9975,
#9976,#9977,#9978,#9979,#9980,#9981,#9982,#9983,#9984,#9985,#9986,#9987,
#9988,#9989,#9990,#9991,#9992,#9993,#9994,#9995,#9996,#9997,#9998));
#2956=EDGE_LOOP('',(#9999,#10000,#10001,#10002,#10003,#10004));
#2957=EDGE_LOOP('',(#10005,#10006,#10007,#10008));
#2958=EDGE_LOOP('',(#10009,#10010,#10011,#10012,#10013,#10014,#10015,#10016,
#10017,#10018,#10019,#10020,#10021,#10022,#10023,#10024,#10025,#10026,#10027,
#10028,#10029,#10030,#10031,#10032,#10033,#10034,#10035,#10036,#10037,#10038,
#10039,#10040,#10041,#10042,#10043,#10044,#10045,#10046,#10047,#10048,#10049,
#10050,#10051,#10052,#10053,#10054,#10055,#10056,#10057,#10058,#10059,#10060,
#10061,#10062,#10063));
#2959=EDGE_LOOP('',(#10064,#10065,#10066,#10067,#10068));
#2960=EDGE_LOOP('',(#10069,#10070,#10071,#10072,#10073,#10074,#10075,#10076,
#10077,#10078,#10079,#10080,#10081,#10082,#10083,#10084,#10085,#10086,#10087,
#10088,#10089,#10090,#10091,#10092,#10093,#10094,#10095,#10096,#10097,#10098,
#10099,#10100,#10101,#10102,#10103,#10104,#10105,#10106,#10107,#10108,#10109,
#10110,#10111,#10112,#10113,#10114,#10115,#10116,#10117,#10118,#10119,#10120,
#10121,#10122));
#2961=EDGE_LOOP('',(#10123,#10124,#10125,#10126,#10127,#10128,#10129));
#2962=EDGE_LOOP('',(#10130));
#2963=EDGE_LOOP('',(#10131));
#2964=EDGE_LOOP('',(#10132,#10133,#10134,#10135,#10136,#10137,#10138));
#2965=EDGE_LOOP('',(#10139));
#2966=EDGE_LOOP('',(#10140,#10141,#10142,#10143));
#2967=EDGE_LOOP('',(#10144,#10145,#10146,#10147));
#2968=EDGE_LOOP('',(#10148,#10149,#10150));
#2969=EDGE_LOOP('',(#10151,#10152,#10153,#10154,#10155,#10156,#10157,#10158,
#10159,#10160,#10161,#10162,#10163,#10164,#10165,#10166,#10167,#10168,#10169,
#10170,#10171,#10172,#10173,#10174,#10175,#10176,#10177,#10178,#10179,#10180,
#10181,#10182,#10183,#10184,#10185,#10186,#10187,#10188,#10189,#10190,#10191,
#10192,#10193,#10194,#10195,#10196,#10197,#10198,#10199,#10200,#10201,#10202,
#10203,#10204,#10205,#10206,#10207,#10208,#10209,#10210,#10211,#10212,#10213,
#10214,#10215,#10216,#10217,#10218,#10219,#10220,#10221,#10222,#10223,#10224,
#10225,#10226,#10227,#10228,#10229,#10230,#10231,#10232,#10233,#10234,#10235,
#10236,#10237,#10238,#10239,#10240,#10241,#10242,#10243,#10244,#10245,#10246,
#10247,#10248,#10249,#10250,#10251,#10252,#10253,#10254,#10255,#10256,#10257,
#10258,#10259,#10260,#10261));
#2970=EDGE_LOOP('',(#10262,#10263,#10264,#10265));
#2971=EDGE_LOOP('',(#10266,#10267,#10268,#10269));
#2972=EDGE_LOOP('',(#10270,#10271,#10272));
#2973=EDGE_LOOP('',(#10273,#10274,#10275,#10276));
#2974=EDGE_LOOP('',(#10277,#10278,#10279,#10280));
#2975=EDGE_LOOP('',(#10281,#10282,#10283));
#2976=EDGE_LOOP('',(#10284,#10285,#10286,#10287));
#2977=EDGE_LOOP('',(#10288,#10289,#10290,#10291));
#2978=EDGE_LOOP('',(#10292,#10293,#10294));
#2979=EDGE_LOOP('',(#10295,#10296,#10297,#10298));
#2980=EDGE_LOOP('',(#10299,#10300,#10301,#10302));
#2981=EDGE_LOOP('',(#10303,#10304,#10305));
#2982=EDGE_LOOP('',(#10306,#10307,#10308,#10309));
#2983=EDGE_LOOP('',(#10310,#10311,#10312,#10313));
#2984=EDGE_LOOP('',(#10314,#10315,#10316));
#2985=EDGE_LOOP('',(#10317,#10318,#10319,#10320));
#2986=EDGE_LOOP('',(#10321,#10322,#10323,#10324));
#2987=EDGE_LOOP('',(#10325,#10326,#10327));
#2988=EDGE_LOOP('',(#10328,#10329,#10330,#10331));
#2989=EDGE_LOOP('',(#10332,#10333,#10334,#10335));
#2990=EDGE_LOOP('',(#10336,#10337,#10338));
#2991=EDGE_LOOP('',(#10339,#10340,#10341,#10342));
#2992=EDGE_LOOP('',(#10343,#10344,#10345,#10346));
#2993=EDGE_LOOP('',(#10347,#10348,#10349));
#2994=EDGE_LOOP('',(#10350,#10351,#10352,#10353));
#2995=EDGE_LOOP('',(#10354,#10355,#10356,#10357));
#2996=EDGE_LOOP('',(#10358,#10359,#10360));
#2997=EDGE_LOOP('',(#10361,#10362,#10363,#10364));
#2998=EDGE_LOOP('',(#10365,#10366,#10367,#10368));
#2999=EDGE_LOOP('',(#10369,#10370,#10371));
#3000=EDGE_LOOP('',(#10372,#10373,#10374,#10375));
#3001=EDGE_LOOP('',(#10376,#10377,#10378,#10379));
#3002=EDGE_LOOP('',(#10380,#10381,#10382));
#3003=EDGE_LOOP('',(#10383,#10384,#10385,#10386));
#3004=EDGE_LOOP('',(#10387,#10388,#10389,#10390));
#3005=EDGE_LOOP('',(#10391,#10392,#10393));
#3006=EDGE_LOOP('',(#10394,#10395,#10396,#10397));
#3007=EDGE_LOOP('',(#10398,#10399,#10400,#10401));
#3008=EDGE_LOOP('',(#10402,#10403,#10404));
#3009=EDGE_LOOP('',(#10405,#10406,#10407,#10408));
#3010=EDGE_LOOP('',(#10409,#10410,#10411,#10412));
#3011=EDGE_LOOP('',(#10413,#10414,#10415));
#3012=EDGE_LOOP('',(#10416,#10417,#10418,#10419));
#3013=EDGE_LOOP('',(#10420,#10421,#10422,#10423));
#3014=EDGE_LOOP('',(#10424,#10425,#10426));
#3015=EDGE_LOOP('',(#10427,#10428,#10429,#10430));
#3016=EDGE_LOOP('',(#10431,#10432,#10433,#10434));
#3017=EDGE_LOOP('',(#10435,#10436,#10437));
#3018=EDGE_LOOP('',(#10438,#10439,#10440,#10441));
#3019=EDGE_LOOP('',(#10442,#10443,#10444,#10445));
#3020=EDGE_LOOP('',(#10446,#10447,#10448,#10449));
#3021=EDGE_LOOP('',(#10450,#10451,#10452,#10453));
#3022=EDGE_LOOP('',(#10454,#10455,#10456,#10457));
#3023=EDGE_LOOP('',(#10458,#10459,#10460));
#3024=EDGE_LOOP('',(#10461,#10462,#10463,#10464));
#3025=EDGE_LOOP('',(#10465,#10466,#10467,#10468));
#3026=EDGE_LOOP('',(#10469,#10470,#10471));
#3027=EDGE_LOOP('',(#10472,#10473,#10474,#10475));
#3028=EDGE_LOOP('',(#10476,#10477,#10478,#10479));
#3029=EDGE_LOOP('',(#10480,#10481,#10482));
#3030=EDGE_LOOP('',(#10483,#10484,#10485,#10486));
#3031=EDGE_LOOP('',(#10487,#10488,#10489,#10490));
#3032=EDGE_LOOP('',(#10491,#10492,#10493));
#3033=EDGE_LOOP('',(#10494,#10495,#10496,#10497));
#3034=EDGE_LOOP('',(#10498,#10499,#10500,#10501));
#3035=EDGE_LOOP('',(#10502,#10503,#10504));
#3036=EDGE_LOOP('',(#10505,#10506,#10507,#10508));
#3037=EDGE_LOOP('',(#10509,#10510,#10511,#10512));
#3038=EDGE_LOOP('',(#10513,#10514,#10515));
#3039=EDGE_LOOP('',(#10516,#10517,#10518,#10519));
#3040=EDGE_LOOP('',(#10520,#10521,#10522,#10523));
#3041=EDGE_LOOP('',(#10524,#10525,#10526));
#3042=EDGE_LOOP('',(#10527,#10528,#10529,#10530));
#3043=EDGE_LOOP('',(#10531,#10532,#10533,#10534));
#3044=EDGE_LOOP('',(#10535,#10536,#10537));
#3045=EDGE_LOOP('',(#10538,#10539,#10540,#10541));
#3046=EDGE_LOOP('',(#10542,#10543,#10544,#10545));
#3047=EDGE_LOOP('',(#10546,#10547,#10548));
#3048=EDGE_LOOP('',(#10549,#10550,#10551,#10552));
#3049=EDGE_LOOP('',(#10553,#10554,#10555,#10556));
#3050=EDGE_LOOP('',(#10557,#10558,#10559));
#3051=EDGE_LOOP('',(#10560,#10561,#10562,#10563));
#3052=EDGE_LOOP('',(#10564,#10565,#10566,#10567));
#3053=EDGE_LOOP('',(#10568,#10569,#10570));
#3054=EDGE_LOOP('',(#10571,#10572,#10573,#10574));
#3055=EDGE_LOOP('',(#10575,#10576,#10577,#10578));
#3056=EDGE_LOOP('',(#10579,#10580,#10581));
#3057=EDGE_LOOP('',(#10582,#10583,#10584,#10585));
#3058=EDGE_LOOP('',(#10586,#10587,#10588,#10589));
#3059=EDGE_LOOP('',(#10590,#10591,#10592));
#3060=EDGE_LOOP('',(#10593,#10594,#10595,#10596));
#3061=EDGE_LOOP('',(#10597,#10598,#10599,#10600));
#3062=EDGE_LOOP('',(#10601,#10602,#10603));
#3063=EDGE_LOOP('',(#10604,#10605,#10606,#10607));
#3064=EDGE_LOOP('',(#10608,#10609,#10610,#10611));
#3065=EDGE_LOOP('',(#10612,#10613,#10614));
#3066=EDGE_LOOP('',(#10615,#10616,#10617,#10618));
#3067=EDGE_LOOP('',(#10619,#10620,#10621,#10622));
#3068=EDGE_LOOP('',(#10623,#10624,#10625));
#3069=EDGE_LOOP('',(#10626,#10627,#10628,#10629));
#3070=EDGE_LOOP('',(#10630,#10631,#10632,#10633));
#3071=EDGE_LOOP('',(#10634,#10635,#10636));
#3072=EDGE_LOOP('',(#10637,#10638,#10639,#10640));
#3073=EDGE_LOOP('',(#10641,#10642,#10643,#10644));
#3074=EDGE_LOOP('',(#10645,#10646,#10647));
#3075=EDGE_LOOP('',(#10648,#10649,#10650,#10651,#10652,#10653,#10654,#10655,
#10656,#10657,#10658,#10659,#10660,#10661,#10662,#10663,#10664,#10665,#10666,
#10667,#10668,#10669,#10670,#10671,#10672,#10673,#10674,#10675,#10676,#10677,
#10678,#10679,#10680,#10681,#10682,#10683,#10684,#10685,#10686,#10687,#10688,
#10689,#10690,#10691,#10692,#10693,#10694,#10695,#10696,#10697,#10698,#10699,
#10700,#10701,#10702,#10703,#10704,#10705,#10706,#10707,#10708,#10709,#10710,
#10711,#10712,#10713,#10714,#10715,#10716,#10717,#10718,#10719,#10720,#10721,
#10722,#10723,#10724,#10725,#10726,#10727,#10728,#10729,#10730,#10731,#10732,
#10733,#10734,#10735,#10736,#10737,#10738,#10739,#10740,#10741,#10742,#10743,
#10744,#10745,#10746,#10747,#10748,#10749,#10750,#10751,#10752,#10753,#10754,
#10755,#10756,#10757,#10758,#10759,#10760,#10761,#10762,#10763,#10764,#10765,
#10766,#10767,#10768,#10769,#10770,#10771,#10772,#10773,#10774,#10775,#10776,
#10777,#10778,#10779,#10780,#10781,#10782,#10783,#10784,#10785,#10786,#10787,
#10788,#10789,#10790,#10791,#10792,#10793,#10794,#10795));
#3076=EDGE_LOOP('',(#10796));
#3077=EDGE_LOOP('',(#10797,#10798,#10799,#10800,#10801,#10802));
#3078=EDGE_LOOP('',(#10803,#10804));
#3079=EDGE_LOOP('',(#10805,#10806));
#3080=EDGE_LOOP('',(#10807,#10808));
#3081=EDGE_LOOP('',(#10809,#10810));
#3082=EDGE_LOOP('',(#10811,#10812));
#3083=EDGE_LOOP('',(#10813,#10814));
#3084=EDGE_LOOP('',(#10815,#10816,#10817,#10818,#10819,#10820,#10821,#10822));
#3085=EDGE_LOOP('',(#10823,#10824,#10825,#10826));
#3086=EDGE_LOOP('',(#10827,#10828,#10829,#10830));
#3087=EDGE_LOOP('',(#10831,#10832,#10833,#10834));
#3088=EDGE_LOOP('',(#10835,#10836,#10837,#10838));
#3089=EDGE_LOOP('',(#10839,#10840,#10841,#10842));
#3090=EDGE_LOOP('',(#10843,#10844,#10845,#10846));
#3091=EDGE_LOOP('',(#10847,#10848,#10849,#10850));
#3092=EDGE_LOOP('',(#10851,#10852,#10853,#10854,#10855,#10856));
#3093=EDGE_LOOP('',(#10857,#10858,#10859,#10860,#10861));
#3094=EDGE_LOOP('',(#10862,#10863,#10864,#10865,#10866));
#3095=EDGE_LOOP('',(#10867,#10868,#10869,#10870,#10871));
#3096=EDGE_LOOP('',(#10872,#10873,#10874,#10875,#10876));
#3097=EDGE_LOOP('',(#10877,#10878,#10879,#10880,#10881));
#3098=EDGE_LOOP('',(#10882,#10883,#10884,#10885,#10886));
#3099=EDGE_LOOP('',(#10887,#10888,#10889,#10890,#10891));
#3100=EDGE_LOOP('',(#10892,#10893,#10894,#10895,#10896));
#3101=EDGE_LOOP('',(#10897,#10898,#10899,#10900,#10901));
#3102=EDGE_LOOP('',(#10902,#10903,#10904,#10905,#10906));
#3103=EDGE_LOOP('',(#10907,#10908,#10909,#10910,#10911));
#3104=EDGE_LOOP('',(#10912,#10913,#10914,#10915,#10916));
#3105=EDGE_LOOP('',(#10917,#10918,#10919,#10920,#10921));
#3106=EDGE_LOOP('',(#10922,#10923,#10924,#10925,#10926));
#3107=EDGE_LOOP('',(#10927,#10928,#10929,#10930,#10931));
#3108=EDGE_LOOP('',(#10932,#10933,#10934,#10935,#10936));
#3109=EDGE_LOOP('',(#10937,#10938,#10939,#10940,#10941));
#3110=EDGE_LOOP('',(#10942,#10943,#10944,#10945,#10946));
#3111=EDGE_LOOP('',(#10947,#10948,#10949,#10950,#10951));
#3112=EDGE_LOOP('',(#10952,#10953,#10954,#10955,#10956,#10957));
#3113=EDGE_LOOP('',(#10958,#10959,#10960,#10961));
#3114=EDGE_LOOP('',(#10962,#10963,#10964,#10965,#10966,#10967));
#3115=EDGE_LOOP('',(#10968,#10969,#10970,#10971,#10972));
#3116=EDGE_LOOP('',(#10973,#10974,#10975,#10976,#10977));
#3117=EDGE_LOOP('',(#10978,#10979,#10980,#10981,#10982));
#3118=EDGE_LOOP('',(#10983,#10984,#10985,#10986,#10987,#10988,#10989,#10990,
#10991,#10992,#10993,#10994,#10995,#10996,#10997,#10998,#10999,#11000,#11001,
#11002,#11003,#11004,#11005,#11006,#11007,#11008,#11009,#11010,#11011,#11012,
#11013,#11014,#11015,#11016,#11017,#11018,#11019,#11020,#11021,#11022,#11023,
#11024,#11025,#11026,#11027,#11028,#11029,#11030,#11031,#11032,#11033,#11034,
#11035,#11036,#11037,#11038,#11039,#11040,#11041,#11042));
#3119=EDGE_LOOP('',(#11043,#11044,#11045,#11046,#11047,#11048));
#3120=EDGE_LOOP('',(#11049,#11050,#11051,#11052));
#3121=EDGE_LOOP('',(#11053,#11054,#11055,#11056,#11057,#11058,#11059,#11060,
#11061,#11062,#11063,#11064,#11065,#11066,#11067,#11068,#11069,#11070,#11071,
#11072,#11073,#11074,#11075,#11076,#11077,#11078,#11079,#11080,#11081,#11082,
#11083,#11084,#11085,#11086,#11087,#11088,#11089,#11090,#11091,#11092,#11093,
#11094,#11095,#11096,#11097,#11098,#11099,#11100,#11101,#11102,#11103,#11104,
#11105,#11106,#11107,#11108,#11109,#11110,#11111,#11112,#11113,#11114,#11115,
#11116,#11117,#11118,#11119,#11120,#11121,#11122,#11123,#11124,#11125,#11126,
#11127));
#3122=EDGE_LOOP('',(#11128,#11129,#11130,#11131,#11132));
#3123=EDGE_LOOP('',(#11133,#11134,#11135,#11136,#11137,#11138,#11139,#11140,
#11141,#11142,#11143,#11144,#11145,#11146,#11147,#11148,#11149,#11150,#11151,
#11152,#11153,#11154,#11155,#11156,#11157,#11158,#11159,#11160,#11161,#11162,
#11163,#11164,#11165,#11166,#11167,#11168,#11169,#11170,#11171,#11172,#11173,
#11174,#11175,#11176,#11177,#11178,#11179,#11180,#11181,#11182,#11183,#11184,
#11185,#11186,#11187,#11188,#11189,#11190,#11191,#11192,#11193,#11194,#11195,
#11196,#11197,#11198,#11199,#11200,#11201,#11202,#11203,#11204,#11205,#11206));
#3124=EDGE_LOOP('',(#11207,#11208,#11209,#11210,#11211,#11212,#11213));
#3125=EDGE_LOOP('',(#11214));
#3126=EDGE_LOOP('',(#11215));
#3127=EDGE_LOOP('',(#11216,#11217,#11218,#11219,#11220,#11221,#11222));
#3128=EDGE_LOOP('',(#11223));
#3129=EDGE_LOOP('',(#11224,#11225,#11226,#11227));
#3130=EDGE_LOOP('',(#11228,#11229,#11230,#11231));
#3131=EDGE_LOOP('',(#11232,#11233,#11234));
#3132=EDGE_LOOP('',(#11235,#11236,#11237,#11238,#11239,#11240,#11241,#11242,
#11243,#11244,#11245,#11246,#11247,#11248,#11249,#11250,#11251,#11252,#11253,
#11254,#11255,#11256,#11257,#11258,#11259,#11260,#11261,#11262,#11263,#11264,
#11265,#11266,#11267,#11268,#11269,#11270,#11271,#11272,#11273,#11274,#11275,
#11276,#11277,#11278,#11279,#11280,#11281,#11282,#11283,#11284,#11285,#11286,
#11287,#11288,#11289,#11290,#11291,#11292,#11293,#11294,#11295,#11296,#11297,
#11298,#11299,#11300,#11301,#11302,#11303,#11304,#11305,#11306,#11307,#11308,
#11309,#11310,#11311,#11312,#11313,#11314,#11315,#11316,#11317,#11318,#11319,
#11320,#11321,#11322,#11323,#11324,#11325,#11326,#11327,#11328,#11329,#11330,
#11331,#11332,#11333,#11334,#11335,#11336,#11337,#11338,#11339,#11340,#11341,
#11342,#11343,#11344,#11345));
#3133=EDGE_LOOP('',(#11346,#11347,#11348));
#3134=EDGE_LOOP('',(#11349,#11350,#11351,#11352));
#3135=EDGE_LOOP('',(#11353,#11354,#11355,#11356));
#3136=EDGE_LOOP('',(#11357,#11358,#11359,#11360,#11361,#11362,#11363,#11364,
#11365,#11366,#11367,#11368,#11369,#11370,#11371,#11372,#11373,#11374,#11375,
#11376,#11377,#11378,#11379,#11380,#11381,#11382,#11383,#11384,#11385,#11386,
#11387,#11388,#11389,#11390,#11391,#11392,#11393,#11394,#11395,#11396,#11397,
#11398,#11399,#11400,#11401,#11402,#11403,#11404,#11405,#11406,#11407,#11408,
#11409,#11410,#11411,#11412,#11413,#11414,#11415,#11416,#11417,#11418,#11419,
#11420,#11421,#11422,#11423,#11424,#11425,#11426,#11427,#11428,#11429,#11430,
#11431,#11432,#11433,#11434,#11435,#11436,#11437,#11438,#11439,#11440,#11441,
#11442,#11443,#11444,#11445,#11446,#11447,#11448,#11449,#11450,#11451,#11452,
#11453,#11454,#11455,#11456,#11457,#11458,#11459,#11460,#11461,#11462,#11463,
#11464,#11465,#11466,#11467,#11468,#11469,#11470,#11471,#11472,#11473,#11474,
#11475,#11476,#11477,#11478,#11479,#11480,#11481,#11482,#11483,#11484,#11485,
#11486,#11487,#11488,#11489,#11490,#11491,#11492,#11493,#11494,#11495,#11496,
#11497,#11498,#11499,#11500,#11501,#11502,#11503,#11504));
#3137=EDGE_LOOP('',(#11505,#11506,#11507,#11508));
#3138=EDGE_LOOP('',(#11509,#11510,#11511,#11512));
#3139=EDGE_LOOP('',(#11513,#11514,#11515));
#3140=EDGE_LOOP('',(#11516,#11517,#11518));
#3141=EDGE_LOOP('',(#11519,#11520,#11521,#11522));
#3142=EDGE_LOOP('',(#11523,#11524,#11525,#11526));
#3143=EDGE_LOOP('',(#11527,#11528,#11529,#11530));
#3144=EDGE_LOOP('',(#11531,#11532,#11533,#11534));
#3145=EDGE_LOOP('',(#11535,#11536,#11537));
#3146=EDGE_LOOP('',(#11538,#11539,#11540));
#3147=EDGE_LOOP('',(#11541,#11542,#11543,#11544));
#3148=EDGE_LOOP('',(#11545,#11546,#11547,#11548));
#3149=EDGE_LOOP('',(#11549,#11550,#11551,#11552));
#3150=EDGE_LOOP('',(#11553,#11554,#11555,#11556));
#3151=EDGE_LOOP('',(#11557,#11558,#11559));
#3152=EDGE_LOOP('',(#11560,#11561,#11562));
#3153=EDGE_LOOP('',(#11563,#11564,#11565,#11566));
#3154=EDGE_LOOP('',(#11567,#11568,#11569,#11570));
#3155=EDGE_LOOP('',(#11571,#11572,#11573,#11574));
#3156=EDGE_LOOP('',(#11575,#11576,#11577,#11578));
#3157=EDGE_LOOP('',(#11579,#11580,#11581));
#3158=EDGE_LOOP('',(#11582,#11583,#11584));
#3159=EDGE_LOOP('',(#11585,#11586,#11587,#11588));
#3160=EDGE_LOOP('',(#11589,#11590,#11591,#11592));
#3161=EDGE_LOOP('',(#11593,#11594,#11595,#11596));
#3162=EDGE_LOOP('',(#11597,#11598,#11599,#11600));
#3163=EDGE_LOOP('',(#11601,#11602,#11603));
#3164=EDGE_LOOP('',(#11604,#11605,#11606));
#3165=EDGE_LOOP('',(#11607,#11608,#11609,#11610));
#3166=EDGE_LOOP('',(#11611,#11612,#11613,#11614));
#3167=EDGE_LOOP('',(#11615,#11616,#11617,#11618));
#3168=EDGE_LOOP('',(#11619,#11620,#11621,#11622));
#3169=EDGE_LOOP('',(#11623,#11624,#11625));
#3170=EDGE_LOOP('',(#11626,#11627,#11628));
#3171=EDGE_LOOP('',(#11629,#11630,#11631,#11632));
#3172=EDGE_LOOP('',(#11633,#11634,#11635,#11636));
#3173=EDGE_LOOP('',(#11637,#11638,#11639,#11640));
#3174=EDGE_LOOP('',(#11641,#11642,#11643,#11644));
#3175=EDGE_LOOP('',(#11645,#11646,#11647));
#3176=EDGE_LOOP('',(#11648,#11649,#11650));
#3177=EDGE_LOOP('',(#11651,#11652,#11653,#11654));
#3178=EDGE_LOOP('',(#11655,#11656,#11657,#11658));
#3179=EDGE_LOOP('',(#11659,#11660,#11661,#11662));
#3180=EDGE_LOOP('',(#11663,#11664,#11665,#11666));
#3181=EDGE_LOOP('',(#11667,#11668,#11669));
#3182=EDGE_LOOP('',(#11670,#11671,#11672,#11673));
#3183=EDGE_LOOP('',(#11674,#11675,#11676,#11677));
#3184=EDGE_LOOP('',(#11678,#11679,#11680,#11681));
#3185=EDGE_LOOP('',(#11682,#11683,#11684,#11685));
#3186=EDGE_LOOP('',(#11686,#11687,#11688,#11689));
#3187=EDGE_LOOP('',(#11690,#11691,#11692));
#3188=EDGE_LOOP('',(#11693,#11694,#11695));
#3189=EDGE_LOOP('',(#11696,#11697,#11698,#11699));
#3190=EDGE_LOOP('',(#11700,#11701,#11702,#11703));
#3191=EDGE_LOOP('',(#11704,#11705,#11706,#11707));
#3192=EDGE_LOOP('',(#11708,#11709,#11710,#11711));
#3193=EDGE_LOOP('',(#11712,#11713,#11714));
#3194=EDGE_LOOP('',(#11715,#11716,#11717));
#3195=EDGE_LOOP('',(#11718,#11719,#11720,#11721));
#3196=EDGE_LOOP('',(#11722,#11723,#11724,#11725));
#3197=EDGE_LOOP('',(#11726,#11727,#11728,#11729));
#3198=EDGE_LOOP('',(#11730,#11731,#11732,#11733));
#3199=EDGE_LOOP('',(#11734,#11735,#11736));
#3200=EDGE_LOOP('',(#11737,#11738,#11739));
#3201=EDGE_LOOP('',(#11740,#11741,#11742,#11743));
#3202=EDGE_LOOP('',(#11744,#11745,#11746,#11747));
#3203=EDGE_LOOP('',(#11748,#11749,#11750,#11751));
#3204=EDGE_LOOP('',(#11752,#11753,#11754,#11755));
#3205=EDGE_LOOP('',(#11756,#11757,#11758));
#3206=EDGE_LOOP('',(#11759,#11760,#11761));
#3207=EDGE_LOOP('',(#11762,#11763,#11764,#11765));
#3208=EDGE_LOOP('',(#11766,#11767,#11768,#11769));
#3209=EDGE_LOOP('',(#11770,#11771,#11772,#11773));
#3210=EDGE_LOOP('',(#11774,#11775,#11776,#11777));
#3211=EDGE_LOOP('',(#11778,#11779,#11780));
#3212=EDGE_LOOP('',(#11781,#11782,#11783));
#3213=EDGE_LOOP('',(#11784,#11785,#11786,#11787));
#3214=EDGE_LOOP('',(#11788,#11789,#11790,#11791));
#3215=EDGE_LOOP('',(#11792,#11793,#11794,#11795));
#3216=EDGE_LOOP('',(#11796,#11797,#11798,#11799));
#3217=EDGE_LOOP('',(#11800,#11801,#11802));
#3218=EDGE_LOOP('',(#11803,#11804,#11805));
#3219=EDGE_LOOP('',(#11806,#11807,#11808,#11809));
#3220=EDGE_LOOP('',(#11810,#11811,#11812,#11813));
#3221=EDGE_LOOP('',(#11814,#11815,#11816,#11817));
#3222=EDGE_LOOP('',(#11818,#11819,#11820,#11821));
#3223=EDGE_LOOP('',(#11822,#11823,#11824));
#3224=EDGE_LOOP('',(#11825,#11826,#11827));
#3225=EDGE_LOOP('',(#11828,#11829,#11830,#11831));
#3226=EDGE_LOOP('',(#11832,#11833,#11834,#11835));
#3227=EDGE_LOOP('',(#11836,#11837,#11838,#11839));
#3228=EDGE_LOOP('',(#11840,#11841,#11842,#11843));
#3229=EDGE_LOOP('',(#11844,#11845,#11846));
#3230=EDGE_LOOP('',(#11847,#11848,#11849));
#3231=EDGE_LOOP('',(#11850,#11851,#11852,#11853));
#3232=EDGE_LOOP('',(#11854,#11855,#11856,#11857));
#3233=EDGE_LOOP('',(#11858,#11859,#11860,#11861));
#3234=EDGE_LOOP('',(#11862,#11863,#11864,#11865));
#3235=EDGE_LOOP('',(#11866,#11867,#11868));
#3236=EDGE_LOOP('',(#11869,#11870,#11871));
#3237=EDGE_LOOP('',(#11872,#11873,#11874,#11875));
#3238=EDGE_LOOP('',(#11876,#11877,#11878,#11879));
#3239=EDGE_LOOP('',(#11880));
#3240=EDGE_LOOP('',(#11881,#11882,#11883,#11884,#11885,#11886));
#3241=EDGE_LOOP('',(#11887,#11888));
#3242=EDGE_LOOP('',(#11889,#11890));
#3243=EDGE_LOOP('',(#11891,#11892));
#3244=EDGE_LOOP('',(#11893,#11894));
#3245=EDGE_LOOP('',(#11895,#11896));
#3246=EDGE_LOOP('',(#11897,#11898));
#3247=EDGE_LOOP('',(#11899,#11900,#11901,#11902,#11903,#11904,#11905,#11906));
#3248=EDGE_LOOP('',(#11907,#11908,#11909,#11910));
#3249=EDGE_LOOP('',(#11911,#11912,#11913,#11914));
#3250=EDGE_LOOP('',(#11915,#11916,#11917,#11918));
#3251=EDGE_LOOP('',(#11919,#11920,#11921,#11922));
#3252=EDGE_LOOP('',(#11923,#11924,#11925,#11926));
#3253=EDGE_LOOP('',(#11927,#11928,#11929,#11930));
#3254=EDGE_LOOP('',(#11931,#11932,#11933,#11934));
#3255=EDGE_LOOP('',(#11935,#11936,#11937,#11938,#11939,#11940));
#3256=EDGE_LOOP('',(#11941,#11942,#11943,#11944,#11945));
#3257=EDGE_LOOP('',(#11946,#11947,#11948,#11949,#11950,#11951));
#3258=EDGE_LOOP('',(#11952,#11953,#11954,#11955,#11956));
#3259=EDGE_LOOP('',(#11957,#11958,#11959,#11960,#11961));
#3260=EDGE_LOOP('',(#11962,#11963,#11964,#11965,#11966));
#3261=EDGE_LOOP('',(#11967,#11968,#11969,#11970,#11971));
#3262=EDGE_LOOP('',(#11972,#11973,#11974,#11975,#11976));
#3263=EDGE_LOOP('',(#11977,#11978,#11979,#11980,#11981));
#3264=EDGE_LOOP('',(#11982,#11983,#11984,#11985,#11986,#11987));
#3265=EDGE_LOOP('',(#11988,#11989,#11990,#11991,#11992));
#3266=EDGE_LOOP('',(#11993,#11994,#11995,#11996,#11997));
#3267=EDGE_LOOP('',(#11998,#11999,#12000,#12001));
#3268=EDGE_LOOP('',(#12002,#12003,#12004,#12005,#12006,#12007,#12008,#12009,
#12010,#12011,#12012,#12013,#12014,#12015,#12016,#12017,#12018,#12019,#12020,
#12021,#12022,#12023,#12024,#12025,#12026,#12027,#12028,#12029,#12030,#12031,
#12032,#12033,#12034,#12035));
#3269=EDGE_LOOP('',(#12036,#12037,#12038,#12039,#12040));
#3270=EDGE_LOOP('',(#12041,#12042,#12043,#12044,#12045,#12046));
#3271=EDGE_LOOP('',(#12047,#12048,#12049,#12050,#12051,#12052,#12053,#12054,
#12055,#12056,#12057,#12058,#12059,#12060,#12061,#12062,#12063,#12064,#12065,
#12066,#12067,#12068,#12069,#12070,#12071,#12072,#12073,#12074,#12075,#12076,
#12077,#12078,#12079,#12080,#12081,#12082,#12083,#12084,#12085,#12086,#12087,
#12088,#12089));
#3272=EDGE_LOOP('',(#12090,#12091,#12092,#12093,#12094));
#3273=EDGE_LOOP('',(#12095,#12096,#12097,#12098,#12099,#12100,#12101,#12102,
#12103,#12104,#12105,#12106,#12107,#12108,#12109,#12110,#12111,#12112,#12113,
#12114,#12115,#12116,#12117,#12118,#12119,#12120,#12121,#12122,#12123,#12124,
#12125,#12126,#12127,#12128,#12129,#12130,#12131,#12132,#12133,#12134,#12135,
#12136));
#3274=EDGE_LOOP('',(#12137,#12138,#12139,#12140,#12141,#12142,#12143));
#3275=EDGE_LOOP('',(#12144));
#3276=EDGE_LOOP('',(#12145));
#3277=EDGE_LOOP('',(#12146,#12147,#12148,#12149,#12150,#12151,#12152));
#3278=EDGE_LOOP('',(#12153));
#3279=EDGE_LOOP('',(#12154,#12155,#12156,#12157));
#3280=EDGE_LOOP('',(#12158,#12159,#12160,#12161));
#3281=EDGE_LOOP('',(#12162,#12163,#12164));
#3282=EDGE_LOOP('',(#12165,#12166,#12167,#12168,#12169,#12170,#12171,#12172,
#12173,#12174,#12175,#12176,#12177,#12178,#12179,#12180,#12181,#12182,#12183,
#12184,#12185,#12186,#12187,#12188,#12189,#12190,#12191,#12192,#12193,#12194,
#12195,#12196,#12197,#12198,#12199,#12200,#12201,#12202,#12203,#12204,#12205,
#12206,#12207,#12208,#12209,#12210,#12211,#12212,#12213,#12214,#12215,#12216,
#12217,#12218,#12219,#12220,#12221,#12222,#12223,#12224,#12225,#12226,#12227,
#12228,#12229,#12230,#12231,#12232,#12233,#12234,#12235,#12236,#12237,#12238,
#12239,#12240,#12241,#12242,#12243,#12244,#12245,#12246,#12247,#12248,#12249,
#12250,#12251,#12252,#12253,#12254,#12255,#12256,#12257,#12258,#12259,#12260,
#12261,#12262,#12263,#12264,#12265,#12266,#12267,#12268,#12269,#12270,#12271,
#12272,#12273,#12274,#12275));
#3283=EDGE_LOOP('',(#12276,#12277,#12278,#12279));
#3284=EDGE_LOOP('',(#12280,#12281,#12282,#12283));
#3285=EDGE_LOOP('',(#12284,#12285,#12286));
#3286=EDGE_LOOP('',(#12287,#12288,#12289,#12290));
#3287=EDGE_LOOP('',(#12291,#12292,#12293,#12294));
#3288=EDGE_LOOP('',(#12295,#12296,#12297));
#3289=EDGE_LOOP('',(#12298,#12299,#12300,#12301));
#3290=EDGE_LOOP('',(#12302,#12303,#12304,#12305));
#3291=EDGE_LOOP('',(#12306,#12307,#12308));
#3292=EDGE_LOOP('',(#12309,#12310,#12311,#12312));
#3293=EDGE_LOOP('',(#12313,#12314,#12315,#12316));
#3294=EDGE_LOOP('',(#12317,#12318,#12319));
#3295=EDGE_LOOP('',(#12320,#12321,#12322,#12323));
#3296=EDGE_LOOP('',(#12324,#12325,#12326,#12327));
#3297=EDGE_LOOP('',(#12328,#12329,#12330));
#3298=EDGE_LOOP('',(#12331,#12332,#12333,#12334));
#3299=EDGE_LOOP('',(#12335,#12336,#12337,#12338));
#3300=EDGE_LOOP('',(#12339,#12340,#12341));
#3301=EDGE_LOOP('',(#12342,#12343,#12344,#12345));
#3302=EDGE_LOOP('',(#12346,#12347,#12348,#12349));
#3303=EDGE_LOOP('',(#12350,#12351,#12352));
#3304=EDGE_LOOP('',(#12353,#12354,#12355,#12356));
#3305=EDGE_LOOP('',(#12357,#12358,#12359,#12360));
#3306=EDGE_LOOP('',(#12361,#12362,#12363));
#3307=EDGE_LOOP('',(#12364,#12365,#12366,#12367));
#3308=EDGE_LOOP('',(#12368,#12369,#12370,#12371));
#3309=EDGE_LOOP('',(#12372,#12373,#12374));
#3310=EDGE_LOOP('',(#12375,#12376,#12377,#12378));
#3311=EDGE_LOOP('',(#12379,#12380,#12381,#12382));
#3312=EDGE_LOOP('',(#12383,#12384,#12385));
#3313=EDGE_LOOP('',(#12386,#12387,#12388,#12389));
#3314=EDGE_LOOP('',(#12390,#12391,#12392,#12393));
#3315=EDGE_LOOP('',(#12394,#12395,#12396));
#3316=EDGE_LOOP('',(#12397,#12398,#12399,#12400));
#3317=EDGE_LOOP('',(#12401,#12402,#12403,#12404));
#3318=EDGE_LOOP('',(#12405,#12406,#12407));
#3319=EDGE_LOOP('',(#12408,#12409,#12410,#12411));
#3320=EDGE_LOOP('',(#12412,#12413,#12414,#12415));
#3321=EDGE_LOOP('',(#12416,#12417,#12418));
#3322=EDGE_LOOP('',(#12419,#12420,#12421,#12422));
#3323=EDGE_LOOP('',(#12423,#12424,#12425,#12426));
#3324=EDGE_LOOP('',(#12427,#12428,#12429));
#3325=EDGE_LOOP('',(#12430,#12431,#12432,#12433));
#3326=EDGE_LOOP('',(#12434,#12435,#12436,#12437));
#3327=EDGE_LOOP('',(#12438,#12439,#12440));
#3328=EDGE_LOOP('',(#12441,#12442,#12443,#12444));
#3329=EDGE_LOOP('',(#12445,#12446,#12447,#12448));
#3330=EDGE_LOOP('',(#12449,#12450,#12451));
#3331=EDGE_LOOP('',(#12452,#12453,#12454,#12455));
#3332=EDGE_LOOP('',(#12456,#12457,#12458,#12459));
#3333=EDGE_LOOP('',(#12460,#12461,#12462,#12463));
#3334=EDGE_LOOP('',(#12464,#12465,#12466,#12467));
#3335=EDGE_LOOP('',(#12468,#12469,#12470,#12471));
#3336=EDGE_LOOP('',(#12472,#12473,#12474));
#3337=EDGE_LOOP('',(#12475,#12476,#12477,#12478));
#3338=EDGE_LOOP('',(#12479,#12480,#12481,#12482));
#3339=EDGE_LOOP('',(#12483,#12484,#12485));
#3340=EDGE_LOOP('',(#12486,#12487,#12488,#12489));
#3341=EDGE_LOOP('',(#12490,#12491,#12492,#12493));
#3342=EDGE_LOOP('',(#12494,#12495,#12496));
#3343=EDGE_LOOP('',(#12497,#12498,#12499,#12500));
#3344=EDGE_LOOP('',(#12501,#12502,#12503,#12504));
#3345=EDGE_LOOP('',(#12505,#12506,#12507));
#3346=EDGE_LOOP('',(#12508,#12509,#12510,#12511));
#3347=EDGE_LOOP('',(#12512,#12513,#12514,#12515));
#3348=EDGE_LOOP('',(#12516,#12517,#12518));
#3349=EDGE_LOOP('',(#12519,#12520,#12521,#12522));
#3350=EDGE_LOOP('',(#12523,#12524,#12525,#12526));
#3351=EDGE_LOOP('',(#12527,#12528,#12529));
#3352=EDGE_LOOP('',(#12530,#12531,#12532,#12533));
#3353=EDGE_LOOP('',(#12534,#12535,#12536,#12537));
#3354=EDGE_LOOP('',(#12538,#12539,#12540));
#3355=EDGE_LOOP('',(#12541,#12542,#12543,#12544));
#3356=EDGE_LOOP('',(#12545,#12546,#12547,#12548));
#3357=EDGE_LOOP('',(#12549,#12550,#12551));
#3358=EDGE_LOOP('',(#12552,#12553,#12554,#12555));
#3359=EDGE_LOOP('',(#12556,#12557,#12558,#12559));
#3360=EDGE_LOOP('',(#12560,#12561,#12562));
#3361=EDGE_LOOP('',(#12563,#12564,#12565,#12566));
#3362=EDGE_LOOP('',(#12567,#12568,#12569,#12570));
#3363=EDGE_LOOP('',(#12571,#12572,#12573));
#3364=EDGE_LOOP('',(#12574,#12575,#12576,#12577));
#3365=EDGE_LOOP('',(#12578,#12579,#12580,#12581));
#3366=EDGE_LOOP('',(#12582,#12583,#12584));
#3367=EDGE_LOOP('',(#12585,#12586,#12587,#12588));
#3368=EDGE_LOOP('',(#12589,#12590,#12591,#12592));
#3369=EDGE_LOOP('',(#12593,#12594,#12595));
#3370=EDGE_LOOP('',(#12596,#12597,#12598,#12599));
#3371=EDGE_LOOP('',(#12600,#12601,#12602,#12603));
#3372=EDGE_LOOP('',(#12604,#12605,#12606));
#3373=EDGE_LOOP('',(#12607,#12608,#12609,#12610));
#3374=EDGE_LOOP('',(#12611,#12612,#12613,#12614));
#3375=EDGE_LOOP('',(#12615,#12616,#12617));
#3376=EDGE_LOOP('',(#12618,#12619,#12620,#12621));
#3377=EDGE_LOOP('',(#12622,#12623,#12624,#12625));
#3378=EDGE_LOOP('',(#12626,#12627,#12628));
#3379=EDGE_LOOP('',(#12629,#12630,#12631,#12632));
#3380=EDGE_LOOP('',(#12633,#12634,#12635,#12636));
#3381=EDGE_LOOP('',(#12637,#12638,#12639));
#3382=EDGE_LOOP('',(#12640,#12641,#12642,#12643));
#3383=EDGE_LOOP('',(#12644,#12645,#12646,#12647));
#3384=EDGE_LOOP('',(#12648,#12649,#12650));
#3385=EDGE_LOOP('',(#12651,#12652,#12653,#12654));
#3386=EDGE_LOOP('',(#12655,#12656,#12657,#12658));
#3387=EDGE_LOOP('',(#12659,#12660,#12661));
#3388=EDGE_LOOP('',(#12662,#12663,#12664,#12665,#12666,#12667,#12668,#12669,
#12670,#12671,#12672,#12673,#12674,#12675,#12676,#12677,#12678,#12679,#12680,
#12681,#12682,#12683,#12684,#12685,#12686,#12687,#12688,#12689,#12690,#12691,
#12692,#12693,#12694,#12695,#12696,#12697,#12698,#12699,#12700,#12701,#12702,
#12703,#12704,#12705,#12706,#12707,#12708,#12709,#12710,#12711,#12712,#12713,
#12714,#12715,#12716,#12717,#12718,#12719,#12720,#12721,#12722,#12723,#12724,
#12725,#12726,#12727,#12728,#12729,#12730,#12731,#12732,#12733,#12734,#12735,
#12736,#12737,#12738,#12739,#12740,#12741,#12742,#12743,#12744,#12745,#12746,
#12747,#12748,#12749,#12750,#12751,#12752,#12753,#12754,#12755,#12756,#12757,
#12758,#12759,#12760,#12761,#12762,#12763,#12764,#12765,#12766,#12767,#12768,
#12769,#12770,#12771,#12772,#12773,#12774,#12775,#12776,#12777,#12778,#12779,
#12780,#12781,#12782,#12783,#12784,#12785,#12786,#12787,#12788,#12789,#12790,
#12791,#12792,#12793,#12794,#12795,#12796,#12797,#12798,#12799,#12800,#12801,
#12802,#12803,#12804,#12805,#12806,#12807,#12808,#12809));
#3389=EDGE_LOOP('',(#12810));
#3390=EDGE_LOOP('',(#12811,#12812,#12813,#12814,#12815,#12816));
#3391=EDGE_LOOP('',(#12817,#12818));
#3392=EDGE_LOOP('',(#12819,#12820));
#3393=EDGE_LOOP('',(#12821,#12822));
#3394=EDGE_LOOP('',(#12823,#12824));
#3395=EDGE_LOOP('',(#12825,#12826));
#3396=EDGE_LOOP('',(#12827,#12828));
#3397=EDGE_LOOP('',(#12829,#12830,#12831,#12832,#12833,#12834,#12835,#12836));
#3398=EDGE_LOOP('',(#12837,#12838,#12839,#12840));
#3399=EDGE_LOOP('',(#12841,#12842,#12843,#12844));
#3400=EDGE_LOOP('',(#12845,#12846,#12847,#12848));
#3401=EDGE_LOOP('',(#12849,#12850,#12851,#12852));
#3402=EDGE_LOOP('',(#12853,#12854,#12855,#12856));
#3403=EDGE_LOOP('',(#12857,#12858,#12859,#12860));
#3404=CIRCLE('',#13760,4.25);
#3405=CIRCLE('',#13762,2.6);
#3406=CIRCLE('',#13766,4.25);
#3407=CIRCLE('',#13768,2.6);
#3408=CIRCLE('',#13772,4.25);
#3409=CIRCLE('',#13774,2.6);
#3410=CIRCLE('',#13778,4.25);
#3411=CIRCLE('',#13780,2.6);
#3412=CIRCLE('',#13784,4.25);
#3413=CIRCLE('',#13786,2.6);
#3414=CIRCLE('',#13790,4.25);
#3415=CIRCLE('',#13792,2.6);
#3416=CIRCLE('',#13795,5.35);
#3417=CIRCLE('',#13796,5.65);
#3418=CIRCLE('',#13798,5.65);
#3419=CIRCLE('',#13799,5.65);
#3420=CIRCLE('',#13800,5.65);
#3421=CIRCLE('',#13802,5.35);
#3422=CIRCLE('',#13804,5.35);
#3423=CIRCLE('',#13806,5.35);
#3424=CIRCLE('',#13808,5.35);
#3425=CIRCLE('',#13810,5.35);
#3426=CIRCLE('',#13812,5.35);
#3427=CIRCLE('',#13814,5.35);
#3428=CIRCLE('',#13816,3.55600000000001);
#3429=CIRCLE('',#13818,3.556);
#3430=CIRCLE('',#13820,3.556);
#3431=CIRCLE('',#13822,3.55600000000001);
#3432=CIRCLE('',#13824,3.55600000000001);
#3433=CIRCLE('',#13826,3.556);
#3434=CIRCLE('',#13828,3.556);
#3435=CIRCLE('',#13830,3.55600000000001);
#3436=CIRCLE('',#13834,6.35);
#3437=CIRCLE('',#13835,6.35);
#3438=CIRCLE('',#13842,6.35);
#3439=CIRCLE('',#13848,6.35);
#3440=CIRCLE('',#13856,4.55000000000001);
#3441=CIRCLE('',#13857,4.25000000000001);
#3442=CIRCLE('',#13859,4.55);
#3443=CIRCLE('',#13860,4.55);
#3444=CIRCLE('',#13861,4.55);
#3445=CIRCLE('',#13862,3.625);
#3446=CIRCLE('',#13863,4.55000000000001);
#3447=CIRCLE('',#13864,3.62499999999999);
#3448=CIRCLE('',#13865,3.62499999999999);
#3449=CIRCLE('',#13866,3.62499999999999);
#3450=CIRCLE('',#13867,3.625);
#3451=CIRCLE('',#13868,4.55);
#3452=CIRCLE('',#13869,3.625);
#3453=CIRCLE('',#13870,4.55);
#3454=CIRCLE('',#13871,3.625);
#3455=CIRCLE('',#13872,3.62499999999999);
#3456=CIRCLE('',#13873,4.55);
#3457=CIRCLE('',#13875,4.25000000000001);
#3458=CIRCLE('',#13877,4.25000000000001);
#3459=CIRCLE('',#13879,4.25);
#3460=CIRCLE('',#13881,4.25);
#3461=CIRCLE('',#13883,4.25);
#3462=CIRCLE('',#13885,4.25);
#3463=CIRCLE('',#13887,4.25);
#3464=CIRCLE('',#13889,4.25);
#3465=CIRCLE('',#13891,4.25000000000001);
#3466=CIRCLE('',#13893,4.25000000000001);
#3467=CIRCLE('',#13895,4.25000000000001);
#3468=CIRCLE('',#13897,4.25000000000001);
#3469=CIRCLE('',#13899,3.225);
#3470=CIRCLE('',#13900,2.6);
#3471=CIRCLE('',#13902,2.6);
#3472=CIRCLE('',#13904,2.6);
#3473=CIRCLE('',#13906,4.25);
#3474=CIRCLE('',#13908,3.225);
#3475=CIRCLE('',#13909,2.6);
#3476=CIRCLE('',#13911,2.6);
#3477=CIRCLE('',#13913,4.25);
#3478=CIRCLE('',#13915,3.225);
#3479=CIRCLE('',#13916,2.6);
#3480=CIRCLE('',#13918,2.6);
#3481=CIRCLE('',#13920,4.25000000000001);
#3482=CIRCLE('',#13922,3.225);
#3483=CIRCLE('',#13923,2.6);
#3484=CIRCLE('',#13925,3.225);
#3485=CIRCLE('',#13926,3.225);
#3486=CIRCLE('',#13928,3.225);
#3487=CIRCLE('',#13929,3.225);
#3488=CIRCLE('',#13931,3.225);
#3489=CIRCLE('',#13932,3.225);
#3490=CIRCLE('',#13934,3.225);
#3491=CIRCLE('',#13935,3.225);
#3492=CIRCLE('',#13937,2.6);
#3493=CIRCLE('',#13939,2.6);
#3494=CIRCLE('',#13941,2.6);
#3495=CIRCLE('',#13943,2.6);
#3496=CIRCLE('',#13945,2.6);
#3497=CIRCLE('',#13947,2.6);
#3498=CIRCLE('',#13949,2.6);
#3499=CIRCLE('',#13951,2.6);
#3500=CIRCLE('',#13953,3.225);
#3501=CIRCLE('',#13955,3.225);
#3502=CIRCLE('',#13957,3.225);
#3503=CIRCLE('',#13959,3.225);
#3504=CIRCLE('',#13961,3.225);
#3505=CIRCLE('',#13963,3.225);
#3506=CIRCLE('',#13965,3.225);
#3507=CIRCLE('',#13967,3.225);
#3508=CIRCLE('',#13969,3.225);
#3509=CIRCLE('',#13971,3.225);
#3510=CIRCLE('',#13973,3.225);
#3511=CIRCLE('',#13975,3.225);
#3512=CIRCLE('',#13995,2.464);
#3513=CIRCLE('',#13998,2.464);
#3514=CIRCLE('',#14001,2.464);
#3515=CIRCLE('',#14004,5.85);
#3516=CIRCLE('',#14006,6.35);
#3517=CIRCLE('',#14008,6.35);
#3518=CIRCLE('',#14010,5.85);
#3519=CIRCLE('',#14014,2.464);
#3520=CIRCLE('',#14015,2.76400000000001);
#3521=CIRCLE('',#14017,2.76400000000001);
#3522=CIRCLE('',#14019,2.464);
#3523=CIRCLE('',#14020,2.464);
#3524=CIRCLE('',#14022,2.464);
#3525=CIRCLE('',#14024,2.464);
#3526=CIRCLE('',#14025,2.464);
#3527=CIRCLE('',#14028,11.1);
#3528=CIRCLE('',#14029,11.1);
#3529=CIRCLE('',#14032,11.5);
#3530=CIRCLE('',#14036,11.5);
#3531=CIRCLE('',#14049,10.7);
#3532=CIRCLE('',#14050,11.1);
#3533=CIRCLE('',#14052,8.75);
#3534=CIRCLE('',#14054,8.75);
#3535=CIRCLE('',#14056,10.7);
#3536=CIRCLE('',#14058,11.1);
#3537=CIRCLE('',#14063,8.75);
#3538=CIRCLE('',#14064,6.45);
#3539=CIRCLE('',#14067,8.75);
#3540=CIRCLE('',#14068,6.45);
#3541=CIRCLE('',#14071,8.75);
#3542=CIRCLE('',#14072,6.45);
#3543=CIRCLE('',#14075,8.75);
#3544=CIRCLE('',#14076,6.45);
#3545=CIRCLE('',#14079,8.75);
#3546=CIRCLE('',#14080,6.45);
#3547=CIRCLE('',#14083,8.75);
#3548=CIRCLE('',#14084,6.45);
#3549=CIRCLE('',#14087,8.75);
#3550=CIRCLE('',#14088,6.45);
#3551=CIRCLE('',#14091,8.75);
#3552=CIRCLE('',#14092,6.45);
#3553=CIRCLE('',#14095,8.75);
#3554=CIRCLE('',#14096,6.45);
#3555=CIRCLE('',#14099,8.75);
#3556=CIRCLE('',#14100,6.45);
#3557=CIRCLE('',#14104,6.45);
#3558=CIRCLE('',#14105,8.75);
#3559=CIRCLE('',#14107,8.75);
#3560=CIRCLE('',#14109,6.45);
#3561=CIRCLE('',#14113,1.190625);
#3562=CIRCLE('',#14116,1.92913);
#3563=CIRCLE('',#14136,2.36347);
#3564=CIRCLE('',#14137,2.36347);
#3565=CIRCLE('',#14138,2.36347);
#3566=CIRCLE('',#14140,1.92913);
#3567=CIRCLE('',#14142,2.36347);
#3568=CIRCLE('',#14144,2.36347);
#3569=CIRCLE('',#14145,2.36347);
#3570=CIRCLE('',#14147,2.56347);
#3571=CIRCLE('',#14148,0.2);
#3572=CIRCLE('',#14150,3.9624);
#3573=CIRCLE('',#14152,1.96347);
#3574=CIRCLE('',#14157,3.9624);
#3575=CIRCLE('',#14159,3.9624);
#3576=CIRCLE('',#14160,3.9624);
#3577=CIRCLE('',#14161,3.9624);
#3578=CIRCLE('',#14162,3.9624);
#3579=CIRCLE('',#14163,3.9624);
#3580=CIRCLE('',#14164,3.9624);
#3581=CIRCLE('',#14165,3.9624);
#3582=CIRCLE('',#14166,3.9624);
#3583=CIRCLE('',#14167,3.9624);
#3584=CIRCLE('',#14168,3.9624);
#3585=CIRCLE('',#14169,3.9624);
#3586=CIRCLE('',#14170,3.9624);
#3587=CIRCLE('',#14171,3.9624);
#3588=CIRCLE('',#14172,3.9624);
#3589=CIRCLE('',#14173,3.9624);
#3590=CIRCLE('',#14174,3.9624);
#3591=CIRCLE('',#14175,3.9624);
#3592=CIRCLE('',#14176,3.9624);
#3593=CIRCLE('',#14177,3.9624);
#3594=CIRCLE('',#14178,3.9624);
#3595=CIRCLE('',#14179,3.9624);
#3596=CIRCLE('',#14180,3.9624);
#3597=CIRCLE('',#14181,3.9624);
#3598=CIRCLE('',#14182,3.9624);
#3599=CIRCLE('',#14183,3.9624);
#3600=CIRCLE('',#14184,3.9624);
#3601=CIRCLE('',#14185,3.9624);
#3602=CIRCLE('',#14186,3.9624);
#3603=CIRCLE('',#14187,3.9624);
#3604=CIRCLE('',#14188,3.9624);
#3605=CIRCLE('',#14189,3.9624);
#3606=CIRCLE('',#14190,3.9624);
#3607=CIRCLE('',#14191,3.9624);
#3608=CIRCLE('',#14192,3.9624);
#3609=CIRCLE('',#14193,3.9624);
#3610=CIRCLE('',#14194,3.9624);
#3611=CIRCLE('',#14195,3.5624);
#3612=CIRCLE('',#14199,3.9624);
#3613=CIRCLE('',#14203,3.9624);
#3614=CIRCLE('',#14207,3.9624);
#3615=CIRCLE('',#14211,3.9624);
#3616=CIRCLE('',#14215,3.9624);
#3617=CIRCLE('',#14219,3.9624);
#3618=CIRCLE('',#14223,3.9624);
#3619=CIRCLE('',#14227,3.9624);
#3620=CIRCLE('',#14231,3.9624);
#3621=CIRCLE('',#14235,3.9624);
#3622=CIRCLE('',#14239,3.9624);
#3623=CIRCLE('',#14243,3.9624);
#3624=CIRCLE('',#14247,3.9624);
#3625=CIRCLE('',#14251,3.9624);
#3626=CIRCLE('',#14255,3.9624);
#3627=CIRCLE('',#14259,3.9624);
#3628=CIRCLE('',#14263,3.9624);
#3629=CIRCLE('',#14264,3.9624);
#3630=CIRCLE('',#14268,3.9624);
#3631=CIRCLE('',#14272,3.9624);
#3632=CIRCLE('',#14276,3.9624);
#3633=CIRCLE('',#14280,3.9624);
#3634=CIRCLE('',#14284,3.9624);
#3635=CIRCLE('',#14288,3.9624);
#3636=CIRCLE('',#14292,3.9624);
#3637=CIRCLE('',#14296,3.9624);
#3638=CIRCLE('',#14300,3.9624);
#3639=CIRCLE('',#14304,3.9624);
#3640=CIRCLE('',#14308,3.9624);
#3641=CIRCLE('',#14312,3.9624);
#3642=CIRCLE('',#14316,3.9624);
#3643=CIRCLE('',#14320,3.9624);
#3644=CIRCLE('',#14324,3.9624);
#3645=CIRCLE('',#14328,3.9624);
#3646=CIRCLE('',#14332,3.9624);
#3647=CIRCLE('',#14336,3.9624);
#3648=CIRCLE('',#14340,2.29135888084632);
#3649=CIRCLE('',#14342,2.29135888084632);
#3650=CIRCLE('',#14344,2.29135888084632);
#3651=CIRCLE('',#14346,2.29135888084632);
#3652=CIRCLE('',#14348,2.29135888084632);
#3653=CIRCLE('',#14350,2.29135888084632);
#3654=CIRCLE('',#14360,1.92913);
#3655=CIRCLE('',#14388,2.36347);
#3656=CIRCLE('',#14389,2.36347);
#3657=CIRCLE('',#14390,2.36347);
#3658=CIRCLE('',#14392,1.92913);
#3659=CIRCLE('',#14394,2.36347);
#3660=CIRCLE('',#14396,2.36347);
#3661=CIRCLE('',#14397,2.36347);
#3662=CIRCLE('',#14399,2.56347);
#3663=CIRCLE('',#14400,0.2);
#3664=CIRCLE('',#14402,3.9624);
#3665=CIRCLE('',#14404,1.96347);
#3666=CIRCLE('',#14409,3.9624);
#3667=CIRCLE('',#14411,3.9624);
#3668=CIRCLE('',#14412,3.9624);
#3669=CIRCLE('',#14413,3.9624);
#3670=CIRCLE('',#14414,3.9624);
#3671=CIRCLE('',#14415,3.9624);
#3672=CIRCLE('',#14416,3.9624);
#3673=CIRCLE('',#14417,3.9624);
#3674=CIRCLE('',#14418,3.9624);
#3675=CIRCLE('',#14419,3.9624);
#3676=CIRCLE('',#14420,3.9624);
#3677=CIRCLE('',#14421,3.9624);
#3678=CIRCLE('',#14422,3.9624);
#3679=CIRCLE('',#14423,3.9624);
#3680=CIRCLE('',#14424,3.9624);
#3681=CIRCLE('',#14425,3.9624);
#3682=CIRCLE('',#14426,3.9624);
#3683=CIRCLE('',#14427,3.9624);
#3684=CIRCLE('',#14428,3.9624);
#3685=CIRCLE('',#14429,3.9624);
#3686=CIRCLE('',#14430,3.9624);
#3687=CIRCLE('',#14431,3.9624);
#3688=CIRCLE('',#14432,3.9624);
#3689=CIRCLE('',#14433,3.9624);
#3690=CIRCLE('',#14434,3.9624);
#3691=CIRCLE('',#14435,3.9624);
#3692=CIRCLE('',#14436,3.9624);
#3693=CIRCLE('',#14437,3.9624);
#3694=CIRCLE('',#14438,3.9624);
#3695=CIRCLE('',#14439,3.9624);
#3696=CIRCLE('',#14440,3.9624);
#3697=CIRCLE('',#14441,3.9624);
#3698=CIRCLE('',#14442,3.9624);
#3699=CIRCLE('',#14443,3.9624);
#3700=CIRCLE('',#14444,3.9624);
#3701=CIRCLE('',#14445,3.9624);
#3702=CIRCLE('',#14446,3.9624);
#3703=CIRCLE('',#14447,3.5624);
#3704=CIRCLE('',#14449,3.9624);
#3705=CIRCLE('',#14453,3.9624);
#3706=CIRCLE('',#14454,3.9624);
#3707=CIRCLE('',#14455,3.9624);
#3708=CIRCLE('',#14456,3.9624);
#3709=CIRCLE('',#14457,3.9624);
#3710=CIRCLE('',#14458,3.9624);
#3711=CIRCLE('',#14459,3.9624);
#3712=CIRCLE('',#14460,3.9624);
#3713=CIRCLE('',#14461,3.9624);
#3714=CIRCLE('',#14462,3.9624);
#3715=CIRCLE('',#14463,3.9624);
#3716=CIRCLE('',#14464,3.9624);
#3717=CIRCLE('',#14465,3.9624);
#3718=CIRCLE('',#14466,3.9624);
#3719=CIRCLE('',#14467,3.9624);
#3720=CIRCLE('',#14468,3.9624);
#3721=CIRCLE('',#14469,3.9624);
#3722=CIRCLE('',#14470,3.9624);
#3723=CIRCLE('',#14471,3.9624);
#3724=CIRCLE('',#14472,3.9624);
#3725=CIRCLE('',#14473,3.9624);
#3726=CIRCLE('',#14474,3.9624);
#3727=CIRCLE('',#14475,3.9624);
#3728=CIRCLE('',#14476,3.9624);
#3729=CIRCLE('',#14477,3.9624);
#3730=CIRCLE('',#14478,3.9624);
#3731=CIRCLE('',#14479,3.9624);
#3732=CIRCLE('',#14480,3.9624);
#3733=CIRCLE('',#14481,3.9624);
#3734=CIRCLE('',#14482,3.9624);
#3735=CIRCLE('',#14483,3.9624);
#3736=CIRCLE('',#14484,3.9624);
#3737=CIRCLE('',#14485,3.9624);
#3738=CIRCLE('',#14486,3.9624);
#3739=CIRCLE('',#14487,3.9624);
#3740=CIRCLE('',#14592,2.29135888084633);
#3741=CIRCLE('',#14594,2.29135888084633);
#3742=CIRCLE('',#14596,2.29135888084633);
#3743=CIRCLE('',#14598,2.29135888084633);
#3744=CIRCLE('',#14600,2.29135888084633);
#3745=CIRCLE('',#14602,2.29135888084633);
#3746=CIRCLE('',#14612,2.40538);
#3747=CIRCLE('',#14627,3.11023);
#3748=CIRCLE('',#14628,3.11023);
#3749=CIRCLE('',#14630,2.40538);
#3750=CIRCLE('',#14632,3.11023);
#3751=CIRCLE('',#14633,3.11023);
#3752=CIRCLE('',#14635,3.11023);
#3753=CIRCLE('',#14636,3.11023);
#3754=CIRCLE('',#14638,3.31023);
#3755=CIRCLE('',#14639,0.2);
#3756=CIRCLE('',#14641,4.7625);
#3757=CIRCLE('',#14643,2.71023);
#3758=CIRCLE('',#14648,4.7625);
#3759=CIRCLE('',#14650,4.7625);
#3760=CIRCLE('',#14651,4.7625);
#3761=CIRCLE('',#14652,4.7625);
#3762=CIRCLE('',#14653,4.7625);
#3763=CIRCLE('',#14654,4.7625);
#3764=CIRCLE('',#14655,4.7625);
#3765=CIRCLE('',#14656,4.7625);
#3766=CIRCLE('',#14657,4.7625);
#3767=CIRCLE('',#14658,4.7625);
#3768=CIRCLE('',#14659,4.7625);
#3769=CIRCLE('',#14660,4.7625);
#3770=CIRCLE('',#14661,4.7625);
#3771=CIRCLE('',#14662,4.7625);
#3772=CIRCLE('',#14663,4.7625);
#3773=CIRCLE('',#14664,4.7625);
#3774=CIRCLE('',#14665,4.7625);
#3775=CIRCLE('',#14666,4.7625);
#3776=CIRCLE('',#14667,4.7625);
#3777=CIRCLE('',#14668,4.7625);
#3778=CIRCLE('',#14669,4.7625);
#3779=CIRCLE('',#14670,4.7625);
#3780=CIRCLE('',#14671,4.7625);
#3781=CIRCLE('',#14672,4.7625);
#3782=CIRCLE('',#14673,4.7625);
#3783=CIRCLE('',#14674,4.7625);
#3784=CIRCLE('',#14675,4.7625);
#3785=CIRCLE('',#14676,4.7625);
#3786=CIRCLE('',#14677,4.7625);
#3787=CIRCLE('',#14678,4.7625);
#3788=CIRCLE('',#14679,4.7625);
#3789=CIRCLE('',#14680,4.7625);
#3790=CIRCLE('',#14681,4.7625);
#3791=CIRCLE('',#14682,4.7625);
#3792=CIRCLE('',#14683,4.7625);
#3793=CIRCLE('',#14684,4.7625);
#3794=CIRCLE('',#14685,4.7625);
#3795=CIRCLE('',#14686,4.3625);
#3796=CIRCLE('',#14690,4.7625);
#3797=CIRCLE('',#14694,4.7625);
#3798=CIRCLE('',#14698,4.7625);
#3799=CIRCLE('',#14702,4.7625);
#3800=CIRCLE('',#14706,4.7625);
#3801=CIRCLE('',#14710,4.7625);
#3802=CIRCLE('',#14714,4.7625);
#3803=CIRCLE('',#14718,4.7625);
#3804=CIRCLE('',#14722,4.7625);
#3805=CIRCLE('',#14726,4.7625);
#3806=CIRCLE('',#14730,4.7625);
#3807=CIRCLE('',#14734,4.7625);
#3808=CIRCLE('',#14738,4.7625);
#3809=CIRCLE('',#14742,4.7625);
#3810=CIRCLE('',#14746,4.7625);
#3811=CIRCLE('',#14750,4.7625);
#3812=CIRCLE('',#14754,4.7625);
#3813=CIRCLE('',#14755,4.7625);
#3814=CIRCLE('',#14759,4.7625);
#3815=CIRCLE('',#14763,4.7625);
#3816=CIRCLE('',#14767,4.7625);
#3817=CIRCLE('',#14771,4.7625);
#3818=CIRCLE('',#14775,4.7625);
#3819=CIRCLE('',#14779,4.7625);
#3820=CIRCLE('',#14783,4.7625);
#3821=CIRCLE('',#14787,4.7625);
#3822=CIRCLE('',#14791,4.7625);
#3823=CIRCLE('',#14795,4.7625);
#3824=CIRCLE('',#14799,4.7625);
#3825=CIRCLE('',#14803,4.7625);
#3826=CIRCLE('',#14807,4.7625);
#3827=CIRCLE('',#14811,4.7625);
#3828=CIRCLE('',#14815,4.7625);
#3829=CIRCLE('',#14819,4.7625);
#3830=CIRCLE('',#14823,4.7625);
#3831=CIRCLE('',#14827,4.7625);
#3832=CIRCLE('',#14831,2.74963065701559);
#3833=CIRCLE('',#14833,2.74963065701559);
#3834=CIRCLE('',#14835,2.74963065701559);
#3835=CIRCLE('',#14837,2.74963065701559);
#3836=CIRCLE('',#14839,2.74963065701559);
#3837=CIRCLE('',#14841,2.74963065701559);
#3838=LINE('',#18534,#4749);
#3839=LINE('',#18541,#4750);
#3840=LINE('',#18583,#4751);
#3841=LINE('',#18590,#4752);
#3842=LINE('',#18632,#4753);
#3843=LINE('',#18639,#4754);
#3844=LINE('',#18681,#4755);
#3845=LINE('',#18688,#4756);
#3846=LINE('',#18730,#4757);
#3847=LINE('',#18737,#4758);
#3848=LINE('',#18779,#4759);
#3849=LINE('',#18786,#4760);
#3850=LINE('',#18828,#4761);
#3851=LINE('',#18833,#4762);
#3852=LINE('',#18835,#4763);
#3853=LINE('',#18837,#4764);
#3854=LINE('',#18838,#4765);
#3855=LINE('',#18847,#4766);
#3856=LINE('',#18852,#4767);
#3857=LINE('',#18855,#4768);
#3858=LINE('',#18860,#4769);
#3859=LINE('',#18863,#4770);
#3860=LINE('',#18868,#4771);
#3861=LINE('',#18871,#4772);
#3862=LINE('',#18887,#4773);
#3863=LINE('',#18891,#4774);
#3864=LINE('',#18895,#4775);
#3865=LINE('',#18899,#4776);
#3866=LINE('',#18904,#4777);
#3867=LINE('',#18906,#4778);
#3868=LINE('',#18908,#4779);
#3869=LINE('',#18909,#4780);
#3870=LINE('',#18911,#4781);
#3871=LINE('',#18912,#4782);
#3872=LINE('',#18915,#4783);
#3873=LINE('',#18917,#4784);
#3874=LINE('',#18921,#4785);
#3875=LINE('',#18923,#4786);
#3876=LINE('',#18925,#4787);
#3877=LINE('',#18927,#4788);
#3878=LINE('',#18929,#4789);
#3879=LINE('',#18931,#4790);
#3880=LINE('',#18933,#4791);
#3881=LINE('',#18937,#4792);
#3882=LINE('',#18939,#4793);
#3883=LINE('',#18941,#4794);
#3884=LINE('',#18942,#4795);
#3885=LINE('',#18946,#4796);
#3886=LINE('',#18947,#4797);
#3887=LINE('',#18948,#4798);
#3888=LINE('',#18951,#4799);
#3889=LINE('',#18952,#4800);
#3890=LINE('',#18956,#4801);
#3891=LINE('',#18957,#4802);
#3892=LINE('',#18958,#4803);
#3893=LINE('',#18961,#4804);
#3894=LINE('',#18962,#4805);
#3895=LINE('',#18965,#4806);
#3896=LINE('',#18966,#4807);
#3897=LINE('',#18969,#4808);
#3898=LINE('',#18972,#4809);
#3899=LINE('',#18975,#4810);
#3900=LINE('',#18976,#4811);
#3901=LINE('',#18978,#4812);
#3902=LINE('',#18981,#4813);
#3903=LINE('',#18982,#4814);
#3904=LINE('',#18985,#4815);
#3905=LINE('',#18986,#4816);
#3906=LINE('',#18990,#4817);
#3907=LINE('',#18992,#4818);
#3908=LINE('',#18994,#4819);
#3909=LINE('',#18997,#4820);
#3910=LINE('',#18998,#4821);
#3911=LINE('',#19000,#4822);
#3912=LINE('',#19025,#4823);
#3913=LINE('',#19027,#4824);
#3914=LINE('',#19029,#4825);
#3915=LINE('',#19030,#4826);
#3916=LINE('',#19063,#4827);
#3917=LINE('',#19066,#4828);
#3918=LINE('',#19087,#4829);
#3919=LINE('',#19090,#4830);
#3920=LINE('',#19111,#4831);
#3921=LINE('',#19114,#4832);
#3922=LINE('',#19119,#4833);
#3923=LINE('',#19122,#4834);
#3924=LINE('',#19147,#4835);
#3925=LINE('',#19151,#4836);
#3926=LINE('',#19173,#4837);
#3927=LINE('',#19177,#4838);
#3928=LINE('',#19196,#4839);
#3929=LINE('',#19200,#4840);
#3930=LINE('',#19219,#4841);
#3931=LINE('',#19223,#4842);
#3932=LINE('',#19250,#4843);
#3933=LINE('',#19254,#4844);
#3934=LINE('',#19258,#4845);
#3935=LINE('',#19262,#4846);
#3936=LINE('',#19266,#4847);
#3937=LINE('',#19270,#4848);
#3938=LINE('',#19274,#4849);
#3939=LINE('',#19278,#4850);
#3940=LINE('',#19283,#4851);
#3941=LINE('',#19286,#4852);
#3942=LINE('',#19291,#4853);
#3943=LINE('',#19294,#4854);
#3944=LINE('',#19298,#4855);
#3945=LINE('',#19302,#4856);
#3946=LINE('',#19306,#4857);
#3947=LINE('',#19310,#4858);
#3948=LINE('',#19315,#4859);
#3949=LINE('',#19318,#4860);
#3950=LINE('',#19323,#4861);
#3951=LINE('',#19326,#4862);
#3952=LINE('',#19330,#4863);
#3953=LINE('',#19333,#4864);
#3954=LINE('',#19336,#4865);
#3955=LINE('',#19339,#4866);
#3956=LINE('',#19342,#4867);
#3957=LINE('',#19345,#4868);
#3958=LINE('',#19348,#4869);
#3959=LINE('',#19351,#4870);
#3960=LINE('',#19354,#4871);
#3961=LINE('',#19356,#4872);
#3962=LINE('',#19357,#4873);
#3963=LINE('',#19360,#4874);
#3964=LINE('',#19361,#4875);
#3965=LINE('',#19364,#4876);
#3966=LINE('',#19365,#4877);
#3967=LINE('',#19367,#4878);
#3968=LINE('',#19370,#4879);
#3969=LINE('',#19372,#4880);
#3970=LINE('',#19373,#4881);
#3971=LINE('',#19376,#4882);
#3972=LINE('',#19377,#4883);
#3973=LINE('',#19380,#4884);
#3974=LINE('',#19381,#4885);
#3975=LINE('',#19383,#4886);
#3976=LINE('',#19426,#4887);
#3977=LINE('',#19430,#4888);
#3978=LINE('',#19471,#4889);
#3979=LINE('',#19475,#4890);
#3980=LINE('',#19516,#4891);
#3981=LINE('',#19520,#4892);
#3982=LINE('',#19527,#4893);
#3983=LINE('',#19531,#4894);
#3984=LINE('',#19534,#4895);
#3985=LINE('',#19542,#4896);
#3986=LINE('',#19547,#4897);
#3987=LINE('',#19549,#4898);
#3988=LINE('',#19551,#4899);
#3989=LINE('',#19552,#4900);
#3990=LINE('',#19557,#4901);
#3991=LINE('',#19579,#4902);
#3992=LINE('',#19582,#4903);
#3993=LINE('',#19603,#4904);
#3994=LINE('',#19623,#4905);
#3995=LINE('',#19626,#4906);
#3996=LINE('',#19643,#4907);
#3997=LINE('',#19646,#4908);
#3998=LINE('',#19649,#4909);
#3999=LINE('',#19652,#4910);
#4000=LINE('',#19654,#4911);
#4001=LINE('',#19655,#4912);
#4002=LINE('',#19657,#4913);
#4003=LINE('',#19659,#4914);
#4004=LINE('',#19661,#4915);
#4005=LINE('',#19663,#4916);
#4006=LINE('',#19664,#4917);
#4007=LINE('',#19667,#4918);
#4008=LINE('',#19669,#4919);
#4009=LINE('',#19670,#4920);
#4010=LINE('',#19673,#4921);
#4011=LINE('',#19677,#4922);
#4012=LINE('',#19679,#4923);
#4013=LINE('',#19681,#4924);
#4014=LINE('',#19683,#4925);
#4015=LINE('',#19684,#4926);
#4016=LINE('',#19686,#4927);
#4017=LINE('',#19687,#4928);
#4018=LINE('',#19689,#4929);
#4019=LINE('',#19691,#4930);
#4020=LINE('',#19693,#4931);
#4021=LINE('',#19695,#4932);
#4022=LINE('',#19697,#4933);
#4023=LINE('',#19704,#4934);
#4024=LINE('',#19706,#4935);
#4025=LINE('',#19708,#4936);
#4026=LINE('',#19710,#4937);
#4027=LINE('',#19712,#4938);
#4028=LINE('',#19713,#4939);
#4029=LINE('',#19717,#4940);
#4030=LINE('',#19719,#4941);
#4031=LINE('',#19721,#4942);
#4032=LINE('',#19723,#4943);
#4033=LINE('',#19725,#4944);
#4034=LINE('',#19726,#4945);
#4035=LINE('',#19743,#4946);
#4036=LINE('',#19745,#4947);
#4037=LINE('',#19747,#4948);
#4038=LINE('',#19748,#4949);
#4039=LINE('',#19754,#4950);
#4040=LINE('',#19757,#4951);
#4041=LINE('',#19759,#4952);
#4042=LINE('',#19760,#4953);
#4043=LINE('',#19767,#4954);
#4044=LINE('',#19769,#4955);
#4045=LINE('',#19771,#4956);
#4046=LINE('',#19772,#4957);
#4047=LINE('',#19778,#4958);
#4048=LINE('',#19781,#4959);
#4049=LINE('',#19783,#4960);
#4050=LINE('',#19784,#4961);
#4051=LINE('',#19791,#4962);
#4052=LINE('',#19793,#4963);
#4053=LINE('',#19795,#4964);
#4054=LINE('',#19796,#4965);
#4055=LINE('',#19802,#4966);
#4056=LINE('',#19805,#4967);
#4057=LINE('',#19807,#4968);
#4058=LINE('',#19808,#4969);
#4059=LINE('',#19815,#4970);
#4060=LINE('',#19817,#4971);
#4061=LINE('',#19819,#4972);
#4062=LINE('',#19820,#4973);
#4063=LINE('',#19826,#4974);
#4064=LINE('',#19829,#4975);
#4065=LINE('',#19831,#4976);
#4066=LINE('',#19832,#4977);
#4067=LINE('',#19839,#4978);
#4068=LINE('',#19841,#4979);
#4069=LINE('',#19843,#4980);
#4070=LINE('',#19844,#4981);
#4071=LINE('',#19850,#4982);
#4072=LINE('',#19853,#4983);
#4073=LINE('',#19855,#4984);
#4074=LINE('',#19856,#4985);
#4075=LINE('',#19863,#4986);
#4076=LINE('',#19865,#4987);
#4077=LINE('',#19867,#4988);
#4078=LINE('',#19868,#4989);
#4079=LINE('',#19872,#4990);
#4080=LINE('',#19874,#4991);
#4081=LINE('',#19876,#4992);
#4082=LINE('',#19877,#4993);
#4083=LINE('',#19895,#4994);
#4084=LINE('',#20117,#4995);
#4085=LINE('',#20543,#4996);
#4086=LINE('',#20965,#4997);
#4087=LINE('',#21427,#4998);
#4088=LINE('',#21847,#4999);
#4089=LINE('',#22311,#5000);
#4090=LINE('',#22733,#5001);
#4091=LINE('',#23232,#5002);
#4092=LINE('',#23492,#5003);
#4093=LINE('',#23796,#5004);
#4094=LINE('',#24185,#5005);
#4095=LINE('',#24610,#5006);
#4096=LINE('',#25046,#5007);
#4097=LINE('',#25484,#5008);
#4098=LINE('',#25912,#5009);
#4099=LINE('',#26354,#5010);
#4100=LINE('',#26786,#5011);
#4101=LINE('',#27252,#5012);
#4102=LINE('',#36519,#5013);
#4103=LINE('',#36525,#5014);
#4104=LINE('',#36527,#5015);
#4105=LINE('',#36529,#5016);
#4106=LINE('',#36536,#5017);
#4107=LINE('',#36540,#5018);
#4108=LINE('',#36896,#5019);
#4109=LINE('',#36900,#5020);
#4110=LINE('',#36902,#5021);
#4111=LINE('',#36903,#5022);
#4112=LINE('',#36906,#5023);
#4113=LINE('',#36907,#5024);
#4114=LINE('',#36912,#5025);
#4115=LINE('',#36914,#5026);
#4116=LINE('',#36915,#5027);
#4117=LINE('',#36918,#5028);
#4118=LINE('',#36919,#5029);
#4119=LINE('',#36924,#5030);
#4120=LINE('',#36926,#5031);
#4121=LINE('',#36927,#5032);
#4122=LINE('',#36930,#5033);
#4123=LINE('',#36931,#5034);
#4124=LINE('',#36936,#5035);
#4125=LINE('',#36938,#5036);
#4126=LINE('',#36939,#5037);
#4127=LINE('',#36942,#5038);
#4128=LINE('',#36943,#5039);
#4129=LINE('',#36948,#5040);
#4130=LINE('',#36950,#5041);
#4131=LINE('',#36951,#5042);
#4132=LINE('',#36954,#5043);
#4133=LINE('',#36955,#5044);
#4134=LINE('',#36960,#5045);
#4135=LINE('',#36962,#5046);
#4136=LINE('',#36963,#5047);
#4137=LINE('',#36966,#5048);
#4138=LINE('',#36967,#5049);
#4139=LINE('',#36972,#5050);
#4140=LINE('',#36974,#5051);
#4141=LINE('',#36975,#5052);
#4142=LINE('',#36978,#5053);
#4143=LINE('',#36979,#5054);
#4144=LINE('',#36984,#5055);
#4145=LINE('',#36986,#5056);
#4146=LINE('',#36987,#5057);
#4147=LINE('',#36990,#5058);
#4148=LINE('',#36991,#5059);
#4149=LINE('',#36996,#5060);
#4150=LINE('',#36998,#5061);
#4151=LINE('',#36999,#5062);
#4152=LINE('',#37002,#5063);
#4153=LINE('',#37003,#5064);
#4154=LINE('',#37008,#5065);
#4155=LINE('',#37010,#5066);
#4156=LINE('',#37011,#5067);
#4157=LINE('',#37014,#5068);
#4158=LINE('',#37015,#5069);
#4159=LINE('',#37020,#5070);
#4160=LINE('',#37022,#5071);
#4161=LINE('',#37023,#5072);
#4162=LINE('',#37026,#5073);
#4163=LINE('',#37027,#5074);
#4164=LINE('',#37032,#5075);
#4165=LINE('',#37034,#5076);
#4166=LINE('',#37035,#5077);
#4167=LINE('',#37038,#5078);
#4168=LINE('',#37039,#5079);
#4169=LINE('',#37044,#5080);
#4170=LINE('',#37046,#5081);
#4171=LINE('',#37047,#5082);
#4172=LINE('',#37050,#5083);
#4173=LINE('',#37051,#5084);
#4174=LINE('',#37056,#5085);
#4175=LINE('',#37058,#5086);
#4176=LINE('',#37059,#5087);
#4177=LINE('',#37062,#5088);
#4178=LINE('',#37063,#5089);
#4179=LINE('',#37068,#5090);
#4180=LINE('',#37070,#5091);
#4181=LINE('',#37071,#5092);
#4182=LINE('',#37074,#5093);
#4183=LINE('',#37075,#5094);
#4184=LINE('',#37080,#5095);
#4185=LINE('',#37082,#5096);
#4186=LINE('',#37083,#5097);
#4187=LINE('',#37086,#5098);
#4188=LINE('',#37087,#5099);
#4189=LINE('',#37092,#5100);
#4190=LINE('',#37094,#5101);
#4191=LINE('',#37095,#5102);
#4192=LINE('',#37098,#5103);
#4193=LINE('',#37099,#5104);
#4194=LINE('',#37106,#5105);
#4195=LINE('',#37108,#5106);
#4196=LINE('',#37109,#5107);
#4197=LINE('',#37112,#5108);
#4198=LINE('',#37113,#5109);
#4199=LINE('',#37118,#5110);
#4200=LINE('',#37120,#5111);
#4201=LINE('',#37121,#5112);
#4202=LINE('',#37124,#5113);
#4203=LINE('',#37125,#5114);
#4204=LINE('',#37130,#5115);
#4205=LINE('',#37132,#5116);
#4206=LINE('',#37133,#5117);
#4207=LINE('',#37136,#5118);
#4208=LINE('',#37137,#5119);
#4209=LINE('',#37142,#5120);
#4210=LINE('',#37144,#5121);
#4211=LINE('',#37145,#5122);
#4212=LINE('',#37148,#5123);
#4213=LINE('',#37149,#5124);
#4214=LINE('',#37154,#5125);
#4215=LINE('',#37156,#5126);
#4216=LINE('',#37157,#5127);
#4217=LINE('',#37160,#5128);
#4218=LINE('',#37161,#5129);
#4219=LINE('',#37166,#5130);
#4220=LINE('',#37168,#5131);
#4221=LINE('',#37169,#5132);
#4222=LINE('',#37172,#5133);
#4223=LINE('',#37173,#5134);
#4224=LINE('',#37178,#5135);
#4225=LINE('',#37180,#5136);
#4226=LINE('',#37181,#5137);
#4227=LINE('',#37184,#5138);
#4228=LINE('',#37185,#5139);
#4229=LINE('',#37190,#5140);
#4230=LINE('',#37192,#5141);
#4231=LINE('',#37193,#5142);
#4232=LINE('',#37196,#5143);
#4233=LINE('',#37197,#5144);
#4234=LINE('',#37202,#5145);
#4235=LINE('',#37204,#5146);
#4236=LINE('',#37205,#5147);
#4237=LINE('',#37208,#5148);
#4238=LINE('',#37209,#5149);
#4239=LINE('',#37214,#5150);
#4240=LINE('',#37216,#5151);
#4241=LINE('',#37217,#5152);
#4242=LINE('',#37220,#5153);
#4243=LINE('',#37221,#5154);
#4244=LINE('',#37226,#5155);
#4245=LINE('',#37228,#5156);
#4246=LINE('',#37229,#5157);
#4247=LINE('',#37232,#5158);
#4248=LINE('',#37233,#5159);
#4249=LINE('',#37238,#5160);
#4250=LINE('',#37240,#5161);
#4251=LINE('',#37241,#5162);
#4252=LINE('',#37244,#5163);
#4253=LINE('',#37245,#5164);
#4254=LINE('',#37250,#5165);
#4255=LINE('',#37252,#5166);
#4256=LINE('',#37253,#5167);
#4257=LINE('',#37256,#5168);
#4258=LINE('',#37257,#5169);
#4259=LINE('',#37262,#5170);
#4260=LINE('',#37264,#5171);
#4261=LINE('',#37265,#5172);
#4262=LINE('',#37268,#5173);
#4263=LINE('',#37269,#5174);
#4264=LINE('',#37274,#5175);
#4265=LINE('',#37276,#5176);
#4266=LINE('',#37277,#5177);
#4267=LINE('',#37280,#5178);
#4268=LINE('',#37281,#5179);
#4269=LINE('',#37286,#5180);
#4270=LINE('',#37288,#5181);
#4271=LINE('',#37289,#5182);
#4272=LINE('',#37292,#5183);
#4273=LINE('',#37293,#5184);
#4274=LINE('',#37298,#5185);
#4275=LINE('',#37300,#5186);
#4276=LINE('',#37301,#5187);
#4277=LINE('',#37304,#5188);
#4278=LINE('',#37305,#5189);
#4279=LINE('',#37310,#5190);
#4280=LINE('',#37312,#5191);
#4281=LINE('',#37313,#5192);
#4282=LINE('',#37316,#5193);
#4283=LINE('',#37317,#5194);
#4284=LINE('',#37321,#5195);
#4285=LINE('',#37325,#5196);
#4286=LINE('',#37327,#5197);
#4287=LINE('',#37329,#5198);
#4288=LINE('',#37331,#5199);
#4289=LINE('',#37333,#5200);
#4290=LINE('',#37334,#5201);
#4291=LINE('',#37338,#5202);
#4292=LINE('',#37342,#5203);
#4293=LINE('',#37346,#5204);
#4294=LINE('',#37350,#5205);
#4295=LINE('',#37354,#5206);
#4296=LINE('',#37357,#5207);
#4297=LINE('',#37361,#5208);
#4298=LINE('',#37363,#5209);
#4299=LINE('',#37364,#5210);
#4300=LINE('',#37366,#5211);
#4301=LINE('',#37368,#5212);
#4302=LINE('',#37370,#5213);
#4303=LINE('',#37372,#5214);
#4304=LINE('',#37378,#5215);
#4305=LINE('',#37600,#5216);
#4306=LINE('',#38015,#5217);
#4307=LINE('',#38451,#5218);
#4308=LINE('',#38912,#5219);
#4309=LINE('',#39451,#5220);
#4310=LINE('',#39914,#5221);
#4311=LINE('',#40417,#5222);
#4312=LINE('',#40894,#5223);
#4313=LINE('',#41353,#5224);
#4314=LINE('',#41796,#5225);
#4315=LINE('',#42255,#5226);
#4316=LINE('',#42724,#5227);
#4317=LINE('',#43181,#5228);
#4318=LINE('',#43630,#5229);
#4319=LINE('',#44093,#5230);
#4320=LINE('',#44530,#5231);
#4321=LINE('',#45011,#5232);
#4322=LINE('',#45502,#5233);
#4323=LINE('',#45947,#5234);
#4324=LINE('',#46416,#5235);
#4325=LINE('',#46842,#5236);
#4326=LINE('',#47342,#5237);
#4327=LINE('',#47794,#5238);
#4328=LINE('',#48245,#5239);
#4329=LINE('',#48697,#5240);
#4330=LINE('',#49204,#5241);
#4331=LINE('',#58902,#5242);
#4332=LINE('',#58908,#5243);
#4333=LINE('',#58910,#5244);
#4334=LINE('',#58912,#5245);
#4335=LINE('',#58922,#5246);
#4336=LINE('',#58923,#5247);
#4337=LINE('',#59279,#5248);
#4338=LINE('',#59286,#5249);
#4339=LINE('',#59287,#5250);
#4340=LINE('',#59289,#5251);
#4341=LINE('',#59290,#5252);
#4342=LINE('',#59292,#5253);
#4343=LINE('',#59297,#5254);
#4344=LINE('',#59300,#5255);
#4345=LINE('',#59302,#5256);
#4346=LINE('',#59305,#5257);
#4347=LINE('',#59307,#5258);
#4348=LINE('',#59310,#5259);
#4349=LINE('',#59312,#5260);
#4350=LINE('',#59315,#5261);
#4351=LINE('',#59317,#5262);
#4352=LINE('',#59320,#5263);
#4353=LINE('',#59322,#5264);
#4354=LINE('',#59325,#5265);
#4355=LINE('',#59327,#5266);
#4356=LINE('',#59330,#5267);
#4357=LINE('',#59332,#5268);
#4358=LINE('',#59335,#5269);
#4359=LINE('',#59337,#5270);
#4360=LINE('',#59340,#5271);
#4361=LINE('',#59342,#5272);
#4362=LINE('',#59345,#5273);
#4363=LINE('',#59347,#5274);
#4364=LINE('',#59350,#5275);
#4365=LINE('',#59352,#5276);
#4366=LINE('',#59355,#5277);
#4367=LINE('',#59357,#5278);
#4368=LINE('',#59360,#5279);
#4369=LINE('',#59362,#5280);
#4370=LINE('',#59365,#5281);
#4371=LINE('',#59367,#5282);
#4372=LINE('',#59370,#5283);
#4373=LINE('',#59372,#5284);
#4374=LINE('',#59375,#5285);
#4375=LINE('',#59377,#5286);
#4376=LINE('',#59380,#5287);
#4377=LINE('',#59382,#5288);
#4378=LINE('',#59385,#5289);
#4379=LINE('',#59387,#5290);
#4380=LINE('',#59390,#5291);
#4381=LINE('',#59392,#5292);
#4382=LINE('',#59395,#5293);
#4383=LINE('',#59397,#5294);
#4384=LINE('',#59400,#5295);
#4385=LINE('',#59402,#5296);
#4386=LINE('',#59405,#5297);
#4387=LINE('',#59407,#5298);
#4388=LINE('',#59410,#5299);
#4389=LINE('',#59412,#5300);
#4390=LINE('',#59415,#5301);
#4391=LINE('',#59417,#5302);
#4392=LINE('',#59420,#5303);
#4393=LINE('',#59422,#5304);
#4394=LINE('',#59425,#5305);
#4395=LINE('',#59427,#5306);
#4396=LINE('',#59430,#5307);
#4397=LINE('',#59432,#5308);
#4398=LINE('',#59435,#5309);
#4399=LINE('',#59437,#5310);
#4400=LINE('',#59440,#5311);
#4401=LINE('',#59442,#5312);
#4402=LINE('',#59445,#5313);
#4403=LINE('',#59447,#5314);
#4404=LINE('',#59450,#5315);
#4405=LINE('',#59452,#5316);
#4406=LINE('',#59455,#5317);
#4407=LINE('',#59457,#5318);
#4408=LINE('',#59460,#5319);
#4409=LINE('',#59462,#5320);
#4410=LINE('',#59465,#5321);
#4411=LINE('',#59466,#5322);
#4412=LINE('',#59469,#5323);
#4413=LINE('',#59470,#5324);
#4414=LINE('',#59472,#5325);
#4415=LINE('',#59476,#5326);
#4416=LINE('',#59477,#5327);
#4417=LINE('',#59479,#5328);
#4418=LINE('',#59483,#5329);
#4419=LINE('',#59484,#5330);
#4420=LINE('',#59486,#5331);
#4421=LINE('',#59490,#5332);
#4422=LINE('',#59491,#5333);
#4423=LINE('',#59493,#5334);
#4424=LINE('',#59497,#5335);
#4425=LINE('',#59498,#5336);
#4426=LINE('',#59500,#5337);
#4427=LINE('',#59504,#5338);
#4428=LINE('',#59505,#5339);
#4429=LINE('',#59507,#5340);
#4430=LINE('',#59511,#5341);
#4431=LINE('',#59512,#5342);
#4432=LINE('',#59514,#5343);
#4433=LINE('',#59518,#5344);
#4434=LINE('',#59519,#5345);
#4435=LINE('',#59521,#5346);
#4436=LINE('',#59525,#5347);
#4437=LINE('',#59526,#5348);
#4438=LINE('',#59528,#5349);
#4439=LINE('',#59532,#5350);
#4440=LINE('',#59533,#5351);
#4441=LINE('',#59535,#5352);
#4442=LINE('',#59539,#5353);
#4443=LINE('',#59540,#5354);
#4444=LINE('',#59542,#5355);
#4445=LINE('',#59546,#5356);
#4446=LINE('',#59547,#5357);
#4447=LINE('',#59549,#5358);
#4448=LINE('',#59553,#5359);
#4449=LINE('',#59554,#5360);
#4450=LINE('',#59556,#5361);
#4451=LINE('',#59560,#5362);
#4452=LINE('',#59561,#5363);
#4453=LINE('',#59563,#5364);
#4454=LINE('',#59567,#5365);
#4455=LINE('',#59568,#5366);
#4456=LINE('',#59570,#5367);
#4457=LINE('',#59574,#5368);
#4458=LINE('',#59575,#5369);
#4459=LINE('',#59577,#5370);
#4460=LINE('',#59581,#5371);
#4461=LINE('',#59582,#5372);
#4462=LINE('',#59584,#5373);
#4463=LINE('',#59588,#5374);
#4464=LINE('',#59589,#5375);
#4465=LINE('',#59591,#5376);
#4466=LINE('',#59595,#5377);
#4467=LINE('',#59596,#5378);
#4468=LINE('',#59598,#5379);
#4469=LINE('',#59602,#5380);
#4470=LINE('',#59603,#5381);
#4471=LINE('',#59605,#5382);
#4472=LINE('',#59609,#5383);
#4473=LINE('',#59610,#5384);
#4474=LINE('',#59612,#5385);
#4475=LINE('',#59616,#5386);
#4476=LINE('',#59617,#5387);
#4477=LINE('',#59619,#5388);
#4478=LINE('',#59623,#5389);
#4479=LINE('',#59624,#5390);
#4480=LINE('',#59626,#5391);
#4481=LINE('',#59630,#5392);
#4482=LINE('',#59631,#5393);
#4483=LINE('',#59633,#5394);
#4484=LINE('',#59637,#5395);
#4485=LINE('',#59638,#5396);
#4486=LINE('',#59640,#5397);
#4487=LINE('',#59644,#5398);
#4488=LINE('',#59645,#5399);
#4489=LINE('',#59647,#5400);
#4490=LINE('',#59651,#5401);
#4491=LINE('',#59652,#5402);
#4492=LINE('',#59654,#5403);
#4493=LINE('',#59658,#5404);
#4494=LINE('',#59659,#5405);
#4495=LINE('',#59661,#5406);
#4496=LINE('',#59665,#5407);
#4497=LINE('',#59666,#5408);
#4498=LINE('',#59668,#5409);
#4499=LINE('',#59672,#5410);
#4500=LINE('',#59673,#5411);
#4501=LINE('',#59675,#5412);
#4502=LINE('',#59679,#5413);
#4503=LINE('',#59680,#5414);
#4504=LINE('',#59682,#5415);
#4505=LINE('',#59686,#5416);
#4506=LINE('',#59687,#5417);
#4507=LINE('',#59689,#5418);
#4508=LINE('',#59693,#5419);
#4509=LINE('',#59694,#5420);
#4510=LINE('',#59696,#5421);
#4511=LINE('',#59700,#5422);
#4512=LINE('',#59701,#5423);
#4513=LINE('',#59703,#5424);
#4514=LINE('',#59708,#5425);
#4515=LINE('',#59710,#5426);
#4516=LINE('',#59712,#5427);
#4517=LINE('',#59714,#5428);
#4518=LINE('',#59716,#5429);
#4519=LINE('',#59717,#5430);
#4520=LINE('',#59721,#5431);
#4521=LINE('',#59725,#5432);
#4522=LINE('',#59729,#5433);
#4523=LINE('',#59733,#5434);
#4524=LINE('',#59737,#5435);
#4525=LINE('',#59740,#5436);
#4526=LINE('',#59744,#5437);
#4527=LINE('',#59746,#5438);
#4528=LINE('',#59747,#5439);
#4529=LINE('',#59749,#5440);
#4530=LINE('',#59751,#5441);
#4531=LINE('',#59753,#5442);
#4532=LINE('',#59755,#5443);
#4533=LINE('',#59761,#5444);
#4534=LINE('',#60034,#5445);
#4535=LINE('',#60434,#5446);
#4536=LINE('',#60650,#5447);
#4537=LINE('',#60872,#5448);
#4538=LINE('',#61255,#5449);
#4539=LINE('',#61640,#5450);
#4540=LINE('',#62097,#5451);
#4541=LINE('',#62580,#5452);
#4542=LINE('',#63075,#5453);
#4543=LINE('',#63306,#5454);
#4544=LINE('',#63543,#5455);
#4545=LINE('',#63914,#5456);
#4546=LINE('',#64382,#5457);
#4547=LINE('',#70723,#5458);
#4548=LINE('',#70729,#5459);
#4549=LINE('',#70731,#5460);
#4550=LINE('',#70733,#5461);
#4551=LINE('',#70740,#5462);
#4552=LINE('',#70744,#5463);
#4553=LINE('',#71100,#5464);
#4554=LINE('',#71104,#5465);
#4555=LINE('',#71106,#5466);
#4556=LINE('',#71107,#5467);
#4557=LINE('',#71110,#5468);
#4558=LINE('',#71111,#5469);
#4559=LINE('',#71116,#5470);
#4560=LINE('',#71118,#5471);
#4561=LINE('',#71119,#5472);
#4562=LINE('',#71122,#5473);
#4563=LINE('',#71123,#5474);
#4564=LINE('',#71128,#5475);
#4565=LINE('',#71130,#5476);
#4566=LINE('',#71131,#5477);
#4567=LINE('',#71134,#5478);
#4568=LINE('',#71135,#5479);
#4569=LINE('',#71140,#5480);
#4570=LINE('',#71142,#5481);
#4571=LINE('',#71143,#5482);
#4572=LINE('',#71146,#5483);
#4573=LINE('',#71147,#5484);
#4574=LINE('',#71152,#5485);
#4575=LINE('',#71154,#5486);
#4576=LINE('',#71155,#5487);
#4577=LINE('',#71158,#5488);
#4578=LINE('',#71159,#5489);
#4579=LINE('',#71164,#5490);
#4580=LINE('',#71166,#5491);
#4581=LINE('',#71167,#5492);
#4582=LINE('',#71170,#5493);
#4583=LINE('',#71171,#5494);
#4584=LINE('',#71176,#5495);
#4585=LINE('',#71178,#5496);
#4586=LINE('',#71179,#5497);
#4587=LINE('',#71182,#5498);
#4588=LINE('',#71183,#5499);
#4589=LINE('',#71188,#5500);
#4590=LINE('',#71190,#5501);
#4591=LINE('',#71191,#5502);
#4592=LINE('',#71194,#5503);
#4593=LINE('',#71195,#5504);
#4594=LINE('',#71200,#5505);
#4595=LINE('',#71202,#5506);
#4596=LINE('',#71203,#5507);
#4597=LINE('',#71206,#5508);
#4598=LINE('',#71207,#5509);
#4599=LINE('',#71212,#5510);
#4600=LINE('',#71214,#5511);
#4601=LINE('',#71215,#5512);
#4602=LINE('',#71218,#5513);
#4603=LINE('',#71219,#5514);
#4604=LINE('',#71224,#5515);
#4605=LINE('',#71226,#5516);
#4606=LINE('',#71227,#5517);
#4607=LINE('',#71230,#5518);
#4608=LINE('',#71231,#5519);
#4609=LINE('',#71236,#5520);
#4610=LINE('',#71238,#5521);
#4611=LINE('',#71239,#5522);
#4612=LINE('',#71242,#5523);
#4613=LINE('',#71243,#5524);
#4614=LINE('',#71248,#5525);
#4615=LINE('',#71250,#5526);
#4616=LINE('',#71251,#5527);
#4617=LINE('',#71254,#5528);
#4618=LINE('',#71255,#5529);
#4619=LINE('',#71260,#5530);
#4620=LINE('',#71262,#5531);
#4621=LINE('',#71263,#5532);
#4622=LINE('',#71266,#5533);
#4623=LINE('',#71267,#5534);
#4624=LINE('',#71272,#5535);
#4625=LINE('',#71274,#5536);
#4626=LINE('',#71275,#5537);
#4627=LINE('',#71278,#5538);
#4628=LINE('',#71279,#5539);
#4629=LINE('',#71284,#5540);
#4630=LINE('',#71286,#5541);
#4631=LINE('',#71287,#5542);
#4632=LINE('',#71290,#5543);
#4633=LINE('',#71291,#5544);
#4634=LINE('',#71296,#5545);
#4635=LINE('',#71298,#5546);
#4636=LINE('',#71299,#5547);
#4637=LINE('',#71302,#5548);
#4638=LINE('',#71303,#5549);
#4639=LINE('',#71310,#5550);
#4640=LINE('',#71312,#5551);
#4641=LINE('',#71313,#5552);
#4642=LINE('',#71316,#5553);
#4643=LINE('',#71317,#5554);
#4644=LINE('',#71322,#5555);
#4645=LINE('',#71324,#5556);
#4646=LINE('',#71325,#5557);
#4647=LINE('',#71328,#5558);
#4648=LINE('',#71329,#5559);
#4649=LINE('',#71334,#5560);
#4650=LINE('',#71336,#5561);
#4651=LINE('',#71337,#5562);
#4652=LINE('',#71340,#5563);
#4653=LINE('',#71341,#5564);
#4654=LINE('',#71346,#5565);
#4655=LINE('',#71348,#5566);
#4656=LINE('',#71349,#5567);
#4657=LINE('',#71352,#5568);
#4658=LINE('',#71353,#5569);
#4659=LINE('',#71358,#5570);
#4660=LINE('',#71360,#5571);
#4661=LINE('',#71361,#5572);
#4662=LINE('',#71364,#5573);
#4663=LINE('',#71365,#5574);
#4664=LINE('',#71370,#5575);
#4665=LINE('',#71372,#5576);
#4666=LINE('',#71373,#5577);
#4667=LINE('',#71376,#5578);
#4668=LINE('',#71377,#5579);
#4669=LINE('',#71382,#5580);
#4670=LINE('',#71384,#5581);
#4671=LINE('',#71385,#5582);
#4672=LINE('',#71388,#5583);
#4673=LINE('',#71389,#5584);
#4674=LINE('',#71394,#5585);
#4675=LINE('',#71396,#5586);
#4676=LINE('',#71397,#5587);
#4677=LINE('',#71400,#5588);
#4678=LINE('',#71401,#5589);
#4679=LINE('',#71406,#5590);
#4680=LINE('',#71408,#5591);
#4681=LINE('',#71409,#5592);
#4682=LINE('',#71412,#5593);
#4683=LINE('',#71413,#5594);
#4684=LINE('',#71418,#5595);
#4685=LINE('',#71420,#5596);
#4686=LINE('',#71421,#5597);
#4687=LINE('',#71424,#5598);
#4688=LINE('',#71425,#5599);
#4689=LINE('',#71430,#5600);
#4690=LINE('',#71432,#5601);
#4691=LINE('',#71433,#5602);
#4692=LINE('',#71436,#5603);
#4693=LINE('',#71437,#5604);
#4694=LINE('',#71442,#5605);
#4695=LINE('',#71444,#5606);
#4696=LINE('',#71445,#5607);
#4697=LINE('',#71448,#5608);
#4698=LINE('',#71449,#5609);
#4699=LINE('',#71454,#5610);
#4700=LINE('',#71456,#5611);
#4701=LINE('',#71457,#5612);
#4702=LINE('',#71460,#5613);
#4703=LINE('',#71461,#5614);
#4704=LINE('',#71466,#5615);
#4705=LINE('',#71468,#5616);
#4706=LINE('',#71469,#5617);
#4707=LINE('',#71472,#5618);
#4708=LINE('',#71473,#5619);
#4709=LINE('',#71478,#5620);
#4710=LINE('',#71480,#5621);
#4711=LINE('',#71481,#5622);
#4712=LINE('',#71484,#5623);
#4713=LINE('',#71485,#5624);
#4714=LINE('',#71490,#5625);
#4715=LINE('',#71492,#5626);
#4716=LINE('',#71493,#5627);
#4717=LINE('',#71496,#5628);
#4718=LINE('',#71497,#5629);
#4719=LINE('',#71502,#5630);
#4720=LINE('',#71504,#5631);
#4721=LINE('',#71505,#5632);
#4722=LINE('',#71508,#5633);
#4723=LINE('',#71509,#5634);
#4724=LINE('',#71514,#5635);
#4725=LINE('',#71516,#5636);
#4726=LINE('',#71517,#5637);
#4727=LINE('',#71520,#5638);
#4728=LINE('',#71521,#5639);
#4729=LINE('',#71525,#5640);
#4730=LINE('',#71529,#5641);
#4731=LINE('',#71531,#5642);
#4732=LINE('',#71533,#5643);
#4733=LINE('',#71535,#5644);
#4734=LINE('',#71537,#5645);
#4735=LINE('',#71538,#5646);
#4736=LINE('',#71542,#5647);
#4737=LINE('',#71546,#5648);
#4738=LINE('',#71550,#5649);
#4739=LINE('',#71554,#5650);
#4740=LINE('',#71558,#5651);
#4741=LINE('',#71561,#5652);
#4742=LINE('',#71565,#5653);
#4743=LINE('',#71567,#5654);
#4744=LINE('',#71568,#5655);
#4745=LINE('',#71570,#5656);
#4746=LINE('',#71572,#5657);
#4747=LINE('',#71574,#5658);
#4748=LINE('',#71576,#5659);
#4749=VECTOR('',#15051,4.25);
#4750=VECTOR('',#15060,2.6);
#4751=VECTOR('',#15065,4.25);
#4752=VECTOR('',#15074,2.6);
#4753=VECTOR('',#15079,4.25);
#4754=VECTOR('',#15088,2.6);
#4755=VECTOR('',#15093,4.25);
#4756=VECTOR('',#15102,2.6);
#4757=VECTOR('',#15107,4.25);
#4758=VECTOR('',#15116,2.6);
#4759=VECTOR('',#15121,4.25);
#4760=VECTOR('',#15130,2.6);
#4761=VECTOR('',#15135,5.5);
#4762=VECTOR('',#15140,10.);
#4763=VECTOR('',#15141,10.);
#4764=VECTOR('',#15142,10.);
#4765=VECTOR('',#15143,10.);
#4766=VECTOR('',#15152,5.35);
#4767=VECTOR('',#15159,5.5);
#4768=VECTOR('',#15162,5.35);
#4769=VECTOR('',#15169,5.5);
#4770=VECTOR('',#15172,5.35);
#4771=VECTOR('',#15179,5.5);
#4772=VECTOR('',#15182,5.35);
#4773=VECTOR('',#15203,3.55600000000001);
#4774=VECTOR('',#15208,3.556);
#4775=VECTOR('',#15213,3.556);
#4776=VECTOR('',#15218,3.55600000000001);
#4777=VECTOR('',#15223,10.);
#4778=VECTOR('',#15224,10.);
#4779=VECTOR('',#15225,10.);
#4780=VECTOR('',#15226,10.);
#4781=VECTOR('',#15229,10.);
#4782=VECTOR('',#15230,10.);
#4783=VECTOR('',#15233,10.);
#4784=VECTOR('',#15234,10.);
#4785=VECTOR('',#15237,10.);
#4786=VECTOR('',#15238,10.);
#4787=VECTOR('',#15239,10.);
#4788=VECTOR('',#15240,10.);
#4789=VECTOR('',#15241,10.);
#4790=VECTOR('',#15242,10.);
#4791=VECTOR('',#15243,10.);
#4792=VECTOR('',#15246,10.);
#4793=VECTOR('',#15247,10.);
#4794=VECTOR('',#15248,10.);
#4795=VECTOR('',#15249,10.);
#4796=VECTOR('',#15252,10.);
#4797=VECTOR('',#15253,10.);
#4798=VECTOR('',#15254,10.);
#4799=VECTOR('',#15257,10.);
#4800=VECTOR('',#15258,10.);
#4801=VECTOR('',#15261,10.);
#4802=VECTOR('',#15262,10.);
#4803=VECTOR('',#15263,10.);
#4804=VECTOR('',#15266,10.);
#4805=VECTOR('',#15267,10.);
#4806=VECTOR('',#15270,10.);
#4807=VECTOR('',#15271,10.);
#4808=VECTOR('',#15274,10.);
#4809=VECTOR('',#15277,10.);
#4810=VECTOR('',#15280,10.);
#4811=VECTOR('',#15281,10.);
#4812=VECTOR('',#15284,10.);
#4813=VECTOR('',#15287,10.);
#4814=VECTOR('',#15288,10.);
#4815=VECTOR('',#15291,10.);
#4816=VECTOR('',#15292,10.);
#4817=VECTOR('',#15297,10.);
#4818=VECTOR('',#15300,10.);
#4819=VECTOR('',#15303,10.);
#4820=VECTOR('',#15306,10.);
#4821=VECTOR('',#15307,10.);
#4822=VECTOR('',#15310,10.);
#4823=VECTOR('',#15323,10.);
#4824=VECTOR('',#15324,10.);
#4825=VECTOR('',#15325,10.);
#4826=VECTOR('',#15326,10.);
#4827=VECTOR('',#15361,4.4);
#4828=VECTOR('',#15364,4.25000000000001);
#4829=VECTOR('',#15375,4.4);
#4830=VECTOR('',#15378,4.25);
#4831=VECTOR('',#15389,4.4);
#4832=VECTOR('',#15392,4.25);
#4833=VECTOR('',#15399,4.4);
#4834=VECTOR('',#15402,4.25000000000001);
#4835=VECTOR('',#15411,10.);
#4836=VECTOR('',#15414,10.);
#4837=VECTOR('',#15431,10.);
#4838=VECTOR('',#15434,10.);
#4839=VECTOR('',#15447,10.);
#4840=VECTOR('',#15450,10.);
#4841=VECTOR('',#15463,10.);
#4842=VECTOR('',#15466,10.);
#4843=VECTOR('',#15499,2.6);
#4844=VECTOR('',#15504,2.6);
#4845=VECTOR('',#15509,2.6);
#4846=VECTOR('',#15514,2.6);
#4847=VECTOR('',#15519,2.6);
#4848=VECTOR('',#15524,2.6);
#4849=VECTOR('',#15529,2.6);
#4850=VECTOR('',#15534,2.6);
#4851=VECTOR('',#15541,3.42499999999999);
#4852=VECTOR('',#15544,3.225);
#4853=VECTOR('',#15551,3.425);
#4854=VECTOR('',#15554,3.225);
#4855=VECTOR('',#15559,3.225);
#4856=VECTOR('',#15564,3.225);
#4857=VECTOR('',#15569,3.225);
#4858=VECTOR('',#15574,3.225);
#4859=VECTOR('',#15581,3.425);
#4860=VECTOR('',#15584,3.225);
#4861=VECTOR('',#15591,3.42499999999999);
#4862=VECTOR('',#15594,3.225);
#4863=VECTOR('',#15599,3.225);
#4864=VECTOR('',#15602,3.225);
#4865=VECTOR('',#15605,3.225);
#4866=VECTOR('',#15608,3.225);
#4867=VECTOR('',#15611,3.22499999999998);
#4868=VECTOR('',#15614,3.22499999999998);
#4869=VECTOR('',#15617,3.225);
#4870=VECTOR('',#15620,3.225);
#4871=VECTOR('',#15623,10.);
#4872=VECTOR('',#15624,10.);
#4873=VECTOR('',#15625,10.);
#4874=VECTOR('',#15628,10.);
#4875=VECTOR('',#15629,10.);
#4876=VECTOR('',#15632,10.);
#4877=VECTOR('',#15633,10.);
#4878=VECTOR('',#15636,10.);
#4879=VECTOR('',#15639,10.);
#4880=VECTOR('',#15640,10.);
#4881=VECTOR('',#15641,10.);
#4882=VECTOR('',#15644,10.);
#4883=VECTOR('',#15645,10.);
#4884=VECTOR('',#15648,10.);
#4885=VECTOR('',#15649,10.);
#4886=VECTOR('',#15652,10.);
#4887=VECTOR('',#15659,2.464);
#4888=VECTOR('',#15664,2.464);
#4889=VECTOR('',#15667,2.464);
#4890=VECTOR('',#15672,2.464);
#4891=VECTOR('',#15675,2.464);
#4892=VECTOR('',#15680,2.464);
#4893=VECTOR('',#15689,6.1);
#4894=VECTOR('',#15694,6.35);
#4895=VECTOR('',#15697,6.1);
#4896=VECTOR('',#15708,2.61400000000001);
#4897=VECTOR('',#15713,10.);
#4898=VECTOR('',#15714,10.);
#4899=VECTOR('',#15715,10.);
#4900=VECTOR('',#15716,10.);
#4901=VECTOR('',#15721,2.464);
#4902=VECTOR('',#15730,2.61400000000001);
#4903=VECTOR('',#15733,2.464);
#4904=VECTOR('',#15740,2.464);
#4905=VECTOR('',#15745,10.);
#4906=VECTOR('',#15748,10.);
#4907=VECTOR('',#15751,2.464);
#4908=VECTOR('',#15754,10.);
#4909=VECTOR('',#15757,10.);
#4910=VECTOR('',#15760,10.);
#4911=VECTOR('',#15761,10.);
#4912=VECTOR('',#15762,10.);
#4913=VECTOR('',#15763,10.);
#4914=VECTOR('',#15764,10.);
#4915=VECTOR('',#15765,10.);
#4916=VECTOR('',#15766,10.);
#4917=VECTOR('',#15767,10.);
#4918=VECTOR('',#15770,10.);
#4919=VECTOR('',#15771,10.);
#4920=VECTOR('',#15772,10.);
#4921=VECTOR('',#15775,10.);
#4922=VECTOR('',#15780,10.);
#4923=VECTOR('',#15781,10.);
#4924=VECTOR('',#15782,10.);
#4925=VECTOR('',#15783,10.);
#4926=VECTOR('',#15784,10.);
#4927=VECTOR('',#15785,10.);
#4928=VECTOR('',#15786,10.);
#4929=VECTOR('',#15789,10.);
#4930=VECTOR('',#15792,10.);
#4931=VECTOR('',#15795,10.);
#4932=VECTOR('',#15798,10.);
#4933=VECTOR('',#15801,10.);
#4934=VECTOR('',#15810,10.);
#4935=VECTOR('',#15811,10.);
#4936=VECTOR('',#15812,10.);
#4937=VECTOR('',#15813,10.);
#4938=VECTOR('',#15814,10.);
#4939=VECTOR('',#15815,10.);
#4940=VECTOR('',#15818,10.);
#4941=VECTOR('',#15819,10.);
#4942=VECTOR('',#15820,9.99999999999999);
#4943=VECTOR('',#15821,10.);
#4944=VECTOR('',#15822,10.);
#4945=VECTOR('',#15823,10.);
#4946=VECTOR('',#15852,10.);
#4947=VECTOR('',#15853,10.);
#4948=VECTOR('',#15854,10.);
#4949=VECTOR('',#15855,10.);
#4950=VECTOR('',#15862,10.);
#4951=VECTOR('',#15865,10.);
#4952=VECTOR('',#15866,10.);
#4953=VECTOR('',#15867,10.);
#4954=VECTOR('',#15876,10.);
#4955=VECTOR('',#15877,10.);
#4956=VECTOR('',#15878,10.);
#4957=VECTOR('',#15879,10.);
#4958=VECTOR('',#15886,10.);
#4959=VECTOR('',#15889,10.);
#4960=VECTOR('',#15890,10.);
#4961=VECTOR('',#15891,10.);
#4962=VECTOR('',#15900,10.);
#4963=VECTOR('',#15901,10.);
#4964=VECTOR('',#15902,10.);
#4965=VECTOR('',#15903,10.);
#4966=VECTOR('',#15910,9.99999999999999);
#4967=VECTOR('',#15913,10.);
#4968=VECTOR('',#15914,10.);
#4969=VECTOR('',#15915,9.99999999999999);
#4970=VECTOR('',#15924,10.);
#4971=VECTOR('',#15925,9.99999999999999);
#4972=VECTOR('',#15926,10.);
#4973=VECTOR('',#15927,9.99999999999999);
#4974=VECTOR('',#15934,10.);
#4975=VECTOR('',#15937,10.);
#4976=VECTOR('',#15938,10.);
#4977=VECTOR('',#15939,10.);
#4978=VECTOR('',#15948,10.);
#4979=VECTOR('',#15949,9.99999999999999);
#4980=VECTOR('',#15950,10.);
#4981=VECTOR('',#15951,9.99999999999999);
#4982=VECTOR('',#15958,10.);
#4983=VECTOR('',#15961,10.);
#4984=VECTOR('',#15962,10.);
#4985=VECTOR('',#15963,10.);
#4986=VECTOR('',#15972,10.);
#4987=VECTOR('',#15973,10.);
#4988=VECTOR('',#15974,10.);
#4989=VECTOR('',#15975,10.);
#4990=VECTOR('',#15978,10.);
#4991=VECTOR('',#15979,10.);
#4992=VECTOR('',#15980,10.);
#4993=VECTOR('',#15981,10.);
#4994=VECTOR('',#16008,1.92913);
#4995=VECTOR('',#16013,1.92913);
#4996=VECTOR('',#16016,1.92913);
#4997=VECTOR('',#16019,1.92913);
#4998=VECTOR('',#16022,1.92913);
#4999=VECTOR('',#16025,1.92913);
#5000=VECTOR('',#16028,1.92913);
#5001=VECTOR('',#16031,1.92913);
#5002=VECTOR('',#16034,1.92913);
#5003=VECTOR('',#16037,1.92913);
#5004=VECTOR('',#16040,1.92913);
#5005=VECTOR('',#16043,1.92913);
#5006=VECTOR('',#16046,1.92913);
#5007=VECTOR('',#16049,1.92913);
#5008=VECTOR('',#16052,1.92913);
#5009=VECTOR('',#16055,1.92913);
#5010=VECTOR('',#16058,1.92913);
#5011=VECTOR('',#16061,1.92913);
#5012=VECTOR('',#16064,1.92913);
#5013=VECTOR('',#16099,2.16347);
#5014=VECTOR('',#16106,10.);
#5015=VECTOR('',#16107,10.);
#5016=VECTOR('',#16108,10.);
#5017=VECTOR('',#16111,10.);
#5018=VECTOR('',#16112,10.);
#5019=VECTOR('',#16191,3.7624);
#5020=VECTOR('',#16196,10.);
#5021=VECTOR('',#16197,10.);
#5022=VECTOR('',#16198,10.);
#5023=VECTOR('',#16201,10.);
#5024=VECTOR('',#16202,10.);
#5025=VECTOR('',#16209,10.);
#5026=VECTOR('',#16210,10.);
#5027=VECTOR('',#16211,10.);
#5028=VECTOR('',#16214,10.);
#5029=VECTOR('',#16215,10.);
#5030=VECTOR('',#16222,10.);
#5031=VECTOR('',#16223,10.);
#5032=VECTOR('',#16224,10.);
#5033=VECTOR('',#16227,10.);
#5034=VECTOR('',#16228,10.);
#5035=VECTOR('',#16235,10.);
#5036=VECTOR('',#16236,10.);
#5037=VECTOR('',#16237,10.);
#5038=VECTOR('',#16240,10.);
#5039=VECTOR('',#16241,10.);
#5040=VECTOR('',#16248,10.);
#5041=VECTOR('',#16249,10.);
#5042=VECTOR('',#16250,10.);
#5043=VECTOR('',#16253,10.);
#5044=VECTOR('',#16254,10.);
#5045=VECTOR('',#16261,10.);
#5046=VECTOR('',#16262,10.);
#5047=VECTOR('',#16263,10.);
#5048=VECTOR('',#16266,10.);
#5049=VECTOR('',#16267,10.);
#5050=VECTOR('',#16274,10.);
#5051=VECTOR('',#16275,10.);
#5052=VECTOR('',#16276,10.);
#5053=VECTOR('',#16279,10.);
#5054=VECTOR('',#16280,10.);
#5055=VECTOR('',#16287,10.);
#5056=VECTOR('',#16288,10.);
#5057=VECTOR('',#16289,10.);
#5058=VECTOR('',#16292,10.);
#5059=VECTOR('',#16293,10.);
#5060=VECTOR('',#16300,10.);
#5061=VECTOR('',#16301,10.);
#5062=VECTOR('',#16302,10.);
#5063=VECTOR('',#16305,10.);
#5064=VECTOR('',#16306,10.);
#5065=VECTOR('',#16313,10.);
#5066=VECTOR('',#16314,10.);
#5067=VECTOR('',#16315,10.);
#5068=VECTOR('',#16318,10.);
#5069=VECTOR('',#16319,10.);
#5070=VECTOR('',#16326,10.);
#5071=VECTOR('',#16327,10.);
#5072=VECTOR('',#16328,10.);
#5073=VECTOR('',#16331,10.);
#5074=VECTOR('',#16332,10.);
#5075=VECTOR('',#16339,10.);
#5076=VECTOR('',#16340,10.);
#5077=VECTOR('',#16341,10.);
#5078=VECTOR('',#16344,10.);
#5079=VECTOR('',#16345,10.);
#5080=VECTOR('',#16352,10.);
#5081=VECTOR('',#16353,10.);
#5082=VECTOR('',#16354,10.);
#5083=VECTOR('',#16357,10.);
#5084=VECTOR('',#16358,10.);
#5085=VECTOR('',#16365,10.);
#5086=VECTOR('',#16366,10.);
#5087=VECTOR('',#16367,10.);
#5088=VECTOR('',#16370,10.);
#5089=VECTOR('',#16371,10.);
#5090=VECTOR('',#16378,10.);
#5091=VECTOR('',#16379,10.);
#5092=VECTOR('',#16380,10.);
#5093=VECTOR('',#16383,10.);
#5094=VECTOR('',#16384,10.);
#5095=VECTOR('',#16391,10.);
#5096=VECTOR('',#16392,10.);
#5097=VECTOR('',#16393,10.);
#5098=VECTOR('',#16396,10.);
#5099=VECTOR('',#16397,10.);
#5100=VECTOR('',#16404,10.);
#5101=VECTOR('',#16405,10.);
#5102=VECTOR('',#16406,10.);
#5103=VECTOR('',#16409,10.);
#5104=VECTOR('',#16410,10.);
#5105=VECTOR('',#16419,10.);
#5106=VECTOR('',#16420,10.);
#5107=VECTOR('',#16421,10.);
#5108=VECTOR('',#16424,10.);
#5109=VECTOR('',#16425,10.);
#5110=VECTOR('',#16432,10.);
#5111=VECTOR('',#16433,10.);
#5112=VECTOR('',#16434,10.);
#5113=VECTOR('',#16437,10.);
#5114=VECTOR('',#16438,10.);
#5115=VECTOR('',#16445,10.);
#5116=VECTOR('',#16446,10.);
#5117=VECTOR('',#16447,10.);
#5118=VECTOR('',#16450,10.);
#5119=VECTOR('',#16451,10.);
#5120=VECTOR('',#16458,10.);
#5121=VECTOR('',#16459,10.);
#5122=VECTOR('',#16460,10.);
#5123=VECTOR('',#16463,10.);
#5124=VECTOR('',#16464,10.);
#5125=VECTOR('',#16471,10.);
#5126=VECTOR('',#16472,10.);
#5127=VECTOR('',#16473,10.);
#5128=VECTOR('',#16476,10.);
#5129=VECTOR('',#16477,10.);
#5130=VECTOR('',#16484,10.);
#5131=VECTOR('',#16485,10.);
#5132=VECTOR('',#16486,10.);
#5133=VECTOR('',#16489,10.);
#5134=VECTOR('',#16490,10.);
#5135=VECTOR('',#16497,10.);
#5136=VECTOR('',#16498,10.);
#5137=VECTOR('',#16499,10.);
#5138=VECTOR('',#16502,10.);
#5139=VECTOR('',#16503,10.);
#5140=VECTOR('',#16510,10.);
#5141=VECTOR('',#16511,10.);
#5142=VECTOR('',#16512,10.);
#5143=VECTOR('',#16515,10.);
#5144=VECTOR('',#16516,10.);
#5145=VECTOR('',#16523,10.);
#5146=VECTOR('',#16524,10.);
#5147=VECTOR('',#16525,10.);
#5148=VECTOR('',#16528,10.);
#5149=VECTOR('',#16529,10.);
#5150=VECTOR('',#16536,10.);
#5151=VECTOR('',#16537,10.);
#5152=VECTOR('',#16538,10.);
#5153=VECTOR('',#16541,10.);
#5154=VECTOR('',#16542,10.);
#5155=VECTOR('',#16549,10.);
#5156=VECTOR('',#16550,10.);
#5157=VECTOR('',#16551,10.);
#5158=VECTOR('',#16554,10.);
#5159=VECTOR('',#16555,10.);
#5160=VECTOR('',#16562,10.);
#5161=VECTOR('',#16563,10.);
#5162=VECTOR('',#16564,10.);
#5163=VECTOR('',#16567,10.);
#5164=VECTOR('',#16568,10.);
#5165=VECTOR('',#16575,10.);
#5166=VECTOR('',#16576,10.);
#5167=VECTOR('',#16577,10.);
#5168=VECTOR('',#16580,10.);
#5169=VECTOR('',#16581,10.);
#5170=VECTOR('',#16588,10.);
#5171=VECTOR('',#16589,10.);
#5172=VECTOR('',#16590,10.);
#5173=VECTOR('',#16593,10.);
#5174=VECTOR('',#16594,10.);
#5175=VECTOR('',#16601,10.);
#5176=VECTOR('',#16602,10.);
#5177=VECTOR('',#16603,10.);
#5178=VECTOR('',#16606,10.);
#5179=VECTOR('',#16607,10.);
#5180=VECTOR('',#16614,10.);
#5181=VECTOR('',#16615,10.);
#5182=VECTOR('',#16616,10.);
#5183=VECTOR('',#16619,10.);
#5184=VECTOR('',#16620,10.);
#5185=VECTOR('',#16627,10.);
#5186=VECTOR('',#16628,10.);
#5187=VECTOR('',#16629,10.);
#5188=VECTOR('',#16632,10.);
#5189=VECTOR('',#16633,10.);
#5190=VECTOR('',#16640,10.);
#5191=VECTOR('',#16641,10.);
#5192=VECTOR('',#16642,10.);
#5193=VECTOR('',#16645,10.);
#5194=VECTOR('',#16646,10.);
#5195=VECTOR('',#16653,3.9624);
#5196=VECTOR('',#16656,10.);
#5197=VECTOR('',#16657,10.);
#5198=VECTOR('',#16658,10.);
#5199=VECTOR('',#16659,10.);
#5200=VECTOR('',#16660,10.);
#5201=VECTOR('',#16661,10.);
#5202=VECTOR('',#16664,10.);
#5203=VECTOR('',#16669,10.);
#5204=VECTOR('',#16674,10.);
#5205=VECTOR('',#16679,10.);
#5206=VECTOR('',#16684,10.);
#5207=VECTOR('',#16689,10.);
#5208=VECTOR('',#16694,2.29135888084632);
#5209=VECTOR('',#16697,10.);
#5210=VECTOR('',#16698,10.);
#5211=VECTOR('',#16701,10.);
#5212=VECTOR('',#16704,10.);
#5213=VECTOR('',#16707,10.);
#5214=VECTOR('',#16710,10.);
#5215=VECTOR('',#16717,1.92913);
#5216=VECTOR('',#16722,1.92913);
#5217=VECTOR('',#16725,1.92913);
#5218=VECTOR('',#16728,1.92913);
#5219=VECTOR('',#16731,1.92913);
#5220=VECTOR('',#16734,1.92913);
#5221=VECTOR('',#16737,1.92913);
#5222=VECTOR('',#16740,1.92913);
#5223=VECTOR('',#16743,1.92913);
#5224=VECTOR('',#16746,1.92913);
#5225=VECTOR('',#16749,1.92913);
#5226=VECTOR('',#16752,1.92913);
#5227=VECTOR('',#16755,1.92913);
#5228=VECTOR('',#16758,1.92913);
#5229=VECTOR('',#16761,1.92913);
#5230=VECTOR('',#16764,1.92913);
#5231=VECTOR('',#16767,1.92913);
#5232=VECTOR('',#16770,1.92913);
#5233=VECTOR('',#16773,1.92913);
#5234=VECTOR('',#16776,1.92913);
#5235=VECTOR('',#16779,1.92913);
#5236=VECTOR('',#16782,1.92913);
#5237=VECTOR('',#16785,1.92913);
#5238=VECTOR('',#16788,1.92913);
#5239=VECTOR('',#16791,1.92913);
#5240=VECTOR('',#16794,1.92913);
#5241=VECTOR('',#16797,1.92913);
#5242=VECTOR('',#16832,2.16347);
#5243=VECTOR('',#16839,10.);
#5244=VECTOR('',#16840,10.);
#5245=VECTOR('',#16841,10.);
#5246=VECTOR('',#16844,10.);
#5247=VECTOR('',#16845,10.);
#5248=VECTOR('',#16924,3.7624);
#5249=VECTOR('',#16931,10.);
#5250=VECTOR('',#16932,10.);
#5251=VECTOR('',#16935,10.);
#5252=VECTOR('',#16936,10.);
#5253=VECTOR('',#16939,10.);
#5254=VECTOR('',#16944,3.9624);
#5255=VECTOR('',#16947,10.);
#5256=VECTOR('',#16948,10.);
#5257=VECTOR('',#16951,10.);
#5258=VECTOR('',#16952,10.);
#5259=VECTOR('',#16955,10.);
#5260=VECTOR('',#16956,10.);
#5261=VECTOR('',#16959,10.);
#5262=VECTOR('',#16960,10.);
#5263=VECTOR('',#16963,10.);
#5264=VECTOR('',#16964,10.);
#5265=VECTOR('',#16967,10.);
#5266=VECTOR('',#16968,10.);
#5267=VECTOR('',#16971,10.);
#5268=VECTOR('',#16972,10.);
#5269=VECTOR('',#16975,10.);
#5270=VECTOR('',#16976,10.);
#5271=VECTOR('',#16979,10.);
#5272=VECTOR('',#16980,10.);
#5273=VECTOR('',#16983,10.);
#5274=VECTOR('',#16984,10.);
#5275=VECTOR('',#16987,10.);
#5276=VECTOR('',#16988,10.);
#5277=VECTOR('',#16991,10.);
#5278=VECTOR('',#16992,10.);
#5279=VECTOR('',#16995,10.);
#5280=VECTOR('',#16996,10.);
#5281=VECTOR('',#16999,10.);
#5282=VECTOR('',#17000,10.);
#5283=VECTOR('',#17003,10.);
#5284=VECTOR('',#17004,10.);
#5285=VECTOR('',#17007,10.);
#5286=VECTOR('',#17008,10.);
#5287=VECTOR('',#17011,10.);
#5288=VECTOR('',#17012,10.);
#5289=VECTOR('',#17015,10.);
#5290=VECTOR('',#17016,10.);
#5291=VECTOR('',#17019,10.);
#5292=VECTOR('',#17020,10.);
#5293=VECTOR('',#17023,10.);
#5294=VECTOR('',#17024,10.);
#5295=VECTOR('',#17027,10.);
#5296=VECTOR('',#17028,10.);
#5297=VECTOR('',#17031,10.);
#5298=VECTOR('',#17032,10.);
#5299=VECTOR('',#17035,10.);
#5300=VECTOR('',#17036,10.);
#5301=VECTOR('',#17039,10.);
#5302=VECTOR('',#17040,10.);
#5303=VECTOR('',#17043,10.);
#5304=VECTOR('',#17044,10.);
#5305=VECTOR('',#17047,10.);
#5306=VECTOR('',#17048,10.);
#5307=VECTOR('',#17051,10.);
#5308=VECTOR('',#17052,10.);
#5309=VECTOR('',#17055,10.);
#5310=VECTOR('',#17056,10.);
#5311=VECTOR('',#17059,10.);
#5312=VECTOR('',#17060,10.);
#5313=VECTOR('',#17063,10.);
#5314=VECTOR('',#17064,10.);
#5315=VECTOR('',#17067,10.);
#5316=VECTOR('',#17068,10.);
#5317=VECTOR('',#17071,10.);
#5318=VECTOR('',#17072,10.);
#5319=VECTOR('',#17075,10.);
#5320=VECTOR('',#17076,10.);
#5321=VECTOR('',#17079,10.);
#5322=VECTOR('',#17080,10.);
#5323=VECTOR('',#17083,10.);
#5324=VECTOR('',#17084,10.);
#5325=VECTOR('',#17087,10.);
#5326=VECTOR('',#17092,10.);
#5327=VECTOR('',#17093,10.);
#5328=VECTOR('',#17096,10.);
#5329=VECTOR('',#17101,10.);
#5330=VECTOR('',#17102,10.);
#5331=VECTOR('',#17105,10.);
#5332=VECTOR('',#17110,10.);
#5333=VECTOR('',#17111,10.);
#5334=VECTOR('',#17114,10.);
#5335=VECTOR('',#17119,10.);
#5336=VECTOR('',#17120,10.);
#5337=VECTOR('',#17123,10.);
#5338=VECTOR('',#17128,10.);
#5339=VECTOR('',#17129,10.);
#5340=VECTOR('',#17132,10.);
#5341=VECTOR('',#17137,10.);
#5342=VECTOR('',#17138,10.);
#5343=VECTOR('',#17141,10.);
#5344=VECTOR('',#17146,10.);
#5345=VECTOR('',#17147,10.);
#5346=VECTOR('',#17150,10.);
#5347=VECTOR('',#17155,10.);
#5348=VECTOR('',#17156,10.);
#5349=VECTOR('',#17159,10.);
#5350=VECTOR('',#17164,10.);
#5351=VECTOR('',#17165,10.);
#5352=VECTOR('',#17168,10.);
#5353=VECTOR('',#17173,10.);
#5354=VECTOR('',#17174,10.);
#5355=VECTOR('',#17177,10.);
#5356=VECTOR('',#17182,10.);
#5357=VECTOR('',#17183,10.);
#5358=VECTOR('',#17186,10.);
#5359=VECTOR('',#17191,10.);
#5360=VECTOR('',#17192,10.);
#5361=VECTOR('',#17195,10.);
#5362=VECTOR('',#17200,10.);
#5363=VECTOR('',#17201,10.);
#5364=VECTOR('',#17204,10.);
#5365=VECTOR('',#17209,10.);
#5366=VECTOR('',#17210,10.);
#5367=VECTOR('',#17213,10.);
#5368=VECTOR('',#17218,10.);
#5369=VECTOR('',#17219,10.);
#5370=VECTOR('',#17222,10.);
#5371=VECTOR('',#17227,10.);
#5372=VECTOR('',#17228,10.);
#5373=VECTOR('',#17231,10.);
#5374=VECTOR('',#17236,10.);
#5375=VECTOR('',#17237,10.);
#5376=VECTOR('',#17240,10.);
#5377=VECTOR('',#17245,10.);
#5378=VECTOR('',#17246,10.);
#5379=VECTOR('',#17249,10.);
#5380=VECTOR('',#17254,10.);
#5381=VECTOR('',#17255,10.);
#5382=VECTOR('',#17258,10.);
#5383=VECTOR('',#17263,10.);
#5384=VECTOR('',#17264,10.);
#5385=VECTOR('',#17267,10.);
#5386=VECTOR('',#17272,10.);
#5387=VECTOR('',#17273,10.);
#5388=VECTOR('',#17276,10.);
#5389=VECTOR('',#17281,10.);
#5390=VECTOR('',#17282,10.);
#5391=VECTOR('',#17285,10.);
#5392=VECTOR('',#17290,10.);
#5393=VECTOR('',#17291,10.);
#5394=VECTOR('',#17294,10.);
#5395=VECTOR('',#17299,10.);
#5396=VECTOR('',#17300,10.);
#5397=VECTOR('',#17303,10.);
#5398=VECTOR('',#17308,10.);
#5399=VECTOR('',#17309,10.);
#5400=VECTOR('',#17312,10.);
#5401=VECTOR('',#17317,10.);
#5402=VECTOR('',#17318,10.);
#5403=VECTOR('',#17321,10.);
#5404=VECTOR('',#17326,10.);
#5405=VECTOR('',#17327,10.);
#5406=VECTOR('',#17330,10.);
#5407=VECTOR('',#17335,10.);
#5408=VECTOR('',#17336,10.);
#5409=VECTOR('',#17339,10.);
#5410=VECTOR('',#17344,10.);
#5411=VECTOR('',#17345,10.);
#5412=VECTOR('',#17348,10.);
#5413=VECTOR('',#17353,10.);
#5414=VECTOR('',#17354,10.);
#5415=VECTOR('',#17357,10.);
#5416=VECTOR('',#17362,10.);
#5417=VECTOR('',#17363,10.);
#5418=VECTOR('',#17366,10.);
#5419=VECTOR('',#17371,10.);
#5420=VECTOR('',#17372,10.);
#5421=VECTOR('',#17375,10.);
#5422=VECTOR('',#17380,10.);
#5423=VECTOR('',#17381,10.);
#5424=VECTOR('',#17384,10.);
#5425=VECTOR('',#17389,10.);
#5426=VECTOR('',#17390,10.);
#5427=VECTOR('',#17391,10.);
#5428=VECTOR('',#17392,10.);
#5429=VECTOR('',#17393,10.);
#5430=VECTOR('',#17394,9.99999999999999);
#5431=VECTOR('',#17397,10.);
#5432=VECTOR('',#17402,10.);
#5433=VECTOR('',#17407,10.);
#5434=VECTOR('',#17412,10.);
#5435=VECTOR('',#17417,10.);
#5436=VECTOR('',#17422,9.99999999999999);
#5437=VECTOR('',#17427,1.14567944042316);
#5438=VECTOR('',#17430,10.);
#5439=VECTOR('',#17431,10.);
#5440=VECTOR('',#17434,10.);
#5441=VECTOR('',#17437,10.);
#5442=VECTOR('',#17440,10.);
#5443=VECTOR('',#17443,10.);
#5444=VECTOR('',#17450,2.40538);
#5445=VECTOR('',#17455,2.40538);
#5446=VECTOR('',#17458,2.40538);
#5447=VECTOR('',#17461,2.40538);
#5448=VECTOR('',#17464,2.40538);
#5449=VECTOR('',#17467,2.40538);
#5450=VECTOR('',#17470,2.40538);
#5451=VECTOR('',#17473,2.40538);
#5452=VECTOR('',#17476,2.40538);
#5453=VECTOR('',#17479,2.40538);
#5454=VECTOR('',#17482,2.40538);
#5455=VECTOR('',#17485,2.40538);
#5456=VECTOR('',#17488,2.40538);
#5457=VECTOR('',#17491,2.40538);
#5458=VECTOR('',#17526,2.91023);
#5459=VECTOR('',#17533,10.);
#5460=VECTOR('',#17534,10.);
#5461=VECTOR('',#17535,10.);
#5462=VECTOR('',#17538,10.);
#5463=VECTOR('',#17539,10.);
#5464=VECTOR('',#17618,4.5625);
#5465=VECTOR('',#17623,10.);
#5466=VECTOR('',#17624,10.);
#5467=VECTOR('',#17625,10.);
#5468=VECTOR('',#17628,10.);
#5469=VECTOR('',#17629,10.);
#5470=VECTOR('',#17636,10.);
#5471=VECTOR('',#17637,10.);
#5472=VECTOR('',#17638,10.);
#5473=VECTOR('',#17641,10.);
#5474=VECTOR('',#17642,10.);
#5475=VECTOR('',#17649,10.);
#5476=VECTOR('',#17650,10.);
#5477=VECTOR('',#17651,10.);
#5478=VECTOR('',#17654,10.);
#5479=VECTOR('',#17655,10.);
#5480=VECTOR('',#17662,10.);
#5481=VECTOR('',#17663,10.);
#5482=VECTOR('',#17664,10.);
#5483=VECTOR('',#17667,10.);
#5484=VECTOR('',#17668,10.);
#5485=VECTOR('',#17675,10.);
#5486=VECTOR('',#17676,10.);
#5487=VECTOR('',#17677,10.);
#5488=VECTOR('',#17680,10.);
#5489=VECTOR('',#17681,10.);
#5490=VECTOR('',#17688,10.);
#5491=VECTOR('',#17689,10.);
#5492=VECTOR('',#17690,10.);
#5493=VECTOR('',#17693,10.);
#5494=VECTOR('',#17694,10.);
#5495=VECTOR('',#17701,10.);
#5496=VECTOR('',#17702,10.);
#5497=VECTOR('',#17703,10.);
#5498=VECTOR('',#17706,10.);
#5499=VECTOR('',#17707,10.);
#5500=VECTOR('',#17714,10.);
#5501=VECTOR('',#17715,10.);
#5502=VECTOR('',#17716,10.);
#5503=VECTOR('',#17719,10.);
#5504=VECTOR('',#17720,10.);
#5505=VECTOR('',#17727,10.);
#5506=VECTOR('',#17728,10.);
#5507=VECTOR('',#17729,10.);
#5508=VECTOR('',#17732,10.);
#5509=VECTOR('',#17733,10.);
#5510=VECTOR('',#17740,10.);
#5511=VECTOR('',#17741,10.);
#5512=VECTOR('',#17742,10.);
#5513=VECTOR('',#17745,10.);
#5514=VECTOR('',#17746,10.);
#5515=VECTOR('',#17753,10.);
#5516=VECTOR('',#17754,10.);
#5517=VECTOR('',#17755,10.);
#5518=VECTOR('',#17758,10.);
#5519=VECTOR('',#17759,10.);
#5520=VECTOR('',#17766,10.);
#5521=VECTOR('',#17767,10.);
#5522=VECTOR('',#17768,10.);
#5523=VECTOR('',#17771,10.);
#5524=VECTOR('',#17772,10.);
#5525=VECTOR('',#17779,10.);
#5526=VECTOR('',#17780,10.);
#5527=VECTOR('',#17781,10.);
#5528=VECTOR('',#17784,10.);
#5529=VECTOR('',#17785,10.);
#5530=VECTOR('',#17792,10.);
#5531=VECTOR('',#17793,10.);
#5532=VECTOR('',#17794,10.);
#5533=VECTOR('',#17797,10.);
#5534=VECTOR('',#17798,10.);
#5535=VECTOR('',#17805,10.);
#5536=VECTOR('',#17806,10.);
#5537=VECTOR('',#17807,10.);
#5538=VECTOR('',#17810,10.);
#5539=VECTOR('',#17811,10.);
#5540=VECTOR('',#17818,10.);
#5541=VECTOR('',#17819,10.);
#5542=VECTOR('',#17820,10.);
#5543=VECTOR('',#17823,10.);
#5544=VECTOR('',#17824,10.);
#5545=VECTOR('',#17831,10.);
#5546=VECTOR('',#17832,10.);
#5547=VECTOR('',#17833,10.);
#5548=VECTOR('',#17836,10.);
#5549=VECTOR('',#17837,10.);
#5550=VECTOR('',#17846,10.);
#5551=VECTOR('',#17847,10.);
#5552=VECTOR('',#17848,10.);
#5553=VECTOR('',#17851,10.);
#5554=VECTOR('',#17852,10.);
#5555=VECTOR('',#17859,10.);
#5556=VECTOR('',#17860,10.);
#5557=VECTOR('',#17861,10.);
#5558=VECTOR('',#17864,10.);
#5559=VECTOR('',#17865,10.);
#5560=VECTOR('',#17872,10.);
#5561=VECTOR('',#17873,10.);
#5562=VECTOR('',#17874,10.);
#5563=VECTOR('',#17877,10.);
#5564=VECTOR('',#17878,10.);
#5565=VECTOR('',#17885,10.);
#5566=VECTOR('',#17886,10.);
#5567=VECTOR('',#17887,10.);
#5568=VECTOR('',#17890,10.);
#5569=VECTOR('',#17891,10.);
#5570=VECTOR('',#17898,10.);
#5571=VECTOR('',#17899,10.);
#5572=VECTOR('',#17900,10.);
#5573=VECTOR('',#17903,10.);
#5574=VECTOR('',#17904,10.);
#5575=VECTOR('',#17911,10.);
#5576=VECTOR('',#17912,10.);
#5577=VECTOR('',#17913,10.);
#5578=VECTOR('',#17916,10.);
#5579=VECTOR('',#17917,10.);
#5580=VECTOR('',#17924,10.);
#5581=VECTOR('',#17925,10.);
#5582=VECTOR('',#17926,10.);
#5583=VECTOR('',#17929,10.);
#5584=VECTOR('',#17930,9.99999999999999);
#5585=VECTOR('',#17937,10.);
#5586=VECTOR('',#17938,10.);
#5587=VECTOR('',#17939,10.);
#5588=VECTOR('',#17942,10.);
#5589=VECTOR('',#17943,10.);
#5590=VECTOR('',#17950,10.);
#5591=VECTOR('',#17951,10.);
#5592=VECTOR('',#17952,10.);
#5593=VECTOR('',#17955,10.);
#5594=VECTOR('',#17956,10.);
#5595=VECTOR('',#17963,10.);
#5596=VECTOR('',#17964,10.);
#5597=VECTOR('',#17965,10.);
#5598=VECTOR('',#17968,10.);
#5599=VECTOR('',#17969,10.);
#5600=VECTOR('',#17976,10.);
#5601=VECTOR('',#17977,10.);
#5602=VECTOR('',#17978,10.);
#5603=VECTOR('',#17981,10.);
#5604=VECTOR('',#17982,10.);
#5605=VECTOR('',#17989,10.);
#5606=VECTOR('',#17990,10.);
#5607=VECTOR('',#17991,10.);
#5608=VECTOR('',#17994,10.);
#5609=VECTOR('',#17995,9.99999999999999);
#5610=VECTOR('',#18002,10.);
#5611=VECTOR('',#18003,10.);
#5612=VECTOR('',#18004,10.);
#5613=VECTOR('',#18007,10.);
#5614=VECTOR('',#18008,10.);
#5615=VECTOR('',#18015,10.);
#5616=VECTOR('',#18016,10.);
#5617=VECTOR('',#18017,10.);
#5618=VECTOR('',#18020,10.);
#5619=VECTOR('',#18021,10.);
#5620=VECTOR('',#18028,10.);
#5621=VECTOR('',#18029,10.);
#5622=VECTOR('',#18030,10.);
#5623=VECTOR('',#18033,10.);
#5624=VECTOR('',#18034,10.);
#5625=VECTOR('',#18041,10.);
#5626=VECTOR('',#18042,10.);
#5627=VECTOR('',#18043,10.);
#5628=VECTOR('',#18046,10.);
#5629=VECTOR('',#18047,10.);
#5630=VECTOR('',#18054,10.);
#5631=VECTOR('',#18055,10.);
#5632=VECTOR('',#18056,10.);
#5633=VECTOR('',#18059,10.);
#5634=VECTOR('',#18060,10.);
#5635=VECTOR('',#18067,10.);
#5636=VECTOR('',#18068,10.);
#5637=VECTOR('',#18069,10.);
#5638=VECTOR('',#18072,10.);
#5639=VECTOR('',#18073,10.);
#5640=VECTOR('',#18080,4.7625);
#5641=VECTOR('',#18083,10.);
#5642=VECTOR('',#18084,10.);
#5643=VECTOR('',#18085,9.99999999999999);
#5644=VECTOR('',#18086,10.);
#5645=VECTOR('',#18087,10.);
#5646=VECTOR('',#18088,10.);
#5647=VECTOR('',#18091,10.);
#5648=VECTOR('',#18096,10.);
#5649=VECTOR('',#18101,9.99999999999999);
#5650=VECTOR('',#18106,10.);
#5651=VECTOR('',#18111,10.);
#5652=VECTOR('',#18116,10.);
#5653=VECTOR('',#18121,2.74963065701559);
#5654=VECTOR('',#18124,10.);
#5655=VECTOR('',#18125,10.);
#5656=VECTOR('',#18128,10.);
#5657=VECTOR('',#18131,10.);
#5658=VECTOR('',#18134,10.);
#5659=VECTOR('',#18137,10.);
#5660=ELLIPSE('',#13759,6.01040764008565,4.25);
#5661=ELLIPSE('',#13765,6.01040764008565,4.25);
#5662=ELLIPSE('',#13771,6.01040764008565,4.25);
#5663=ELLIPSE('',#13777,6.01040764008566,4.25);
#5664=ELLIPSE('',#13783,6.01040764008566,4.25);
#5665=ELLIPSE('',#13789,6.01040764008566,4.25);
#5666=VERTEX_POINT('',#18531);
#5667=VERTEX_POINT('',#18533);
#5668=VERTEX_POINT('',#18537);
#5669=VERTEX_POINT('',#18540);
#5670=VERTEX_POINT('',#18542);
#5671=VERTEX_POINT('',#18580);
#5672=VERTEX_POINT('',#18582);
#5673=VERTEX_POINT('',#18586);
#5674=VERTEX_POINT('',#18589);
#5675=VERTEX_POINT('',#18591);
#5676=VERTEX_POINT('',#18629);
#5677=VERTEX_POINT('',#18631);
#5678=VERTEX_POINT('',#18635);
#5679=VERTEX_POINT('',#18638);
#5680=VERTEX_POINT('',#18640);
#5681=VERTEX_POINT('',#18678);
#5682=VERTEX_POINT('',#18680);
#5683=VERTEX_POINT('',#18684);
#5684=VERTEX_POINT('',#18687);
#5685=VERTEX_POINT('',#18689);
#5686=VERTEX_POINT('',#18727);
#5687=VERTEX_POINT('',#18729);
#5688=VERTEX_POINT('',#18733);
#5689=VERTEX_POINT('',#18736);
#5690=VERTEX_POINT('',#18738);
#5691=VERTEX_POINT('',#18776);
#5692=VERTEX_POINT('',#18778);
#5693=VERTEX_POINT('',#18782);
#5694=VERTEX_POINT('',#18785);
#5695=VERTEX_POINT('',#18787);
#5696=VERTEX_POINT('',#18825);
#5697=VERTEX_POINT('',#18827);
#5698=VERTEX_POINT('',#18831);
#5699=VERTEX_POINT('',#18832);
#5700=VERTEX_POINT('',#18834);
#5701=VERTEX_POINT('',#18836);
#5702=VERTEX_POINT('',#18839);
#5703=VERTEX_POINT('',#18841);
#5704=VERTEX_POINT('',#18843);
#5705=VERTEX_POINT('',#18846);
#5706=VERTEX_POINT('',#18850);
#5707=VERTEX_POINT('',#18854);
#5708=VERTEX_POINT('',#18858);
#5709=VERTEX_POINT('',#18862);
#5710=VERTEX_POINT('',#18866);
#5711=VERTEX_POINT('',#18870);
#5712=VERTEX_POINT('',#18874);
#5713=VERTEX_POINT('',#18877);
#5714=VERTEX_POINT('',#18880);
#5715=VERTEX_POINT('',#18883);
#5716=VERTEX_POINT('',#18886);
#5717=VERTEX_POINT('',#18890);
#5718=VERTEX_POINT('',#18894);
#5719=VERTEX_POINT('',#18898);
#5720=VERTEX_POINT('',#18902);
#5721=VERTEX_POINT('',#18903);
#5722=VERTEX_POINT('',#18905);
#5723=VERTEX_POINT('',#18907);
#5724=VERTEX_POINT('',#18914);
#5725=VERTEX_POINT('',#18916);
#5726=VERTEX_POINT('',#18918);
#5727=VERTEX_POINT('',#18920);
#5728=VERTEX_POINT('',#18922);
#5729=VERTEX_POINT('',#18924);
#5730=VERTEX_POINT('',#18926);
#5731=VERTEX_POINT('',#18928);
#5732=VERTEX_POINT('',#18930);
#5733=VERTEX_POINT('',#18932);
#5734=VERTEX_POINT('',#18934);
#5735=VERTEX_POINT('',#18936);
#5736=VERTEX_POINT('',#18938);
#5737=VERTEX_POINT('',#18940);
#5738=VERTEX_POINT('',#18944);
#5739=VERTEX_POINT('',#18945);
#5740=VERTEX_POINT('',#18950);
#5741=VERTEX_POINT('',#18954);
#5742=VERTEX_POINT('',#18955);
#5743=VERTEX_POINT('',#18960);
#5744=VERTEX_POINT('',#18964);
#5745=VERTEX_POINT('',#18968);
#5746=VERTEX_POINT('',#18970);
#5747=VERTEX_POINT('',#18974);
#5748=VERTEX_POINT('',#18980);
#5749=VERTEX_POINT('',#18984);
#5750=VERTEX_POINT('',#18988);
#5751=VERTEX_POINT('',#18996);
#5752=VERTEX_POINT('',#19004);
#5753=VERTEX_POINT('',#19005);
#5754=VERTEX_POINT('',#19012);
#5755=VERTEX_POINT('',#19014);
#5756=VERTEX_POINT('',#19023);
#5757=VERTEX_POINT('',#19024);
#5758=VERTEX_POINT('',#19026);
#5759=VERTEX_POINT('',#19028);
#5760=VERTEX_POINT('',#19031);
#5761=VERTEX_POINT('',#19033);
#5762=VERTEX_POINT('',#19035);
#5763=VERTEX_POINT('',#19037);
#5764=VERTEX_POINT('',#19039);
#5765=VERTEX_POINT('',#19040);
#5766=VERTEX_POINT('',#19044);
#5767=VERTEX_POINT('',#19046);
#5768=VERTEX_POINT('',#19048);
#5769=VERTEX_POINT('',#19049);
#5770=VERTEX_POINT('',#19052);
#5771=VERTEX_POINT('',#19053);
#5772=VERTEX_POINT('',#19056);
#5773=VERTEX_POINT('',#19058);
#5774=VERTEX_POINT('',#19061);
#5775=VERTEX_POINT('',#19065);
#5776=VERTEX_POINT('',#19069);
#5777=VERTEX_POINT('',#19076);
#5778=VERTEX_POINT('',#19085);
#5779=VERTEX_POINT('',#19089);
#5780=VERTEX_POINT('',#19093);
#5781=VERTEX_POINT('',#19100);
#5782=VERTEX_POINT('',#19109);
#5783=VERTEX_POINT('',#19113);
#5784=VERTEX_POINT('',#19117);
#5785=VERTEX_POINT('',#19121);
#5786=VERTEX_POINT('',#19125);
#5787=VERTEX_POINT('',#19132);
#5788=VERTEX_POINT('',#19141);
#5789=VERTEX_POINT('',#19146);
#5790=VERTEX_POINT('',#19148);
#5791=VERTEX_POINT('',#19150);
#5792=VERTEX_POINT('',#19158);
#5793=VERTEX_POINT('',#19161);
#5794=VERTEX_POINT('',#19164);
#5795=VERTEX_POINT('',#19167);
#5796=VERTEX_POINT('',#19172);
#5797=VERTEX_POINT('',#19174);
#5798=VERTEX_POINT('',#19176);
#5799=VERTEX_POINT('',#19184);
#5800=VERTEX_POINT('',#19187);
#5801=VERTEX_POINT('',#19190);
#5802=VERTEX_POINT('',#19195);
#5803=VERTEX_POINT('',#19197);
#5804=VERTEX_POINT('',#19199);
#5805=VERTEX_POINT('',#19207);
#5806=VERTEX_POINT('',#19210);
#5807=VERTEX_POINT('',#19213);
#5808=VERTEX_POINT('',#19218);
#5809=VERTEX_POINT('',#19220);
#5810=VERTEX_POINT('',#19222);
#5811=VERTEX_POINT('',#19230);
#5812=VERTEX_POINT('',#19233);
#5813=VERTEX_POINT('',#19237);
#5814=VERTEX_POINT('',#19241);
#5815=VERTEX_POINT('',#19245);
#5816=VERTEX_POINT('',#19249);
#5817=VERTEX_POINT('',#19253);
#5818=VERTEX_POINT('',#19257);
#5819=VERTEX_POINT('',#19261);
#5820=VERTEX_POINT('',#19265);
#5821=VERTEX_POINT('',#19269);
#5822=VERTEX_POINT('',#19273);
#5823=VERTEX_POINT('',#19277);
#5824=VERTEX_POINT('',#19281);
#5825=VERTEX_POINT('',#19285);
#5826=VERTEX_POINT('',#19289);
#5827=VERTEX_POINT('',#19293);
#5828=VERTEX_POINT('',#19297);
#5829=VERTEX_POINT('',#19301);
#5830=VERTEX_POINT('',#19305);
#5831=VERTEX_POINT('',#19309);
#5832=VERTEX_POINT('',#19313);
#5833=VERTEX_POINT('',#19317);
#5834=VERTEX_POINT('',#19321);
#5835=VERTEX_POINT('',#19325);
#5836=VERTEX_POINT('',#19329);
#5837=VERTEX_POINT('',#19332);
#5838=VERTEX_POINT('',#19335);
#5839=VERTEX_POINT('',#19338);
#5840=VERTEX_POINT('',#19341);
#5841=VERTEX_POINT('',#19344);
#5842=VERTEX_POINT('',#19347);
#5843=VERTEX_POINT('',#19350);
#5844=VERTEX_POINT('',#19353);
#5845=VERTEX_POINT('',#19355);
#5846=VERTEX_POINT('',#19359);
#5847=VERTEX_POINT('',#19363);
#5848=VERTEX_POINT('',#19369);
#5849=VERTEX_POINT('',#19371);
#5850=VERTEX_POINT('',#19375);
#5851=VERTEX_POINT('',#19379);
#5852=VERTEX_POINT('',#19387);
#5853=VERTEX_POINT('',#19388);
#5854=VERTEX_POINT('',#19425);
#5855=VERTEX_POINT('',#19429);
#5856=VERTEX_POINT('',#19432);
#5857=VERTEX_POINT('',#19433);
#5858=VERTEX_POINT('',#19470);
#5859=VERTEX_POINT('',#19474);
#5860=VERTEX_POINT('',#19477);
#5861=VERTEX_POINT('',#19478);
#5862=VERTEX_POINT('',#19515);
#5863=VERTEX_POINT('',#19519);
#5864=VERTEX_POINT('',#19522);
#5865=VERTEX_POINT('',#19525);
#5866=VERTEX_POINT('',#19529);
#5867=VERTEX_POINT('',#19533);
#5868=VERTEX_POINT('',#19539);
#5869=VERTEX_POINT('',#19541);
#5870=VERTEX_POINT('',#19545);
#5871=VERTEX_POINT('',#19546);
#5872=VERTEX_POINT('',#19548);
#5873=VERTEX_POINT('',#19550);
#5874=VERTEX_POINT('',#19553);
#5875=VERTEX_POINT('',#19556);
#5876=VERTEX_POINT('',#19558);
#5877=VERTEX_POINT('',#19560);
#5878=VERTEX_POINT('',#19577);
#5879=VERTEX_POINT('',#19581);
#5880=VERTEX_POINT('',#19583);
#5881=VERTEX_POINT('',#19585);
#5882=VERTEX_POINT('',#19602);
#5883=VERTEX_POINT('',#19619);
#5884=VERTEX_POINT('',#19620);
#5885=VERTEX_POINT('',#19622);
#5886=VERTEX_POINT('',#19624);
#5887=VERTEX_POINT('',#19642);
#5888=VERTEX_POINT('',#19645);
#5889=VERTEX_POINT('',#19647);
#5890=VERTEX_POINT('',#19651);
#5891=VERTEX_POINT('',#19653);
#5892=VERTEX_POINT('',#19656);
#5893=VERTEX_POINT('',#19658);
#5894=VERTEX_POINT('',#19660);
#5895=VERTEX_POINT('',#19662);
#5896=VERTEX_POINT('',#19666);
#5897=VERTEX_POINT('',#19668);
#5898=VERTEX_POINT('',#19672);
#5899=VERTEX_POINT('',#19676);
#5900=VERTEX_POINT('',#19678);
#5901=VERTEX_POINT('',#19680);
#5902=VERTEX_POINT('',#19682);
#5903=VERTEX_POINT('',#19685);
#5904=VERTEX_POINT('',#19702);
#5905=VERTEX_POINT('',#19703);
#5906=VERTEX_POINT('',#19705);
#5907=VERTEX_POINT('',#19707);
#5908=VERTEX_POINT('',#19709);
#5909=VERTEX_POINT('',#19711);
#5910=VERTEX_POINT('',#19715);
#5911=VERTEX_POINT('',#19716);
#5912=VERTEX_POINT('',#19718);
#5913=VERTEX_POINT('',#19720);
#5914=VERTEX_POINT('',#19722);
#5915=VERTEX_POINT('',#19724);
#5916=VERTEX_POINT('',#19741);
#5917=VERTEX_POINT('',#19742);
#5918=VERTEX_POINT('',#19744);
#5919=VERTEX_POINT('',#19746);
#5920=VERTEX_POINT('',#19750);
#5921=VERTEX_POINT('',#19752);
#5922=VERTEX_POINT('',#19756);
#5923=VERTEX_POINT('',#19758);
#5924=VERTEX_POINT('',#19765);
#5925=VERTEX_POINT('',#19766);
#5926=VERTEX_POINT('',#19768);
#5927=VERTEX_POINT('',#19770);
#5928=VERTEX_POINT('',#19774);
#5929=VERTEX_POINT('',#19776);
#5930=VERTEX_POINT('',#19780);
#5931=VERTEX_POINT('',#19782);
#5932=VERTEX_POINT('',#19789);
#5933=VERTEX_POINT('',#19790);
#5934=VERTEX_POINT('',#19792);
#5935=VERTEX_POINT('',#19794);
#5936=VERTEX_POINT('',#19798);
#5937=VERTEX_POINT('',#19800);
#5938=VERTEX_POINT('',#19804);
#5939=VERTEX_POINT('',#19806);
#5940=VERTEX_POINT('',#19813);
#5941=VERTEX_POINT('',#19814);
#5942=VERTEX_POINT('',#19816);
#5943=VERTEX_POINT('',#19818);
#5944=VERTEX_POINT('',#19822);
#5945=VERTEX_POINT('',#19824);
#5946=VERTEX_POINT('',#19828);
#5947=VERTEX_POINT('',#19830);
#5948=VERTEX_POINT('',#19837);
#5949=VERTEX_POINT('',#19838);
#5950=VERTEX_POINT('',#19840);
#5951=VERTEX_POINT('',#19842);
#5952=VERTEX_POINT('',#19846);
#5953=VERTEX_POINT('',#19848);
#5954=VERTEX_POINT('',#19852);
#5955=VERTEX_POINT('',#19854);
#5956=VERTEX_POINT('',#19861);
#5957=VERTEX_POINT('',#19862);
#5958=VERTEX_POINT('',#19864);
#5959=VERTEX_POINT('',#19866);
#5960=VERTEX_POINT('',#19870);
#5961=VERTEX_POINT('',#19871);
#5962=VERTEX_POINT('',#19873);
#5963=VERTEX_POINT('',#19875);
#5964=VERTEX_POINT('',#19888);
#5965=VERTEX_POINT('',#19889);
#5966=VERTEX_POINT('',#19893);
#5967=VERTEX_POINT('',#19894);
#5968=VERTEX_POINT('',#19896);
#5969=VERTEX_POINT('',#20027);
#5970=VERTEX_POINT('',#20115);
#5971=VERTEX_POINT('',#20116);
#5972=VERTEX_POINT('',#20118);
#5973=VERTEX_POINT('',#20333);
#5974=VERTEX_POINT('',#20541);
#5975=VERTEX_POINT('',#20542);
#5976=VERTEX_POINT('',#20963);
#5977=VERTEX_POINT('',#20964);
#5978=VERTEX_POINT('',#20966);
#5979=VERTEX_POINT('',#21183);
#5980=VERTEX_POINT('',#21425);
#5981=VERTEX_POINT('',#21426);
#5982=VERTEX_POINT('',#21845);
#5983=VERTEX_POINT('',#21846);
#5984=VERTEX_POINT('',#21848);
#5985=VERTEX_POINT('',#22087);
#5986=VERTEX_POINT('',#22309);
#5987=VERTEX_POINT('',#22310);
#5988=VERTEX_POINT('',#22731);
#5989=VERTEX_POINT('',#22732);
#5990=VERTEX_POINT('',#22734);
#5991=VERTEX_POINT('',#23033);
#5992=VERTEX_POINT('',#23230);
#5993=VERTEX_POINT('',#23231);
#5994=VERTEX_POINT('',#23439);
#5995=VERTEX_POINT('',#23490);
#5996=VERTEX_POINT('',#23491);
#5997=VERTEX_POINT('',#23493);
#5998=VERTEX_POINT('',#23611);
#5999=VERTEX_POINT('',#23794);
#6000=VERTEX_POINT('',#23795);
#6001=VERTEX_POINT('',#23797);
#6002=VERTEX_POINT('',#24183);
#6003=VERTEX_POINT('',#24184);
#6004=VERTEX_POINT('',#24186);
#6005=VERTEX_POINT('',#24398);
#6006=VERTEX_POINT('',#24608);
#6007=VERTEX_POINT('',#24609);
#6008=VERTEX_POINT('',#25044);
#6009=VERTEX_POINT('',#25045);
#6010=VERTEX_POINT('',#25047);
#6011=VERTEX_POINT('',#25264);
#6012=VERTEX_POINT('',#25482);
#6013=VERTEX_POINT('',#25483);
#6014=VERTEX_POINT('',#25910);
#6015=VERTEX_POINT('',#25911);
#6016=VERTEX_POINT('',#25913);
#6017=VERTEX_POINT('',#26130);
#6018=VERTEX_POINT('',#26352);
#6019=VERTEX_POINT('',#26353);
#6020=VERTEX_POINT('',#26784);
#6021=VERTEX_POINT('',#26785);
#6022=VERTEX_POINT('',#26787);
#6023=VERTEX_POINT('',#27008);
#6024=VERTEX_POINT('',#27250);
#6025=VERTEX_POINT('',#27251);
#6026=VERTEX_POINT('',#27668);
#6027=VERTEX_POINT('',#27669);
#6028=VERTEX_POINT('',#27737);
#6029=VERTEX_POINT('',#27739);
#6030=VERTEX_POINT('',#27745);
#6031=VERTEX_POINT('',#27939);
#6032=VERTEX_POINT('',#28130);
#6033=VERTEX_POINT('',#28321);
#6034=VERTEX_POINT('',#28512);
#6035=VERTEX_POINT('',#28703);
#6036=VERTEX_POINT('',#28897);
#6037=VERTEX_POINT('',#29088);
#6038=VERTEX_POINT('',#29279);
#6039=VERTEX_POINT('',#29470);
#6040=VERTEX_POINT('',#29661);
#6041=VERTEX_POINT('',#29852);
#6042=VERTEX_POINT('',#30046);
#6043=VERTEX_POINT('',#30237);
#6044=VERTEX_POINT('',#30425);
#6045=VERTEX_POINT('',#30616);
#6046=VERTEX_POINT('',#30807);
#6047=VERTEX_POINT('',#30998);
#6048=VERTEX_POINT('',#31192);
#6049=VERTEX_POINT('',#31386);
#6050=VERTEX_POINT('',#31403);
#6051=VERTEX_POINT('',#31405);
#6052=VERTEX_POINT('',#31407);
#6053=VERTEX_POINT('',#31417);
#6054=VERTEX_POINT('',#31608);
#6055=VERTEX_POINT('',#31799);
#6056=VERTEX_POINT('',#31993);
#6057=VERTEX_POINT('',#32187);
#6058=VERTEX_POINT('',#32378);
#6059=VERTEX_POINT('',#32569);
#6060=VERTEX_POINT('',#32760);
#6061=VERTEX_POINT('',#32951);
#6062=VERTEX_POINT('',#33145);
#6063=VERTEX_POINT('',#33339);
#6064=VERTEX_POINT('',#33530);
#6065=VERTEX_POINT('',#33721);
#6066=VERTEX_POINT('',#33912);
#6067=VERTEX_POINT('',#34106);
#6068=VERTEX_POINT('',#34297);
#6069=VERTEX_POINT('',#34488);
#6070=VERTEX_POINT('',#34870);
#6071=VERTEX_POINT('',#34921);
#6072=VERTEX_POINT('',#35040);
#6073=VERTEX_POINT('',#35042);
#6074=VERTEX_POINT('',#35171);
#6075=VERTEX_POINT('',#35919);
#6076=VERTEX_POINT('',#35920);
#6077=VERTEX_POINT('',#36511);
#6078=VERTEX_POINT('',#36515);
#6079=VERTEX_POINT('',#36518);
#6080=VERTEX_POINT('',#36523);
#6081=VERTEX_POINT('',#36524);
#6082=VERTEX_POINT('',#36526);
#6083=VERTEX_POINT('',#36528);
#6084=VERTEX_POINT('',#36534);
#6085=VERTEX_POINT('',#36535);
#6086=VERTEX_POINT('',#36544);
#6087=VERTEX_POINT('',#36545);
#6088=VERTEX_POINT('',#36549);
#6089=VERTEX_POINT('',#36551);
#6090=VERTEX_POINT('',#36555);
#6091=VERTEX_POINT('',#36559);
#6092=VERTEX_POINT('',#36561);
#6093=VERTEX_POINT('',#36565);
#6094=VERTEX_POINT('',#36569);
#6095=VERTEX_POINT('',#36571);
#6096=VERTEX_POINT('',#36575);
#6097=VERTEX_POINT('',#36579);
#6098=VERTEX_POINT('',#36581);
#6099=VERTEX_POINT('',#36585);
#6100=VERTEX_POINT('',#36589);
#6101=VERTEX_POINT('',#36591);
#6102=VERTEX_POINT('',#36595);
#6103=VERTEX_POINT('',#36599);
#6104=VERTEX_POINT('',#36601);
#6105=VERTEX_POINT('',#36605);
#6106=VERTEX_POINT('',#36609);
#6107=VERTEX_POINT('',#36611);
#6108=VERTEX_POINT('',#36615);
#6109=VERTEX_POINT('',#36619);
#6110=VERTEX_POINT('',#36621);
#6111=VERTEX_POINT('',#36625);
#6112=VERTEX_POINT('',#36629);
#6113=VERTEX_POINT('',#36631);
#6114=VERTEX_POINT('',#36635);
#6115=VERTEX_POINT('',#36639);
#6116=VERTEX_POINT('',#36641);
#6117=VERTEX_POINT('',#36645);
#6118=VERTEX_POINT('',#36649);
#6119=VERTEX_POINT('',#36651);
#6120=VERTEX_POINT('',#36655);
#6121=VERTEX_POINT('',#36659);
#6122=VERTEX_POINT('',#36661);
#6123=VERTEX_POINT('',#36665);
#6124=VERTEX_POINT('',#36669);
#6125=VERTEX_POINT('',#36671);
#6126=VERTEX_POINT('',#36675);
#6127=VERTEX_POINT('',#36679);
#6128=VERTEX_POINT('',#36681);
#6129=VERTEX_POINT('',#36685);
#6130=VERTEX_POINT('',#36689);
#6131=VERTEX_POINT('',#36691);
#6132=VERTEX_POINT('',#36695);
#6133=VERTEX_POINT('',#36699);
#6134=VERTEX_POINT('',#36701);
#6135=VERTEX_POINT('',#36705);
#6136=VERTEX_POINT('',#36709);
#6137=VERTEX_POINT('',#36711);
#6138=VERTEX_POINT('',#36715);
#6139=VERTEX_POINT('',#36719);
#6140=VERTEX_POINT('',#36721);
#6141=VERTEX_POINT('',#36725);
#6142=VERTEX_POINT('',#36730);
#6143=VERTEX_POINT('',#36732);
#6144=VERTEX_POINT('',#36736);
#6145=VERTEX_POINT('',#36740);
#6146=VERTEX_POINT('',#36742);
#6147=VERTEX_POINT('',#36746);
#6148=VERTEX_POINT('',#36750);
#6149=VERTEX_POINT('',#36752);
#6150=VERTEX_POINT('',#36756);
#6151=VERTEX_POINT('',#36760);
#6152=VERTEX_POINT('',#36762);
#6153=VERTEX_POINT('',#36766);
#6154=VERTEX_POINT('',#36770);
#6155=VERTEX_POINT('',#36772);
#6156=VERTEX_POINT('',#36776);
#6157=VERTEX_POINT('',#36780);
#6158=VERTEX_POINT('',#36782);
#6159=VERTEX_POINT('',#36786);
#6160=VERTEX_POINT('',#36790);
#6161=VERTEX_POINT('',#36792);
#6162=VERTEX_POINT('',#36796);
#6163=VERTEX_POINT('',#36800);
#6164=VERTEX_POINT('',#36802);
#6165=VERTEX_POINT('',#36806);
#6166=VERTEX_POINT('',#36810);
#6167=VERTEX_POINT('',#36812);
#6168=VERTEX_POINT('',#36816);
#6169=VERTEX_POINT('',#36820);
#6170=VERTEX_POINT('',#36822);
#6171=VERTEX_POINT('',#36826);
#6172=VERTEX_POINT('',#36830);
#6173=VERTEX_POINT('',#36832);
#6174=VERTEX_POINT('',#36836);
#6175=VERTEX_POINT('',#36840);
#6176=VERTEX_POINT('',#36842);
#6177=VERTEX_POINT('',#36846);
#6178=VERTEX_POINT('',#36850);
#6179=VERTEX_POINT('',#36852);
#6180=VERTEX_POINT('',#36856);
#6181=VERTEX_POINT('',#36860);
#6182=VERTEX_POINT('',#36862);
#6183=VERTEX_POINT('',#36866);
#6184=VERTEX_POINT('',#36870);
#6185=VERTEX_POINT('',#36872);
#6186=VERTEX_POINT('',#36876);
#6187=VERTEX_POINT('',#36880);
#6188=VERTEX_POINT('',#36882);
#6189=VERTEX_POINT('',#36886);
#6190=VERTEX_POINT('',#36890);
#6191=VERTEX_POINT('',#36895);
#6192=VERTEX_POINT('',#36899);
#6193=VERTEX_POINT('',#36901);
#6194=VERTEX_POINT('',#36905);
#6195=VERTEX_POINT('',#36911);
#6196=VERTEX_POINT('',#36913);
#6197=VERTEX_POINT('',#36917);
#6198=VERTEX_POINT('',#36923);
#6199=VERTEX_POINT('',#36925);
#6200=VERTEX_POINT('',#36929);
#6201=VERTEX_POINT('',#36935);
#6202=VERTEX_POINT('',#36937);
#6203=VERTEX_POINT('',#36941);
#6204=VERTEX_POINT('',#36947);
#6205=VERTEX_POINT('',#36949);
#6206=VERTEX_POINT('',#36953);
#6207=VERTEX_POINT('',#36959);
#6208=VERTEX_POINT('',#36961);
#6209=VERTEX_POINT('',#36965);
#6210=VERTEX_POINT('',#36971);
#6211=VERTEX_POINT('',#36973);
#6212=VERTEX_POINT('',#36977);
#6213=VERTEX_POINT('',#36983);
#6214=VERTEX_POINT('',#36985);
#6215=VERTEX_POINT('',#36989);
#6216=VERTEX_POINT('',#36995);
#6217=VERTEX_POINT('',#36997);
#6218=VERTEX_POINT('',#37001);
#6219=VERTEX_POINT('',#37007);
#6220=VERTEX_POINT('',#37009);
#6221=VERTEX_POINT('',#37013);
#6222=VERTEX_POINT('',#37019);
#6223=VERTEX_POINT('',#37021);
#6224=VERTEX_POINT('',#37025);
#6225=VERTEX_POINT('',#37031);
#6226=VERTEX_POINT('',#37033);
#6227=VERTEX_POINT('',#37037);
#6228=VERTEX_POINT('',#37043);
#6229=VERTEX_POINT('',#37045);
#6230=VERTEX_POINT('',#37049);
#6231=VERTEX_POINT('',#37055);
#6232=VERTEX_POINT('',#37057);
#6233=VERTEX_POINT('',#37061);
#6234=VERTEX_POINT('',#37067);
#6235=VERTEX_POINT('',#37069);
#6236=VERTEX_POINT('',#37073);
#6237=VERTEX_POINT('',#37079);
#6238=VERTEX_POINT('',#37081);
#6239=VERTEX_POINT('',#37085);
#6240=VERTEX_POINT('',#37091);
#6241=VERTEX_POINT('',#37093);
#6242=VERTEX_POINT('',#37097);
#6243=VERTEX_POINT('',#37101);
#6244=VERTEX_POINT('',#37105);
#6245=VERTEX_POINT('',#37107);
#6246=VERTEX_POINT('',#37111);
#6247=VERTEX_POINT('',#37117);
#6248=VERTEX_POINT('',#37119);
#6249=VERTEX_POINT('',#37123);
#6250=VERTEX_POINT('',#37129);
#6251=VERTEX_POINT('',#37131);
#6252=VERTEX_POINT('',#37135);
#6253=VERTEX_POINT('',#37141);
#6254=VERTEX_POINT('',#37143);
#6255=VERTEX_POINT('',#37147);
#6256=VERTEX_POINT('',#37153);
#6257=VERTEX_POINT('',#37155);
#6258=VERTEX_POINT('',#37159);
#6259=VERTEX_POINT('',#37165);
#6260=VERTEX_POINT('',#37167);
#6261=VERTEX_POINT('',#37171);
#6262=VERTEX_POINT('',#37177);
#6263=VERTEX_POINT('',#37179);
#6264=VERTEX_POINT('',#37183);
#6265=VERTEX_POINT('',#37189);
#6266=VERTEX_POINT('',#37191);
#6267=VERTEX_POINT('',#37195);
#6268=VERTEX_POINT('',#37201);
#6269=VERTEX_POINT('',#37203);
#6270=VERTEX_POINT('',#37207);
#6271=VERTEX_POINT('',#37213);
#6272=VERTEX_POINT('',#37215);
#6273=VERTEX_POINT('',#37219);
#6274=VERTEX_POINT('',#37225);
#6275=VERTEX_POINT('',#37227);
#6276=VERTEX_POINT('',#37231);
#6277=VERTEX_POINT('',#37237);
#6278=VERTEX_POINT('',#37239);
#6279=VERTEX_POINT('',#37243);
#6280=VERTEX_POINT('',#37249);
#6281=VERTEX_POINT('',#37251);
#6282=VERTEX_POINT('',#37255);
#6283=VERTEX_POINT('',#37261);
#6284=VERTEX_POINT('',#37263);
#6285=VERTEX_POINT('',#37267);
#6286=VERTEX_POINT('',#37273);
#6287=VERTEX_POINT('',#37275);
#6288=VERTEX_POINT('',#37279);
#6289=VERTEX_POINT('',#37285);
#6290=VERTEX_POINT('',#37287);
#6291=VERTEX_POINT('',#37291);
#6292=VERTEX_POINT('',#37297);
#6293=VERTEX_POINT('',#37299);
#6294=VERTEX_POINT('',#37303);
#6295=VERTEX_POINT('',#37309);
#6296=VERTEX_POINT('',#37311);
#6297=VERTEX_POINT('',#37315);
#6298=VERTEX_POINT('',#37323);
#6299=VERTEX_POINT('',#37324);
#6300=VERTEX_POINT('',#37326);
#6301=VERTEX_POINT('',#37328);
#6302=VERTEX_POINT('',#37330);
#6303=VERTEX_POINT('',#37332);
#6304=VERTEX_POINT('',#37336);
#6305=VERTEX_POINT('',#37337);
#6306=VERTEX_POINT('',#37341);
#6307=VERTEX_POINT('',#37345);
#6308=VERTEX_POINT('',#37349);
#6309=VERTEX_POINT('',#37353);
#6310=VERTEX_POINT('',#37360);
#6311=VERTEX_POINT('',#37376);
#6312=VERTEX_POINT('',#37377);
#6313=VERTEX_POINT('',#37379);
#6314=VERTEX_POINT('',#37510);
#6315=VERTEX_POINT('',#37598);
#6316=VERTEX_POINT('',#37599);
#6317=VERTEX_POINT('',#37601);
#6318=VERTEX_POINT('',#37793);
#6319=VERTEX_POINT('',#38013);
#6320=VERTEX_POINT('',#38014);
#6321=VERTEX_POINT('',#38016);
#6322=VERTEX_POINT('',#38449);
#6323=VERTEX_POINT('',#38450);
#6324=VERTEX_POINT('',#38680);
#6325=VERTEX_POINT('',#38910);
#6326=VERTEX_POINT('',#38911);
#6327=VERTEX_POINT('',#38913);
#6328=VERTEX_POINT('',#39449);
#6329=VERTEX_POINT('',#39450);
#6330=VERTEX_POINT('',#39686);
#6331=VERTEX_POINT('',#39912);
#6332=VERTEX_POINT('',#39913);
#6333=VERTEX_POINT('',#39915);
#6334=VERTEX_POINT('',#40415);
#6335=VERTEX_POINT('',#40416);
#6336=VERTEX_POINT('',#40634);
#6337=VERTEX_POINT('',#40892);
#6338=VERTEX_POINT('',#40893);
#6339=VERTEX_POINT('',#40895);
#6340=VERTEX_POINT('',#41351);
#6341=VERTEX_POINT('',#41352);
#6342=VERTEX_POINT('',#41562);
#6343=VERTEX_POINT('',#41794);
#6344=VERTEX_POINT('',#41795);
#6345=VERTEX_POINT('',#41797);
#6346=VERTEX_POINT('',#42253);
#6347=VERTEX_POINT('',#42254);
#6348=VERTEX_POINT('',#42484);
#6349=VERTEX_POINT('',#42722);
#6350=VERTEX_POINT('',#42723);
#6351=VERTEX_POINT('',#42725);
#6352=VERTEX_POINT('',#43179);
#6353=VERTEX_POINT('',#43180);
#6354=VERTEX_POINT('',#43408);
#6355=VERTEX_POINT('',#43628);
#6356=VERTEX_POINT('',#43629);
#6357=VERTEX_POINT('',#43631);
#6358=VERTEX_POINT('',#44091);
#6359=VERTEX_POINT('',#44092);
#6360=VERTEX_POINT('',#44306);
#6361=VERTEX_POINT('',#44528);
#6362=VERTEX_POINT('',#44529);
#6363=VERTEX_POINT('',#44531);
#6364=VERTEX_POINT('',#45009);
#6365=VERTEX_POINT('',#45010);
#6366=VERTEX_POINT('',#45228);
#6367=VERTEX_POINT('',#45500);
#6368=VERTEX_POINT('',#45501);
#6369=VERTEX_POINT('',#45503);
#6370=VERTEX_POINT('',#45945);
#6371=VERTEX_POINT('',#45946);
#6372=VERTEX_POINT('',#46178);
#6373=VERTEX_POINT('',#46414);
#6374=VERTEX_POINT('',#46415);
#6375=VERTEX_POINT('',#46417);
#6376=VERTEX_POINT('',#46840);
#6377=VERTEX_POINT('',#46841);
#6378=VERTEX_POINT('',#46843);
#6379=VERTEX_POINT('',#47066);
#6380=VERTEX_POINT('',#47340);
#6381=VERTEX_POINT('',#47341);
#6382=VERTEX_POINT('',#47792);
#6383=VERTEX_POINT('',#47793);
#6384=VERTEX_POINT('',#47795);
#6385=VERTEX_POINT('',#48024);
#6386=VERTEX_POINT('',#48243);
#6387=VERTEX_POINT('',#48244);
#6388=VERTEX_POINT('',#48476);
#6389=VERTEX_POINT('',#48695);
#6390=VERTEX_POINT('',#48696);
#6391=VERTEX_POINT('',#48698);
#6392=VERTEX_POINT('',#49202);
#6393=VERTEX_POINT('',#49203);
#6394=VERTEX_POINT('',#49431);
#6395=VERTEX_POINT('',#49636);
#6396=VERTEX_POINT('',#49637);
#6397=VERTEX_POINT('',#49705);
#6398=VERTEX_POINT('',#49707);
#6399=VERTEX_POINT('',#49713);
#6400=VERTEX_POINT('',#49904);
#6401=VERTEX_POINT('',#50098);
#6402=VERTEX_POINT('',#50292);
#6403=VERTEX_POINT('',#50483);
#6404=VERTEX_POINT('',#50494);
#6405=VERTEX_POINT('',#50505);
#6406=VERTEX_POINT('',#50517);
#6407=VERTEX_POINT('',#50528);
#6408=VERTEX_POINT('',#50539);
#6409=VERTEX_POINT('',#50551);
#6410=VERTEX_POINT('',#50562);
#6411=VERTEX_POINT('',#50573);
#6412=VERTEX_POINT('',#50764);
#6413=VERTEX_POINT('',#50958);
#6414=VERTEX_POINT('',#51149);
#6415=VERTEX_POINT('',#51340);
#6416=VERTEX_POINT('',#51531);
#6417=VERTEX_POINT('',#51725);
#6418=VERTEX_POINT('',#51916);
#6419=VERTEX_POINT('',#52110);
#6420=VERTEX_POINT('',#52304);
#6421=VERTEX_POINT('',#52495);
#6422=VERTEX_POINT('',#52689);
#6423=VERTEX_POINT('',#52880);
#6424=VERTEX_POINT('',#53074);
#6425=VERTEX_POINT('',#53265);
#6426=VERTEX_POINT('',#53276);
#6427=VERTEX_POINT('',#53293);
#6428=VERTEX_POINT('',#53295);
#6429=VERTEX_POINT('',#53297);
#6430=VERTEX_POINT('',#53473);
#6431=VERTEX_POINT('',#53664);
#6432=VERTEX_POINT('',#53855);
#6433=VERTEX_POINT('',#54049);
#6434=VERTEX_POINT('',#54240);
#6435=VERTEX_POINT('',#54434);
#6436=VERTEX_POINT('',#54628);
#6437=VERTEX_POINT('',#54819);
#6438=VERTEX_POINT('',#55013);
#6439=VERTEX_POINT('',#55204);
#6440=VERTEX_POINT('',#55215);
#6441=VERTEX_POINT('',#55227);
#6442=VERTEX_POINT('',#55238);
#6443=VERTEX_POINT('',#55249);
#6444=VERTEX_POINT('',#55261);
#6445=VERTEX_POINT('',#55272);
#6446=VERTEX_POINT('',#55283);
#6447=VERTEX_POINT('',#55295);
#6448=VERTEX_POINT('',#55306);
#6449=VERTEX_POINT('',#55500);
#6450=VERTEX_POINT('',#55691);
#6451=VERTEX_POINT('',#55885);
#6452=VERTEX_POINT('',#56076);
#6453=VERTEX_POINT('',#56270);
#6454=VERTEX_POINT('',#56461);
#6455=VERTEX_POINT('',#56849);
#6456=VERTEX_POINT('',#56890);
#6457=VERTEX_POINT('',#57009);
#6458=VERTEX_POINT('',#57011);
#6459=VERTEX_POINT('',#57140);
#6460=VERTEX_POINT('',#58095);
#6461=VERTEX_POINT('',#58096);
#6462=VERTEX_POINT('',#58894);
#6463=VERTEX_POINT('',#58898);
#6464=VERTEX_POINT('',#58901);
#6465=VERTEX_POINT('',#58906);
#6466=VERTEX_POINT('',#58907);
#6467=VERTEX_POINT('',#58909);
#6468=VERTEX_POINT('',#58911);
#6469=VERTEX_POINT('',#58917);
#6470=VERTEX_POINT('',#58921);
#6471=VERTEX_POINT('',#58927);
#6472=VERTEX_POINT('',#58928);
#6473=VERTEX_POINT('',#58932);
#6474=VERTEX_POINT('',#58934);
#6475=VERTEX_POINT('',#58938);
#6476=VERTEX_POINT('',#58942);
#6477=VERTEX_POINT('',#58944);
#6478=VERTEX_POINT('',#58948);
#6479=VERTEX_POINT('',#58952);
#6480=VERTEX_POINT('',#58954);
#6481=VERTEX_POINT('',#58958);
#6482=VERTEX_POINT('',#58962);
#6483=VERTEX_POINT('',#58964);
#6484=VERTEX_POINT('',#58968);
#6485=VERTEX_POINT('',#58972);
#6486=VERTEX_POINT('',#58974);
#6487=VERTEX_POINT('',#58978);
#6488=VERTEX_POINT('',#58982);
#6489=VERTEX_POINT('',#58984);
#6490=VERTEX_POINT('',#58988);
#6491=VERTEX_POINT('',#58992);
#6492=VERTEX_POINT('',#58994);
#6493=VERTEX_POINT('',#58998);
#6494=VERTEX_POINT('',#59002);
#6495=VERTEX_POINT('',#59004);
#6496=VERTEX_POINT('',#59008);
#6497=VERTEX_POINT('',#59012);
#6498=VERTEX_POINT('',#59014);
#6499=VERTEX_POINT('',#59018);
#6500=VERTEX_POINT('',#59022);
#6501=VERTEX_POINT('',#59024);
#6502=VERTEX_POINT('',#59028);
#6503=VERTEX_POINT('',#59032);
#6504=VERTEX_POINT('',#59034);
#6505=VERTEX_POINT('',#59038);
#6506=VERTEX_POINT('',#59042);
#6507=VERTEX_POINT('',#59044);
#6508=VERTEX_POINT('',#59048);
#6509=VERTEX_POINT('',#59052);
#6510=VERTEX_POINT('',#59054);
#6511=VERTEX_POINT('',#59058);
#6512=VERTEX_POINT('',#59062);
#6513=VERTEX_POINT('',#59064);
#6514=VERTEX_POINT('',#59068);
#6515=VERTEX_POINT('',#59072);
#6516=VERTEX_POINT('',#59074);
#6517=VERTEX_POINT('',#59078);
#6518=VERTEX_POINT('',#59082);
#6519=VERTEX_POINT('',#59084);
#6520=VERTEX_POINT('',#59088);
#6521=VERTEX_POINT('',#59092);
#6522=VERTEX_POINT('',#59094);
#6523=VERTEX_POINT('',#59098);
#6524=VERTEX_POINT('',#59102);
#6525=VERTEX_POINT('',#59104);
#6526=VERTEX_POINT('',#59108);
#6527=VERTEX_POINT('',#59113);
#6528=VERTEX_POINT('',#59115);
#6529=VERTEX_POINT('',#59119);
#6530=VERTEX_POINT('',#59123);
#6531=VERTEX_POINT('',#59125);
#6532=VERTEX_POINT('',#59129);
#6533=VERTEX_POINT('',#59133);
#6534=VERTEX_POINT('',#59135);
#6535=VERTEX_POINT('',#59139);
#6536=VERTEX_POINT('',#59143);
#6537=VERTEX_POINT('',#59145);
#6538=VERTEX_POINT('',#59149);
#6539=VERTEX_POINT('',#59153);
#6540=VERTEX_POINT('',#59155);
#6541=VERTEX_POINT('',#59159);
#6542=VERTEX_POINT('',#59163);
#6543=VERTEX_POINT('',#59165);
#6544=VERTEX_POINT('',#59169);
#6545=VERTEX_POINT('',#59173);
#6546=VERTEX_POINT('',#59175);
#6547=VERTEX_POINT('',#59179);
#6548=VERTEX_POINT('',#59183);
#6549=VERTEX_POINT('',#59185);
#6550=VERTEX_POINT('',#59189);
#6551=VERTEX_POINT('',#59193);
#6552=VERTEX_POINT('',#59195);
#6553=VERTEX_POINT('',#59199);
#6554=VERTEX_POINT('',#59203);
#6555=VERTEX_POINT('',#59205);
#6556=VERTEX_POINT('',#59209);
#6557=VERTEX_POINT('',#59213);
#6558=VERTEX_POINT('',#59215);
#6559=VERTEX_POINT('',#59219);
#6560=VERTEX_POINT('',#59223);
#6561=VERTEX_POINT('',#59225);
#6562=VERTEX_POINT('',#59229);
#6563=VERTEX_POINT('',#59233);
#6564=VERTEX_POINT('',#59235);
#6565=VERTEX_POINT('',#59239);
#6566=VERTEX_POINT('',#59243);
#6567=VERTEX_POINT('',#59245);
#6568=VERTEX_POINT('',#59249);
#6569=VERTEX_POINT('',#59253);
#6570=VERTEX_POINT('',#59255);
#6571=VERTEX_POINT('',#59259);
#6572=VERTEX_POINT('',#59263);
#6573=VERTEX_POINT('',#59265);
#6574=VERTEX_POINT('',#59269);
#6575=VERTEX_POINT('',#59273);
#6576=VERTEX_POINT('',#59278);
#6577=VERTEX_POINT('',#59282);
#6578=VERTEX_POINT('',#59283);
#6579=VERTEX_POINT('',#59285);
#6580=VERTEX_POINT('',#59294);
#6581=VERTEX_POINT('',#59295);
#6582=VERTEX_POINT('',#59298);
#6583=VERTEX_POINT('',#59301);
#6584=VERTEX_POINT('',#59303);
#6585=VERTEX_POINT('',#59306);
#6586=VERTEX_POINT('',#59308);
#6587=VERTEX_POINT('',#59311);
#6588=VERTEX_POINT('',#59313);
#6589=VERTEX_POINT('',#59316);
#6590=VERTEX_POINT('',#59318);
#6591=VERTEX_POINT('',#59321);
#6592=VERTEX_POINT('',#59323);
#6593=VERTEX_POINT('',#59326);
#6594=VERTEX_POINT('',#59328);
#6595=VERTEX_POINT('',#59331);
#6596=VERTEX_POINT('',#59333);
#6597=VERTEX_POINT('',#59336);
#6598=VERTEX_POINT('',#59338);
#6599=VERTEX_POINT('',#59341);
#6600=VERTEX_POINT('',#59343);
#6601=VERTEX_POINT('',#59346);
#6602=VERTEX_POINT('',#59348);
#6603=VERTEX_POINT('',#59351);
#6604=VERTEX_POINT('',#59353);
#6605=VERTEX_POINT('',#59356);
#6606=VERTEX_POINT('',#59358);
#6607=VERTEX_POINT('',#59361);
#6608=VERTEX_POINT('',#59363);
#6609=VERTEX_POINT('',#59366);
#6610=VERTEX_POINT('',#59368);
#6611=VERTEX_POINT('',#59371);
#6612=VERTEX_POINT('',#59373);
#6613=VERTEX_POINT('',#59376);
#6614=VERTEX_POINT('',#59378);
#6615=VERTEX_POINT('',#59381);
#6616=VERTEX_POINT('',#59383);
#6617=VERTEX_POINT('',#59386);
#6618=VERTEX_POINT('',#59388);
#6619=VERTEX_POINT('',#59391);
#6620=VERTEX_POINT('',#59393);
#6621=VERTEX_POINT('',#59396);
#6622=VERTEX_POINT('',#59398);
#6623=VERTEX_POINT('',#59401);
#6624=VERTEX_POINT('',#59403);
#6625=VERTEX_POINT('',#59406);
#6626=VERTEX_POINT('',#59408);
#6627=VERTEX_POINT('',#59411);
#6628=VERTEX_POINT('',#59413);
#6629=VERTEX_POINT('',#59416);
#6630=VERTEX_POINT('',#59418);
#6631=VERTEX_POINT('',#59421);
#6632=VERTEX_POINT('',#59423);
#6633=VERTEX_POINT('',#59426);
#6634=VERTEX_POINT('',#59428);
#6635=VERTEX_POINT('',#59431);
#6636=VERTEX_POINT('',#59433);
#6637=VERTEX_POINT('',#59436);
#6638=VERTEX_POINT('',#59438);
#6639=VERTEX_POINT('',#59441);
#6640=VERTEX_POINT('',#59443);
#6641=VERTEX_POINT('',#59446);
#6642=VERTEX_POINT('',#59448);
#6643=VERTEX_POINT('',#59451);
#6644=VERTEX_POINT('',#59453);
#6645=VERTEX_POINT('',#59456);
#6646=VERTEX_POINT('',#59458);
#6647=VERTEX_POINT('',#59461);
#6648=VERTEX_POINT('',#59463);
#6649=VERTEX_POINT('',#59468);
#6650=VERTEX_POINT('',#59475);
#6651=VERTEX_POINT('',#59482);
#6652=VERTEX_POINT('',#59489);
#6653=VERTEX_POINT('',#59496);
#6654=VERTEX_POINT('',#59503);
#6655=VERTEX_POINT('',#59510);
#6656=VERTEX_POINT('',#59517);
#6657=VERTEX_POINT('',#59524);
#6658=VERTEX_POINT('',#59531);
#6659=VERTEX_POINT('',#59538);
#6660=VERTEX_POINT('',#59545);
#6661=VERTEX_POINT('',#59552);
#6662=VERTEX_POINT('',#59559);
#6663=VERTEX_POINT('',#59566);
#6664=VERTEX_POINT('',#59573);
#6665=VERTEX_POINT('',#59580);
#6666=VERTEX_POINT('',#59587);
#6667=VERTEX_POINT('',#59594);
#6668=VERTEX_POINT('',#59601);
#6669=VERTEX_POINT('',#59608);
#6670=VERTEX_POINT('',#59615);
#6671=VERTEX_POINT('',#59622);
#6672=VERTEX_POINT('',#59629);
#6673=VERTEX_POINT('',#59636);
#6674=VERTEX_POINT('',#59643);
#6675=VERTEX_POINT('',#59650);
#6676=VERTEX_POINT('',#59657);
#6677=VERTEX_POINT('',#59664);
#6678=VERTEX_POINT('',#59671);
#6679=VERTEX_POINT('',#59678);
#6680=VERTEX_POINT('',#59685);
#6681=VERTEX_POINT('',#59692);
#6682=VERTEX_POINT('',#59699);
#6683=VERTEX_POINT('',#59706);
#6684=VERTEX_POINT('',#59707);
#6685=VERTEX_POINT('',#59709);
#6686=VERTEX_POINT('',#59711);
#6687=VERTEX_POINT('',#59713);
#6688=VERTEX_POINT('',#59715);
#6689=VERTEX_POINT('',#59719);
#6690=VERTEX_POINT('',#59720);
#6691=VERTEX_POINT('',#59724);
#6692=VERTEX_POINT('',#59728);
#6693=VERTEX_POINT('',#59732);
#6694=VERTEX_POINT('',#59736);
#6695=VERTEX_POINT('',#59743);
#6696=VERTEX_POINT('',#59759);
#6697=VERTEX_POINT('',#59760);
#6698=VERTEX_POINT('',#59762);
#6699=VERTEX_POINT('',#59917);
#6700=VERTEX_POINT('',#60032);
#6701=VERTEX_POINT('',#60033);
#6702=VERTEX_POINT('',#60035);
#6703=VERTEX_POINT('',#60233);
#6704=VERTEX_POINT('',#60432);
#6705=VERTEX_POINT('',#60433);
#6706=VERTEX_POINT('',#60623);
#6707=VERTEX_POINT('',#60648);
#6708=VERTEX_POINT('',#60649);
#6709=VERTEX_POINT('',#60651);
#6710=VERTEX_POINT('',#60680);
#6711=VERTEX_POINT('',#60870);
#6712=VERTEX_POINT('',#60871);
#6713=VERTEX_POINT('',#60873);
#6714=VERTEX_POINT('',#61253);
#6715=VERTEX_POINT('',#61254);
#6716=VERTEX_POINT('',#61450);
#6717=VERTEX_POINT('',#61638);
#6718=VERTEX_POINT('',#61639);
#6719=VERTEX_POINT('',#61641);
#6720=VERTEX_POINT('',#62095);
#6721=VERTEX_POINT('',#62096);
#6722=VERTEX_POINT('',#62370);
#6723=VERTEX_POINT('',#62578);
#6724=VERTEX_POINT('',#62579);
#6725=VERTEX_POINT('',#62581);
#6726=VERTEX_POINT('',#63073);
#6727=VERTEX_POINT('',#63074);
#6728=VERTEX_POINT('',#63274);
#6729=VERTEX_POINT('',#63304);
#6730=VERTEX_POINT('',#63305);
#6731=VERTEX_POINT('',#63307);
#6732=VERTEX_POINT('',#63326);
#6733=VERTEX_POINT('',#63541);
#6734=VERTEX_POINT('',#63542);
#6735=VERTEX_POINT('',#63544);
#6736=VERTEX_POINT('',#63912);
#6737=VERTEX_POINT('',#63913);
#6738=VERTEX_POINT('',#63915);
#6739=VERTEX_POINT('',#64380);
#6740=VERTEX_POINT('',#64381);
#6741=VERTEX_POINT('',#64762);
#6742=VERTEX_POINT('',#64763);
#6743=VERTEX_POINT('',#64834);
#6744=VERTEX_POINT('',#64836);
#6745=VERTEX_POINT('',#64842);
#6746=VERTEX_POINT('',#65054);
#6747=VERTEX_POINT('',#65065);
#6748=VERTEX_POINT('',#65274);
#6749=VERTEX_POINT('',#65486);
#6750=VERTEX_POINT('',#65698);
#6751=VERTEX_POINT('',#65710);
#6752=VERTEX_POINT('',#65919);
#6753=VERTEX_POINT('',#66128);
#6754=VERTEX_POINT('',#66140);
#6755=VERTEX_POINT('',#66349);
#6756=VERTEX_POINT('',#66558);
#6757=VERTEX_POINT('',#66770);
#6758=VERTEX_POINT('',#66781);
#6759=VERTEX_POINT('',#66993);
#6760=VERTEX_POINT('',#67070);
#6761=VERTEX_POINT('',#67072);
#6762=VERTEX_POINT('',#67078);
#6763=VERTEX_POINT('',#67089);
#6764=VERTEX_POINT('',#67298);
#6765=VERTEX_POINT('',#67510);
#6766=VERTEX_POINT('',#67521);
#6767=VERTEX_POINT('',#67730);
#6768=VERTEX_POINT('',#67942);
#6769=VERTEX_POINT('',#68154);
#6770=VERTEX_POINT('',#68165);
#6771=VERTEX_POINT('',#68377);
#6772=VERTEX_POINT('',#68589);
#6773=VERTEX_POINT('',#68600);
#6774=VERTEX_POINT('',#68809);
#6775=VERTEX_POINT('',#69227);
#6776=VERTEX_POINT('',#69406);
#6777=VERTEX_POINT('',#69408);
#6778=VERTEX_POINT('',#69555);
#6779=VERTEX_POINT('',#69556);
#6780=VERTEX_POINT('',#69652);
#6781=VERTEX_POINT('',#70227);
#6782=VERTEX_POINT('',#70228);
#6783=VERTEX_POINT('',#70715);
#6784=VERTEX_POINT('',#70719);
#6785=VERTEX_POINT('',#70722);
#6786=VERTEX_POINT('',#70727);
#6787=VERTEX_POINT('',#70728);
#6788=VERTEX_POINT('',#70730);
#6789=VERTEX_POINT('',#70732);
#6790=VERTEX_POINT('',#70738);
#6791=VERTEX_POINT('',#70739);
#6792=VERTEX_POINT('',#70748);
#6793=VERTEX_POINT('',#70749);
#6794=VERTEX_POINT('',#70753);
#6795=VERTEX_POINT('',#70755);
#6796=VERTEX_POINT('',#70759);
#6797=VERTEX_POINT('',#70763);
#6798=VERTEX_POINT('',#70765);
#6799=VERTEX_POINT('',#70769);
#6800=VERTEX_POINT('',#70773);
#6801=VERTEX_POINT('',#70775);
#6802=VERTEX_POINT('',#70779);
#6803=VERTEX_POINT('',#70783);
#6804=VERTEX_POINT('',#70785);
#6805=VERTEX_POINT('',#70789);
#6806=VERTEX_POINT('',#70793);
#6807=VERTEX_POINT('',#70795);
#6808=VERTEX_POINT('',#70799);
#6809=VERTEX_POINT('',#70803);
#6810=VERTEX_POINT('',#70805);
#6811=VERTEX_POINT('',#70809);
#6812=VERTEX_POINT('',#70813);
#6813=VERTEX_POINT('',#70815);
#6814=VERTEX_POINT('',#70819);
#6815=VERTEX_POINT('',#70823);
#6816=VERTEX_POINT('',#70825);
#6817=VERTEX_POINT('',#70829);
#6818=VERTEX_POINT('',#70833);
#6819=VERTEX_POINT('',#70835);
#6820=VERTEX_POINT('',#70839);
#6821=VERTEX_POINT('',#70843);
#6822=VERTEX_POINT('',#70845);
#6823=VERTEX_POINT('',#70849);
#6824=VERTEX_POINT('',#70853);
#6825=VERTEX_POINT('',#70855);
#6826=VERTEX_POINT('',#70859);
#6827=VERTEX_POINT('',#70863);
#6828=VERTEX_POINT('',#70865);
#6829=VERTEX_POINT('',#70869);
#6830=VERTEX_POINT('',#70873);
#6831=VERTEX_POINT('',#70875);
#6832=VERTEX_POINT('',#70879);
#6833=VERTEX_POINT('',#70883);
#6834=VERTEX_POINT('',#70885);
#6835=VERTEX_POINT('',#70889);
#6836=VERTEX_POINT('',#70893);
#6837=VERTEX_POINT('',#70895);
#6838=VERTEX_POINT('',#70899);
#6839=VERTEX_POINT('',#70903);
#6840=VERTEX_POINT('',#70905);
#6841=VERTEX_POINT('',#70909);
#6842=VERTEX_POINT('',#70913);
#6843=VERTEX_POINT('',#70915);
#6844=VERTEX_POINT('',#70919);
#6845=VERTEX_POINT('',#70923);
#6846=VERTEX_POINT('',#70925);
#6847=VERTEX_POINT('',#70929);
#6848=VERTEX_POINT('',#70934);
#6849=VERTEX_POINT('',#70936);
#6850=VERTEX_POINT('',#70940);
#6851=VERTEX_POINT('',#70944);
#6852=VERTEX_POINT('',#70946);
#6853=VERTEX_POINT('',#70950);
#6854=VERTEX_POINT('',#70954);
#6855=VERTEX_POINT('',#70956);
#6856=VERTEX_POINT('',#70960);
#6857=VERTEX_POINT('',#70964);
#6858=VERTEX_POINT('',#70966);
#6859=VERTEX_POINT('',#70970);
#6860=VERTEX_POINT('',#70974);
#6861=VERTEX_POINT('',#70976);
#6862=VERTEX_POINT('',#70980);
#6863=VERTEX_POINT('',#70984);
#6864=VERTEX_POINT('',#70986);
#6865=VERTEX_POINT('',#70990);
#6866=VERTEX_POINT('',#70994);
#6867=VERTEX_POINT('',#70996);
#6868=VERTEX_POINT('',#71000);
#6869=VERTEX_POINT('',#71004);
#6870=VERTEX_POINT('',#71006);
#6871=VERTEX_POINT('',#71010);
#6872=VERTEX_POINT('',#71014);
#6873=VERTEX_POINT('',#71016);
#6874=VERTEX_POINT('',#71020);
#6875=VERTEX_POINT('',#71024);
#6876=VERTEX_POINT('',#71026);
#6877=VERTEX_POINT('',#71030);
#6878=VERTEX_POINT('',#71034);
#6879=VERTEX_POINT('',#71036);
#6880=VERTEX_POINT('',#71040);
#6881=VERTEX_POINT('',#71044);
#6882=VERTEX_POINT('',#71046);
#6883=VERTEX_POINT('',#71050);
#6884=VERTEX_POINT('',#71054);
#6885=VERTEX_POINT('',#71056);
#6886=VERTEX_POINT('',#71060);
#6887=VERTEX_POINT('',#71064);
#6888=VERTEX_POINT('',#71066);
#6889=VERTEX_POINT('',#71070);
#6890=VERTEX_POINT('',#71074);
#6891=VERTEX_POINT('',#71076);
#6892=VERTEX_POINT('',#71080);
#6893=VERTEX_POINT('',#71084);
#6894=VERTEX_POINT('',#71086);
#6895=VERTEX_POINT('',#71090);
#6896=VERTEX_POINT('',#71094);
#6897=VERTEX_POINT('',#71099);
#6898=VERTEX_POINT('',#71103);
#6899=VERTEX_POINT('',#71105);
#6900=VERTEX_POINT('',#71109);
#6901=VERTEX_POINT('',#71115);
#6902=VERTEX_POINT('',#71117);
#6903=VERTEX_POINT('',#71121);
#6904=VERTEX_POINT('',#71127);
#6905=VERTEX_POINT('',#71129);
#6906=VERTEX_POINT('',#71133);
#6907=VERTEX_POINT('',#71139);
#6908=VERTEX_POINT('',#71141);
#6909=VERTEX_POINT('',#71145);
#6910=VERTEX_POINT('',#71151);
#6911=VERTEX_POINT('',#71153);
#6912=VERTEX_POINT('',#71157);
#6913=VERTEX_POINT('',#71163);
#6914=VERTEX_POINT('',#71165);
#6915=VERTEX_POINT('',#71169);
#6916=VERTEX_POINT('',#71175);
#6917=VERTEX_POINT('',#71177);
#6918=VERTEX_POINT('',#71181);
#6919=VERTEX_POINT('',#71187);
#6920=VERTEX_POINT('',#71189);
#6921=VERTEX_POINT('',#71193);
#6922=VERTEX_POINT('',#71199);
#6923=VERTEX_POINT('',#71201);
#6924=VERTEX_POINT('',#71205);
#6925=VERTEX_POINT('',#71211);
#6926=VERTEX_POINT('',#71213);
#6927=VERTEX_POINT('',#71217);
#6928=VERTEX_POINT('',#71223);
#6929=VERTEX_POINT('',#71225);
#6930=VERTEX_POINT('',#71229);
#6931=VERTEX_POINT('',#71235);
#6932=VERTEX_POINT('',#71237);
#6933=VERTEX_POINT('',#71241);
#6934=VERTEX_POINT('',#71247);
#6935=VERTEX_POINT('',#71249);
#6936=VERTEX_POINT('',#71253);
#6937=VERTEX_POINT('',#71259);
#6938=VERTEX_POINT('',#71261);
#6939=VERTEX_POINT('',#71265);
#6940=VERTEX_POINT('',#71271);
#6941=VERTEX_POINT('',#71273);
#6942=VERTEX_POINT('',#71277);
#6943=VERTEX_POINT('',#71283);
#6944=VERTEX_POINT('',#71285);
#6945=VERTEX_POINT('',#71289);
#6946=VERTEX_POINT('',#71295);
#6947=VERTEX_POINT('',#71297);
#6948=VERTEX_POINT('',#71301);
#6949=VERTEX_POINT('',#71305);
#6950=VERTEX_POINT('',#71309);
#6951=VERTEX_POINT('',#71311);
#6952=VERTEX_POINT('',#71315);
#6953=VERTEX_POINT('',#71321);
#6954=VERTEX_POINT('',#71323);
#6955=VERTEX_POINT('',#71327);
#6956=VERTEX_POINT('',#71333);
#6957=VERTEX_POINT('',#71335);
#6958=VERTEX_POINT('',#71339);
#6959=VERTEX_POINT('',#71345);
#6960=VERTEX_POINT('',#71347);
#6961=VERTEX_POINT('',#71351);
#6962=VERTEX_POINT('',#71357);
#6963=VERTEX_POINT('',#71359);
#6964=VERTEX_POINT('',#71363);
#6965=VERTEX_POINT('',#71369);
#6966=VERTEX_POINT('',#71371);
#6967=VERTEX_POINT('',#71375);
#6968=VERTEX_POINT('',#71381);
#6969=VERTEX_POINT('',#71383);
#6970=VERTEX_POINT('',#71387);
#6971=VERTEX_POINT('',#71393);
#6972=VERTEX_POINT('',#71395);
#6973=VERTEX_POINT('',#71399);
#6974=VERTEX_POINT('',#71405);
#6975=VERTEX_POINT('',#71407);
#6976=VERTEX_POINT('',#71411);
#6977=VERTEX_POINT('',#71417);
#6978=VERTEX_POINT('',#71419);
#6979=VERTEX_POINT('',#71423);
#6980=VERTEX_POINT('',#71429);
#6981=VERTEX_POINT('',#71431);
#6982=VERTEX_POINT('',#71435);
#6983=VERTEX_POINT('',#71441);
#6984=VERTEX_POINT('',#71443);
#6985=VERTEX_POINT('',#71447);
#6986=VERTEX_POINT('',#71453);
#6987=VERTEX_POINT('',#71455);
#6988=VERTEX_POINT('',#71459);
#6989=VERTEX_POINT('',#71465);
#6990=VERTEX_POINT('',#71467);
#6991=VERTEX_POINT('',#71471);
#6992=VERTEX_POINT('',#71477);
#6993=VERTEX_POINT('',#71479);
#6994=VERTEX_POINT('',#71483);
#6995=VERTEX_POINT('',#71489);
#6996=VERTEX_POINT('',#71491);
#6997=VERTEX_POINT('',#71495);
#6998=VERTEX_POINT('',#71501);
#6999=VERTEX_POINT('',#71503);
#7000=VERTEX_POINT('',#71507);
#7001=VERTEX_POINT('',#71513);
#7002=VERTEX_POINT('',#71515);
#7003=VERTEX_POINT('',#71519);
#7004=VERTEX_POINT('',#71527);
#7005=VERTEX_POINT('',#71528);
#7006=VERTEX_POINT('',#71530);
#7007=VERTEX_POINT('',#71532);
#7008=VERTEX_POINT('',#71534);
#7009=VERTEX_POINT('',#71536);
#7010=VERTEX_POINT('',#71540);
#7011=VERTEX_POINT('',#71541);
#7012=VERTEX_POINT('',#71545);
#7013=VERTEX_POINT('',#71549);
#7014=VERTEX_POINT('',#71553);
#7015=VERTEX_POINT('',#71557);
#7016=VERTEX_POINT('',#71564);
#7017=EDGE_CURVE('',#5666,#5666,#5660,.T.);
#7018=EDGE_CURVE('',#5666,#5667,#3838,.T.);
#7019=EDGE_CURVE('',#5667,#5667,#3404,.T.);
#7020=EDGE_CURVE('',#5668,#5668,#3405,.T.);
#7021=EDGE_CURVE('',#5668,#5669,#3839,.T.);
#7022=EDGE_CURVE('',#5670,#5669,#1103,.T.);
#7023=EDGE_CURVE('',#5669,#5670,#1104,.T.);
#7024=EDGE_CURVE('',#5671,#5671,#5661,.T.);
#7025=EDGE_CURVE('',#5671,#5672,#3840,.T.);
#7026=EDGE_CURVE('',#5672,#5672,#3406,.T.);
#7027=EDGE_CURVE('',#5673,#5673,#3407,.T.);
#7028=EDGE_CURVE('',#5673,#5674,#3841,.T.);
#7029=EDGE_CURVE('',#5675,#5674,#1105,.T.);
#7030=EDGE_CURVE('',#5674,#5675,#1106,.T.);
#7031=EDGE_CURVE('',#5676,#5676,#5662,.T.);
#7032=EDGE_CURVE('',#5676,#5677,#3842,.T.);
#7033=EDGE_CURVE('',#5677,#5677,#3408,.T.);
#7034=EDGE_CURVE('',#5678,#5678,#3409,.T.);
#7035=EDGE_CURVE('',#5678,#5679,#3843,.T.);
#7036=EDGE_CURVE('',#5680,#5679,#1107,.T.);
#7037=EDGE_CURVE('',#5679,#5680,#1108,.T.);
#7038=EDGE_CURVE('',#5681,#5681,#5663,.T.);
#7039=EDGE_CURVE('',#5681,#5682,#3844,.T.);
#7040=EDGE_CURVE('',#5682,#5682,#3410,.T.);
#7041=EDGE_CURVE('',#5683,#5683,#3411,.T.);
#7042=EDGE_CURVE('',#5683,#5684,#3845,.T.);
#7043=EDGE_CURVE('',#5685,#5684,#1109,.T.);
#7044=EDGE_CURVE('',#5684,#5685,#1110,.T.);
#7045=EDGE_CURVE('',#5686,#5686,#5664,.T.);
#7046=EDGE_CURVE('',#5686,#5687,#3846,.T.);
#7047=EDGE_CURVE('',#5687,#5687,#3412,.T.);
#7048=EDGE_CURVE('',#5688,#5688,#3413,.T.);
#7049=EDGE_CURVE('',#5688,#5689,#3847,.T.);
#7050=EDGE_CURVE('',#5690,#5689,#1111,.T.);
#7051=EDGE_CURVE('',#5689,#5690,#1112,.T.);
#7052=EDGE_CURVE('',#5691,#5691,#5665,.T.);
#7053=EDGE_CURVE('',#5691,#5692,#3848,.T.);
#7054=EDGE_CURVE('',#5692,#5692,#3414,.T.);
#7055=EDGE_CURVE('',#5693,#5693,#3415,.T.);
#7056=EDGE_CURVE('',#5693,#5694,#3849,.T.);
#7057=EDGE_CURVE('',#5695,#5694,#1113,.T.);
#7058=EDGE_CURVE('',#5694,#5695,#1114,.T.);
#7059=EDGE_CURVE('',#5696,#5696,#3416,.T.);
#7060=EDGE_CURVE('',#5696,#5697,#3850,.T.);
#7061=EDGE_CURVE('',#5697,#5697,#3417,.T.);
#7062=EDGE_CURVE('',#5698,#5699,#3851,.T.);
#7063=EDGE_CURVE('',#5699,#5700,#3852,.T.);
#7064=EDGE_CURVE('',#5701,#5700,#3853,.T.);
#7065=EDGE_CURVE('',#5698,#5701,#3854,.T.);
#7066=EDGE_CURVE('',#5702,#5702,#3418,.T.);
#7067=EDGE_CURVE('',#5703,#5703,#3419,.T.);
#7068=EDGE_CURVE('',#5704,#5704,#3420,.T.);
#7069=EDGE_CURVE('',#5696,#5705,#3855,.T.);
#7070=EDGE_CURVE('',#5705,#5705,#3421,.T.);
#7071=EDGE_CURVE('',#5706,#5706,#3422,.T.);
#7072=EDGE_CURVE('',#5706,#5702,#3856,.T.);
#7073=EDGE_CURVE('',#5706,#5707,#3857,.T.);
#7074=EDGE_CURVE('',#5707,#5707,#3423,.T.);
#7075=EDGE_CURVE('',#5708,#5708,#3424,.T.);
#7076=EDGE_CURVE('',#5708,#5704,#3858,.T.);
#7077=EDGE_CURVE('',#5708,#5709,#3859,.T.);
#7078=EDGE_CURVE('',#5709,#5709,#3425,.T.);
#7079=EDGE_CURVE('',#5710,#5710,#3426,.T.);
#7080=EDGE_CURVE('',#5710,#5703,#3860,.T.);
#7081=EDGE_CURVE('',#5710,#5711,#3861,.T.);
#7082=EDGE_CURVE('',#5711,#5711,#3427,.T.);
#7083=EDGE_CURVE('',#5712,#5712,#3428,.T.);
#7084=EDGE_CURVE('',#5713,#5713,#3429,.T.);
#7085=EDGE_CURVE('',#5714,#5714,#3430,.T.);
#7086=EDGE_CURVE('',#5715,#5715,#3431,.T.);
#7087=EDGE_CURVE('',#5712,#5716,#3862,.T.);
#7088=EDGE_CURVE('',#5716,#5716,#3432,.T.);
#7089=EDGE_CURVE('',#5713,#5717,#3863,.T.);
#7090=EDGE_CURVE('',#5717,#5717,#3433,.T.);
#7091=EDGE_CURVE('',#5714,#5718,#3864,.T.);
#7092=EDGE_CURVE('',#5718,#5718,#3434,.T.);
#7093=EDGE_CURVE('',#5715,#5719,#3865,.T.);
#7094=EDGE_CURVE('',#5719,#5719,#3435,.T.);
#7095=EDGE_CURVE('',#5720,#5721,#3866,.T.);
#7096=EDGE_CURVE('',#5721,#5722,#3867,.T.);
#7097=EDGE_CURVE('',#5722,#5723,#3868,.T.);
#7098=EDGE_CURVE('',#5723,#5720,#3869,.T.);
#7099=EDGE_CURVE('',#5723,#5698,#3870,.T.);
#7100=EDGE_CURVE('',#5720,#5701,#3871,.T.);
#7101=EDGE_CURVE('',#5724,#5722,#3872,.T.);
#7102=EDGE_CURVE('',#5725,#5724,#3873,.T.);
#7103=EDGE_CURVE('',#5725,#5726,#3436,.T.);
#7104=EDGE_CURVE('',#5727,#5726,#3874,.T.);
#7105=EDGE_CURVE('',#5728,#5727,#3875,.T.);
#7106=EDGE_CURVE('',#5729,#5728,#3876,.T.);
#7107=EDGE_CURVE('',#5729,#5730,#3877,.T.);
#7108=EDGE_CURVE('',#5731,#5730,#3878,.T.);
#7109=EDGE_CURVE('',#5731,#5732,#3879,.T.);
#7110=EDGE_CURVE('',#5732,#5733,#3880,.T.);
#7111=EDGE_CURVE('',#5733,#5734,#3437,.T.);
#7112=EDGE_CURVE('',#5734,#5735,#3881,.T.);
#7113=EDGE_CURVE('',#5735,#5736,#3882,.T.);
#7114=EDGE_CURVE('',#5737,#5736,#3883,.T.);
#7115=EDGE_CURVE('',#5737,#5699,#3884,.T.);
#7116=EDGE_CURVE('',#5738,#5739,#3885,.T.);
#7117=EDGE_CURVE('',#5739,#5737,#3886,.T.);
#7118=EDGE_CURVE('',#5736,#5738,#3887,.T.);
#7119=EDGE_CURVE('',#5735,#5740,#3888,.T.);
#7120=EDGE_CURVE('',#5738,#5740,#3889,.T.);
#7121=EDGE_CURVE('',#5741,#5742,#3890,.T.);
#7122=EDGE_CURVE('',#5742,#5731,#3891,.T.);
#7123=EDGE_CURVE('',#5730,#5741,#3892,.T.);
#7124=EDGE_CURVE('',#5743,#5729,#3893,.T.);
#7125=EDGE_CURVE('',#5741,#5743,#3894,.T.);
#7126=EDGE_CURVE('',#5744,#5743,#3895,.T.);
#7127=EDGE_CURVE('',#5728,#5744,#3896,.T.);
#7128=EDGE_CURVE('',#5725,#5745,#3897,.T.);
#7129=EDGE_CURVE('',#5746,#5745,#3438,.T.);
#7130=EDGE_CURVE('',#5726,#5746,#3898,.T.);
#7131=EDGE_CURVE('',#5747,#5746,#3899,.T.);
#7132=EDGE_CURVE('',#5727,#5747,#3900,.T.);
#7133=EDGE_CURVE('',#5744,#5747,#3901,.T.);
#7134=EDGE_CURVE('',#5748,#5742,#3902,.T.);
#7135=EDGE_CURVE('',#5732,#5748,#3903,.T.);
#7136=EDGE_CURVE('',#5749,#5748,#3904,.T.);
#7137=EDGE_CURVE('',#5733,#5749,#3905,.T.);
#7138=EDGE_CURVE('',#5750,#5749,#3439,.T.);
#7139=EDGE_CURVE('',#5734,#5750,#3906,.T.);
#7140=EDGE_CURVE('',#5740,#5750,#3907,.T.);
#7141=EDGE_CURVE('',#5700,#5739,#3908,.T.);
#7142=EDGE_CURVE('',#5751,#5721,#3909,.T.);
#7143=EDGE_CURVE('',#5724,#5751,#3910,.T.);
#7144=EDGE_CURVE('',#5745,#5751,#3911,.T.);
#7145=EDGE_CURVE('',#5752,#5753,#1115,.T.);
#7146=EDGE_CURVE('',#5753,#5754,#3440,.T.);
#7147=EDGE_CURVE('',#5754,#5755,#1116,.T.);
#7148=EDGE_CURVE('',#5755,#5752,#3441,.T.);
#7149=EDGE_CURVE('',#5756,#5757,#3912,.T.);
#7150=EDGE_CURVE('',#5758,#5756,#3913,.T.);
#7151=EDGE_CURVE('',#5759,#5758,#3914,.T.);
#7152=EDGE_CURVE('',#5757,#5759,#3915,.T.);
#7153=EDGE_CURVE('',#5760,#5760,#3442,.T.);
#7154=EDGE_CURVE('',#5761,#5761,#3443,.T.);
#7155=EDGE_CURVE('',#5762,#5762,#3444,.T.);
#7156=EDGE_CURVE('',#5763,#5763,#3445,.T.);
#7157=EDGE_CURVE('',#5764,#5765,#3446,.T.);
#7158=EDGE_CURVE('',#5765,#5764,#3447,.T.);
#7159=EDGE_CURVE('',#5754,#5753,#3448,.T.);
#7160=EDGE_CURVE('',#5766,#5766,#3449,.T.);
#7161=EDGE_CURVE('',#5767,#5767,#3450,.T.);
#7162=EDGE_CURVE('',#5768,#5769,#3451,.T.);
#7163=EDGE_CURVE('',#5769,#5768,#3452,.T.);
#7164=EDGE_CURVE('',#5770,#5771,#3453,.T.);
#7165=EDGE_CURVE('',#5771,#5770,#3454,.T.);
#7166=EDGE_CURVE('',#5772,#5772,#3455,.T.);
#7167=EDGE_CURVE('',#5773,#5773,#3456,.T.);
#7168=EDGE_CURVE('',#5774,#5774,#3457,.T.);
#7169=EDGE_CURVE('',#5774,#5760,#3916,.T.);
#7170=EDGE_CURVE('',#5774,#5775,#3917,.T.);
#7171=EDGE_CURVE('',#5775,#5775,#3458,.T.);
#7172=EDGE_CURVE('',#5776,#5770,#1117,.T.);
#7173=EDGE_CURVE('',#5771,#5777,#1118,.T.);
#7174=EDGE_CURVE('',#5777,#5776,#3459,.T.);
#7175=EDGE_CURVE('',#5778,#5778,#3460,.T.);
#7176=EDGE_CURVE('',#5778,#5761,#3918,.T.);
#7177=EDGE_CURVE('',#5778,#5779,#3919,.T.);
#7178=EDGE_CURVE('',#5779,#5779,#3461,.T.);
#7179=EDGE_CURVE('',#5780,#5768,#1119,.T.);
#7180=EDGE_CURVE('',#5769,#5781,#1120,.T.);
#7181=EDGE_CURVE('',#5781,#5780,#3462,.T.);
#7182=EDGE_CURVE('',#5782,#5782,#3463,.T.);
#7183=EDGE_CURVE('',#5782,#5762,#3920,.T.);
#7184=EDGE_CURVE('',#5782,#5783,#3921,.T.);
#7185=EDGE_CURVE('',#5783,#5783,#3464,.T.);
#7186=EDGE_CURVE('',#5784,#5784,#3465,.T.);
#7187=EDGE_CURVE('',#5784,#5773,#3922,.T.);
#7188=EDGE_CURVE('',#5784,#5785,#3923,.T.);
#7189=EDGE_CURVE('',#5785,#5785,#3466,.T.);
#7190=EDGE_CURVE('',#5786,#5764,#1121,.T.);
#7191=EDGE_CURVE('',#5765,#5787,#1122,.T.);
#7192=EDGE_CURVE('',#5787,#5786,#3467,.T.);
#7193=EDGE_CURVE('',#5788,#5787,#1123,.T.);
#7194=EDGE_CURVE('',#5789,#5788,#3924,.T.);
#7195=EDGE_CURVE('',#5789,#5790,#3468,.T.);
#7196=EDGE_CURVE('',#5791,#5790,#3925,.T.);
#7197=EDGE_CURVE('',#5786,#5791,#1124,.T.);
#7198=EDGE_CURVE('',#5790,#5789,#3469,.T.);
#7199=EDGE_CURVE('',#5792,#5792,#3470,.T.);
#7200=EDGE_CURVE('',#5793,#5793,#3471,.T.);
#7201=EDGE_CURVE('',#5794,#5794,#3472,.T.);
#7202=EDGE_CURVE('',#5795,#5781,#1125,.T.);
#7203=EDGE_CURVE('',#5796,#5795,#3926,.T.);
#7204=EDGE_CURVE('',#5796,#5797,#3473,.T.);
#7205=EDGE_CURVE('',#5798,#5797,#3927,.T.);
#7206=EDGE_CURVE('',#5780,#5798,#1126,.T.);
#7207=EDGE_CURVE('',#5797,#5796,#3474,.T.);
#7208=EDGE_CURVE('',#5799,#5799,#3475,.T.);
#7209=EDGE_CURVE('',#5800,#5800,#3476,.T.);
#7210=EDGE_CURVE('',#5801,#5777,#1127,.T.);
#7211=EDGE_CURVE('',#5802,#5801,#3928,.T.);
#7212=EDGE_CURVE('',#5802,#5803,#3477,.T.);
#7213=EDGE_CURVE('',#5804,#5803,#3929,.T.);
#7214=EDGE_CURVE('',#5776,#5804,#1128,.T.);
#7215=EDGE_CURVE('',#5803,#5802,#3478,.T.);
#7216=EDGE_CURVE('',#5805,#5805,#3479,.T.);
#7217=EDGE_CURVE('',#5806,#5806,#3480,.T.);
#7218=EDGE_CURVE('',#5807,#5755,#1129,.T.);
#7219=EDGE_CURVE('',#5808,#5807,#3930,.T.);
#7220=EDGE_CURVE('',#5808,#5809,#3481,.T.);
#7221=EDGE_CURVE('',#5810,#5809,#3931,.T.);
#7222=EDGE_CURVE('',#5752,#5810,#1130,.T.);
#7223=EDGE_CURVE('',#5809,#5808,#3482,.T.);
#7224=EDGE_CURVE('',#5811,#5811,#3483,.T.);
#7225=EDGE_CURVE('',#5791,#5812,#3484,.T.);
#7226=EDGE_CURVE('',#5812,#5788,#3485,.T.);
#7227=EDGE_CURVE('',#5798,#5813,#3486,.T.);
#7228=EDGE_CURVE('',#5813,#5795,#3487,.T.);
#7229=EDGE_CURVE('',#5804,#5814,#3488,.T.);
#7230=EDGE_CURVE('',#5814,#5801,#3489,.T.);
#7231=EDGE_CURVE('',#5810,#5815,#3490,.T.);
#7232=EDGE_CURVE('',#5815,#5807,#3491,.T.);
#7233=EDGE_CURVE('',#5792,#5816,#3932,.T.);
#7234=EDGE_CURVE('',#5816,#5816,#3492,.T.);
#7235=EDGE_CURVE('',#5793,#5817,#3933,.T.);
#7236=EDGE_CURVE('',#5817,#5817,#3493,.T.);
#7237=EDGE_CURVE('',#5794,#5818,#3934,.T.);
#7238=EDGE_CURVE('',#5818,#5818,#3494,.T.);
#7239=EDGE_CURVE('',#5799,#5819,#3935,.T.);
#7240=EDGE_CURVE('',#5819,#5819,#3495,.T.);
#7241=EDGE_CURVE('',#5800,#5820,#3936,.T.);
#7242=EDGE_CURVE('',#5820,#5820,#3496,.T.);
#7243=EDGE_CURVE('',#5805,#5821,#3937,.T.);
#7244=EDGE_CURVE('',#5821,#5821,#3497,.T.);
#7245=EDGE_CURVE('',#5806,#5822,#3938,.T.);
#7246=EDGE_CURVE('',#5822,#5822,#3498,.T.);
#7247=EDGE_CURVE('',#5811,#5823,#3939,.T.);
#7248=EDGE_CURVE('',#5823,#5823,#3499,.T.);
#7249=EDGE_CURVE('',#5824,#5824,#3500,.T.);
#7250=EDGE_CURVE('',#5824,#5772,#3940,.T.);
#7251=EDGE_CURVE('',#5824,#5825,#3941,.T.);
#7252=EDGE_CURVE('',#5825,#5825,#3501,.T.);
#7253=EDGE_CURVE('',#5826,#5826,#3502,.T.);
#7254=EDGE_CURVE('',#5826,#5763,#3942,.T.);
#7255=EDGE_CURVE('',#5826,#5827,#3943,.T.);
#7256=EDGE_CURVE('',#5827,#5827,#3503,.T.);
#7257=EDGE_CURVE('',#5814,#5828,#3944,.T.);
#7258=EDGE_CURVE('',#5828,#5828,#3504,.T.);
#7259=EDGE_CURVE('',#5812,#5829,#3945,.T.);
#7260=EDGE_CURVE('',#5829,#5829,#3505,.T.);
#7261=EDGE_CURVE('',#5813,#5830,#3946,.T.);
#7262=EDGE_CURVE('',#5830,#5830,#3506,.T.);
#7263=EDGE_CURVE('',#5815,#5831,#3947,.T.);
#7264=EDGE_CURVE('',#5831,#5831,#3507,.T.);
#7265=EDGE_CURVE('',#5832,#5832,#3508,.T.);
#7266=EDGE_CURVE('',#5832,#5767,#3948,.T.);
#7267=EDGE_CURVE('',#5832,#5833,#3949,.T.);
#7268=EDGE_CURVE('',#5833,#5833,#3509,.T.);
#7269=EDGE_CURVE('',#5834,#5834,#3510,.T.);
#7270=EDGE_CURVE('',#5834,#5766,#3950,.T.);
#7271=EDGE_CURVE('',#5834,#5835,#3951,.T.);
#7272=EDGE_CURVE('',#5835,#5835,#3511,.T.);
#7273=EDGE_CURVE('',#5836,#5825,#3952,.T.);
#7274=EDGE_CURVE('',#5837,#5835,#3953,.T.);
#7275=EDGE_CURVE('',#5838,#5827,#3954,.T.);
#7276=EDGE_CURVE('',#5839,#5833,#3955,.T.);
#7277=EDGE_CURVE('',#5840,#5831,#3956,.T.);
#7278=EDGE_CURVE('',#5841,#5829,#3957,.T.);
#7279=EDGE_CURVE('',#5842,#5830,#3958,.T.);
#7280=EDGE_CURVE('',#5843,#5828,#3959,.T.);
#7281=EDGE_CURVE('',#5757,#5844,#3960,.T.);
#7282=EDGE_CURVE('',#5844,#5845,#3961,.T.);
#7283=EDGE_CURVE('',#5756,#5845,#3962,.T.);
#7284=EDGE_CURVE('',#5759,#5846,#3963,.T.);
#7285=EDGE_CURVE('',#5846,#5844,#3964,.T.);
#7286=EDGE_CURVE('',#5758,#5847,#3965,.T.);
#7287=EDGE_CURVE('',#5847,#5846,#3966,.T.);
#7288=EDGE_CURVE('',#5845,#5847,#3967,.T.);
#7289=EDGE_CURVE('',#5848,#5845,#3968,.T.);
#7290=EDGE_CURVE('',#5849,#5848,#3969,.T.);
#7291=EDGE_CURVE('',#5849,#5847,#3970,.T.);
#7292=EDGE_CURVE('',#5850,#5844,#3971,.T.);
#7293=EDGE_CURVE('',#5848,#5850,#3972,.T.);
#7294=EDGE_CURVE('',#5851,#5849,#3973,.T.);
#7295=EDGE_CURVE('',#5851,#5846,#3974,.T.);
#7296=EDGE_CURVE('',#5850,#5851,#3975,.T.);
#7297=EDGE_CURVE('',#5852,#5853,#1131,.T.);
#7298=EDGE_CURVE('',#5853,#5852,#1132,.T.);
#7299=EDGE_CURVE('',#5853,#5854,#3976,.T.);
#7300=EDGE_CURVE('',#5854,#5854,#3512,.T.);
#7301=EDGE_CURVE('',#5855,#5854,#3977,.T.);
#7302=EDGE_CURVE('',#5856,#5857,#1133,.T.);
#7303=EDGE_CURVE('',#5857,#5856,#1134,.T.);
#7304=EDGE_CURVE('',#5857,#5858,#3978,.T.);
#7305=EDGE_CURVE('',#5858,#5858,#3513,.T.);
#7306=EDGE_CURVE('',#5859,#5858,#3979,.T.);
#7307=EDGE_CURVE('',#5860,#5861,#1135,.T.);
#7308=EDGE_CURVE('',#5861,#5860,#1136,.T.);
#7309=EDGE_CURVE('',#5861,#5862,#3980,.T.);
#7310=EDGE_CURVE('',#5862,#5862,#3514,.T.);
#7311=EDGE_CURVE('',#5863,#5862,#3981,.T.);
#7312=EDGE_CURVE('',#5864,#5864,#3515,.T.);
#7313=EDGE_CURVE('',#5865,#5865,#3516,.T.);
#7314=EDGE_CURVE('',#5865,#5864,#3982,.T.);
#7315=EDGE_CURVE('',#5866,#5866,#3517,.T.);
#7316=EDGE_CURVE('',#5866,#5865,#3983,.T.);
#7317=EDGE_CURVE('',#5866,#5867,#3984,.T.);
#7318=EDGE_CURVE('',#5867,#5867,#3518,.T.);
#7319=EDGE_CURVE('',#5868,#5868,#3519,.T.);
#7320=EDGE_CURVE('',#5868,#5869,#3985,.T.);
#7321=EDGE_CURVE('',#5869,#5869,#3520,.T.);
#7322=EDGE_CURVE('',#5870,#5871,#3986,.T.);
#7323=EDGE_CURVE('',#5872,#5870,#3987,.T.);
#7324=EDGE_CURVE('',#5873,#5872,#3988,.T.);
#7325=EDGE_CURVE('',#5871,#5873,#3989,.T.);
#7326=EDGE_CURVE('',#5874,#5874,#3521,.T.);
#7327=EDGE_CURVE('',#5868,#5875,#3990,.T.);
#7328=EDGE_CURVE('',#5875,#5876,#3522,.T.);
#7329=EDGE_CURVE('',#5877,#5876,#1137,.T.);
#7330=EDGE_CURVE('',#5877,#5875,#3523,.T.);
#7331=EDGE_CURVE('',#5878,#5878,#3524,.T.);
#7332=EDGE_CURVE('',#5878,#5874,#3991,.T.);
#7333=EDGE_CURVE('',#5878,#5879,#3992,.T.);
#7334=EDGE_CURVE('',#5879,#5880,#3525,.T.);
#7335=EDGE_CURVE('',#5881,#5880,#1138,.T.);
#7336=EDGE_CURVE('',#5881,#5879,#3526,.T.);
#7337=EDGE_CURVE('',#5882,#5875,#3993,.T.);
#7338=EDGE_CURVE('',#5876,#5877,#1139,.T.);
#7339=EDGE_CURVE('',#5883,#5884,#3527,.T.);
#7340=EDGE_CURVE('',#5885,#5883,#3994,.T.);
#7341=EDGE_CURVE('',#5886,#5885,#3528,.T.);
#7342=EDGE_CURVE('',#5884,#5886,#3995,.T.);
#7343=EDGE_CURVE('',#5880,#5881,#1140,.T.);
#7344=EDGE_CURVE('',#5887,#5879,#3996,.T.);
#7345=EDGE_CURVE('',#5884,#5888,#3997,.T.);
#7346=EDGE_CURVE('',#5888,#5889,#3529,.T.);
#7347=EDGE_CURVE('',#5889,#5883,#3998,.T.);
#7348=EDGE_CURVE('',#5888,#5890,#3999,.T.);
#7349=EDGE_CURVE('',#5890,#5891,#4000,.T.);
#7350=EDGE_CURVE('',#5871,#5891,#4001,.T.);
#7351=EDGE_CURVE('',#5892,#5873,#4002,.T.);
#7352=EDGE_CURVE('',#5892,#5893,#4003,.T.);
#7353=EDGE_CURVE('',#5894,#5893,#4004,.T.);
#7354=EDGE_CURVE('',#5894,#5895,#4005,.T.);
#7355=EDGE_CURVE('',#5895,#5889,#4006,.T.);
#7356=EDGE_CURVE('',#5896,#5886,#4007,.T.);
#7357=EDGE_CURVE('',#5897,#5896,#4008,.T.);
#7358=EDGE_CURVE('',#5897,#5890,#4009,.T.);
#7359=EDGE_CURVE('',#5885,#5898,#4010,.T.);
#7360=EDGE_CURVE('',#5898,#5896,#3530,.T.);
#7361=EDGE_CURVE('',#5898,#5899,#4011,.T.);
#7362=EDGE_CURVE('',#5899,#5900,#4012,.T.);
#7363=EDGE_CURVE('',#5901,#5900,#4013,.T.);
#7364=EDGE_CURVE('',#5901,#5902,#4014,.T.);
#7365=EDGE_CURVE('',#5872,#5902,#4015,.T.);
#7366=EDGE_CURVE('',#5903,#5870,#4016,.T.);
#7367=EDGE_CURVE('',#5903,#5897,#4017,.T.);
#7368=EDGE_CURVE('',#5899,#5895,#4018,.T.);
#7369=EDGE_CURVE('',#5891,#5903,#4019,.T.);
#7370=EDGE_CURVE('',#5902,#5892,#4020,.T.);
#7371=EDGE_CURVE('',#5893,#5901,#4021,.T.);
#7372=EDGE_CURVE('',#5900,#5894,#4022,.T.);
#7373=EDGE_CURVE('',#5904,#5905,#4023,.T.);
#7374=EDGE_CURVE('',#5906,#5904,#4024,.T.);
#7375=EDGE_CURVE('',#5907,#5906,#4025,.T.);
#7376=EDGE_CURVE('',#5908,#5907,#4026,.T.);
#7377=EDGE_CURVE('',#5909,#5908,#4027,.T.);
#7378=EDGE_CURVE('',#5905,#5909,#4028,.T.);
#7379=EDGE_CURVE('',#5910,#5911,#4029,.T.);
#7380=EDGE_CURVE('',#5912,#5910,#4030,.T.);
#7381=EDGE_CURVE('',#5913,#5912,#4031,.T.);
#7382=EDGE_CURVE('',#5914,#5913,#4032,.T.);
#7383=EDGE_CURVE('',#5915,#5914,#4033,.T.);
#7384=EDGE_CURVE('',#5911,#5915,#4034,.T.);
#7385=EDGE_CURVE('',#5904,#5911,#3531,.T.);
#7386=EDGE_CURVE('',#5905,#5910,#3532,.T.);
#7387=EDGE_CURVE('',#5906,#5915,#3533,.T.);
#7388=EDGE_CURVE('',#5907,#5914,#3534,.T.);
#7389=EDGE_CURVE('',#5908,#5913,#3535,.T.);
#7390=EDGE_CURVE('',#5909,#5912,#3536,.T.);
#7391=EDGE_CURVE('',#5916,#5917,#4035,.T.);
#7392=EDGE_CURVE('',#5916,#5918,#4036,.T.);
#7393=EDGE_CURVE('',#5919,#5918,#4037,.T.);
#7394=EDGE_CURVE('',#5919,#5917,#4038,.T.);
#7395=EDGE_CURVE('',#5917,#5920,#3537,.T.);
#7396=EDGE_CURVE('',#5921,#5919,#3538,.T.);
#7397=EDGE_CURVE('',#5920,#5921,#4039,.T.);
#7398=EDGE_CURVE('',#5920,#5922,#4040,.T.);
#7399=EDGE_CURVE('',#5923,#5921,#4041,.T.);
#7400=EDGE_CURVE('',#5923,#5922,#4042,.T.);
#7401=EDGE_CURVE('',#5922,#5916,#3539,.T.);
#7402=EDGE_CURVE('',#5918,#5923,#3540,.T.);
#7403=EDGE_CURVE('',#5924,#5925,#4043,.T.);
#7404=EDGE_CURVE('',#5924,#5926,#4044,.T.);
#7405=EDGE_CURVE('',#5927,#5926,#4045,.T.);
#7406=EDGE_CURVE('',#5927,#5925,#4046,.T.);
#7407=EDGE_CURVE('',#5925,#5928,#3541,.T.);
#7408=EDGE_CURVE('',#5929,#5927,#3542,.T.);
#7409=EDGE_CURVE('',#5928,#5929,#4047,.T.);
#7410=EDGE_CURVE('',#5928,#5930,#4048,.T.);
#7411=EDGE_CURVE('',#5931,#5929,#4049,.T.);
#7412=EDGE_CURVE('',#5931,#5930,#4050,.T.);
#7413=EDGE_CURVE('',#5930,#5924,#3543,.T.);
#7414=EDGE_CURVE('',#5926,#5931,#3544,.T.);
#7415=EDGE_CURVE('',#5932,#5933,#4051,.T.);
#7416=EDGE_CURVE('',#5932,#5934,#4052,.T.);
#7417=EDGE_CURVE('',#5935,#5934,#4053,.T.);
#7418=EDGE_CURVE('',#5935,#5933,#4054,.T.);
#7419=EDGE_CURVE('',#5933,#5936,#3545,.T.);
#7420=EDGE_CURVE('',#5937,#5935,#3546,.T.);
#7421=EDGE_CURVE('',#5936,#5937,#4055,.T.);
#7422=EDGE_CURVE('',#5936,#5938,#4056,.T.);
#7423=EDGE_CURVE('',#5939,#5937,#4057,.T.);
#7424=EDGE_CURVE('',#5939,#5938,#4058,.T.);
#7425=EDGE_CURVE('',#5938,#5932,#3547,.T.);
#7426=EDGE_CURVE('',#5934,#5939,#3548,.T.);
#7427=EDGE_CURVE('',#5940,#5941,#4059,.T.);
#7428=EDGE_CURVE('',#5940,#5942,#4060,.T.);
#7429=EDGE_CURVE('',#5943,#5942,#4061,.T.);
#7430=EDGE_CURVE('',#5943,#5941,#4062,.T.);
#7431=EDGE_CURVE('',#5941,#5944,#3549,.T.);
#7432=EDGE_CURVE('',#5945,#5943,#3550,.T.);
#7433=EDGE_CURVE('',#5944,#5945,#4063,.T.);
#7434=EDGE_CURVE('',#5944,#5946,#4064,.T.);
#7435=EDGE_CURVE('',#5947,#5945,#4065,.T.);
#7436=EDGE_CURVE('',#5947,#5946,#4066,.T.);
#7437=EDGE_CURVE('',#5946,#5940,#3551,.T.);
#7438=EDGE_CURVE('',#5942,#5947,#3552,.T.);
#7439=EDGE_CURVE('',#5948,#5949,#4067,.T.);
#7440=EDGE_CURVE('',#5948,#5950,#4068,.T.);
#7441=EDGE_CURVE('',#5951,#5950,#4069,.T.);
#7442=EDGE_CURVE('',#5951,#5949,#4070,.T.);
#7443=EDGE_CURVE('',#5949,#5952,#3553,.T.);
#7444=EDGE_CURVE('',#5953,#5951,#3554,.T.);
#7445=EDGE_CURVE('',#5952,#5953,#4071,.T.);
#7446=EDGE_CURVE('',#5952,#5954,#4072,.T.);
#7447=EDGE_CURVE('',#5955,#5953,#4073,.T.);
#7448=EDGE_CURVE('',#5955,#5954,#4074,.T.);
#7449=EDGE_CURVE('',#5954,#5948,#3555,.T.);
#7450=EDGE_CURVE('',#5950,#5955,#3556,.T.);
#7451=EDGE_CURVE('',#5956,#5957,#4075,.T.);
#7452=EDGE_CURVE('',#5958,#5956,#4076,.T.);
#7453=EDGE_CURVE('',#5959,#5958,#4077,.T.);
#7454=EDGE_CURVE('',#5957,#5959,#4078,.T.);
#7455=EDGE_CURVE('',#5960,#5961,#4079,.T.);
#7456=EDGE_CURVE('',#5962,#5960,#4080,.T.);
#7457=EDGE_CURVE('',#5963,#5962,#4081,.T.);
#7458=EDGE_CURVE('',#5961,#5963,#4082,.T.);
#7459=EDGE_CURVE('',#5961,#5956,#3557,.T.);
#7460=EDGE_CURVE('',#5963,#5958,#3558,.T.);
#7461=EDGE_CURVE('',#5962,#5959,#3559,.T.);
#7462=EDGE_CURVE('',#5960,#5957,#3560,.T.);
#7463=EDGE_CURVE('',#5964,#5965,#3561,.T.);
#7464=EDGE_CURVE('',#5966,#5967,#4083,.T.);
#7465=EDGE_CURVE('',#5968,#5966,#1141,.T.);
#7466=EDGE_CURVE('',#5969,#5968,#3562,.T.);
#7467=EDGE_CURVE('',#5969,#5967,#1142,.T.);
#7468=EDGE_CURVE('',#5970,#5971,#4084,.T.);
#7469=EDGE_CURVE('',#5972,#5970,#1143,.F.);
#7470=EDGE_CURVE('',#5966,#5972,#1144,.T.);
#7471=EDGE_CURVE('',#5967,#5973,#1145,.T.);
#7472=EDGE_CURVE('',#5973,#5971,#1146,.T.);
#7473=EDGE_CURVE('',#5974,#5975,#4085,.T.);
#7474=EDGE_CURVE('',#5970,#5974,#1147,.F.);
#7475=EDGE_CURVE('',#5971,#5975,#1148,.T.);
#7476=EDGE_CURVE('',#5976,#5977,#4086,.T.);
#7477=EDGE_CURVE('',#5978,#5976,#1149,.F.);
#7478=EDGE_CURVE('',#5974,#5978,#1150,.F.);
#7479=EDGE_CURVE('',#5975,#5979,#1151,.T.);
#7480=EDGE_CURVE('',#5979,#5977,#1152,.T.);
#7481=EDGE_CURVE('',#5980,#5981,#4087,.T.);
#7482=EDGE_CURVE('',#5976,#5980,#1153,.F.);
#7483=EDGE_CURVE('',#5977,#5981,#1154,.T.);
#7484=EDGE_CURVE('',#5982,#5983,#4088,.T.);
#7485=EDGE_CURVE('',#5984,#5982,#1155,.F.);
#7486=EDGE_CURVE('',#5980,#5984,#1156,.F.);
#7487=EDGE_CURVE('',#5981,#5985,#1157,.T.);
#7488=EDGE_CURVE('',#5985,#5983,#1158,.T.);
#7489=EDGE_CURVE('',#5986,#5987,#4089,.T.);
#7490=EDGE_CURVE('',#5982,#5986,#1159,.F.);
#7491=EDGE_CURVE('',#5983,#5987,#1160,.T.);
#7492=EDGE_CURVE('',#5988,#5989,#4090,.T.);
#7493=EDGE_CURVE('',#5990,#5988,#1161,.F.);
#7494=EDGE_CURVE('',#5986,#5990,#1162,.F.);
#7495=EDGE_CURVE('',#5987,#5991,#1163,.T.);
#7496=EDGE_CURVE('',#5991,#5989,#1164,.T.);
#7497=EDGE_CURVE('',#5992,#5993,#4091,.T.);
#7498=EDGE_CURVE('',#5988,#5992,#1165,.F.);
#7499=EDGE_CURVE('',#5989,#5994,#1166,.T.);
#7500=EDGE_CURVE('',#5994,#5993,#1167,.T.);
#7501=EDGE_CURVE('',#5995,#5996,#4092,.T.);
#7502=EDGE_CURVE('',#5997,#5995,#1168,.T.);
#7503=EDGE_CURVE('',#5992,#5997,#1169,.F.);
#7504=EDGE_CURVE('',#5993,#5998,#1170,.T.);
#7505=EDGE_CURVE('',#5998,#5996,#1171,.T.);
#7506=EDGE_CURVE('',#5999,#6000,#4093,.T.);
#7507=EDGE_CURVE('',#6001,#5999,#1172,.T.);
#7508=EDGE_CURVE('',#5995,#6001,#1173,.T.);
#7509=EDGE_CURVE('',#5996,#6000,#1174,.T.);
#7510=EDGE_CURVE('',#6002,#6003,#4094,.T.);
#7511=EDGE_CURVE('',#6004,#6002,#1175,.F.);
#7512=EDGE_CURVE('',#5999,#6004,#1176,.T.);
#7513=EDGE_CURVE('',#6000,#6005,#1177,.T.);
#7514=EDGE_CURVE('',#6005,#6003,#1178,.T.);
#7515=EDGE_CURVE('',#6006,#6007,#4095,.T.);
#7516=EDGE_CURVE('',#6002,#6006,#1179,.F.);
#7517=EDGE_CURVE('',#6003,#6007,#1180,.T.);
#7518=EDGE_CURVE('',#6008,#6009,#4096,.T.);
#7519=EDGE_CURVE('',#6010,#6008,#1181,.F.);
#7520=EDGE_CURVE('',#6006,#6010,#1182,.F.);
#7521=EDGE_CURVE('',#6007,#6011,#1183,.T.);
#7522=EDGE_CURVE('',#6011,#6009,#1184,.T.);
#7523=EDGE_CURVE('',#6012,#6013,#4097,.T.);
#7524=EDGE_CURVE('',#6008,#6012,#1185,.F.);
#7525=EDGE_CURVE('',#6009,#6013,#1186,.T.);
#7526=EDGE_CURVE('',#6014,#6015,#4098,.T.);
#7527=EDGE_CURVE('',#6016,#6014,#1187,.F.);
#7528=EDGE_CURVE('',#6012,#6016,#1188,.F.);
#7529=EDGE_CURVE('',#6013,#6017,#1189,.T.);
#7530=EDGE_CURVE('',#6017,#6015,#1190,.T.);
#7531=EDGE_CURVE('',#6018,#6019,#4099,.T.);
#7532=EDGE_CURVE('',#6014,#6018,#1191,.F.);
#7533=EDGE_CURVE('',#6015,#6019,#1192,.T.);
#7534=EDGE_CURVE('',#6020,#6021,#4100,.T.);
#7535=EDGE_CURVE('',#6022,#6020,#1193,.F.);
#7536=EDGE_CURVE('',#6018,#6022,#1194,.F.);
#7537=EDGE_CURVE('',#6019,#6023,#1195,.T.);
#7538=EDGE_CURVE('',#6023,#6021,#1196,.T.);
#7539=EDGE_CURVE('',#6024,#6025,#4101,.T.);
#7540=EDGE_CURVE('',#6020,#6024,#1197,.F.);
#7541=EDGE_CURVE('',#6021,#6025,#1198,.T.);
#7542=EDGE_CURVE('',#6026,#6027,#1199,.T.);
#7543=EDGE_CURVE('',#6028,#6027,#3563,.T.);
#7544=EDGE_CURVE('',#6028,#6029,#1200,.T.);
#7545=EDGE_CURVE('',#6029,#6030,#1201,.T.);
#7546=EDGE_CURVE('',#6030,#6031,#1202,.T.);
#7547=EDGE_CURVE('',#6031,#6032,#1203,.T.);
#7548=EDGE_CURVE('',#6032,#6033,#1204,.T.);
#7549=EDGE_CURVE('',#6033,#6034,#1205,.T.);
#7550=EDGE_CURVE('',#6034,#6035,#1206,.T.);
#7551=EDGE_CURVE('',#6035,#6036,#1207,.T.);
#7552=EDGE_CURVE('',#6036,#6037,#1208,.T.);
#7553=EDGE_CURVE('',#6037,#6038,#1209,.T.);
#7554=EDGE_CURVE('',#6038,#6039,#1210,.T.);
#7555=EDGE_CURVE('',#6039,#6040,#1211,.T.);
#7556=EDGE_CURVE('',#6040,#6041,#1212,.T.);
#7557=EDGE_CURVE('',#6041,#6042,#1213,.T.);
#7558=EDGE_CURVE('',#6042,#6043,#1214,.T.);
#7559=EDGE_CURVE('',#6043,#6044,#1215,.T.);
#7560=EDGE_CURVE('',#6044,#6045,#1216,.T.);
#7561=EDGE_CURVE('',#6045,#6046,#1217,.T.);
#7562=EDGE_CURVE('',#6046,#6047,#1218,.T.);
#7563=EDGE_CURVE('',#6047,#6048,#1219,.T.);
#7564=EDGE_CURVE('',#6048,#6049,#1220,.T.);
#7565=EDGE_CURVE('',#6050,#6049,#3564,.T.);
#7566=EDGE_CURVE('',#6051,#6050,#3565,.T.);
#7567=EDGE_CURVE('',#6051,#6052,#1221,.T.);
#7568=EDGE_CURVE('',#6052,#6053,#1222,.T.);
#7569=EDGE_CURVE('',#6053,#6054,#1223,.T.);
#7570=EDGE_CURVE('',#6054,#6055,#1224,.T.);
#7571=EDGE_CURVE('',#6055,#6056,#1225,.T.);
#7572=EDGE_CURVE('',#6056,#6057,#1226,.T.);
#7573=EDGE_CURVE('',#6057,#6058,#1227,.T.);
#7574=EDGE_CURVE('',#6058,#6059,#1228,.T.);
#7575=EDGE_CURVE('',#6059,#6060,#1229,.T.);
#7576=EDGE_CURVE('',#6060,#6061,#1230,.T.);
#7577=EDGE_CURVE('',#6061,#6062,#1231,.T.);
#7578=EDGE_CURVE('',#6062,#6063,#1232,.T.);
#7579=EDGE_CURVE('',#6063,#6064,#1233,.T.);
#7580=EDGE_CURVE('',#6064,#6065,#1234,.T.);
#7581=EDGE_CURVE('',#6065,#6066,#1235,.T.);
#7582=EDGE_CURVE('',#6066,#6067,#1236,.T.);
#7583=EDGE_CURVE('',#6067,#6068,#1237,.T.);
#7584=EDGE_CURVE('',#6068,#6069,#1238,.T.);
#7585=EDGE_CURVE('',#6069,#6026,#1239,.T.);
#7586=EDGE_CURVE('',#6025,#6070,#1240,.T.);
#7587=EDGE_CURVE('',#6070,#6071,#1241,.T.);
#7588=EDGE_CURVE('',#6072,#6071,#3566,.T.);
#7589=EDGE_CURVE('',#6073,#6072,#1242,.T.);
#7590=EDGE_CURVE('',#6024,#6073,#1243,.F.);
#7591=EDGE_CURVE('',#6074,#6051,#3567,.T.);
#7592=EDGE_CURVE('',#6074,#6072,#1244,.T.);
#7593=EDGE_CURVE('',#6071,#6051,#1245,.T.);
#7594=EDGE_CURVE('',#6049,#6074,#1246,.T.);
#7595=EDGE_CURVE('',#5968,#6028,#1247,.T.);
#7596=EDGE_CURVE('',#6075,#6076,#3568,.T.);
#7597=EDGE_CURVE('',#6075,#5969,#1248,.T.);
#7598=EDGE_CURVE('',#6076,#6028,#3569,.T.);
#7599=EDGE_CURVE('',#6027,#6075,#1249,.T.);
#7600=EDGE_CURVE('',#6077,#6077,#3570,.T.);
#7601=EDGE_CURVE('',#6077,#6076,#3571,.T.);
#7602=EDGE_CURVE('',#6078,#6078,#3572,.T.);
#7603=EDGE_CURVE('',#6050,#6079,#4102,.T.);
#7604=EDGE_CURVE('',#6079,#6079,#3573,.T.);
#7605=EDGE_CURVE('',#6080,#6081,#4103,.T.);
#7606=EDGE_CURVE('',#6080,#6082,#4104,.T.);
#7607=EDGE_CURVE('',#6083,#6082,#4105,.T.);
#7608=EDGE_CURVE('',#6081,#6083,#787,.T.);
#7609=EDGE_CURVE('',#6084,#6085,#4106,.T.);
#7610=EDGE_CURVE('',#6083,#6084,#788,.T.);
#7611=EDGE_CURVE('',#6082,#6085,#4107,.T.);
#7612=EDGE_CURVE('',#6085,#6080,#3574,.T.);
#7613=EDGE_CURVE('',#6086,#6087,#789,.T.);
#7614=EDGE_CURVE('',#6087,#6088,#3575,.T.);
#7615=EDGE_CURVE('',#6088,#6089,#790,.T.);
#7616=EDGE_CURVE('',#6089,#6090,#791,.T.);
#7617=EDGE_CURVE('',#6090,#6091,#3576,.T.);
#7618=EDGE_CURVE('',#6091,#6092,#792,.T.);
#7619=EDGE_CURVE('',#6092,#6093,#793,.T.);
#7620=EDGE_CURVE('',#6093,#6094,#3577,.T.);
#7621=EDGE_CURVE('',#6094,#6095,#794,.T.);
#7622=EDGE_CURVE('',#6095,#6096,#795,.T.);
#7623=EDGE_CURVE('',#6096,#6097,#3578,.T.);
#7624=EDGE_CURVE('',#6097,#6098,#796,.T.);
#7625=EDGE_CURVE('',#6098,#6099,#797,.T.);
#7626=EDGE_CURVE('',#6099,#6100,#3579,.T.);
#7627=EDGE_CURVE('',#6100,#6101,#798,.T.);
#7628=EDGE_CURVE('',#6101,#6102,#799,.T.);
#7629=EDGE_CURVE('',#6102,#6103,#3580,.T.);
#7630=EDGE_CURVE('',#6103,#6104,#800,.T.);
#7631=EDGE_CURVE('',#6104,#6105,#801,.T.);
#7632=EDGE_CURVE('',#6105,#6106,#3581,.T.);
#7633=EDGE_CURVE('',#6106,#6107,#802,.T.);
#7634=EDGE_CURVE('',#6107,#6108,#803,.T.);
#7635=EDGE_CURVE('',#6108,#6109,#3582,.T.);
#7636=EDGE_CURVE('',#6109,#6110,#804,.T.);
#7637=EDGE_CURVE('',#6110,#6111,#805,.T.);
#7638=EDGE_CURVE('',#6111,#6112,#3583,.T.);
#7639=EDGE_CURVE('',#6112,#6113,#806,.T.);
#7640=EDGE_CURVE('',#6113,#6114,#807,.T.);
#7641=EDGE_CURVE('',#6114,#6115,#3584,.T.);
#7642=EDGE_CURVE('',#6115,#6116,#808,.T.);
#7643=EDGE_CURVE('',#6116,#6117,#809,.T.);
#7644=EDGE_CURVE('',#6117,#6118,#3585,.T.);
#7645=EDGE_CURVE('',#6118,#6119,#810,.T.);
#7646=EDGE_CURVE('',#6119,#6120,#811,.T.);
#7647=EDGE_CURVE('',#6120,#6121,#3586,.T.);
#7648=EDGE_CURVE('',#6121,#6122,#812,.T.);
#7649=EDGE_CURVE('',#6122,#6123,#813,.T.);
#7650=EDGE_CURVE('',#6123,#6124,#3587,.T.);
#7651=EDGE_CURVE('',#6124,#6125,#814,.T.);
#7652=EDGE_CURVE('',#6125,#6126,#815,.T.);
#7653=EDGE_CURVE('',#6126,#6127,#3588,.T.);
#7654=EDGE_CURVE('',#6127,#6128,#816,.T.);
#7655=EDGE_CURVE('',#6128,#6129,#817,.T.);
#7656=EDGE_CURVE('',#6129,#6130,#3589,.T.);
#7657=EDGE_CURVE('',#6130,#6131,#818,.T.);
#7658=EDGE_CURVE('',#6131,#6132,#819,.T.);
#7659=EDGE_CURVE('',#6132,#6133,#3590,.T.);
#7660=EDGE_CURVE('',#6133,#6134,#820,.T.);
#7661=EDGE_CURVE('',#6134,#6135,#821,.T.);
#7662=EDGE_CURVE('',#6135,#6136,#3591,.T.);
#7663=EDGE_CURVE('',#6136,#6137,#822,.T.);
#7664=EDGE_CURVE('',#6137,#6138,#823,.T.);
#7665=EDGE_CURVE('',#6138,#6139,#3592,.T.);
#7666=EDGE_CURVE('',#6139,#6140,#824,.T.);
#7667=EDGE_CURVE('',#6140,#6141,#825,.T.);
#7668=EDGE_CURVE('',#6141,#6081,#3593,.T.);
#7669=EDGE_CURVE('',#6084,#6142,#3594,.T.);
#7670=EDGE_CURVE('',#6142,#6143,#826,.T.);
#7671=EDGE_CURVE('',#6143,#6144,#827,.T.);
#7672=EDGE_CURVE('',#6144,#6145,#3595,.T.);
#7673=EDGE_CURVE('',#6145,#6146,#828,.T.);
#7674=EDGE_CURVE('',#6146,#6147,#829,.T.);
#7675=EDGE_CURVE('',#6147,#6148,#3596,.T.);
#7676=EDGE_CURVE('',#6148,#6149,#830,.T.);
#7677=EDGE_CURVE('',#6149,#6150,#831,.T.);
#7678=EDGE_CURVE('',#6150,#6151,#3597,.T.);
#7679=EDGE_CURVE('',#6151,#6152,#832,.T.);
#7680=EDGE_CURVE('',#6152,#6153,#833,.T.);
#7681=EDGE_CURVE('',#6153,#6154,#3598,.T.);
#7682=EDGE_CURVE('',#6154,#6155,#834,.T.);
#7683=EDGE_CURVE('',#6155,#6156,#835,.T.);
#7684=EDGE_CURVE('',#6156,#6157,#3599,.T.);
#7685=EDGE_CURVE('',#6157,#6158,#836,.T.);
#7686=EDGE_CURVE('',#6158,#6159,#837,.T.);
#7687=EDGE_CURVE('',#6159,#6160,#3600,.T.);
#7688=EDGE_CURVE('',#6160,#6161,#838,.T.);
#7689=EDGE_CURVE('',#6161,#6162,#839,.T.);
#7690=EDGE_CURVE('',#6162,#6163,#3601,.T.);
#7691=EDGE_CURVE('',#6163,#6164,#840,.T.);
#7692=EDGE_CURVE('',#6164,#6165,#841,.T.);
#7693=EDGE_CURVE('',#6165,#6166,#3602,.T.);
#7694=EDGE_CURVE('',#6166,#6167,#842,.T.);
#7695=EDGE_CURVE('',#6167,#6168,#843,.T.);
#7696=EDGE_CURVE('',#6168,#6169,#3603,.T.);
#7697=EDGE_CURVE('',#6169,#6170,#844,.T.);
#7698=EDGE_CURVE('',#6170,#6171,#845,.T.);
#7699=EDGE_CURVE('',#6171,#6172,#3604,.T.);
#7700=EDGE_CURVE('',#6172,#6173,#846,.T.);
#7701=EDGE_CURVE('',#6173,#6174,#847,.T.);
#7702=EDGE_CURVE('',#6174,#6175,#3605,.T.);
#7703=EDGE_CURVE('',#6175,#6176,#848,.T.);
#7704=EDGE_CURVE('',#6176,#6177,#849,.T.);
#7705=EDGE_CURVE('',#6177,#6178,#3606,.T.);
#7706=EDGE_CURVE('',#6178,#6179,#850,.T.);
#7707=EDGE_CURVE('',#6179,#6180,#851,.T.);
#7708=EDGE_CURVE('',#6180,#6181,#3607,.T.);
#7709=EDGE_CURVE('',#6181,#6182,#852,.T.);
#7710=EDGE_CURVE('',#6182,#6183,#853,.T.);
#7711=EDGE_CURVE('',#6183,#6184,#3608,.T.);
#7712=EDGE_CURVE('',#6184,#6185,#854,.T.);
#7713=EDGE_CURVE('',#6185,#6186,#855,.T.);
#7714=EDGE_CURVE('',#6186,#6187,#3609,.T.);
#7715=EDGE_CURVE('',#6187,#6188,#856,.T.);
#7716=EDGE_CURVE('',#6188,#6189,#857,.T.);
#7717=EDGE_CURVE('',#6189,#6190,#3610,.T.);
#7718=EDGE_CURVE('',#6190,#6086,#858,.T.);
#7719=EDGE_CURVE('',#6086,#6191,#4108,.T.);
#7720=EDGE_CURVE('',#6191,#6191,#3611,.T.);
#7721=EDGE_CURVE('',#6192,#6142,#4109,.T.);
#7722=EDGE_CURVE('',#6192,#6193,#4110,.T.);
#7723=EDGE_CURVE('',#6143,#6193,#4111,.T.);
#7724=EDGE_CURVE('',#6144,#6194,#4112,.T.);
#7725=EDGE_CURVE('',#6193,#6194,#4113,.T.);
#7726=EDGE_CURVE('',#6194,#6192,#3612,.T.);
#7727=EDGE_CURVE('',#6195,#6145,#4114,.T.);
#7728=EDGE_CURVE('',#6195,#6196,#4115,.T.);
#7729=EDGE_CURVE('',#6146,#6196,#4116,.T.);
#7730=EDGE_CURVE('',#6147,#6197,#4117,.T.);
#7731=EDGE_CURVE('',#6196,#6197,#4118,.T.);
#7732=EDGE_CURVE('',#6197,#6195,#3613,.T.);
#7733=EDGE_CURVE('',#6198,#6148,#4119,.T.);
#7734=EDGE_CURVE('',#6198,#6199,#4120,.T.);
#7735=EDGE_CURVE('',#6149,#6199,#4121,.T.);
#7736=EDGE_CURVE('',#6150,#6200,#4122,.T.);
#7737=EDGE_CURVE('',#6199,#6200,#4123,.T.);
#7738=EDGE_CURVE('',#6200,#6198,#3614,.T.);
#7739=EDGE_CURVE('',#6201,#6151,#4124,.T.);
#7740=EDGE_CURVE('',#6201,#6202,#4125,.T.);
#7741=EDGE_CURVE('',#6152,#6202,#4126,.T.);
#7742=EDGE_CURVE('',#6153,#6203,#4127,.T.);
#7743=EDGE_CURVE('',#6202,#6203,#4128,.T.);
#7744=EDGE_CURVE('',#6203,#6201,#3615,.T.);
#7745=EDGE_CURVE('',#6204,#6154,#4129,.T.);
#7746=EDGE_CURVE('',#6204,#6205,#4130,.T.);
#7747=EDGE_CURVE('',#6155,#6205,#4131,.T.);
#7748=EDGE_CURVE('',#6156,#6206,#4132,.T.);
#7749=EDGE_CURVE('',#6205,#6206,#4133,.T.);
#7750=EDGE_CURVE('',#6206,#6204,#3616,.T.);
#7751=EDGE_CURVE('',#6207,#6157,#4134,.T.);
#7752=EDGE_CURVE('',#6207,#6208,#4135,.T.);
#7753=EDGE_CURVE('',#6158,#6208,#4136,.T.);
#7754=EDGE_CURVE('',#6159,#6209,#4137,.T.);
#7755=EDGE_CURVE('',#6208,#6209,#4138,.T.);
#7756=EDGE_CURVE('',#6209,#6207,#3617,.T.);
#7757=EDGE_CURVE('',#6210,#6160,#4139,.T.);
#7758=EDGE_CURVE('',#6210,#6211,#4140,.T.);
#7759=EDGE_CURVE('',#6161,#6211,#4141,.T.);
#7760=EDGE_CURVE('',#6162,#6212,#4142,.T.);
#7761=EDGE_CURVE('',#6211,#6212,#4143,.T.);
#7762=EDGE_CURVE('',#6212,#6210,#3618,.T.);
#7763=EDGE_CURVE('',#6213,#6163,#4144,.T.);
#7764=EDGE_CURVE('',#6213,#6214,#4145,.T.);
#7765=EDGE_CURVE('',#6164,#6214,#4146,.T.);
#7766=EDGE_CURVE('',#6165,#6215,#4147,.T.);
#7767=EDGE_CURVE('',#6214,#6215,#4148,.T.);
#7768=EDGE_CURVE('',#6215,#6213,#3619,.T.);
#7769=EDGE_CURVE('',#6216,#6166,#4149,.T.);
#7770=EDGE_CURVE('',#6216,#6217,#4150,.T.);
#7771=EDGE_CURVE('',#6167,#6217,#4151,.T.);
#7772=EDGE_CURVE('',#6168,#6218,#4152,.T.);
#7773=EDGE_CURVE('',#6217,#6218,#4153,.T.);
#7774=EDGE_CURVE('',#6218,#6216,#3620,.T.);
#7775=EDGE_CURVE('',#6219,#6169,#4154,.T.);
#7776=EDGE_CURVE('',#6219,#6220,#4155,.T.);
#7777=EDGE_CURVE('',#6170,#6220,#4156,.T.);
#7778=EDGE_CURVE('',#6171,#6221,#4157,.T.);
#7779=EDGE_CURVE('',#6220,#6221,#4158,.T.);
#7780=EDGE_CURVE('',#6221,#6219,#3621,.T.);
#7781=EDGE_CURVE('',#6222,#6172,#4159,.T.);
#7782=EDGE_CURVE('',#6222,#6223,#4160,.T.);
#7783=EDGE_CURVE('',#6173,#6223,#4161,.T.);
#7784=EDGE_CURVE('',#6174,#6224,#4162,.T.);
#7785=EDGE_CURVE('',#6223,#6224,#4163,.T.);
#7786=EDGE_CURVE('',#6224,#6222,#3622,.T.);
#7787=EDGE_CURVE('',#6225,#6175,#4164,.T.);
#7788=EDGE_CURVE('',#6225,#6226,#4165,.T.);
#7789=EDGE_CURVE('',#6176,#6226,#4166,.T.);
#7790=EDGE_CURVE('',#6177,#6227,#4167,.T.);
#7791=EDGE_CURVE('',#6226,#6227,#4168,.T.);
#7792=EDGE_CURVE('',#6227,#6225,#3623,.T.);
#7793=EDGE_CURVE('',#6228,#6178,#4169,.T.);
#7794=EDGE_CURVE('',#6228,#6229,#4170,.T.);
#7795=EDGE_CURVE('',#6179,#6229,#4171,.T.);
#7796=EDGE_CURVE('',#6180,#6230,#4172,.T.);
#7797=EDGE_CURVE('',#6229,#6230,#4173,.T.);
#7798=EDGE_CURVE('',#6230,#6228,#3624,.T.);
#7799=EDGE_CURVE('',#6231,#6181,#4174,.T.);
#7800=EDGE_CURVE('',#6231,#6232,#4175,.T.);
#7801=EDGE_CURVE('',#6182,#6232,#4176,.T.);
#7802=EDGE_CURVE('',#6183,#6233,#4177,.T.);
#7803=EDGE_CURVE('',#6232,#6233,#4178,.T.);
#7804=EDGE_CURVE('',#6233,#6231,#3625,.T.);
#7805=EDGE_CURVE('',#6234,#6184,#4179,.T.);
#7806=EDGE_CURVE('',#6234,#6235,#4180,.T.);
#7807=EDGE_CURVE('',#6185,#6235,#4181,.T.);
#7808=EDGE_CURVE('',#6186,#6236,#4182,.T.);
#7809=EDGE_CURVE('',#6235,#6236,#4183,.T.);
#7810=EDGE_CURVE('',#6236,#6234,#3626,.T.);
#7811=EDGE_CURVE('',#6237,#6187,#4184,.T.);
#7812=EDGE_CURVE('',#6237,#6238,#4185,.T.);
#7813=EDGE_CURVE('',#6188,#6238,#4186,.T.);
#7814=EDGE_CURVE('',#6189,#6239,#4187,.T.);
#7815=EDGE_CURVE('',#6238,#6239,#4188,.T.);
#7816=EDGE_CURVE('',#6239,#6237,#3627,.T.);
#7817=EDGE_CURVE('',#6240,#6190,#4189,.T.);
#7818=EDGE_CURVE('',#6240,#6241,#4190,.T.);
#7819=EDGE_CURVE('',#6086,#6241,#4191,.T.);
#7820=EDGE_CURVE('',#6087,#6242,#4192,.T.);
#7821=EDGE_CURVE('',#6241,#6242,#4193,.T.);
#7822=EDGE_CURVE('',#6242,#6243,#3628,.T.);
#7823=EDGE_CURVE('',#6243,#6240,#3629,.T.);
#7824=EDGE_CURVE('',#6244,#6088,#4194,.T.);
#7825=EDGE_CURVE('',#6244,#6245,#4195,.T.);
#7826=EDGE_CURVE('',#6089,#6245,#4196,.T.);
#7827=EDGE_CURVE('',#6090,#6246,#4197,.T.);
#7828=EDGE_CURVE('',#6245,#6246,#4198,.T.);
#7829=EDGE_CURVE('',#6246,#6244,#3630,.T.);
#7830=EDGE_CURVE('',#6247,#6091,#4199,.T.);
#7831=EDGE_CURVE('',#6247,#6248,#4200,.T.);
#7832=EDGE_CURVE('',#6092,#6248,#4201,.T.);
#7833=EDGE_CURVE('',#6093,#6249,#4202,.T.);
#7834=EDGE_CURVE('',#6248,#6249,#4203,.T.);
#7835=EDGE_CURVE('',#6249,#6247,#3631,.T.);
#7836=EDGE_CURVE('',#6250,#6094,#4204,.T.);
#7837=EDGE_CURVE('',#6250,#6251,#4205,.T.);
#7838=EDGE_CURVE('',#6095,#6251,#4206,.T.);
#7839=EDGE_CURVE('',#6096,#6252,#4207,.T.);
#7840=EDGE_CURVE('',#6251,#6252,#4208,.T.);
#7841=EDGE_CURVE('',#6252,#6250,#3632,.T.);
#7842=EDGE_CURVE('',#6253,#6097,#4209,.T.);
#7843=EDGE_CURVE('',#6253,#6254,#4210,.T.);
#7844=EDGE_CURVE('',#6098,#6254,#4211,.T.);
#7845=EDGE_CURVE('',#6099,#6255,#4212,.T.);
#7846=EDGE_CURVE('',#6254,#6255,#4213,.T.);
#7847=EDGE_CURVE('',#6255,#6253,#3633,.T.);
#7848=EDGE_CURVE('',#6256,#6100,#4214,.T.);
#7849=EDGE_CURVE('',#6256,#6257,#4215,.T.);
#7850=EDGE_CURVE('',#6101,#6257,#4216,.T.);
#7851=EDGE_CURVE('',#6102,#6258,#4217,.T.);
#7852=EDGE_CURVE('',#6257,#6258,#4218,.T.);
#7853=EDGE_CURVE('',#6258,#6256,#3634,.T.);
#7854=EDGE_CURVE('',#6259,#6103,#4219,.T.);
#7855=EDGE_CURVE('',#6259,#6260,#4220,.T.);
#7856=EDGE_CURVE('',#6104,#6260,#4221,.T.);
#7857=EDGE_CURVE('',#6105,#6261,#4222,.T.);
#7858=EDGE_CURVE('',#6260,#6261,#4223,.T.);
#7859=EDGE_CURVE('',#6261,#6259,#3635,.T.);
#7860=EDGE_CURVE('',#6262,#6106,#4224,.T.);
#7861=EDGE_CURVE('',#6262,#6263,#4225,.T.);
#7862=EDGE_CURVE('',#6107,#6263,#4226,.T.);
#7863=EDGE_CURVE('',#6108,#6264,#4227,.T.);
#7864=EDGE_CURVE('',#6263,#6264,#4228,.T.);
#7865=EDGE_CURVE('',#6264,#6262,#3636,.T.);
#7866=EDGE_CURVE('',#6265,#6109,#4229,.T.);
#7867=EDGE_CURVE('',#6265,#6266,#4230,.T.);
#7868=EDGE_CURVE('',#6110,#6266,#4231,.T.);
#7869=EDGE_CURVE('',#6111,#6267,#4232,.T.);
#7870=EDGE_CURVE('',#6266,#6267,#4233,.T.);
#7871=EDGE_CURVE('',#6267,#6265,#3637,.T.);
#7872=EDGE_CURVE('',#6268,#6112,#4234,.T.);
#7873=EDGE_CURVE('',#6268,#6269,#4235,.T.);
#7874=EDGE_CURVE('',#6113,#6269,#4236,.T.);
#7875=EDGE_CURVE('',#6114,#6270,#4237,.T.);
#7876=EDGE_CURVE('',#6269,#6270,#4238,.T.);
#7877=EDGE_CURVE('',#6270,#6268,#3638,.T.);
#7878=EDGE_CURVE('',#6271,#6115,#4239,.T.);
#7879=EDGE_CURVE('',#6271,#6272,#4240,.T.);
#7880=EDGE_CURVE('',#6116,#6272,#4241,.T.);
#7881=EDGE_CURVE('',#6117,#6273,#4242,.T.);
#7882=EDGE_CURVE('',#6272,#6273,#4243,.T.);
#7883=EDGE_CURVE('',#6273,#6271,#3639,.T.);
#7884=EDGE_CURVE('',#6274,#6118,#4244,.T.);
#7885=EDGE_CURVE('',#6274,#6275,#4245,.T.);
#7886=EDGE_CURVE('',#6119,#6275,#4246,.T.);
#7887=EDGE_CURVE('',#6120,#6276,#4247,.T.);
#7888=EDGE_CURVE('',#6275,#6276,#4248,.T.);
#7889=EDGE_CURVE('',#6276,#6274,#3640,.T.);
#7890=EDGE_CURVE('',#6277,#6121,#4249,.T.);
#7891=EDGE_CURVE('',#6277,#6278,#4250,.T.);
#7892=EDGE_CURVE('',#6122,#6278,#4251,.T.);
#7893=EDGE_CURVE('',#6123,#6279,#4252,.T.);
#7894=EDGE_CURVE('',#6278,#6279,#4253,.T.);
#7895=EDGE_CURVE('',#6279,#6277,#3641,.T.);
#7896=EDGE_CURVE('',#6280,#6124,#4254,.T.);
#7897=EDGE_CURVE('',#6280,#6281,#4255,.T.);
#7898=EDGE_CURVE('',#6125,#6281,#4256,.T.);
#7899=EDGE_CURVE('',#6126,#6282,#4257,.T.);
#7900=EDGE_CURVE('',#6281,#6282,#4258,.T.);
#7901=EDGE_CURVE('',#6282,#6280,#3642,.T.);
#7902=EDGE_CURVE('',#6283,#6127,#4259,.T.);
#7903=EDGE_CURVE('',#6283,#6284,#4260,.T.);
#7904=EDGE_CURVE('',#6128,#6284,#4261,.T.);
#7905=EDGE_CURVE('',#6129,#6285,#4262,.T.);
#7906=EDGE_CURVE('',#6284,#6285,#4263,.T.);
#7907=EDGE_CURVE('',#6285,#6283,#3643,.T.);
#7908=EDGE_CURVE('',#6286,#6130,#4264,.T.);
#7909=EDGE_CURVE('',#6286,#6287,#4265,.T.);
#7910=EDGE_CURVE('',#6131,#6287,#4266,.T.);
#7911=EDGE_CURVE('',#6132,#6288,#4267,.T.);
#7912=EDGE_CURVE('',#6287,#6288,#4268,.T.);
#7913=EDGE_CURVE('',#6288,#6286,#3644,.T.);
#7914=EDGE_CURVE('',#6289,#6133,#4269,.T.);
#7915=EDGE_CURVE('',#6289,#6290,#4270,.T.);
#7916=EDGE_CURVE('',#6134,#6290,#4271,.T.);
#7917=EDGE_CURVE('',#6135,#6291,#4272,.T.);
#7918=EDGE_CURVE('',#6290,#6291,#4273,.T.);
#7919=EDGE_CURVE('',#6291,#6289,#3645,.T.);
#7920=EDGE_CURVE('',#6292,#6136,#4274,.T.);
#7921=EDGE_CURVE('',#6292,#6293,#4275,.T.);
#7922=EDGE_CURVE('',#6137,#6293,#4276,.T.);
#7923=EDGE_CURVE('',#6138,#6294,#4277,.T.);
#7924=EDGE_CURVE('',#6293,#6294,#4278,.T.);
#7925=EDGE_CURVE('',#6294,#6292,#3646,.T.);
#7926=EDGE_CURVE('',#6295,#6139,#4279,.T.);
#7927=EDGE_CURVE('',#6295,#6296,#4280,.T.);
#7928=EDGE_CURVE('',#6140,#6296,#4281,.T.);
#7929=EDGE_CURVE('',#6141,#6297,#4282,.T.);
#7930=EDGE_CURVE('',#6296,#6297,#4283,.T.);
#7931=EDGE_CURVE('',#6297,#6295,#3647,.T.);
#7932=EDGE_CURVE('',#6243,#6078,#4284,.T.);
#7933=EDGE_CURVE('',#6298,#6299,#4285,.T.);
#7934=EDGE_CURVE('',#6299,#6300,#4286,.T.);
#7935=EDGE_CURVE('',#6300,#6301,#4287,.T.);
#7936=EDGE_CURVE('',#6301,#6302,#4288,.T.);
#7937=EDGE_CURVE('',#6302,#6303,#4289,.T.);
#7938=EDGE_CURVE('',#6303,#6298,#4290,.T.);
#7939=EDGE_CURVE('',#6304,#6305,#4291,.T.);
#7940=EDGE_CURVE('',#6304,#6305,#3648,.T.);
#7941=EDGE_CURVE('',#6305,#6306,#4292,.T.);
#7942=EDGE_CURVE('',#6305,#6306,#3649,.T.);
#7943=EDGE_CURVE('',#6306,#6307,#4293,.T.);
#7944=EDGE_CURVE('',#6306,#6307,#3650,.T.);
#7945=EDGE_CURVE('',#6307,#6308,#4294,.T.);
#7946=EDGE_CURVE('',#6307,#6308,#3651,.T.);
#7947=EDGE_CURVE('',#6308,#6309,#4295,.T.);
#7948=EDGE_CURVE('',#6308,#6309,#3652,.T.);
#7949=EDGE_CURVE('',#6309,#6304,#4296,.T.);
#7950=EDGE_CURVE('',#6309,#6304,#3653,.T.);
#7951=EDGE_CURVE('',#6310,#6304,#4297,.T.);
#7952=EDGE_CURVE('',#6298,#6304,#4298,.T.);
#7953=EDGE_CURVE('',#6299,#6305,#4299,.T.);
#7954=EDGE_CURVE('',#6303,#6309,#4300,.T.);
#7955=EDGE_CURVE('',#6302,#6308,#4301,.T.);
#7956=EDGE_CURVE('',#6301,#6307,#4302,.T.);
#7957=EDGE_CURVE('',#6300,#6306,#4303,.T.);
#7958=EDGE_CURVE('',#6311,#6312,#4304,.T.);
#7959=EDGE_CURVE('',#6313,#6311,#1250,.T.);
#7960=EDGE_CURVE('',#6314,#6313,#3654,.T.);
#7961=EDGE_CURVE('',#6314,#6312,#1251,.T.);
#7962=EDGE_CURVE('',#6315,#6316,#4305,.T.);
#7963=EDGE_CURVE('',#6317,#6315,#1252,.T.);
#7964=EDGE_CURVE('',#6311,#6317,#1253,.T.);
#7965=EDGE_CURVE('',#6312,#6318,#1254,.T.);
#7966=EDGE_CURVE('',#6318,#6316,#1255,.T.);
#7967=EDGE_CURVE('',#6319,#6320,#4306,.T.);
#7968=EDGE_CURVE('',#6321,#6319,#1256,.F.);
#7969=EDGE_CURVE('',#6315,#6321,#1257,.T.);
#7970=EDGE_CURVE('',#6316,#6320,#1258,.T.);
#7971=EDGE_CURVE('',#6322,#6323,#4307,.T.);
#7972=EDGE_CURVE('',#6319,#6322,#1259,.F.);
#7973=EDGE_CURVE('',#6320,#6324,#1260,.T.);
#7974=EDGE_CURVE('',#6324,#6323,#1261,.T.);
#7975=EDGE_CURVE('',#6325,#6326,#4308,.T.);
#7976=EDGE_CURVE('',#6327,#6325,#1262,.F.);
#7977=EDGE_CURVE('',#6322,#6327,#1263,.F.);
#7978=EDGE_CURVE('',#6323,#6326,#1264,.T.);
#7979=EDGE_CURVE('',#6328,#6329,#4309,.T.);
#7980=EDGE_CURVE('',#6325,#6328,#1265,.F.);
#7981=EDGE_CURVE('',#6326,#6330,#1266,.T.);
#7982=EDGE_CURVE('',#6330,#6329,#1267,.T.);
#7983=EDGE_CURVE('',#6331,#6332,#4310,.T.);
#7984=EDGE_CURVE('',#6333,#6331,#1268,.F.);
#7985=EDGE_CURVE('',#6328,#6333,#1269,.F.);
#7986=EDGE_CURVE('',#6329,#6332,#1270,.T.);
#7987=EDGE_CURVE('',#6334,#6335,#4311,.T.);
#7988=EDGE_CURVE('',#6331,#6334,#1271,.F.);
#7989=EDGE_CURVE('',#6332,#6336,#1272,.T.);
#7990=EDGE_CURVE('',#6336,#6335,#1273,.T.);
#7991=EDGE_CURVE('',#6337,#6338,#4312,.T.);
#7992=EDGE_CURVE('',#6339,#6337,#1274,.F.);
#7993=EDGE_CURVE('',#6334,#6339,#1275,.F.);
#7994=EDGE_CURVE('',#6335,#6338,#1276,.T.);
#7995=EDGE_CURVE('',#6340,#6341,#4313,.T.);
#7996=EDGE_CURVE('',#6337,#6340,#1277,.F.);
#7997=EDGE_CURVE('',#6338,#6342,#1278,.T.);
#7998=EDGE_CURVE('',#6342,#6341,#1279,.T.);
#7999=EDGE_CURVE('',#6343,#6344,#4314,.T.);
#8000=EDGE_CURVE('',#6345,#6343,#1280,.F.);
#8001=EDGE_CURVE('',#6340,#6345,#1281,.F.);
#8002=EDGE_CURVE('',#6341,#6344,#1282,.T.);
#8003=EDGE_CURVE('',#6346,#6347,#4315,.T.);
#8004=EDGE_CURVE('',#6343,#6346,#1283,.F.);
#8005=EDGE_CURVE('',#6344,#6348,#1284,.T.);
#8006=EDGE_CURVE('',#6348,#6347,#1285,.T.);
#8007=EDGE_CURVE('',#6349,#6350,#4316,.T.);
#8008=EDGE_CURVE('',#6351,#6349,#1286,.F.);
#8009=EDGE_CURVE('',#6346,#6351,#1287,.F.);
#8010=EDGE_CURVE('',#6347,#6350,#1288,.T.);
#8011=EDGE_CURVE('',#6352,#6353,#4317,.T.);
#8012=EDGE_CURVE('',#6349,#6352,#1289,.F.);
#8013=EDGE_CURVE('',#6350,#6354,#1290,.T.);
#8014=EDGE_CURVE('',#6354,#6353,#1291,.T.);
#8015=EDGE_CURVE('',#6355,#6356,#4318,.T.);
#8016=EDGE_CURVE('',#6357,#6355,#1292,.F.);
#8017=EDGE_CURVE('',#6352,#6357,#1293,.F.);
#8018=EDGE_CURVE('',#6353,#6356,#1294,.T.);
#8019=EDGE_CURVE('',#6358,#6359,#4319,.T.);
#8020=EDGE_CURVE('',#6355,#6358,#1295,.F.);
#8021=EDGE_CURVE('',#6356,#6360,#1296,.T.);
#8022=EDGE_CURVE('',#6360,#6359,#1297,.T.);
#8023=EDGE_CURVE('',#6361,#6362,#4320,.T.);
#8024=EDGE_CURVE('',#6363,#6361,#1298,.F.);
#8025=EDGE_CURVE('',#6358,#6363,#1299,.F.);
#8026=EDGE_CURVE('',#6359,#6362,#1300,.T.);
#8027=EDGE_CURVE('',#6364,#6365,#4321,.T.);
#8028=EDGE_CURVE('',#6361,#6364,#1301,.F.);
#8029=EDGE_CURVE('',#6362,#6366,#1302,.T.);
#8030=EDGE_CURVE('',#6366,#6365,#1303,.T.);
#8031=EDGE_CURVE('',#6367,#6368,#4322,.T.);
#8032=EDGE_CURVE('',#6369,#6367,#1304,.F.);
#8033=EDGE_CURVE('',#6364,#6369,#1305,.F.);
#8034=EDGE_CURVE('',#6365,#6368,#1306,.T.);
#8035=EDGE_CURVE('',#6370,#6371,#4323,.T.);
#8036=EDGE_CURVE('',#6367,#6370,#1307,.F.);
#8037=EDGE_CURVE('',#6368,#6372,#1308,.T.);
#8038=EDGE_CURVE('',#6372,#6371,#1309,.T.);
#8039=EDGE_CURVE('',#6373,#6374,#4324,.T.);
#8040=EDGE_CURVE('',#6375,#6373,#1310,.T.);
#8041=EDGE_CURVE('',#6370,#6375,#1311,.F.);
#8042=EDGE_CURVE('',#6371,#6374,#1312,.T.);
#8043=EDGE_CURVE('',#6376,#6377,#4325,.T.);
#8044=EDGE_CURVE('',#6378,#6376,#1313,.F.);
#8045=EDGE_CURVE('',#6373,#6378,#1314,.T.);
#8046=EDGE_CURVE('',#6374,#6379,#1315,.T.);
#8047=EDGE_CURVE('',#6379,#6377,#1316,.T.);
#8048=EDGE_CURVE('',#6380,#6381,#4326,.T.);
#8049=EDGE_CURVE('',#6376,#6380,#1317,.F.);
#8050=EDGE_CURVE('',#6377,#6381,#1318,.T.);
#8051=EDGE_CURVE('',#6382,#6383,#4327,.T.);
#8052=EDGE_CURVE('',#6384,#6382,#1319,.F.);
#8053=EDGE_CURVE('',#6380,#6384,#1320,.F.);
#8054=EDGE_CURVE('',#6381,#6385,#1321,.T.);
#8055=EDGE_CURVE('',#6385,#6383,#1322,.T.);
#8056=EDGE_CURVE('',#6386,#6387,#4328,.T.);
#8057=EDGE_CURVE('',#6382,#6386,#1323,.F.);
#8058=EDGE_CURVE('',#6383,#6388,#1324,.T.);
#8059=EDGE_CURVE('',#6388,#6387,#1325,.T.);
#8060=EDGE_CURVE('',#6389,#6390,#4329,.T.);
#8061=EDGE_CURVE('',#6391,#6389,#1326,.F.);
#8062=EDGE_CURVE('',#6386,#6391,#1327,.F.);
#8063=EDGE_CURVE('',#6387,#6390,#1328,.T.);
#8064=EDGE_CURVE('',#6392,#6393,#4330,.T.);
#8065=EDGE_CURVE('',#6389,#6392,#1329,.F.);
#8066=EDGE_CURVE('',#6390,#6394,#1330,.T.);
#8067=EDGE_CURVE('',#6394,#6393,#1331,.T.);
#8068=EDGE_CURVE('',#6395,#6396,#1332,.T.);
#8069=EDGE_CURVE('',#6397,#6396,#3655,.T.);
#8070=EDGE_CURVE('',#6397,#6398,#1333,.T.);
#8071=EDGE_CURVE('',#6398,#6399,#1334,.T.);
#8072=EDGE_CURVE('',#6399,#6400,#1335,.T.);
#8073=EDGE_CURVE('',#6400,#6401,#1336,.T.);
#8074=EDGE_CURVE('',#6401,#6402,#1337,.T.);
#8075=EDGE_CURVE('',#6402,#6403,#1338,.T.);
#8076=EDGE_CURVE('',#6403,#6404,#1339,.T.);
#8077=EDGE_CURVE('',#6404,#6405,#1340,.T.);
#8078=EDGE_CURVE('',#6405,#6406,#1341,.T.);
#8079=EDGE_CURVE('',#6406,#6407,#1342,.T.);
#8080=EDGE_CURVE('',#6407,#6408,#1343,.T.);
#8081=EDGE_CURVE('',#6408,#6409,#1344,.T.);
#8082=EDGE_CURVE('',#6409,#6410,#1345,.T.);
#8083=EDGE_CURVE('',#6410,#6411,#1346,.T.);
#8084=EDGE_CURVE('',#6411,#6412,#1347,.T.);
#8085=EDGE_CURVE('',#6412,#6413,#1348,.T.);
#8086=EDGE_CURVE('',#6413,#6414,#1349,.T.);
#8087=EDGE_CURVE('',#6414,#6415,#1350,.T.);
#8088=EDGE_CURVE('',#6415,#6416,#1351,.T.);
#8089=EDGE_CURVE('',#6416,#6417,#1352,.T.);
#8090=EDGE_CURVE('',#6417,#6418,#1353,.T.);
#8091=EDGE_CURVE('',#6418,#6419,#1354,.T.);
#8092=EDGE_CURVE('',#6419,#6420,#1355,.T.);
#8093=EDGE_CURVE('',#6420,#6421,#1356,.T.);
#8094=EDGE_CURVE('',#6421,#6422,#1357,.T.);
#8095=EDGE_CURVE('',#6422,#6423,#1358,.T.);
#8096=EDGE_CURVE('',#6423,#6424,#1359,.T.);
#8097=EDGE_CURVE('',#6424,#6425,#1360,.T.);
#8098=EDGE_CURVE('',#6425,#6426,#1361,.T.);
#8099=EDGE_CURVE('',#6427,#6426,#3656,.T.);
#8100=EDGE_CURVE('',#6428,#6427,#3657,.T.);
#8101=EDGE_CURVE('',#6428,#6429,#1362,.T.);
#8102=EDGE_CURVE('',#6429,#6430,#1363,.T.);
#8103=EDGE_CURVE('',#6430,#6431,#1364,.T.);
#8104=EDGE_CURVE('',#6431,#6432,#1365,.T.);
#8105=EDGE_CURVE('',#6432,#6433,#1366,.T.);
#8106=EDGE_CURVE('',#6433,#6434,#1367,.T.);
#8107=EDGE_CURVE('',#6434,#6435,#1368,.T.);
#8108=EDGE_CURVE('',#6435,#6436,#1369,.T.);
#8109=EDGE_CURVE('',#6436,#6437,#1370,.T.);
#8110=EDGE_CURVE('',#6437,#6438,#1371,.T.);
#8111=EDGE_CURVE('',#6438,#6439,#1372,.T.);
#8112=EDGE_CURVE('',#6439,#6440,#1373,.T.);
#8113=EDGE_CURVE('',#6440,#6441,#1374,.T.);
#8114=EDGE_CURVE('',#6441,#6442,#1375,.T.);
#8115=EDGE_CURVE('',#6442,#6443,#1376,.T.);
#8116=EDGE_CURVE('',#6443,#6444,#1377,.T.);
#8117=EDGE_CURVE('',#6444,#6445,#1378,.T.);
#8118=EDGE_CURVE('',#6445,#6446,#1379,.T.);
#8119=EDGE_CURVE('',#6446,#6447,#1380,.T.);
#8120=EDGE_CURVE('',#6447,#6448,#1381,.T.);
#8121=EDGE_CURVE('',#6448,#6449,#1382,.T.);
#8122=EDGE_CURVE('',#6449,#6450,#1383,.T.);
#8123=EDGE_CURVE('',#6450,#6451,#1384,.T.);
#8124=EDGE_CURVE('',#6451,#6452,#1385,.T.);
#8125=EDGE_CURVE('',#6452,#6453,#1386,.T.);
#8126=EDGE_CURVE('',#6453,#6454,#1387,.T.);
#8127=EDGE_CURVE('',#6454,#6395,#1388,.T.);
#8128=EDGE_CURVE('',#6393,#6455,#1389,.T.);
#8129=EDGE_CURVE('',#6455,#6456,#1390,.T.);
#8130=EDGE_CURVE('',#6457,#6456,#3658,.T.);
#8131=EDGE_CURVE('',#6458,#6457,#1391,.T.);
#8132=EDGE_CURVE('',#6392,#6458,#1392,.F.);
#8133=EDGE_CURVE('',#6459,#6428,#3659,.T.);
#8134=EDGE_CURVE('',#6459,#6457,#1393,.T.);
#8135=EDGE_CURVE('',#6456,#6428,#1394,.T.);
#8136=EDGE_CURVE('',#6426,#6459,#1395,.T.);
#8137=EDGE_CURVE('',#6313,#6397,#1396,.T.);
#8138=EDGE_CURVE('',#6460,#6461,#3660,.T.);
#8139=EDGE_CURVE('',#6460,#6314,#1397,.T.);
#8140=EDGE_CURVE('',#6461,#6397,#3661,.T.);
#8141=EDGE_CURVE('',#6396,#6460,#1398,.T.);
#8142=EDGE_CURVE('',#6462,#6462,#3662,.T.);
#8143=EDGE_CURVE('',#6462,#6461,#3663,.T.);
#8144=EDGE_CURVE('',#6463,#6463,#3664,.T.);
#8145=EDGE_CURVE('',#6427,#6464,#4331,.T.);
#8146=EDGE_CURVE('',#6464,#6464,#3665,.T.);
#8147=EDGE_CURVE('',#6465,#6466,#4332,.T.);
#8148=EDGE_CURVE('',#6465,#6467,#4333,.T.);
#8149=EDGE_CURVE('',#6468,#6467,#4334,.T.);
#8150=EDGE_CURVE('',#6466,#6468,#859,.T.);
#8151=EDGE_CURVE('',#6468,#6469,#860,.T.);
#8152=EDGE_CURVE('',#6467,#6470,#4335,.T.);
#8153=EDGE_CURVE('',#6469,#6470,#4336,.T.);
#8154=EDGE_CURVE('',#6470,#6465,#3666,.T.);
#8155=EDGE_CURVE('',#6471,#6472,#861,.T.);
#8156=EDGE_CURVE('',#6472,#6473,#3667,.T.);
#8157=EDGE_CURVE('',#6473,#6474,#862,.T.);
#8158=EDGE_CURVE('',#6474,#6475,#863,.T.);
#8159=EDGE_CURVE('',#6475,#6476,#3668,.T.);
#8160=EDGE_CURVE('',#6476,#6477,#864,.T.);
#8161=EDGE_CURVE('',#6477,#6478,#865,.T.);
#8162=EDGE_CURVE('',#6478,#6479,#3669,.T.);
#8163=EDGE_CURVE('',#6479,#6480,#866,.T.);
#8164=EDGE_CURVE('',#6480,#6481,#867,.T.);
#8165=EDGE_CURVE('',#6481,#6482,#3670,.T.);
#8166=EDGE_CURVE('',#6482,#6483,#868,.T.);
#8167=EDGE_CURVE('',#6483,#6484,#869,.T.);
#8168=EDGE_CURVE('',#6484,#6485,#3671,.T.);
#8169=EDGE_CURVE('',#6485,#6486,#870,.T.);
#8170=EDGE_CURVE('',#6486,#6487,#871,.T.);
#8171=EDGE_CURVE('',#6487,#6488,#3672,.T.);
#8172=EDGE_CURVE('',#6488,#6489,#872,.T.);
#8173=EDGE_CURVE('',#6489,#6490,#873,.T.);
#8174=EDGE_CURVE('',#6490,#6491,#3673,.T.);
#8175=EDGE_CURVE('',#6491,#6492,#874,.T.);
#8176=EDGE_CURVE('',#6492,#6493,#875,.T.);
#8177=EDGE_CURVE('',#6493,#6494,#3674,.T.);
#8178=EDGE_CURVE('',#6494,#6495,#876,.T.);
#8179=EDGE_CURVE('',#6495,#6496,#877,.T.);
#8180=EDGE_CURVE('',#6496,#6497,#3675,.T.);
#8181=EDGE_CURVE('',#6497,#6498,#878,.T.);
#8182=EDGE_CURVE('',#6498,#6499,#879,.T.);
#8183=EDGE_CURVE('',#6499,#6500,#3676,.T.);
#8184=EDGE_CURVE('',#6500,#6501,#880,.T.);
#8185=EDGE_CURVE('',#6501,#6502,#881,.T.);
#8186=EDGE_CURVE('',#6502,#6503,#3677,.T.);
#8187=EDGE_CURVE('',#6503,#6504,#882,.T.);
#8188=EDGE_CURVE('',#6504,#6505,#883,.T.);
#8189=EDGE_CURVE('',#6505,#6506,#3678,.T.);
#8190=EDGE_CURVE('',#6506,#6507,#884,.T.);
#8191=EDGE_CURVE('',#6507,#6508,#885,.T.);
#8192=EDGE_CURVE('',#6508,#6509,#3679,.T.);
#8193=EDGE_CURVE('',#6509,#6510,#886,.T.);
#8194=EDGE_CURVE('',#6510,#6511,#887,.T.);
#8195=EDGE_CURVE('',#6511,#6512,#3680,.T.);
#8196=EDGE_CURVE('',#6512,#6513,#888,.T.);
#8197=EDGE_CURVE('',#6513,#6514,#889,.T.);
#8198=EDGE_CURVE('',#6514,#6515,#3681,.T.);
#8199=EDGE_CURVE('',#6515,#6516,#890,.T.);
#8200=EDGE_CURVE('',#6516,#6517,#891,.T.);
#8201=EDGE_CURVE('',#6517,#6518,#3682,.T.);
#8202=EDGE_CURVE('',#6518,#6519,#892,.T.);
#8203=EDGE_CURVE('',#6519,#6520,#893,.T.);
#8204=EDGE_CURVE('',#6520,#6521,#3683,.T.);
#8205=EDGE_CURVE('',#6521,#6522,#894,.T.);
#8206=EDGE_CURVE('',#6522,#6523,#895,.T.);
#8207=EDGE_CURVE('',#6523,#6524,#3684,.T.);
#8208=EDGE_CURVE('',#6524,#6525,#896,.T.);
#8209=EDGE_CURVE('',#6525,#6526,#897,.T.);
#8210=EDGE_CURVE('',#6526,#6466,#3685,.T.);
#8211=EDGE_CURVE('',#6469,#6527,#3686,.T.);
#8212=EDGE_CURVE('',#6527,#6528,#898,.T.);
#8213=EDGE_CURVE('',#6528,#6529,#899,.T.);
#8214=EDGE_CURVE('',#6529,#6530,#3687,.T.);
#8215=EDGE_CURVE('',#6530,#6531,#900,.T.);
#8216=EDGE_CURVE('',#6531,#6532,#901,.T.);
#8217=EDGE_CURVE('',#6532,#6533,#3688,.T.);
#8218=EDGE_CURVE('',#6533,#6534,#902,.T.);
#8219=EDGE_CURVE('',#6534,#6535,#903,.T.);
#8220=EDGE_CURVE('',#6535,#6536,#3689,.T.);
#8221=EDGE_CURVE('',#6536,#6537,#904,.T.);
#8222=EDGE_CURVE('',#6537,#6538,#905,.T.);
#8223=EDGE_CURVE('',#6538,#6539,#3690,.T.);
#8224=EDGE_CURVE('',#6539,#6540,#906,.T.);
#8225=EDGE_CURVE('',#6540,#6541,#907,.T.);
#8226=EDGE_CURVE('',#6541,#6542,#3691,.T.);
#8227=EDGE_CURVE('',#6542,#6543,#908,.T.);
#8228=EDGE_CURVE('',#6543,#6544,#909,.T.);
#8229=EDGE_CURVE('',#6544,#6545,#3692,.T.);
#8230=EDGE_CURVE('',#6545,#6546,#910,.T.);
#8231=EDGE_CURVE('',#6546,#6547,#911,.T.);
#8232=EDGE_CURVE('',#6547,#6548,#3693,.T.);
#8233=EDGE_CURVE('',#6548,#6549,#912,.T.);
#8234=EDGE_CURVE('',#6549,#6550,#913,.T.);
#8235=EDGE_CURVE('',#6550,#6551,#3694,.T.);
#8236=EDGE_CURVE('',#6551,#6552,#914,.T.);
#8237=EDGE_CURVE('',#6552,#6553,#915,.T.);
#8238=EDGE_CURVE('',#6553,#6554,#3695,.T.);
#8239=EDGE_CURVE('',#6554,#6555,#916,.T.);
#8240=EDGE_CURVE('',#6555,#6556,#917,.T.);
#8241=EDGE_CURVE('',#6556,#6557,#3696,.T.);
#8242=EDGE_CURVE('',#6557,#6558,#918,.T.);
#8243=EDGE_CURVE('',#6558,#6559,#919,.T.);
#8244=EDGE_CURVE('',#6559,#6560,#3697,.T.);
#8245=EDGE_CURVE('',#6560,#6561,#920,.T.);
#8246=EDGE_CURVE('',#6561,#6562,#921,.T.);
#8247=EDGE_CURVE('',#6562,#6563,#3698,.T.);
#8248=EDGE_CURVE('',#6563,#6564,#922,.T.);
#8249=EDGE_CURVE('',#6564,#6565,#923,.T.);
#8250=EDGE_CURVE('',#6565,#6566,#3699,.T.);
#8251=EDGE_CURVE('',#6566,#6567,#924,.T.);
#8252=EDGE_CURVE('',#6567,#6568,#925,.T.);
#8253=EDGE_CURVE('',#6568,#6569,#3700,.T.);
#8254=EDGE_CURVE('',#6569,#6570,#926,.T.);
#8255=EDGE_CURVE('',#6570,#6571,#927,.T.);
#8256=EDGE_CURVE('',#6571,#6572,#3701,.T.);
#8257=EDGE_CURVE('',#6572,#6573,#928,.T.);
#8258=EDGE_CURVE('',#6573,#6574,#929,.T.);
#8259=EDGE_CURVE('',#6574,#6575,#3702,.T.);
#8260=EDGE_CURVE('',#6575,#6471,#930,.T.);
#8261=EDGE_CURVE('',#6471,#6576,#4337,.T.);
#8262=EDGE_CURVE('',#6576,#6576,#3703,.T.);
#8263=EDGE_CURVE('',#6577,#6578,#3704,.T.);
#8264=EDGE_CURVE('',#6579,#6577,#4338,.T.);
#8265=EDGE_CURVE('',#6578,#6579,#4339,.T.);
#8266=EDGE_CURVE('',#6578,#6527,#4340,.T.);
#8267=EDGE_CURVE('',#6528,#6579,#4341,.T.);
#8268=EDGE_CURVE('',#6529,#6577,#4342,.T.);
#8269=EDGE_CURVE('',#6580,#6581,#3705,.T.);
#8270=EDGE_CURVE('',#6581,#6463,#4343,.T.);
#8271=EDGE_CURVE('',#6581,#6582,#3706,.T.);
#8272=EDGE_CURVE('',#6582,#6575,#4344,.T.);
#8273=EDGE_CURVE('',#6574,#6583,#4345,.T.);
#8274=EDGE_CURVE('',#6583,#6584,#3707,.T.);
#8275=EDGE_CURVE('',#6584,#6572,#4346,.T.);
#8276=EDGE_CURVE('',#6571,#6585,#4347,.T.);
#8277=EDGE_CURVE('',#6585,#6586,#3708,.T.);
#8278=EDGE_CURVE('',#6586,#6569,#4348,.T.);
#8279=EDGE_CURVE('',#6568,#6587,#4349,.T.);
#8280=EDGE_CURVE('',#6587,#6588,#3709,.T.);
#8281=EDGE_CURVE('',#6588,#6566,#4350,.T.);
#8282=EDGE_CURVE('',#6565,#6589,#4351,.T.);
#8283=EDGE_CURVE('',#6589,#6590,#3710,.T.);
#8284=EDGE_CURVE('',#6590,#6563,#4352,.T.);
#8285=EDGE_CURVE('',#6562,#6591,#4353,.T.);
#8286=EDGE_CURVE('',#6591,#6592,#3711,.T.);
#8287=EDGE_CURVE('',#6592,#6560,#4354,.T.);
#8288=EDGE_CURVE('',#6559,#6593,#4355,.T.);
#8289=EDGE_CURVE('',#6593,#6594,#3712,.T.);
#8290=EDGE_CURVE('',#6594,#6557,#4356,.T.);
#8291=EDGE_CURVE('',#6556,#6595,#4357,.T.);
#8292=EDGE_CURVE('',#6595,#6596,#3713,.T.);
#8293=EDGE_CURVE('',#6596,#6554,#4358,.T.);
#8294=EDGE_CURVE('',#6553,#6597,#4359,.T.);
#8295=EDGE_CURVE('',#6597,#6598,#3714,.T.);
#8296=EDGE_CURVE('',#6598,#6551,#4360,.T.);
#8297=EDGE_CURVE('',#6550,#6599,#4361,.T.);
#8298=EDGE_CURVE('',#6599,#6600,#3715,.T.);
#8299=EDGE_CURVE('',#6600,#6548,#4362,.T.);
#8300=EDGE_CURVE('',#6547,#6601,#4363,.T.);
#8301=EDGE_CURVE('',#6601,#6602,#3716,.T.);
#8302=EDGE_CURVE('',#6602,#6545,#4364,.T.);
#8303=EDGE_CURVE('',#6544,#6603,#4365,.T.);
#8304=EDGE_CURVE('',#6603,#6604,#3717,.T.);
#8305=EDGE_CURVE('',#6604,#6542,#4366,.T.);
#8306=EDGE_CURVE('',#6541,#6605,#4367,.T.);
#8307=EDGE_CURVE('',#6605,#6606,#3718,.T.);
#8308=EDGE_CURVE('',#6606,#6539,#4368,.T.);
#8309=EDGE_CURVE('',#6538,#6607,#4369,.T.);
#8310=EDGE_CURVE('',#6607,#6608,#3719,.T.);
#8311=EDGE_CURVE('',#6608,#6536,#4370,.T.);
#8312=EDGE_CURVE('',#6535,#6609,#4371,.T.);
#8313=EDGE_CURVE('',#6609,#6610,#3720,.T.);
#8314=EDGE_CURVE('',#6610,#6533,#4372,.T.);
#8315=EDGE_CURVE('',#6532,#6611,#4373,.T.);
#8316=EDGE_CURVE('',#6611,#6612,#3721,.T.);
#8317=EDGE_CURVE('',#6612,#6530,#4374,.T.);
#8318=EDGE_CURVE('',#6526,#6613,#4375,.T.);
#8319=EDGE_CURVE('',#6613,#6614,#3722,.T.);
#8320=EDGE_CURVE('',#6614,#6524,#4376,.T.);
#8321=EDGE_CURVE('',#6523,#6615,#4377,.T.);
#8322=EDGE_CURVE('',#6615,#6616,#3723,.T.);
#8323=EDGE_CURVE('',#6616,#6521,#4378,.T.);
#8324=EDGE_CURVE('',#6520,#6617,#4379,.T.);
#8325=EDGE_CURVE('',#6617,#6618,#3724,.T.);
#8326=EDGE_CURVE('',#6618,#6518,#4380,.T.);
#8327=EDGE_CURVE('',#6517,#6619,#4381,.T.);
#8328=EDGE_CURVE('',#6619,#6620,#3725,.T.);
#8329=EDGE_CURVE('',#6620,#6515,#4382,.T.);
#8330=EDGE_CURVE('',#6514,#6621,#4383,.T.);
#8331=EDGE_CURVE('',#6621,#6622,#3726,.T.);
#8332=EDGE_CURVE('',#6622,#6512,#4384,.T.);
#8333=EDGE_CURVE('',#6511,#6623,#4385,.T.);
#8334=EDGE_CURVE('',#6623,#6624,#3727,.T.);
#8335=EDGE_CURVE('',#6624,#6509,#4386,.T.);
#8336=EDGE_CURVE('',#6508,#6625,#4387,.T.);
#8337=EDGE_CURVE('',#6625,#6626,#3728,.T.);
#8338=EDGE_CURVE('',#6626,#6506,#4388,.T.);
#8339=EDGE_CURVE('',#6505,#6627,#4389,.T.);
#8340=EDGE_CURVE('',#6627,#6628,#3729,.T.);
#8341=EDGE_CURVE('',#6628,#6503,#4390,.T.);
#8342=EDGE_CURVE('',#6502,#6629,#4391,.T.);
#8343=EDGE_CURVE('',#6629,#6630,#3730,.T.);
#8344=EDGE_CURVE('',#6630,#6500,#4392,.T.);
#8345=EDGE_CURVE('',#6499,#6631,#4393,.T.);
#8346=EDGE_CURVE('',#6631,#6632,#3731,.T.);
#8347=EDGE_CURVE('',#6632,#6497,#4394,.T.);
#8348=EDGE_CURVE('',#6496,#6633,#4395,.T.);
#8349=EDGE_CURVE('',#6633,#6634,#3732,.T.);
#8350=EDGE_CURVE('',#6634,#6494,#4396,.T.);
#8351=EDGE_CURVE('',#6493,#6635,#4397,.T.);
#8352=EDGE_CURVE('',#6635,#6636,#3733,.T.);
#8353=EDGE_CURVE('',#6636,#6491,#4398,.T.);
#8354=EDGE_CURVE('',#6490,#6637,#4399,.T.);
#8355=EDGE_CURVE('',#6637,#6638,#3734,.T.);
#8356=EDGE_CURVE('',#6638,#6488,#4400,.T.);
#8357=EDGE_CURVE('',#6487,#6639,#4401,.T.);
#8358=EDGE_CURVE('',#6639,#6640,#3735,.T.);
#8359=EDGE_CURVE('',#6640,#6485,#4402,.T.);
#8360=EDGE_CURVE('',#6484,#6641,#4403,.T.);
#8361=EDGE_CURVE('',#6641,#6642,#3736,.T.);
#8362=EDGE_CURVE('',#6642,#6482,#4404,.T.);
#8363=EDGE_CURVE('',#6481,#6643,#4405,.T.);
#8364=EDGE_CURVE('',#6643,#6644,#3737,.T.);
#8365=EDGE_CURVE('',#6644,#6479,#4406,.T.);
#8366=EDGE_CURVE('',#6478,#6645,#4407,.T.);
#8367=EDGE_CURVE('',#6645,#6646,#3738,.T.);
#8368=EDGE_CURVE('',#6646,#6476,#4408,.T.);
#8369=EDGE_CURVE('',#6475,#6647,#4409,.T.);
#8370=EDGE_CURVE('',#6647,#6648,#3739,.T.);
#8371=EDGE_CURVE('',#6648,#6473,#4410,.T.);
#8372=EDGE_CURVE('',#6472,#6580,#4411,.T.);
#8373=EDGE_CURVE('',#6612,#6649,#4412,.T.);
#8374=EDGE_CURVE('',#6531,#6649,#4413,.T.);
#8375=EDGE_CURVE('',#6649,#6611,#4414,.T.);
#8376=EDGE_CURVE('',#6650,#6609,#4415,.T.);
#8377=EDGE_CURVE('',#6610,#6650,#4416,.T.);
#8378=EDGE_CURVE('',#6534,#6650,#4417,.T.);
#8379=EDGE_CURVE('',#6608,#6651,#4418,.T.);
#8380=EDGE_CURVE('',#6537,#6651,#4419,.T.);
#8381=EDGE_CURVE('',#6651,#6607,#4420,.T.);
#8382=EDGE_CURVE('',#6652,#6605,#4421,.T.);
#8383=EDGE_CURVE('',#6606,#6652,#4422,.T.);
#8384=EDGE_CURVE('',#6540,#6652,#4423,.T.);
#8385=EDGE_CURVE('',#6604,#6653,#4424,.T.);
#8386=EDGE_CURVE('',#6543,#6653,#4425,.T.);
#8387=EDGE_CURVE('',#6653,#6603,#4426,.T.);
#8388=EDGE_CURVE('',#6654,#6601,#4427,.T.);
#8389=EDGE_CURVE('',#6602,#6654,#4428,.T.);
#8390=EDGE_CURVE('',#6546,#6654,#4429,.T.);
#8391=EDGE_CURVE('',#6600,#6655,#4430,.T.);
#8392=EDGE_CURVE('',#6549,#6655,#4431,.T.);
#8393=EDGE_CURVE('',#6655,#6599,#4432,.T.);
#8394=EDGE_CURVE('',#6656,#6597,#4433,.T.);
#8395=EDGE_CURVE('',#6598,#6656,#4434,.T.);
#8396=EDGE_CURVE('',#6552,#6656,#4435,.T.);
#8397=EDGE_CURVE('',#6596,#6657,#4436,.T.);
#8398=EDGE_CURVE('',#6555,#6657,#4437,.T.);
#8399=EDGE_CURVE('',#6657,#6595,#4438,.T.);
#8400=EDGE_CURVE('',#6658,#6593,#4439,.T.);
#8401=EDGE_CURVE('',#6594,#6658,#4440,.T.);
#8402=EDGE_CURVE('',#6558,#6658,#4441,.T.);
#8403=EDGE_CURVE('',#6592,#6659,#4442,.T.);
#8404=EDGE_CURVE('',#6561,#6659,#4443,.T.);
#8405=EDGE_CURVE('',#6659,#6591,#4444,.T.);
#8406=EDGE_CURVE('',#6660,#6589,#4445,.T.);
#8407=EDGE_CURVE('',#6590,#6660,#4446,.T.);
#8408=EDGE_CURVE('',#6564,#6660,#4447,.T.);
#8409=EDGE_CURVE('',#6588,#6661,#4448,.T.);
#8410=EDGE_CURVE('',#6567,#6661,#4449,.T.);
#8411=EDGE_CURVE('',#6661,#6587,#4450,.T.);
#8412=EDGE_CURVE('',#6662,#6585,#4451,.T.);
#8413=EDGE_CURVE('',#6586,#6662,#4452,.T.);
#8414=EDGE_CURVE('',#6570,#6662,#4453,.T.);
#8415=EDGE_CURVE('',#6584,#6663,#4454,.T.);
#8416=EDGE_CURVE('',#6573,#6663,#4455,.T.);
#8417=EDGE_CURVE('',#6663,#6583,#4456,.T.);
#8418=EDGE_CURVE('',#6664,#6580,#4457,.T.);
#8419=EDGE_CURVE('',#6582,#6664,#4458,.T.);
#8420=EDGE_CURVE('',#6471,#6664,#4459,.T.);
#8421=EDGE_CURVE('',#6648,#6665,#4460,.T.);
#8422=EDGE_CURVE('',#6474,#6665,#4461,.T.);
#8423=EDGE_CURVE('',#6665,#6647,#4462,.T.);
#8424=EDGE_CURVE('',#6666,#6645,#4463,.T.);
#8425=EDGE_CURVE('',#6646,#6666,#4464,.T.);
#8426=EDGE_CURVE('',#6477,#6666,#4465,.T.);
#8427=EDGE_CURVE('',#6644,#6667,#4466,.T.);
#8428=EDGE_CURVE('',#6480,#6667,#4467,.T.);
#8429=EDGE_CURVE('',#6667,#6643,#4468,.T.);
#8430=EDGE_CURVE('',#6668,#6641,#4469,.T.);
#8431=EDGE_CURVE('',#6642,#6668,#4470,.T.);
#8432=EDGE_CURVE('',#6483,#6668,#4471,.T.);
#8433=EDGE_CURVE('',#6640,#6669,#4472,.T.);
#8434=EDGE_CURVE('',#6486,#6669,#4473,.T.);
#8435=EDGE_CURVE('',#6669,#6639,#4474,.T.);
#8436=EDGE_CURVE('',#6670,#6637,#4475,.T.);
#8437=EDGE_CURVE('',#6638,#6670,#4476,.T.);
#8438=EDGE_CURVE('',#6489,#6670,#4477,.T.);
#8439=EDGE_CURVE('',#6636,#6671,#4478,.T.);
#8440=EDGE_CURVE('',#6492,#6671,#4479,.T.);
#8441=EDGE_CURVE('',#6671,#6635,#4480,.T.);
#8442=EDGE_CURVE('',#6672,#6633,#4481,.T.);
#8443=EDGE_CURVE('',#6634,#6672,#4482,.T.);
#8444=EDGE_CURVE('',#6495,#6672,#4483,.T.);
#8445=EDGE_CURVE('',#6632,#6673,#4484,.T.);
#8446=EDGE_CURVE('',#6498,#6673,#4485,.T.);
#8447=EDGE_CURVE('',#6673,#6631,#4486,.T.);
#8448=EDGE_CURVE('',#6674,#6629,#4487,.T.);
#8449=EDGE_CURVE('',#6630,#6674,#4488,.T.);
#8450=EDGE_CURVE('',#6501,#6674,#4489,.T.);
#8451=EDGE_CURVE('',#6628,#6675,#4490,.T.);
#8452=EDGE_CURVE('',#6504,#6675,#4491,.T.);
#8453=EDGE_CURVE('',#6675,#6627,#4492,.T.);
#8454=EDGE_CURVE('',#6676,#6625,#4493,.T.);
#8455=EDGE_CURVE('',#6626,#6676,#4494,.T.);
#8456=EDGE_CURVE('',#6507,#6676,#4495,.T.);
#8457=EDGE_CURVE('',#6624,#6677,#4496,.T.);
#8458=EDGE_CURVE('',#6510,#6677,#4497,.T.);
#8459=EDGE_CURVE('',#6677,#6623,#4498,.T.);
#8460=EDGE_CURVE('',#6678,#6621,#4499,.T.);
#8461=EDGE_CURVE('',#6622,#6678,#4500,.T.);
#8462=EDGE_CURVE('',#6513,#6678,#4501,.T.);
#8463=EDGE_CURVE('',#6620,#6679,#4502,.T.);
#8464=EDGE_CURVE('',#6516,#6679,#4503,.T.);
#8465=EDGE_CURVE('',#6679,#6619,#4504,.T.);
#8466=EDGE_CURVE('',#6680,#6617,#4505,.T.);
#8467=EDGE_CURVE('',#6618,#6680,#4506,.T.);
#8468=EDGE_CURVE('',#6519,#6680,#4507,.T.);
#8469=EDGE_CURVE('',#6616,#6681,#4508,.T.);
#8470=EDGE_CURVE('',#6522,#6681,#4509,.T.);
#8471=EDGE_CURVE('',#6681,#6615,#4510,.T.);
#8472=EDGE_CURVE('',#6682,#6613,#4511,.T.);
#8473=EDGE_CURVE('',#6614,#6682,#4512,.T.);
#8474=EDGE_CURVE('',#6525,#6682,#4513,.T.);
#8475=EDGE_CURVE('',#6683,#6684,#4514,.T.);
#8476=EDGE_CURVE('',#6684,#6685,#4515,.T.);
#8477=EDGE_CURVE('',#6685,#6686,#4516,.T.);
#8478=EDGE_CURVE('',#6686,#6687,#4517,.T.);
#8479=EDGE_CURVE('',#6687,#6688,#4518,.T.);
#8480=EDGE_CURVE('',#6688,#6683,#4519,.T.);
#8481=EDGE_CURVE('',#6689,#6690,#4520,.T.);
#8482=EDGE_CURVE('',#6690,#6689,#3740,.T.);
#8483=EDGE_CURVE('',#6690,#6691,#4521,.T.);
#8484=EDGE_CURVE('',#6691,#6690,#3741,.T.);
#8485=EDGE_CURVE('',#6691,#6692,#4522,.T.);
#8486=EDGE_CURVE('',#6692,#6691,#3742,.T.);
#8487=EDGE_CURVE('',#6692,#6693,#4523,.T.);
#8488=EDGE_CURVE('',#6693,#6692,#3743,.T.);
#8489=EDGE_CURVE('',#6693,#6694,#4524,.T.);
#8490=EDGE_CURVE('',#6694,#6693,#3744,.T.);
#8491=EDGE_CURVE('',#6694,#6689,#4525,.T.);
#8492=EDGE_CURVE('',#6689,#6694,#3745,.T.);
#8493=EDGE_CURVE('',#6695,#6692,#4526,.T.);
#8494=EDGE_CURVE('',#6683,#6689,#4527,.T.);
#8495=EDGE_CURVE('',#6684,#6690,#4528,.T.);
#8496=EDGE_CURVE('',#6688,#6694,#4529,.T.);
#8497=EDGE_CURVE('',#6687,#6693,#4530,.T.);
#8498=EDGE_CURVE('',#6686,#6692,#4531,.T.);
#8499=EDGE_CURVE('',#6685,#6691,#4532,.T.);
#8500=EDGE_CURVE('',#6696,#6697,#4533,.T.);
#8501=EDGE_CURVE('',#6698,#6696,#1399,.T.);
#8502=EDGE_CURVE('',#6699,#6698,#3746,.T.);
#8503=EDGE_CURVE('',#6699,#6697,#1400,.T.);
#8504=EDGE_CURVE('',#6700,#6701,#4534,.T.);
#8505=EDGE_CURVE('',#6702,#6700,#1401,.F.);
#8506=EDGE_CURVE('',#6696,#6702,#1402,.T.);
#8507=EDGE_CURVE('',#6697,#6703,#1403,.T.);
#8508=EDGE_CURVE('',#6703,#6701,#1404,.T.);
#8509=EDGE_CURVE('',#6704,#6705,#4535,.T.);
#8510=EDGE_CURVE('',#6700,#6704,#1405,.F.);
#8511=EDGE_CURVE('',#6701,#6706,#1406,.T.);
#8512=EDGE_CURVE('',#6706,#6705,#1407,.T.);
#8513=EDGE_CURVE('',#6707,#6708,#4536,.T.);
#8514=EDGE_CURVE('',#6709,#6707,#1408,.T.);
#8515=EDGE_CURVE('',#6704,#6709,#1409,.F.);
#8516=EDGE_CURVE('',#6705,#6710,#1410,.T.);
#8517=EDGE_CURVE('',#6710,#6708,#1411,.T.);
#8518=EDGE_CURVE('',#6711,#6712,#4537,.T.);
#8519=EDGE_CURVE('',#6713,#6711,#1412,.F.);
#8520=EDGE_CURVE('',#6707,#6713,#1413,.T.);
#8521=EDGE_CURVE('',#6708,#6712,#1414,.T.);
#8522=EDGE_CURVE('',#6714,#6715,#4538,.T.);
#8523=EDGE_CURVE('',#6711,#6714,#1415,.F.);
#8524=EDGE_CURVE('',#6712,#6716,#1416,.T.);
#8525=EDGE_CURVE('',#6716,#6715,#1417,.T.);
#8526=EDGE_CURVE('',#6717,#6718,#4539,.T.);
#8527=EDGE_CURVE('',#6719,#6717,#1418,.F.);
#8528=EDGE_CURVE('',#6714,#6719,#1419,.F.);
#8529=EDGE_CURVE('',#6715,#6718,#1420,.T.);
#8530=EDGE_CURVE('',#6720,#6721,#4540,.T.);
#8531=EDGE_CURVE('',#6717,#6720,#1421,.F.);
#8532=EDGE_CURVE('',#6718,#6722,#1422,.T.);
#8533=EDGE_CURVE('',#6722,#6721,#1423,.T.);
#8534=EDGE_CURVE('',#6723,#6724,#4541,.T.);
#8535=EDGE_CURVE('',#6725,#6723,#1424,.F.);
#8536=EDGE_CURVE('',#6720,#6725,#1425,.F.);
#8537=EDGE_CURVE('',#6721,#6724,#1426,.T.);
#8538=EDGE_CURVE('',#6726,#6727,#4542,.T.);
#8539=EDGE_CURVE('',#6723,#6726,#1427,.F.);
#8540=EDGE_CURVE('',#6724,#6728,#1428,.T.);
#8541=EDGE_CURVE('',#6728,#6727,#1429,.T.);
#8542=EDGE_CURVE('',#6729,#6730,#4543,.T.);
#8543=EDGE_CURVE('',#6731,#6729,#1430,.T.);
#8544=EDGE_CURVE('',#6726,#6731,#1431,.F.);
#8545=EDGE_CURVE('',#6727,#6732,#1432,.T.);
#8546=EDGE_CURVE('',#6732,#6730,#1433,.T.);
#8547=EDGE_CURVE('',#6733,#6734,#4544,.T.);
#8548=EDGE_CURVE('',#6735,#6733,#1434,.T.);
#8549=EDGE_CURVE('',#6729,#6735,#1435,.T.);
#8550=EDGE_CURVE('',#6730,#6734,#1436,.T.);
#8551=EDGE_CURVE('',#6736,#6737,#4545,.T.);
#8552=EDGE_CURVE('',#6738,#6736,#1437,.F.);
#8553=EDGE_CURVE('',#6733,#6738,#1438,.T.);
#8554=EDGE_CURVE('',#6734,#6737,#1439,.T.);
#8555=EDGE_CURVE('',#6739,#6740,#4546,.T.);
#8556=EDGE_CURVE('',#6736,#6739,#1440,.F.);
#8557=EDGE_CURVE('',#6737,#6740,#1441,.T.);
#8558=EDGE_CURVE('',#6741,#6742,#1442,.T.);
#8559=EDGE_CURVE('',#6743,#6742,#3747,.T.);
#8560=EDGE_CURVE('',#6743,#6744,#1443,.T.);
#8561=EDGE_CURVE('',#6744,#6745,#1444,.T.);
#8562=EDGE_CURVE('',#6745,#6746,#1445,.T.);
#8563=EDGE_CURVE('',#6746,#6747,#1446,.T.);
#8564=EDGE_CURVE('',#6747,#6748,#1447,.T.);
#8565=EDGE_CURVE('',#6748,#6749,#1448,.T.);
#8566=EDGE_CURVE('',#6749,#6750,#1449,.T.);
#8567=EDGE_CURVE('',#6750,#6751,#1450,.T.);
#8568=EDGE_CURVE('',#6751,#6752,#1451,.T.);
#8569=EDGE_CURVE('',#6752,#6753,#1452,.T.);
#8570=EDGE_CURVE('',#6753,#6754,#1453,.T.);
#8571=EDGE_CURVE('',#6754,#6755,#1454,.T.);
#8572=EDGE_CURVE('',#6755,#6756,#1455,.T.);
#8573=EDGE_CURVE('',#6756,#6757,#1456,.T.);
#8574=EDGE_CURVE('',#6757,#6758,#1457,.T.);
#8575=EDGE_CURVE('',#6758,#6759,#1458,.T.);
#8576=EDGE_CURVE('',#6760,#6759,#3748,.T.);
#8577=EDGE_CURVE('',#6760,#6761,#1459,.T.);
#8578=EDGE_CURVE('',#6761,#6762,#1460,.T.);
#8579=EDGE_CURVE('',#6762,#6763,#1461,.T.);
#8580=EDGE_CURVE('',#6763,#6764,#1462,.T.);
#8581=EDGE_CURVE('',#6764,#6765,#1463,.T.);
#8582=EDGE_CURVE('',#6765,#6766,#1464,.T.);
#8583=EDGE_CURVE('',#6766,#6767,#1465,.T.);
#8584=EDGE_CURVE('',#6767,#6768,#1466,.T.);
#8585=EDGE_CURVE('',#6768,#6769,#1467,.T.);
#8586=EDGE_CURVE('',#6769,#6770,#1468,.T.);
#8587=EDGE_CURVE('',#6770,#6771,#1469,.T.);
#8588=EDGE_CURVE('',#6771,#6772,#1470,.T.);
#8589=EDGE_CURVE('',#6772,#6773,#1471,.T.);
#8590=EDGE_CURVE('',#6773,#6774,#1472,.T.);
#8591=EDGE_CURVE('',#6774,#6741,#1473,.T.);
#8592=EDGE_CURVE('',#6740,#6775,#1474,.T.);
#8593=EDGE_CURVE('',#6776,#6775,#3749,.T.);
#8594=EDGE_CURVE('',#6777,#6776,#1475,.T.);
#8595=EDGE_CURVE('',#6739,#6777,#1476,.F.);
#8596=EDGE_CURVE('',#6778,#6779,#3750,.T.);
#8597=EDGE_CURVE('',#6778,#6776,#1477,.T.);
#8598=EDGE_CURVE('',#6775,#6780,#1478,.T.);
#8599=EDGE_CURVE('',#6780,#6760,#1479,.T.);
#8600=EDGE_CURVE('',#6779,#6760,#3751,.T.);
#8601=EDGE_CURVE('',#6759,#6778,#1480,.T.);
#8602=EDGE_CURVE('',#6698,#6743,#1481,.T.);
#8603=EDGE_CURVE('',#6781,#6782,#3752,.T.);
#8604=EDGE_CURVE('',#6781,#6699,#1482,.T.);
#8605=EDGE_CURVE('',#6782,#6743,#3753,.T.);
#8606=EDGE_CURVE('',#6742,#6781,#1483,.T.);
#8607=EDGE_CURVE('',#6783,#6783,#3754,.T.);
#8608=EDGE_CURVE('',#6783,#6782,#3755,.T.);
#8609=EDGE_CURVE('',#6784,#6784,#3756,.T.);
#8610=EDGE_CURVE('',#6779,#6785,#4547,.T.);
#8611=EDGE_CURVE('',#6785,#6785,#3757,.T.);
#8612=EDGE_CURVE('',#6786,#6787,#4548,.T.);
#8613=EDGE_CURVE('',#6786,#6788,#4549,.T.);
#8614=EDGE_CURVE('',#6789,#6788,#4550,.T.);
#8615=EDGE_CURVE('',#6787,#6789,#931,.T.);
#8616=EDGE_CURVE('',#6790,#6791,#4551,.T.);
#8617=EDGE_CURVE('',#6789,#6790,#932,.T.);
#8618=EDGE_CURVE('',#6788,#6791,#4552,.T.);
#8619=EDGE_CURVE('',#6791,#6786,#3758,.T.);
#8620=EDGE_CURVE('',#6792,#6793,#933,.T.);
#8621=EDGE_CURVE('',#6793,#6794,#3759,.T.);
#8622=EDGE_CURVE('',#6794,#6795,#934,.T.);
#8623=EDGE_CURVE('',#6795,#6796,#935,.T.);
#8624=EDGE_CURVE('',#6796,#6797,#3760,.T.);
#8625=EDGE_CURVE('',#6797,#6798,#936,.T.);
#8626=EDGE_CURVE('',#6798,#6799,#937,.T.);
#8627=EDGE_CURVE('',#6799,#6800,#3761,.T.);
#8628=EDGE_CURVE('',#6800,#6801,#938,.T.);
#8629=EDGE_CURVE('',#6801,#6802,#939,.T.);
#8630=EDGE_CURVE('',#6802,#6803,#3762,.T.);
#8631=EDGE_CURVE('',#6803,#6804,#940,.T.);
#8632=EDGE_CURVE('',#6804,#6805,#941,.T.);
#8633=EDGE_CURVE('',#6805,#6806,#3763,.T.);
#8634=EDGE_CURVE('',#6806,#6807,#942,.T.);
#8635=EDGE_CURVE('',#6807,#6808,#943,.T.);
#8636=EDGE_CURVE('',#6808,#6809,#3764,.T.);
#8637=EDGE_CURVE('',#6809,#6810,#944,.T.);
#8638=EDGE_CURVE('',#6810,#6811,#945,.T.);
#8639=EDGE_CURVE('',#6811,#6812,#3765,.T.);
#8640=EDGE_CURVE('',#6812,#6813,#946,.T.);
#8641=EDGE_CURVE('',#6813,#6814,#947,.T.);
#8642=EDGE_CURVE('',#6814,#6815,#3766,.T.);
#8643=EDGE_CURVE('',#6815,#6816,#948,.T.);
#8644=EDGE_CURVE('',#6816,#6817,#949,.T.);
#8645=EDGE_CURVE('',#6817,#6818,#3767,.T.);
#8646=EDGE_CURVE('',#6818,#6819,#950,.T.);
#8647=EDGE_CURVE('',#6819,#6820,#951,.T.);
#8648=EDGE_CURVE('',#6820,#6821,#3768,.T.);
#8649=EDGE_CURVE('',#6821,#6822,#952,.T.);
#8650=EDGE_CURVE('',#6822,#6823,#953,.T.);
#8651=EDGE_CURVE('',#6823,#6824,#3769,.T.);
#8652=EDGE_CURVE('',#6824,#6825,#954,.T.);
#8653=EDGE_CURVE('',#6825,#6826,#955,.T.);
#8654=EDGE_CURVE('',#6826,#6827,#3770,.T.);
#8655=EDGE_CURVE('',#6827,#6828,#956,.T.);
#8656=EDGE_CURVE('',#6828,#6829,#957,.T.);
#8657=EDGE_CURVE('',#6829,#6830,#3771,.T.);
#8658=EDGE_CURVE('',#6830,#6831,#958,.T.);
#8659=EDGE_CURVE('',#6831,#6832,#959,.T.);
#8660=EDGE_CURVE('',#6832,#6833,#3772,.T.);
#8661=EDGE_CURVE('',#6833,#6834,#960,.T.);
#8662=EDGE_CURVE('',#6834,#6835,#961,.T.);
#8663=EDGE_CURVE('',#6835,#6836,#3773,.T.);
#8664=EDGE_CURVE('',#6836,#6837,#962,.T.);
#8665=EDGE_CURVE('',#6837,#6838,#963,.T.);
#8666=EDGE_CURVE('',#6838,#6839,#3774,.T.);
#8667=EDGE_CURVE('',#6839,#6840,#964,.T.);
#8668=EDGE_CURVE('',#6840,#6841,#965,.T.);
#8669=EDGE_CURVE('',#6841,#6842,#3775,.T.);
#8670=EDGE_CURVE('',#6842,#6843,#966,.T.);
#8671=EDGE_CURVE('',#6843,#6844,#967,.T.);
#8672=EDGE_CURVE('',#6844,#6845,#3776,.T.);
#8673=EDGE_CURVE('',#6845,#6846,#968,.T.);
#8674=EDGE_CURVE('',#6846,#6847,#969,.T.);
#8675=EDGE_CURVE('',#6847,#6787,#3777,.T.);
#8676=EDGE_CURVE('',#6790,#6848,#3778,.T.);
#8677=EDGE_CURVE('',#6848,#6849,#970,.T.);
#8678=EDGE_CURVE('',#6849,#6850,#971,.T.);
#8679=EDGE_CURVE('',#6850,#6851,#3779,.T.);
#8680=EDGE_CURVE('',#6851,#6852,#972,.T.);
#8681=EDGE_CURVE('',#6852,#6853,#973,.T.);
#8682=EDGE_CURVE('',#6853,#6854,#3780,.T.);
#8683=EDGE_CURVE('',#6854,#6855,#974,.T.);
#8684=EDGE_CURVE('',#6855,#6856,#975,.T.);
#8685=EDGE_CURVE('',#6856,#6857,#3781,.T.);
#8686=EDGE_CURVE('',#6857,#6858,#976,.T.);
#8687=EDGE_CURVE('',#6858,#6859,#977,.T.);
#8688=EDGE_CURVE('',#6859,#6860,#3782,.T.);
#8689=EDGE_CURVE('',#6860,#6861,#978,.T.);
#8690=EDGE_CURVE('',#6861,#6862,#979,.T.);
#8691=EDGE_CURVE('',#6862,#6863,#3783,.T.);
#8692=EDGE_CURVE('',#6863,#6864,#980,.T.);
#8693=EDGE_CURVE('',#6864,#6865,#981,.T.);
#8694=EDGE_CURVE('',#6865,#6866,#3784,.T.);
#8695=EDGE_CURVE('',#6866,#6867,#982,.T.);
#8696=EDGE_CURVE('',#6867,#6868,#983,.T.);
#8697=EDGE_CURVE('',#6868,#6869,#3785,.T.);
#8698=EDGE_CURVE('',#6869,#6870,#984,.T.);
#8699=EDGE_CURVE('',#6870,#6871,#985,.T.);
#8700=EDGE_CURVE('',#6871,#6872,#3786,.T.);
#8701=EDGE_CURVE('',#6872,#6873,#986,.T.);
#8702=EDGE_CURVE('',#6873,#6874,#987,.T.);
#8703=EDGE_CURVE('',#6874,#6875,#3787,.T.);
#8704=EDGE_CURVE('',#6875,#6876,#988,.T.);
#8705=EDGE_CURVE('',#6876,#6877,#989,.T.);
#8706=EDGE_CURVE('',#6877,#6878,#3788,.T.);
#8707=EDGE_CURVE('',#6878,#6879,#990,.T.);
#8708=EDGE_CURVE('',#6879,#6880,#991,.T.);
#8709=EDGE_CURVE('',#6880,#6881,#3789,.T.);
#8710=EDGE_CURVE('',#6881,#6882,#992,.T.);
#8711=EDGE_CURVE('',#6882,#6883,#993,.T.);
#8712=EDGE_CURVE('',#6883,#6884,#3790,.T.);
#8713=EDGE_CURVE('',#6884,#6885,#994,.T.);
#8714=EDGE_CURVE('',#6885,#6886,#995,.T.);
#8715=EDGE_CURVE('',#6886,#6887,#3791,.T.);
#8716=EDGE_CURVE('',#6887,#6888,#996,.T.);
#8717=EDGE_CURVE('',#6888,#6889,#997,.T.);
#8718=EDGE_CURVE('',#6889,#6890,#3792,.T.);
#8719=EDGE_CURVE('',#6890,#6891,#998,.T.);
#8720=EDGE_CURVE('',#6891,#6892,#999,.T.);
#8721=EDGE_CURVE('',#6892,#6893,#3793,.T.);
#8722=EDGE_CURVE('',#6893,#6894,#1000,.T.);
#8723=EDGE_CURVE('',#6894,#6895,#1001,.T.);
#8724=EDGE_CURVE('',#6895,#6896,#3794,.T.);
#8725=EDGE_CURVE('',#6896,#6792,#1002,.T.);
#8726=EDGE_CURVE('',#6792,#6897,#4553,.T.);
#8727=EDGE_CURVE('',#6897,#6897,#3795,.T.);
#8728=EDGE_CURVE('',#6898,#6848,#4554,.T.);
#8729=EDGE_CURVE('',#6898,#6899,#4555,.T.);
#8730=EDGE_CURVE('',#6849,#6899,#4556,.T.);
#8731=EDGE_CURVE('',#6850,#6900,#4557,.T.);
#8732=EDGE_CURVE('',#6899,#6900,#4558,.T.);
#8733=EDGE_CURVE('',#6900,#6898,#3796,.T.);
#8734=EDGE_CURVE('',#6901,#6851,#4559,.T.);
#8735=EDGE_CURVE('',#6901,#6902,#4560,.T.);
#8736=EDGE_CURVE('',#6852,#6902,#4561,.T.);
#8737=EDGE_CURVE('',#6853,#6903,#4562,.T.);
#8738=EDGE_CURVE('',#6902,#6903,#4563,.T.);
#8739=EDGE_CURVE('',#6903,#6901,#3797,.T.);
#8740=EDGE_CURVE('',#6904,#6854,#4564,.T.);
#8741=EDGE_CURVE('',#6904,#6905,#4565,.T.);
#8742=EDGE_CURVE('',#6855,#6905,#4566,.T.);
#8743=EDGE_CURVE('',#6856,#6906,#4567,.T.);
#8744=EDGE_CURVE('',#6905,#6906,#4568,.T.);
#8745=EDGE_CURVE('',#6906,#6904,#3798,.T.);
#8746=EDGE_CURVE('',#6907,#6857,#4569,.T.);
#8747=EDGE_CURVE('',#6907,#6908,#4570,.T.);
#8748=EDGE_CURVE('',#6858,#6908,#4571,.T.);
#8749=EDGE_CURVE('',#6859,#6909,#4572,.T.);
#8750=EDGE_CURVE('',#6908,#6909,#4573,.T.);
#8751=EDGE_CURVE('',#6909,#6907,#3799,.T.);
#8752=EDGE_CURVE('',#6910,#6860,#4574,.T.);
#8753=EDGE_CURVE('',#6910,#6911,#4575,.T.);
#8754=EDGE_CURVE('',#6861,#6911,#4576,.T.);
#8755=EDGE_CURVE('',#6862,#6912,#4577,.T.);
#8756=EDGE_CURVE('',#6911,#6912,#4578,.T.);
#8757=EDGE_CURVE('',#6912,#6910,#3800,.T.);
#8758=EDGE_CURVE('',#6913,#6863,#4579,.T.);
#8759=EDGE_CURVE('',#6913,#6914,#4580,.T.);
#8760=EDGE_CURVE('',#6864,#6914,#4581,.T.);
#8761=EDGE_CURVE('',#6865,#6915,#4582,.T.);
#8762=EDGE_CURVE('',#6914,#6915,#4583,.T.);
#8763=EDGE_CURVE('',#6915,#6913,#3801,.T.);
#8764=EDGE_CURVE('',#6916,#6866,#4584,.T.);
#8765=EDGE_CURVE('',#6916,#6917,#4585,.T.);
#8766=EDGE_CURVE('',#6867,#6917,#4586,.T.);
#8767=EDGE_CURVE('',#6868,#6918,#4587,.T.);
#8768=EDGE_CURVE('',#6917,#6918,#4588,.T.);
#8769=EDGE_CURVE('',#6918,#6916,#3802,.T.);
#8770=EDGE_CURVE('',#6919,#6869,#4589,.T.);
#8771=EDGE_CURVE('',#6919,#6920,#4590,.T.);
#8772=EDGE_CURVE('',#6870,#6920,#4591,.T.);
#8773=EDGE_CURVE('',#6871,#6921,#4592,.T.);
#8774=EDGE_CURVE('',#6920,#6921,#4593,.T.);
#8775=EDGE_CURVE('',#6921,#6919,#3803,.T.);
#8776=EDGE_CURVE('',#6922,#6872,#4594,.T.);
#8777=EDGE_CURVE('',#6922,#6923,#4595,.T.);
#8778=EDGE_CURVE('',#6873,#6923,#4596,.T.);
#8779=EDGE_CURVE('',#6874,#6924,#4597,.T.);
#8780=EDGE_CURVE('',#6923,#6924,#4598,.T.);
#8781=EDGE_CURVE('',#6924,#6922,#3804,.T.);
#8782=EDGE_CURVE('',#6925,#6875,#4599,.T.);
#8783=EDGE_CURVE('',#6925,#6926,#4600,.T.);
#8784=EDGE_CURVE('',#6876,#6926,#4601,.T.);
#8785=EDGE_CURVE('',#6877,#6927,#4602,.T.);
#8786=EDGE_CURVE('',#6926,#6927,#4603,.T.);
#8787=EDGE_CURVE('',#6927,#6925,#3805,.T.);
#8788=EDGE_CURVE('',#6928,#6878,#4604,.T.);
#8789=EDGE_CURVE('',#6928,#6929,#4605,.T.);
#8790=EDGE_CURVE('',#6879,#6929,#4606,.T.);
#8791=EDGE_CURVE('',#6880,#6930,#4607,.T.);
#8792=EDGE_CURVE('',#6929,#6930,#4608,.T.);
#8793=EDGE_CURVE('',#6930,#6928,#3806,.T.);
#8794=EDGE_CURVE('',#6931,#6881,#4609,.T.);
#8795=EDGE_CURVE('',#6931,#6932,#4610,.T.);
#8796=EDGE_CURVE('',#6882,#6932,#4611,.T.);
#8797=EDGE_CURVE('',#6883,#6933,#4612,.T.);
#8798=EDGE_CURVE('',#6932,#6933,#4613,.T.);
#8799=EDGE_CURVE('',#6933,#6931,#3807,.T.);
#8800=EDGE_CURVE('',#6934,#6884,#4614,.T.);
#8801=EDGE_CURVE('',#6934,#6935,#4615,.T.);
#8802=EDGE_CURVE('',#6885,#6935,#4616,.T.);
#8803=EDGE_CURVE('',#6886,#6936,#4617,.T.);
#8804=EDGE_CURVE('',#6935,#6936,#4618,.T.);
#8805=EDGE_CURVE('',#6936,#6934,#3808,.T.);
#8806=EDGE_CURVE('',#6937,#6887,#4619,.T.);
#8807=EDGE_CURVE('',#6937,#6938,#4620,.T.);
#8808=EDGE_CURVE('',#6888,#6938,#4621,.T.);
#8809=EDGE_CURVE('',#6889,#6939,#4622,.T.);
#8810=EDGE_CURVE('',#6938,#6939,#4623,.T.);
#8811=EDGE_CURVE('',#6939,#6937,#3809,.T.);
#8812=EDGE_CURVE('',#6940,#6890,#4624,.T.);
#8813=EDGE_CURVE('',#6940,#6941,#4625,.T.);
#8814=EDGE_CURVE('',#6891,#6941,#4626,.T.);
#8815=EDGE_CURVE('',#6892,#6942,#4627,.T.);
#8816=EDGE_CURVE('',#6941,#6942,#4628,.T.);
#8817=EDGE_CURVE('',#6942,#6940,#3810,.T.);
#8818=EDGE_CURVE('',#6943,#6893,#4629,.T.);
#8819=EDGE_CURVE('',#6943,#6944,#4630,.T.);
#8820=EDGE_CURVE('',#6894,#6944,#4631,.T.);
#8821=EDGE_CURVE('',#6895,#6945,#4632,.T.);
#8822=EDGE_CURVE('',#6944,#6945,#4633,.T.);
#8823=EDGE_CURVE('',#6945,#6943,#3811,.T.);
#8824=EDGE_CURVE('',#6946,#6896,#4634,.T.);
#8825=EDGE_CURVE('',#6946,#6947,#4635,.T.);
#8826=EDGE_CURVE('',#6792,#6947,#4636,.T.);
#8827=EDGE_CURVE('',#6793,#6948,#4637,.T.);
#8828=EDGE_CURVE('',#6947,#6948,#4638,.T.);
#8829=EDGE_CURVE('',#6948,#6949,#3812,.T.);
#8830=EDGE_CURVE('',#6949,#6946,#3813,.T.);
#8831=EDGE_CURVE('',#6950,#6794,#4639,.T.);
#8832=EDGE_CURVE('',#6950,#6951,#4640,.T.);
#8833=EDGE_CURVE('',#6795,#6951,#4641,.T.);
#8834=EDGE_CURVE('',#6796,#6952,#4642,.T.);
#8835=EDGE_CURVE('',#6951,#6952,#4643,.T.);
#8836=EDGE_CURVE('',#6952,#6950,#3814,.T.);
#8837=EDGE_CURVE('',#6953,#6797,#4644,.T.);
#8838=EDGE_CURVE('',#6953,#6954,#4645,.T.);
#8839=EDGE_CURVE('',#6798,#6954,#4646,.T.);
#8840=EDGE_CURVE('',#6799,#6955,#4647,.T.);
#8841=EDGE_CURVE('',#6954,#6955,#4648,.T.);
#8842=EDGE_CURVE('',#6955,#6953,#3815,.T.);
#8843=EDGE_CURVE('',#6956,#6800,#4649,.T.);
#8844=EDGE_CURVE('',#6956,#6957,#4650,.T.);
#8845=EDGE_CURVE('',#6801,#6957,#4651,.T.);
#8846=EDGE_CURVE('',#6802,#6958,#4652,.T.);
#8847=EDGE_CURVE('',#6957,#6958,#4653,.T.);
#8848=EDGE_CURVE('',#6958,#6956,#3816,.T.);
#8849=EDGE_CURVE('',#6959,#6803,#4654,.T.);
#8850=EDGE_CURVE('',#6959,#6960,#4655,.T.);
#8851=EDGE_CURVE('',#6804,#6960,#4656,.T.);
#8852=EDGE_CURVE('',#6805,#6961,#4657,.T.);
#8853=EDGE_CURVE('',#6960,#6961,#4658,.T.);
#8854=EDGE_CURVE('',#6961,#6959,#3817,.T.);
#8855=EDGE_CURVE('',#6962,#6806,#4659,.T.);
#8856=EDGE_CURVE('',#6962,#6963,#4660,.T.);
#8857=EDGE_CURVE('',#6807,#6963,#4661,.T.);
#8858=EDGE_CURVE('',#6808,#6964,#4662,.T.);
#8859=EDGE_CURVE('',#6963,#6964,#4663,.T.);
#8860=EDGE_CURVE('',#6964,#6962,#3818,.T.);
#8861=EDGE_CURVE('',#6965,#6809,#4664,.T.);
#8862=EDGE_CURVE('',#6965,#6966,#4665,.T.);
#8863=EDGE_CURVE('',#6810,#6966,#4666,.T.);
#8864=EDGE_CURVE('',#6811,#6967,#4667,.T.);
#8865=EDGE_CURVE('',#6966,#6967,#4668,.T.);
#8866=EDGE_CURVE('',#6967,#6965,#3819,.T.);
#8867=EDGE_CURVE('',#6968,#6812,#4669,.T.);
#8868=EDGE_CURVE('',#6968,#6969,#4670,.T.);
#8869=EDGE_CURVE('',#6813,#6969,#4671,.T.);
#8870=EDGE_CURVE('',#6814,#6970,#4672,.T.);
#8871=EDGE_CURVE('',#6969,#6970,#4673,.T.);
#8872=EDGE_CURVE('',#6970,#6968,#3820,.T.);
#8873=EDGE_CURVE('',#6971,#6815,#4674,.T.);
#8874=EDGE_CURVE('',#6971,#6972,#4675,.T.);
#8875=EDGE_CURVE('',#6816,#6972,#4676,.T.);
#8876=EDGE_CURVE('',#6817,#6973,#4677,.T.);
#8877=EDGE_CURVE('',#6972,#6973,#4678,.T.);
#8878=EDGE_CURVE('',#6973,#6971,#3821,.T.);
#8879=EDGE_CURVE('',#6974,#6818,#4679,.T.);
#8880=EDGE_CURVE('',#6974,#6975,#4680,.T.);
#8881=EDGE_CURVE('',#6819,#6975,#4681,.T.);
#8882=EDGE_CURVE('',#6820,#6976,#4682,.T.);
#8883=EDGE_CURVE('',#6975,#6976,#4683,.T.);
#8884=EDGE_CURVE('',#6976,#6974,#3822,.T.);
#8885=EDGE_CURVE('',#6977,#6821,#4684,.T.);
#8886=EDGE_CURVE('',#6977,#6978,#4685,.T.);
#8887=EDGE_CURVE('',#6822,#6978,#4686,.T.);
#8888=EDGE_CURVE('',#6823,#6979,#4687,.T.);
#8889=EDGE_CURVE('',#6978,#6979,#4688,.T.);
#8890=EDGE_CURVE('',#6979,#6977,#3823,.T.);
#8891=EDGE_CURVE('',#6980,#6824,#4689,.T.);
#8892=EDGE_CURVE('',#6980,#6981,#4690,.T.);
#8893=EDGE_CURVE('',#6825,#6981,#4691,.T.);
#8894=EDGE_CURVE('',#6826,#6982,#4692,.T.);
#8895=EDGE_CURVE('',#6981,#6982,#4693,.T.);
#8896=EDGE_CURVE('',#6982,#6980,#3824,.T.);
#8897=EDGE_CURVE('',#6983,#6827,#4694,.T.);
#8898=EDGE_CURVE('',#6983,#6984,#4695,.T.);
#8899=EDGE_CURVE('',#6828,#6984,#4696,.T.);
#8900=EDGE_CURVE('',#6829,#6985,#4697,.T.);
#8901=EDGE_CURVE('',#6984,#6985,#4698,.T.);
#8902=EDGE_CURVE('',#6985,#6983,#3825,.T.);
#8903=EDGE_CURVE('',#6986,#6830,#4699,.T.);
#8904=EDGE_CURVE('',#6986,#6987,#4700,.T.);
#8905=EDGE_CURVE('',#6831,#6987,#4701,.T.);
#8906=EDGE_CURVE('',#6832,#6988,#4702,.T.);
#8907=EDGE_CURVE('',#6987,#6988,#4703,.T.);
#8908=EDGE_CURVE('',#6988,#6986,#3826,.T.);
#8909=EDGE_CURVE('',#6989,#6833,#4704,.T.);
#8910=EDGE_CURVE('',#6989,#6990,#4705,.T.);
#8911=EDGE_CURVE('',#6834,#6990,#4706,.T.);
#8912=EDGE_CURVE('',#6835,#6991,#4707,.T.);
#8913=EDGE_CURVE('',#6990,#6991,#4708,.T.);
#8914=EDGE_CURVE('',#6991,#6989,#3827,.T.);
#8915=EDGE_CURVE('',#6992,#6836,#4709,.T.);
#8916=EDGE_CURVE('',#6992,#6993,#4710,.T.);
#8917=EDGE_CURVE('',#6837,#6993,#4711,.T.);
#8918=EDGE_CURVE('',#6838,#6994,#4712,.T.);
#8919=EDGE_CURVE('',#6993,#6994,#4713,.T.);
#8920=EDGE_CURVE('',#6994,#6992,#3828,.T.);
#8921=EDGE_CURVE('',#6995,#6839,#4714,.T.);
#8922=EDGE_CURVE('',#6995,#6996,#4715,.T.);
#8923=EDGE_CURVE('',#6840,#6996,#4716,.T.);
#8924=EDGE_CURVE('',#6841,#6997,#4717,.T.);
#8925=EDGE_CURVE('',#6996,#6997,#4718,.T.);
#8926=EDGE_CURVE('',#6997,#6995,#3829,.T.);
#8927=EDGE_CURVE('',#6998,#6842,#4719,.T.);
#8928=EDGE_CURVE('',#6998,#6999,#4720,.T.);
#8929=EDGE_CURVE('',#6843,#6999,#4721,.T.);
#8930=EDGE_CURVE('',#6844,#7000,#4722,.T.);
#8931=EDGE_CURVE('',#6999,#7000,#4723,.T.);
#8932=EDGE_CURVE('',#7000,#6998,#3830,.T.);
#8933=EDGE_CURVE('',#7001,#6845,#4724,.T.);
#8934=EDGE_CURVE('',#7001,#7002,#4725,.T.);
#8935=EDGE_CURVE('',#6846,#7002,#4726,.T.);
#8936=EDGE_CURVE('',#6847,#7003,#4727,.T.);
#8937=EDGE_CURVE('',#7002,#7003,#4728,.T.);
#8938=EDGE_CURVE('',#7003,#7001,#3831,.T.);
#8939=EDGE_CURVE('',#6949,#6784,#4729,.T.);
#8940=EDGE_CURVE('',#7004,#7005,#4730,.T.);
#8941=EDGE_CURVE('',#7005,#7006,#4731,.T.);
#8942=EDGE_CURVE('',#7006,#7007,#4732,.T.);
#8943=EDGE_CURVE('',#7007,#7008,#4733,.T.);
#8944=EDGE_CURVE('',#7008,#7009,#4734,.T.);
#8945=EDGE_CURVE('',#7009,#7004,#4735,.T.);
#8946=EDGE_CURVE('',#7010,#7011,#4736,.T.);
#8947=EDGE_CURVE('',#7010,#7011,#3832,.T.);
#8948=EDGE_CURVE('',#7011,#7012,#4737,.T.);
#8949=EDGE_CURVE('',#7011,#7012,#3833,.T.);
#8950=EDGE_CURVE('',#7012,#7013,#4738,.T.);
#8951=EDGE_CURVE('',#7012,#7013,#3834,.T.);
#8952=EDGE_CURVE('',#7013,#7014,#4739,.T.);
#8953=EDGE_CURVE('',#7013,#7014,#3835,.T.);
#8954=EDGE_CURVE('',#7014,#7015,#4740,.T.);
#8955=EDGE_CURVE('',#7014,#7015,#3836,.T.);
#8956=EDGE_CURVE('',#7015,#7010,#4741,.T.);
#8957=EDGE_CURVE('',#7015,#7010,#3837,.T.);
#8958=EDGE_CURVE('',#7016,#7010,#4742,.T.);
#8959=EDGE_CURVE('',#7004,#7010,#4743,.T.);
#8960=EDGE_CURVE('',#7005,#7011,#4744,.T.);
#8961=EDGE_CURVE('',#7009,#7015,#4745,.T.);
#8962=EDGE_CURVE('',#7008,#7014,#4746,.T.);
#8963=EDGE_CURVE('',#7007,#7013,#4747,.T.);
#8964=EDGE_CURVE('',#7006,#7012,#4748,.T.);
#8965=ORIENTED_EDGE('',*,*,#7017,.F.);
#8966=ORIENTED_EDGE('',*,*,#7018,.T.);
#8967=ORIENTED_EDGE('',*,*,#7019,.T.);
#8968=ORIENTED_EDGE('',*,*,#7018,.F.);
#8969=ORIENTED_EDGE('',*,*,#7019,.F.);
#8970=ORIENTED_EDGE('',*,*,#7020,.T.);
#8971=ORIENTED_EDGE('',*,*,#7020,.F.);
#8972=ORIENTED_EDGE('',*,*,#7021,.T.);
#8973=ORIENTED_EDGE('',*,*,#7022,.F.);
#8974=ORIENTED_EDGE('',*,*,#7023,.F.);
#8975=ORIENTED_EDGE('',*,*,#7021,.F.);
#8976=ORIENTED_EDGE('',*,*,#7024,.F.);
#8977=ORIENTED_EDGE('',*,*,#7025,.T.);
#8978=ORIENTED_EDGE('',*,*,#7026,.T.);
#8979=ORIENTED_EDGE('',*,*,#7025,.F.);
#8980=ORIENTED_EDGE('',*,*,#7026,.F.);
#8981=ORIENTED_EDGE('',*,*,#7027,.T.);
#8982=ORIENTED_EDGE('',*,*,#7027,.F.);
#8983=ORIENTED_EDGE('',*,*,#7028,.T.);
#8984=ORIENTED_EDGE('',*,*,#7029,.F.);
#8985=ORIENTED_EDGE('',*,*,#7030,.F.);
#8986=ORIENTED_EDGE('',*,*,#7028,.F.);
#8987=ORIENTED_EDGE('',*,*,#7031,.F.);
#8988=ORIENTED_EDGE('',*,*,#7032,.T.);
#8989=ORIENTED_EDGE('',*,*,#7033,.T.);
#8990=ORIENTED_EDGE('',*,*,#7032,.F.);
#8991=ORIENTED_EDGE('',*,*,#7033,.F.);
#8992=ORIENTED_EDGE('',*,*,#7034,.T.);
#8993=ORIENTED_EDGE('',*,*,#7034,.F.);
#8994=ORIENTED_EDGE('',*,*,#7035,.T.);
#8995=ORIENTED_EDGE('',*,*,#7036,.F.);
#8996=ORIENTED_EDGE('',*,*,#7037,.F.);
#8997=ORIENTED_EDGE('',*,*,#7035,.F.);
#8998=ORIENTED_EDGE('',*,*,#7038,.F.);
#8999=ORIENTED_EDGE('',*,*,#7039,.T.);
#9000=ORIENTED_EDGE('',*,*,#7040,.T.);
#9001=ORIENTED_EDGE('',*,*,#7039,.F.);
#9002=ORIENTED_EDGE('',*,*,#7040,.F.);
#9003=ORIENTED_EDGE('',*,*,#7041,.T.);
#9004=ORIENTED_EDGE('',*,*,#7041,.F.);
#9005=ORIENTED_EDGE('',*,*,#7042,.T.);
#9006=ORIENTED_EDGE('',*,*,#7043,.F.);
#9007=ORIENTED_EDGE('',*,*,#7044,.F.);
#9008=ORIENTED_EDGE('',*,*,#7042,.F.);
#9009=ORIENTED_EDGE('',*,*,#7045,.F.);
#9010=ORIENTED_EDGE('',*,*,#7046,.T.);
#9011=ORIENTED_EDGE('',*,*,#7047,.T.);
#9012=ORIENTED_EDGE('',*,*,#7046,.F.);
#9013=ORIENTED_EDGE('',*,*,#7047,.F.);
#9014=ORIENTED_EDGE('',*,*,#7048,.T.);
#9015=ORIENTED_EDGE('',*,*,#7048,.F.);
#9016=ORIENTED_EDGE('',*,*,#7049,.T.);
#9017=ORIENTED_EDGE('',*,*,#7050,.F.);
#9018=ORIENTED_EDGE('',*,*,#7051,.F.);
#9019=ORIENTED_EDGE('',*,*,#7049,.F.);
#9020=ORIENTED_EDGE('',*,*,#7052,.F.);
#9021=ORIENTED_EDGE('',*,*,#7053,.T.);
#9022=ORIENTED_EDGE('',*,*,#7054,.T.);
#9023=ORIENTED_EDGE('',*,*,#7053,.F.);
#9024=ORIENTED_EDGE('',*,*,#7054,.F.);
#9025=ORIENTED_EDGE('',*,*,#7055,.T.);
#9026=ORIENTED_EDGE('',*,*,#7055,.F.);
#9027=ORIENTED_EDGE('',*,*,#7056,.T.);
#9028=ORIENTED_EDGE('',*,*,#7057,.F.);
#9029=ORIENTED_EDGE('',*,*,#7058,.F.);
#9030=ORIENTED_EDGE('',*,*,#7056,.F.);
#9031=ORIENTED_EDGE('',*,*,#7059,.T.);
#9032=ORIENTED_EDGE('',*,*,#7060,.T.);
#9033=ORIENTED_EDGE('',*,*,#7061,.T.);
#9034=ORIENTED_EDGE('',*,*,#7060,.F.);
#9035=ORIENTED_EDGE('',*,*,#7062,.T.);
#9036=ORIENTED_EDGE('',*,*,#7063,.T.);
#9037=ORIENTED_EDGE('',*,*,#7064,.F.);
#9038=ORIENTED_EDGE('',*,*,#7065,.F.);
#9039=ORIENTED_EDGE('',*,*,#7066,.F.);
#9040=ORIENTED_EDGE('',*,*,#7067,.F.);
#9041=ORIENTED_EDGE('',*,*,#7068,.F.);
#9042=ORIENTED_EDGE('',*,*,#7061,.F.);
#9043=ORIENTED_EDGE('',*,*,#7059,.F.);
#9044=ORIENTED_EDGE('',*,*,#7069,.T.);
#9045=ORIENTED_EDGE('',*,*,#7070,.T.);
#9046=ORIENTED_EDGE('',*,*,#7069,.F.);
#9047=ORIENTED_EDGE('',*,*,#7071,.T.);
#9048=ORIENTED_EDGE('',*,*,#7072,.T.);
#9049=ORIENTED_EDGE('',*,*,#7066,.T.);
#9050=ORIENTED_EDGE('',*,*,#7072,.F.);
#9051=ORIENTED_EDGE('',*,*,#7071,.F.);
#9052=ORIENTED_EDGE('',*,*,#7073,.T.);
#9053=ORIENTED_EDGE('',*,*,#7074,.T.);
#9054=ORIENTED_EDGE('',*,*,#7073,.F.);
#9055=ORIENTED_EDGE('',*,*,#7075,.T.);
#9056=ORIENTED_EDGE('',*,*,#7076,.T.);
#9057=ORIENTED_EDGE('',*,*,#7068,.T.);
#9058=ORIENTED_EDGE('',*,*,#7076,.F.);
#9059=ORIENTED_EDGE('',*,*,#7075,.F.);
#9060=ORIENTED_EDGE('',*,*,#7077,.T.);
#9061=ORIENTED_EDGE('',*,*,#7078,.T.);
#9062=ORIENTED_EDGE('',*,*,#7077,.F.);
#9063=ORIENTED_EDGE('',*,*,#7079,.T.);
#9064=ORIENTED_EDGE('',*,*,#7080,.T.);
#9065=ORIENTED_EDGE('',*,*,#7067,.T.);
#9066=ORIENTED_EDGE('',*,*,#7080,.F.);
#9067=ORIENTED_EDGE('',*,*,#7079,.F.);
#9068=ORIENTED_EDGE('',*,*,#7081,.T.);
#9069=ORIENTED_EDGE('',*,*,#7082,.T.);
#9070=ORIENTED_EDGE('',*,*,#7081,.F.);
#9071=ORIENTED_EDGE('',*,*,#7082,.F.);
#9072=ORIENTED_EDGE('',*,*,#7083,.F.);
#9073=ORIENTED_EDGE('',*,*,#7078,.F.);
#9074=ORIENTED_EDGE('',*,*,#7084,.F.);
#9075=ORIENTED_EDGE('',*,*,#7074,.F.);
#9076=ORIENTED_EDGE('',*,*,#7085,.F.);
#9077=ORIENTED_EDGE('',*,*,#7070,.F.);
#9078=ORIENTED_EDGE('',*,*,#7086,.F.);
#9079=ORIENTED_EDGE('',*,*,#7083,.T.);
#9080=ORIENTED_EDGE('',*,*,#7087,.T.);
#9081=ORIENTED_EDGE('',*,*,#7088,.F.);
#9082=ORIENTED_EDGE('',*,*,#7087,.F.);
#9083=ORIENTED_EDGE('',*,*,#7084,.T.);
#9084=ORIENTED_EDGE('',*,*,#7089,.T.);
#9085=ORIENTED_EDGE('',*,*,#7090,.F.);
#9086=ORIENTED_EDGE('',*,*,#7089,.F.);
#9087=ORIENTED_EDGE('',*,*,#7085,.T.);
#9088=ORIENTED_EDGE('',*,*,#7091,.T.);
#9089=ORIENTED_EDGE('',*,*,#7092,.F.);
#9090=ORIENTED_EDGE('',*,*,#7091,.F.);
#9091=ORIENTED_EDGE('',*,*,#7086,.T.);
#9092=ORIENTED_EDGE('',*,*,#7093,.T.);
#9093=ORIENTED_EDGE('',*,*,#7094,.F.);
#9094=ORIENTED_EDGE('',*,*,#7093,.F.);
#9095=ORIENTED_EDGE('',*,*,#7095,.T.);
#9096=ORIENTED_EDGE('',*,*,#7096,.T.);
#9097=ORIENTED_EDGE('',*,*,#7097,.T.);
#9098=ORIENTED_EDGE('',*,*,#7098,.T.);
#9099=ORIENTED_EDGE('',*,*,#7098,.F.);
#9100=ORIENTED_EDGE('',*,*,#7099,.T.);
#9101=ORIENTED_EDGE('',*,*,#7065,.T.);
#9102=ORIENTED_EDGE('',*,*,#7100,.F.);
#9103=ORIENTED_EDGE('',*,*,#7097,.F.);
#9104=ORIENTED_EDGE('',*,*,#7101,.F.);
#9105=ORIENTED_EDGE('',*,*,#7102,.F.);
#9106=ORIENTED_EDGE('',*,*,#7103,.T.);
#9107=ORIENTED_EDGE('',*,*,#7104,.F.);
#9108=ORIENTED_EDGE('',*,*,#7105,.F.);
#9109=ORIENTED_EDGE('',*,*,#7106,.F.);
#9110=ORIENTED_EDGE('',*,*,#7107,.T.);
#9111=ORIENTED_EDGE('',*,*,#7108,.F.);
#9112=ORIENTED_EDGE('',*,*,#7109,.T.);
#9113=ORIENTED_EDGE('',*,*,#7110,.T.);
#9114=ORIENTED_EDGE('',*,*,#7111,.T.);
#9115=ORIENTED_EDGE('',*,*,#7112,.T.);
#9116=ORIENTED_EDGE('',*,*,#7113,.T.);
#9117=ORIENTED_EDGE('',*,*,#7114,.F.);
#9118=ORIENTED_EDGE('',*,*,#7115,.T.);
#9119=ORIENTED_EDGE('',*,*,#7062,.F.);
#9120=ORIENTED_EDGE('',*,*,#7099,.F.);
#9121=ORIENTED_EDGE('',*,*,#7116,.T.);
#9122=ORIENTED_EDGE('',*,*,#7117,.T.);
#9123=ORIENTED_EDGE('',*,*,#7114,.T.);
#9124=ORIENTED_EDGE('',*,*,#7118,.T.);
#9125=ORIENTED_EDGE('',*,*,#7118,.F.);
#9126=ORIENTED_EDGE('',*,*,#7113,.F.);
#9127=ORIENTED_EDGE('',*,*,#7119,.T.);
#9128=ORIENTED_EDGE('',*,*,#7120,.F.);
#9129=ORIENTED_EDGE('',*,*,#7121,.T.);
#9130=ORIENTED_EDGE('',*,*,#7122,.T.);
#9131=ORIENTED_EDGE('',*,*,#7108,.T.);
#9132=ORIENTED_EDGE('',*,*,#7123,.T.);
#9133=ORIENTED_EDGE('',*,*,#7123,.F.);
#9134=ORIENTED_EDGE('',*,*,#7107,.F.);
#9135=ORIENTED_EDGE('',*,*,#7124,.F.);
#9136=ORIENTED_EDGE('',*,*,#7125,.F.);
#9137=ORIENTED_EDGE('',*,*,#7024,.T.);
#9138=ORIENTED_EDGE('',*,*,#7094,.T.);
#9139=ORIENTED_EDGE('',*,*,#7092,.T.);
#9140=ORIENTED_EDGE('',*,*,#7090,.T.);
#9141=ORIENTED_EDGE('',*,*,#7088,.T.);
#9142=ORIENTED_EDGE('',*,*,#7052,.T.);
#9143=ORIENTED_EDGE('',*,*,#7045,.T.);
#9144=ORIENTED_EDGE('',*,*,#7038,.T.);
#9145=ORIENTED_EDGE('',*,*,#7031,.T.);
#9146=ORIENTED_EDGE('',*,*,#7017,.T.);
#9147=ORIENTED_EDGE('',*,*,#7126,.T.);
#9148=ORIENTED_EDGE('',*,*,#7124,.T.);
#9149=ORIENTED_EDGE('',*,*,#7106,.T.);
#9150=ORIENTED_EDGE('',*,*,#7127,.T.);
#9151=ORIENTED_EDGE('',*,*,#7103,.F.);
#9152=ORIENTED_EDGE('',*,*,#7128,.T.);
#9153=ORIENTED_EDGE('',*,*,#7129,.F.);
#9154=ORIENTED_EDGE('',*,*,#7130,.F.);
#9155=ORIENTED_EDGE('',*,*,#7022,.T.);
#9156=ORIENTED_EDGE('',*,*,#7023,.T.);
#9157=ORIENTED_EDGE('',*,*,#7029,.T.);
#9158=ORIENTED_EDGE('',*,*,#7030,.T.);
#9159=ORIENTED_EDGE('',*,*,#7036,.T.);
#9160=ORIENTED_EDGE('',*,*,#7037,.T.);
#9161=ORIENTED_EDGE('',*,*,#7104,.T.);
#9162=ORIENTED_EDGE('',*,*,#7130,.T.);
#9163=ORIENTED_EDGE('',*,*,#7131,.F.);
#9164=ORIENTED_EDGE('',*,*,#7132,.F.);
#9165=ORIENTED_EDGE('',*,*,#7127,.F.);
#9166=ORIENTED_EDGE('',*,*,#7105,.T.);
#9167=ORIENTED_EDGE('',*,*,#7132,.T.);
#9168=ORIENTED_EDGE('',*,*,#7133,.F.);
#9169=ORIENTED_EDGE('',*,*,#7122,.F.);
#9170=ORIENTED_EDGE('',*,*,#7134,.F.);
#9171=ORIENTED_EDGE('',*,*,#7135,.F.);
#9172=ORIENTED_EDGE('',*,*,#7109,.F.);
#9173=ORIENTED_EDGE('',*,*,#7110,.F.);
#9174=ORIENTED_EDGE('',*,*,#7135,.T.);
#9175=ORIENTED_EDGE('',*,*,#7136,.F.);
#9176=ORIENTED_EDGE('',*,*,#7137,.F.);
#9177=ORIENTED_EDGE('',*,*,#7111,.F.);
#9178=ORIENTED_EDGE('',*,*,#7137,.T.);
#9179=ORIENTED_EDGE('',*,*,#7138,.F.);
#9180=ORIENTED_EDGE('',*,*,#7139,.F.);
#9181=ORIENTED_EDGE('',*,*,#7043,.T.);
#9182=ORIENTED_EDGE('',*,*,#7044,.T.);
#9183=ORIENTED_EDGE('',*,*,#7050,.T.);
#9184=ORIENTED_EDGE('',*,*,#7051,.T.);
#9185=ORIENTED_EDGE('',*,*,#7057,.T.);
#9186=ORIENTED_EDGE('',*,*,#7058,.T.);
#9187=ORIENTED_EDGE('',*,*,#7112,.F.);
#9188=ORIENTED_EDGE('',*,*,#7139,.T.);
#9189=ORIENTED_EDGE('',*,*,#7140,.F.);
#9190=ORIENTED_EDGE('',*,*,#7119,.F.);
#9191=ORIENTED_EDGE('',*,*,#7117,.F.);
#9192=ORIENTED_EDGE('',*,*,#7141,.F.);
#9193=ORIENTED_EDGE('',*,*,#7063,.F.);
#9194=ORIENTED_EDGE('',*,*,#7115,.F.);
#9195=ORIENTED_EDGE('',*,*,#7096,.F.);
#9196=ORIENTED_EDGE('',*,*,#7142,.F.);
#9197=ORIENTED_EDGE('',*,*,#7143,.F.);
#9198=ORIENTED_EDGE('',*,*,#7101,.T.);
#9199=ORIENTED_EDGE('',*,*,#7102,.T.);
#9200=ORIENTED_EDGE('',*,*,#7143,.T.);
#9201=ORIENTED_EDGE('',*,*,#7144,.F.);
#9202=ORIENTED_EDGE('',*,*,#7128,.F.);
#9203=ORIENTED_EDGE('',*,*,#7095,.F.);
#9204=ORIENTED_EDGE('',*,*,#7100,.T.);
#9205=ORIENTED_EDGE('',*,*,#7064,.T.);
#9206=ORIENTED_EDGE('',*,*,#7141,.T.);
#9207=ORIENTED_EDGE('',*,*,#7116,.F.);
#9208=ORIENTED_EDGE('',*,*,#7120,.T.);
#9209=ORIENTED_EDGE('',*,*,#7140,.T.);
#9210=ORIENTED_EDGE('',*,*,#7138,.T.);
#9211=ORIENTED_EDGE('',*,*,#7136,.T.);
#9212=ORIENTED_EDGE('',*,*,#7134,.T.);
#9213=ORIENTED_EDGE('',*,*,#7121,.F.);
#9214=ORIENTED_EDGE('',*,*,#7125,.T.);
#9215=ORIENTED_EDGE('',*,*,#7126,.F.);
#9216=ORIENTED_EDGE('',*,*,#7133,.T.);
#9217=ORIENTED_EDGE('',*,*,#7131,.T.);
#9218=ORIENTED_EDGE('',*,*,#7129,.T.);
#9219=ORIENTED_EDGE('',*,*,#7144,.T.);
#9220=ORIENTED_EDGE('',*,*,#7142,.T.);
#9221=ORIENTED_EDGE('',*,*,#7145,.T.);
#9222=ORIENTED_EDGE('',*,*,#7146,.T.);
#9223=ORIENTED_EDGE('',*,*,#7147,.T.);
#9224=ORIENTED_EDGE('',*,*,#7148,.T.);
#9225=ORIENTED_EDGE('',*,*,#7149,.F.);
#9226=ORIENTED_EDGE('',*,*,#7150,.F.);
#9227=ORIENTED_EDGE('',*,*,#7151,.F.);
#9228=ORIENTED_EDGE('',*,*,#7152,.F.);
#9229=ORIENTED_EDGE('',*,*,#7153,.F.);
#9230=ORIENTED_EDGE('',*,*,#7154,.F.);
#9231=ORIENTED_EDGE('',*,*,#7155,.F.);
#9232=ORIENTED_EDGE('',*,*,#7156,.F.);
#9233=ORIENTED_EDGE('',*,*,#7157,.F.);
#9234=ORIENTED_EDGE('',*,*,#7158,.F.);
#9235=ORIENTED_EDGE('',*,*,#7146,.F.);
#9236=ORIENTED_EDGE('',*,*,#7159,.F.);
#9237=ORIENTED_EDGE('',*,*,#7160,.F.);
#9238=ORIENTED_EDGE('',*,*,#7161,.F.);
#9239=ORIENTED_EDGE('',*,*,#7162,.F.);
#9240=ORIENTED_EDGE('',*,*,#7163,.F.);
#9241=ORIENTED_EDGE('',*,*,#7164,.F.);
#9242=ORIENTED_EDGE('',*,*,#7165,.F.);
#9243=ORIENTED_EDGE('',*,*,#7166,.F.);
#9244=ORIENTED_EDGE('',*,*,#7167,.F.);
#9245=ORIENTED_EDGE('',*,*,#7168,.T.);
#9246=ORIENTED_EDGE('',*,*,#7169,.T.);
#9247=ORIENTED_EDGE('',*,*,#7153,.T.);
#9248=ORIENTED_EDGE('',*,*,#7169,.F.);
#9249=ORIENTED_EDGE('',*,*,#7168,.F.);
#9250=ORIENTED_EDGE('',*,*,#7170,.T.);
#9251=ORIENTED_EDGE('',*,*,#7171,.T.);
#9252=ORIENTED_EDGE('',*,*,#7170,.F.);
#9253=ORIENTED_EDGE('',*,*,#7172,.T.);
#9254=ORIENTED_EDGE('',*,*,#7164,.T.);
#9255=ORIENTED_EDGE('',*,*,#7173,.T.);
#9256=ORIENTED_EDGE('',*,*,#7174,.T.);
#9257=ORIENTED_EDGE('',*,*,#7175,.T.);
#9258=ORIENTED_EDGE('',*,*,#7176,.T.);
#9259=ORIENTED_EDGE('',*,*,#7154,.T.);
#9260=ORIENTED_EDGE('',*,*,#7176,.F.);
#9261=ORIENTED_EDGE('',*,*,#7175,.F.);
#9262=ORIENTED_EDGE('',*,*,#7177,.T.);
#9263=ORIENTED_EDGE('',*,*,#7178,.T.);
#9264=ORIENTED_EDGE('',*,*,#7177,.F.);
#9265=ORIENTED_EDGE('',*,*,#7179,.T.);
#9266=ORIENTED_EDGE('',*,*,#7162,.T.);
#9267=ORIENTED_EDGE('',*,*,#7180,.T.);
#9268=ORIENTED_EDGE('',*,*,#7181,.T.);
#9269=ORIENTED_EDGE('',*,*,#7182,.T.);
#9270=ORIENTED_EDGE('',*,*,#7183,.T.);
#9271=ORIENTED_EDGE('',*,*,#7155,.T.);
#9272=ORIENTED_EDGE('',*,*,#7183,.F.);
#9273=ORIENTED_EDGE('',*,*,#7182,.F.);
#9274=ORIENTED_EDGE('',*,*,#7184,.T.);
#9275=ORIENTED_EDGE('',*,*,#7185,.T.);
#9276=ORIENTED_EDGE('',*,*,#7184,.F.);
#9277=ORIENTED_EDGE('',*,*,#7186,.T.);
#9278=ORIENTED_EDGE('',*,*,#7187,.T.);
#9279=ORIENTED_EDGE('',*,*,#7167,.T.);
#9280=ORIENTED_EDGE('',*,*,#7187,.F.);
#9281=ORIENTED_EDGE('',*,*,#7186,.F.);
#9282=ORIENTED_EDGE('',*,*,#7188,.T.);
#9283=ORIENTED_EDGE('',*,*,#7189,.T.);
#9284=ORIENTED_EDGE('',*,*,#7188,.F.);
#9285=ORIENTED_EDGE('',*,*,#7190,.T.);
#9286=ORIENTED_EDGE('',*,*,#7157,.T.);
#9287=ORIENTED_EDGE('',*,*,#7191,.T.);
#9288=ORIENTED_EDGE('',*,*,#7192,.T.);
#9289=ORIENTED_EDGE('',*,*,#7192,.F.);
#9290=ORIENTED_EDGE('',*,*,#7193,.F.);
#9291=ORIENTED_EDGE('',*,*,#7194,.F.);
#9292=ORIENTED_EDGE('',*,*,#7195,.T.);
#9293=ORIENTED_EDGE('',*,*,#7196,.F.);
#9294=ORIENTED_EDGE('',*,*,#7197,.F.);
#9295=ORIENTED_EDGE('',*,*,#7198,.F.);
#9296=ORIENTED_EDGE('',*,*,#7195,.F.);
#9297=ORIENTED_EDGE('',*,*,#7199,.F.);
#9298=ORIENTED_EDGE('',*,*,#7189,.F.);
#9299=ORIENTED_EDGE('',*,*,#7200,.F.);
#9300=ORIENTED_EDGE('',*,*,#7185,.F.);
#9301=ORIENTED_EDGE('',*,*,#7201,.F.);
#9302=ORIENTED_EDGE('',*,*,#7181,.F.);
#9303=ORIENTED_EDGE('',*,*,#7202,.F.);
#9304=ORIENTED_EDGE('',*,*,#7203,.F.);
#9305=ORIENTED_EDGE('',*,*,#7204,.T.);
#9306=ORIENTED_EDGE('',*,*,#7205,.F.);
#9307=ORIENTED_EDGE('',*,*,#7206,.F.);
#9308=ORIENTED_EDGE('',*,*,#7207,.F.);
#9309=ORIENTED_EDGE('',*,*,#7204,.F.);
#9310=ORIENTED_EDGE('',*,*,#7208,.F.);
#9311=ORIENTED_EDGE('',*,*,#7178,.F.);
#9312=ORIENTED_EDGE('',*,*,#7209,.F.);
#9313=ORIENTED_EDGE('',*,*,#7174,.F.);
#9314=ORIENTED_EDGE('',*,*,#7210,.F.);
#9315=ORIENTED_EDGE('',*,*,#7211,.F.);
#9316=ORIENTED_EDGE('',*,*,#7212,.T.);
#9317=ORIENTED_EDGE('',*,*,#7213,.F.);
#9318=ORIENTED_EDGE('',*,*,#7214,.F.);
#9319=ORIENTED_EDGE('',*,*,#7215,.F.);
#9320=ORIENTED_EDGE('',*,*,#7212,.F.);
#9321=ORIENTED_EDGE('',*,*,#7216,.F.);
#9322=ORIENTED_EDGE('',*,*,#7171,.F.);
#9323=ORIENTED_EDGE('',*,*,#7217,.F.);
#9324=ORIENTED_EDGE('',*,*,#7148,.F.);
#9325=ORIENTED_EDGE('',*,*,#7218,.F.);
#9326=ORIENTED_EDGE('',*,*,#7219,.F.);
#9327=ORIENTED_EDGE('',*,*,#7220,.T.);
#9328=ORIENTED_EDGE('',*,*,#7221,.F.);
#9329=ORIENTED_EDGE('',*,*,#7222,.F.);
#9330=ORIENTED_EDGE('',*,*,#7223,.F.);
#9331=ORIENTED_EDGE('',*,*,#7220,.F.);
#9332=ORIENTED_EDGE('',*,*,#7224,.F.);
#9333=ORIENTED_EDGE('',*,*,#7191,.F.);
#9334=ORIENTED_EDGE('',*,*,#7158,.T.);
#9335=ORIENTED_EDGE('',*,*,#7190,.F.);
#9336=ORIENTED_EDGE('',*,*,#7197,.T.);
#9337=ORIENTED_EDGE('',*,*,#7225,.T.);
#9338=ORIENTED_EDGE('',*,*,#7226,.T.);
#9339=ORIENTED_EDGE('',*,*,#7193,.T.);
#9340=ORIENTED_EDGE('',*,*,#7180,.F.);
#9341=ORIENTED_EDGE('',*,*,#7163,.T.);
#9342=ORIENTED_EDGE('',*,*,#7179,.F.);
#9343=ORIENTED_EDGE('',*,*,#7206,.T.);
#9344=ORIENTED_EDGE('',*,*,#7227,.T.);
#9345=ORIENTED_EDGE('',*,*,#7228,.T.);
#9346=ORIENTED_EDGE('',*,*,#7202,.T.);
#9347=ORIENTED_EDGE('',*,*,#7173,.F.);
#9348=ORIENTED_EDGE('',*,*,#7165,.T.);
#9349=ORIENTED_EDGE('',*,*,#7172,.F.);
#9350=ORIENTED_EDGE('',*,*,#7214,.T.);
#9351=ORIENTED_EDGE('',*,*,#7229,.T.);
#9352=ORIENTED_EDGE('',*,*,#7230,.T.);
#9353=ORIENTED_EDGE('',*,*,#7210,.T.);
#9354=ORIENTED_EDGE('',*,*,#7147,.F.);
#9355=ORIENTED_EDGE('',*,*,#7159,.T.);
#9356=ORIENTED_EDGE('',*,*,#7145,.F.);
#9357=ORIENTED_EDGE('',*,*,#7222,.T.);
#9358=ORIENTED_EDGE('',*,*,#7231,.T.);
#9359=ORIENTED_EDGE('',*,*,#7232,.T.);
#9360=ORIENTED_EDGE('',*,*,#7218,.T.);
#9361=ORIENTED_EDGE('',*,*,#7199,.T.);
#9362=ORIENTED_EDGE('',*,*,#7233,.T.);
#9363=ORIENTED_EDGE('',*,*,#7234,.F.);
#9364=ORIENTED_EDGE('',*,*,#7233,.F.);
#9365=ORIENTED_EDGE('',*,*,#7200,.T.);
#9366=ORIENTED_EDGE('',*,*,#7235,.T.);
#9367=ORIENTED_EDGE('',*,*,#7236,.F.);
#9368=ORIENTED_EDGE('',*,*,#7235,.F.);
#9369=ORIENTED_EDGE('',*,*,#7201,.T.);
#9370=ORIENTED_EDGE('',*,*,#7237,.T.);
#9371=ORIENTED_EDGE('',*,*,#7238,.F.);
#9372=ORIENTED_EDGE('',*,*,#7237,.F.);
#9373=ORIENTED_EDGE('',*,*,#7208,.T.);
#9374=ORIENTED_EDGE('',*,*,#7239,.T.);
#9375=ORIENTED_EDGE('',*,*,#7240,.F.);
#9376=ORIENTED_EDGE('',*,*,#7239,.F.);
#9377=ORIENTED_EDGE('',*,*,#7209,.T.);
#9378=ORIENTED_EDGE('',*,*,#7241,.T.);
#9379=ORIENTED_EDGE('',*,*,#7242,.F.);
#9380=ORIENTED_EDGE('',*,*,#7241,.F.);
#9381=ORIENTED_EDGE('',*,*,#7216,.T.);
#9382=ORIENTED_EDGE('',*,*,#7243,.T.);
#9383=ORIENTED_EDGE('',*,*,#7244,.F.);
#9384=ORIENTED_EDGE('',*,*,#7243,.F.);
#9385=ORIENTED_EDGE('',*,*,#7217,.T.);
#9386=ORIENTED_EDGE('',*,*,#7245,.T.);
#9387=ORIENTED_EDGE('',*,*,#7246,.F.);
#9388=ORIENTED_EDGE('',*,*,#7245,.F.);
#9389=ORIENTED_EDGE('',*,*,#7224,.T.);
#9390=ORIENTED_EDGE('',*,*,#7247,.T.);
#9391=ORIENTED_EDGE('',*,*,#7248,.F.);
#9392=ORIENTED_EDGE('',*,*,#7247,.F.);
#9393=ORIENTED_EDGE('',*,*,#7249,.T.);
#9394=ORIENTED_EDGE('',*,*,#7250,.T.);
#9395=ORIENTED_EDGE('',*,*,#7166,.T.);
#9396=ORIENTED_EDGE('',*,*,#7250,.F.);
#9397=ORIENTED_EDGE('',*,*,#7249,.F.);
#9398=ORIENTED_EDGE('',*,*,#7251,.T.);
#9399=ORIENTED_EDGE('',*,*,#7252,.T.);
#9400=ORIENTED_EDGE('',*,*,#7251,.F.);
#9401=ORIENTED_EDGE('',*,*,#7253,.T.);
#9402=ORIENTED_EDGE('',*,*,#7254,.T.);
#9403=ORIENTED_EDGE('',*,*,#7156,.T.);
#9404=ORIENTED_EDGE('',*,*,#7254,.F.);
#9405=ORIENTED_EDGE('',*,*,#7253,.F.);
#9406=ORIENTED_EDGE('',*,*,#7255,.T.);
#9407=ORIENTED_EDGE('',*,*,#7256,.T.);
#9408=ORIENTED_EDGE('',*,*,#7255,.F.);
#9409=ORIENTED_EDGE('',*,*,#7229,.F.);
#9410=ORIENTED_EDGE('',*,*,#7213,.T.);
#9411=ORIENTED_EDGE('',*,*,#7215,.T.);
#9412=ORIENTED_EDGE('',*,*,#7211,.T.);
#9413=ORIENTED_EDGE('',*,*,#7230,.F.);
#9414=ORIENTED_EDGE('',*,*,#7257,.T.);
#9415=ORIENTED_EDGE('',*,*,#7258,.T.);
#9416=ORIENTED_EDGE('',*,*,#7257,.F.);
#9417=ORIENTED_EDGE('',*,*,#7225,.F.);
#9418=ORIENTED_EDGE('',*,*,#7196,.T.);
#9419=ORIENTED_EDGE('',*,*,#7198,.T.);
#9420=ORIENTED_EDGE('',*,*,#7194,.T.);
#9421=ORIENTED_EDGE('',*,*,#7226,.F.);
#9422=ORIENTED_EDGE('',*,*,#7259,.T.);
#9423=ORIENTED_EDGE('',*,*,#7260,.T.);
#9424=ORIENTED_EDGE('',*,*,#7259,.F.);
#9425=ORIENTED_EDGE('',*,*,#7227,.F.);
#9426=ORIENTED_EDGE('',*,*,#7205,.T.);
#9427=ORIENTED_EDGE('',*,*,#7207,.T.);
#9428=ORIENTED_EDGE('',*,*,#7203,.T.);
#9429=ORIENTED_EDGE('',*,*,#7228,.F.);
#9430=ORIENTED_EDGE('',*,*,#7261,.T.);
#9431=ORIENTED_EDGE('',*,*,#7262,.T.);
#9432=ORIENTED_EDGE('',*,*,#7261,.F.);
#9433=ORIENTED_EDGE('',*,*,#7231,.F.);
#9434=ORIENTED_EDGE('',*,*,#7221,.T.);
#9435=ORIENTED_EDGE('',*,*,#7223,.T.);
#9436=ORIENTED_EDGE('',*,*,#7219,.T.);
#9437=ORIENTED_EDGE('',*,*,#7232,.F.);
#9438=ORIENTED_EDGE('',*,*,#7263,.T.);
#9439=ORIENTED_EDGE('',*,*,#7264,.T.);
#9440=ORIENTED_EDGE('',*,*,#7263,.F.);
#9441=ORIENTED_EDGE('',*,*,#7265,.T.);
#9442=ORIENTED_EDGE('',*,*,#7266,.T.);
#9443=ORIENTED_EDGE('',*,*,#7161,.T.);
#9444=ORIENTED_EDGE('',*,*,#7266,.F.);
#9445=ORIENTED_EDGE('',*,*,#7265,.F.);
#9446=ORIENTED_EDGE('',*,*,#7267,.T.);
#9447=ORIENTED_EDGE('',*,*,#7268,.T.);
#9448=ORIENTED_EDGE('',*,*,#7267,.F.);
#9449=ORIENTED_EDGE('',*,*,#7269,.T.);
#9450=ORIENTED_EDGE('',*,*,#7270,.T.);
#9451=ORIENTED_EDGE('',*,*,#7160,.T.);
#9452=ORIENTED_EDGE('',*,*,#7270,.F.);
#9453=ORIENTED_EDGE('',*,*,#7269,.F.);
#9454=ORIENTED_EDGE('',*,*,#7271,.T.);
#9455=ORIENTED_EDGE('',*,*,#7272,.T.);
#9456=ORIENTED_EDGE('',*,*,#7271,.F.);
#9457=ORIENTED_EDGE('',*,*,#7273,.T.);
#9458=ORIENTED_EDGE('',*,*,#7252,.F.);
#9459=ORIENTED_EDGE('',*,*,#7273,.F.);
#9460=ORIENTED_EDGE('',*,*,#7274,.T.);
#9461=ORIENTED_EDGE('',*,*,#7272,.F.);
#9462=ORIENTED_EDGE('',*,*,#7274,.F.);
#9463=ORIENTED_EDGE('',*,*,#7275,.T.);
#9464=ORIENTED_EDGE('',*,*,#7256,.F.);
#9465=ORIENTED_EDGE('',*,*,#7275,.F.);
#9466=ORIENTED_EDGE('',*,*,#7276,.T.);
#9467=ORIENTED_EDGE('',*,*,#7268,.F.);
#9468=ORIENTED_EDGE('',*,*,#7276,.F.);
#9469=ORIENTED_EDGE('',*,*,#7277,.T.);
#9470=ORIENTED_EDGE('',*,*,#7264,.F.);
#9471=ORIENTED_EDGE('',*,*,#7277,.F.);
#9472=ORIENTED_EDGE('',*,*,#7278,.T.);
#9473=ORIENTED_EDGE('',*,*,#7260,.F.);
#9474=ORIENTED_EDGE('',*,*,#7278,.F.);
#9475=ORIENTED_EDGE('',*,*,#7279,.T.);
#9476=ORIENTED_EDGE('',*,*,#7262,.F.);
#9477=ORIENTED_EDGE('',*,*,#7279,.F.);
#9478=ORIENTED_EDGE('',*,*,#7280,.T.);
#9479=ORIENTED_EDGE('',*,*,#7258,.F.);
#9480=ORIENTED_EDGE('',*,*,#7280,.F.);
#9481=ORIENTED_EDGE('',*,*,#7149,.T.);
#9482=ORIENTED_EDGE('',*,*,#7281,.T.);
#9483=ORIENTED_EDGE('',*,*,#7282,.T.);
#9484=ORIENTED_EDGE('',*,*,#7283,.F.);
#9485=ORIENTED_EDGE('',*,*,#7152,.T.);
#9486=ORIENTED_EDGE('',*,*,#7284,.T.);
#9487=ORIENTED_EDGE('',*,*,#7285,.T.);
#9488=ORIENTED_EDGE('',*,*,#7281,.F.);
#9489=ORIENTED_EDGE('',*,*,#7151,.T.);
#9490=ORIENTED_EDGE('',*,*,#7286,.T.);
#9491=ORIENTED_EDGE('',*,*,#7287,.T.);
#9492=ORIENTED_EDGE('',*,*,#7284,.F.);
#9493=ORIENTED_EDGE('',*,*,#7288,.T.);
#9494=ORIENTED_EDGE('',*,*,#7286,.F.);
#9495=ORIENTED_EDGE('',*,*,#7150,.T.);
#9496=ORIENTED_EDGE('',*,*,#7283,.T.);
#9497=ORIENTED_EDGE('',*,*,#7288,.F.);
#9498=ORIENTED_EDGE('',*,*,#7289,.F.);
#9499=ORIENTED_EDGE('',*,*,#7290,.F.);
#9500=ORIENTED_EDGE('',*,*,#7291,.T.);
#9501=ORIENTED_EDGE('',*,*,#7282,.F.);
#9502=ORIENTED_EDGE('',*,*,#7292,.F.);
#9503=ORIENTED_EDGE('',*,*,#7293,.F.);
#9504=ORIENTED_EDGE('',*,*,#7289,.T.);
#9505=ORIENTED_EDGE('',*,*,#7287,.F.);
#9506=ORIENTED_EDGE('',*,*,#7291,.F.);
#9507=ORIENTED_EDGE('',*,*,#7294,.F.);
#9508=ORIENTED_EDGE('',*,*,#7295,.T.);
#9509=ORIENTED_EDGE('',*,*,#7285,.F.);
#9510=ORIENTED_EDGE('',*,*,#7295,.F.);
#9511=ORIENTED_EDGE('',*,*,#7296,.F.);
#9512=ORIENTED_EDGE('',*,*,#7292,.T.);
#9513=ORIENTED_EDGE('',*,*,#7296,.T.);
#9514=ORIENTED_EDGE('',*,*,#7294,.T.);
#9515=ORIENTED_EDGE('',*,*,#7290,.T.);
#9516=ORIENTED_EDGE('',*,*,#7293,.T.);
#9517=ORIENTED_EDGE('',*,*,#7248,.T.);
#9518=ORIENTED_EDGE('',*,*,#7246,.T.);
#9519=ORIENTED_EDGE('',*,*,#7244,.T.);
#9520=ORIENTED_EDGE('',*,*,#7242,.T.);
#9521=ORIENTED_EDGE('',*,*,#7240,.T.);
#9522=ORIENTED_EDGE('',*,*,#7238,.T.);
#9523=ORIENTED_EDGE('',*,*,#7236,.T.);
#9524=ORIENTED_EDGE('',*,*,#7234,.T.);
#9525=ORIENTED_EDGE('',*,*,#7297,.F.);
#9526=ORIENTED_EDGE('',*,*,#7298,.F.);
#9527=ORIENTED_EDGE('',*,*,#7299,.T.);
#9528=ORIENTED_EDGE('',*,*,#7300,.T.);
#9529=ORIENTED_EDGE('',*,*,#7299,.F.);
#9530=ORIENTED_EDGE('',*,*,#7301,.T.);
#9531=ORIENTED_EDGE('',*,*,#7300,.F.);
#9532=ORIENTED_EDGE('',*,*,#7301,.F.);
#9533=ORIENTED_EDGE('',*,*,#7302,.F.);
#9534=ORIENTED_EDGE('',*,*,#7303,.F.);
#9535=ORIENTED_EDGE('',*,*,#7304,.T.);
#9536=ORIENTED_EDGE('',*,*,#7305,.T.);
#9537=ORIENTED_EDGE('',*,*,#7304,.F.);
#9538=ORIENTED_EDGE('',*,*,#7306,.T.);
#9539=ORIENTED_EDGE('',*,*,#7305,.F.);
#9540=ORIENTED_EDGE('',*,*,#7306,.F.);
#9541=ORIENTED_EDGE('',*,*,#7307,.F.);
#9542=ORIENTED_EDGE('',*,*,#7308,.F.);
#9543=ORIENTED_EDGE('',*,*,#7309,.T.);
#9544=ORIENTED_EDGE('',*,*,#7310,.T.);
#9545=ORIENTED_EDGE('',*,*,#7309,.F.);
#9546=ORIENTED_EDGE('',*,*,#7311,.T.);
#9547=ORIENTED_EDGE('',*,*,#7310,.F.);
#9548=ORIENTED_EDGE('',*,*,#7311,.F.);
#9549=ORIENTED_EDGE('',*,*,#7312,.F.);
#9550=ORIENTED_EDGE('',*,*,#7313,.F.);
#9551=ORIENTED_EDGE('',*,*,#7314,.T.);
#9552=ORIENTED_EDGE('',*,*,#7312,.T.);
#9553=ORIENTED_EDGE('',*,*,#7314,.F.);
#9554=ORIENTED_EDGE('',*,*,#7315,.F.);
#9555=ORIENTED_EDGE('',*,*,#7316,.T.);
#9556=ORIENTED_EDGE('',*,*,#7313,.T.);
#9557=ORIENTED_EDGE('',*,*,#7316,.F.);
#9558=ORIENTED_EDGE('',*,*,#7297,.T.);
#9559=ORIENTED_EDGE('',*,*,#7298,.T.);
#9560=ORIENTED_EDGE('',*,*,#7302,.T.);
#9561=ORIENTED_EDGE('',*,*,#7303,.T.);
#9562=ORIENTED_EDGE('',*,*,#7307,.T.);
#9563=ORIENTED_EDGE('',*,*,#7308,.T.);
#9564=ORIENTED_EDGE('',*,*,#7315,.T.);
#9565=ORIENTED_EDGE('',*,*,#7317,.T.);
#9566=ORIENTED_EDGE('',*,*,#7318,.F.);
#9567=ORIENTED_EDGE('',*,*,#7317,.F.);
#9568=ORIENTED_EDGE('',*,*,#7318,.T.);
#9569=ORIENTED_EDGE('',*,*,#7319,.T.);
#9570=ORIENTED_EDGE('',*,*,#7320,.T.);
#9571=ORIENTED_EDGE('',*,*,#7321,.T.);
#9572=ORIENTED_EDGE('',*,*,#7320,.F.);
#9573=ORIENTED_EDGE('',*,*,#7322,.F.);
#9574=ORIENTED_EDGE('',*,*,#7323,.F.);
#9575=ORIENTED_EDGE('',*,*,#7324,.F.);
#9576=ORIENTED_EDGE('',*,*,#7325,.F.);
#9577=ORIENTED_EDGE('',*,*,#7326,.F.);
#9578=ORIENTED_EDGE('',*,*,#7321,.F.);
#9579=ORIENTED_EDGE('',*,*,#7319,.F.);
#9580=ORIENTED_EDGE('',*,*,#7327,.T.);
#9581=ORIENTED_EDGE('',*,*,#7328,.T.);
#9582=ORIENTED_EDGE('',*,*,#7329,.F.);
#9583=ORIENTED_EDGE('',*,*,#7330,.T.);
#9584=ORIENTED_EDGE('',*,*,#7327,.F.);
#9585=ORIENTED_EDGE('',*,*,#7331,.T.);
#9586=ORIENTED_EDGE('',*,*,#7332,.T.);
#9587=ORIENTED_EDGE('',*,*,#7326,.T.);
#9588=ORIENTED_EDGE('',*,*,#7332,.F.);
#9589=ORIENTED_EDGE('',*,*,#7331,.F.);
#9590=ORIENTED_EDGE('',*,*,#7333,.T.);
#9591=ORIENTED_EDGE('',*,*,#7334,.T.);
#9592=ORIENTED_EDGE('',*,*,#7335,.F.);
#9593=ORIENTED_EDGE('',*,*,#7336,.T.);
#9594=ORIENTED_EDGE('',*,*,#7333,.F.);
#9595=ORIENTED_EDGE('',*,*,#7337,.T.);
#9596=ORIENTED_EDGE('',*,*,#7330,.F.);
#9597=ORIENTED_EDGE('',*,*,#7338,.F.);
#9598=ORIENTED_EDGE('',*,*,#7328,.F.);
#9599=ORIENTED_EDGE('',*,*,#7337,.F.);
#9600=ORIENTED_EDGE('',*,*,#7339,.F.);
#9601=ORIENTED_EDGE('',*,*,#7340,.F.);
#9602=ORIENTED_EDGE('',*,*,#7341,.F.);
#9603=ORIENTED_EDGE('',*,*,#7342,.F.);
#9604=ORIENTED_EDGE('',*,*,#7343,.T.);
#9605=ORIENTED_EDGE('',*,*,#7335,.T.);
#9606=ORIENTED_EDGE('',*,*,#7338,.T.);
#9607=ORIENTED_EDGE('',*,*,#7329,.T.);
#9608=ORIENTED_EDGE('',*,*,#7344,.T.);
#9609=ORIENTED_EDGE('',*,*,#7336,.F.);
#9610=ORIENTED_EDGE('',*,*,#7343,.F.);
#9611=ORIENTED_EDGE('',*,*,#7334,.F.);
#9612=ORIENTED_EDGE('',*,*,#7344,.F.);
#9613=ORIENTED_EDGE('',*,*,#7345,.T.);
#9614=ORIENTED_EDGE('',*,*,#7346,.T.);
#9615=ORIENTED_EDGE('',*,*,#7347,.T.);
#9616=ORIENTED_EDGE('',*,*,#7339,.T.);
#9617=ORIENTED_EDGE('',*,*,#7346,.F.);
#9618=ORIENTED_EDGE('',*,*,#7348,.T.);
#9619=ORIENTED_EDGE('',*,*,#7349,.T.);
#9620=ORIENTED_EDGE('',*,*,#7350,.F.);
#9621=ORIENTED_EDGE('',*,*,#7325,.T.);
#9622=ORIENTED_EDGE('',*,*,#7351,.F.);
#9623=ORIENTED_EDGE('',*,*,#7352,.T.);
#9624=ORIENTED_EDGE('',*,*,#7353,.F.);
#9625=ORIENTED_EDGE('',*,*,#7354,.T.);
#9626=ORIENTED_EDGE('',*,*,#7355,.T.);
#9627=ORIENTED_EDGE('',*,*,#7345,.F.);
#9628=ORIENTED_EDGE('',*,*,#7342,.T.);
#9629=ORIENTED_EDGE('',*,*,#7356,.F.);
#9630=ORIENTED_EDGE('',*,*,#7357,.F.);
#9631=ORIENTED_EDGE('',*,*,#7358,.T.);
#9632=ORIENTED_EDGE('',*,*,#7348,.F.);
#9633=ORIENTED_EDGE('',*,*,#7359,.T.);
#9634=ORIENTED_EDGE('',*,*,#7360,.T.);
#9635=ORIENTED_EDGE('',*,*,#7356,.T.);
#9636=ORIENTED_EDGE('',*,*,#7341,.T.);
#9637=ORIENTED_EDGE('',*,*,#7360,.F.);
#9638=ORIENTED_EDGE('',*,*,#7361,.T.);
#9639=ORIENTED_EDGE('',*,*,#7362,.T.);
#9640=ORIENTED_EDGE('',*,*,#7363,.F.);
#9641=ORIENTED_EDGE('',*,*,#7364,.T.);
#9642=ORIENTED_EDGE('',*,*,#7365,.F.);
#9643=ORIENTED_EDGE('',*,*,#7323,.T.);
#9644=ORIENTED_EDGE('',*,*,#7366,.F.);
#9645=ORIENTED_EDGE('',*,*,#7367,.T.);
#9646=ORIENTED_EDGE('',*,*,#7357,.T.);
#9647=ORIENTED_EDGE('',*,*,#7347,.F.);
#9648=ORIENTED_EDGE('',*,*,#7355,.F.);
#9649=ORIENTED_EDGE('',*,*,#7368,.F.);
#9650=ORIENTED_EDGE('',*,*,#7361,.F.);
#9651=ORIENTED_EDGE('',*,*,#7359,.F.);
#9652=ORIENTED_EDGE('',*,*,#7340,.T.);
#9653=ORIENTED_EDGE('',*,*,#7350,.T.);
#9654=ORIENTED_EDGE('',*,*,#7369,.T.);
#9655=ORIENTED_EDGE('',*,*,#7366,.T.);
#9656=ORIENTED_EDGE('',*,*,#7322,.T.);
#9657=ORIENTED_EDGE('',*,*,#7351,.T.);
#9658=ORIENTED_EDGE('',*,*,#7324,.T.);
#9659=ORIENTED_EDGE('',*,*,#7365,.T.);
#9660=ORIENTED_EDGE('',*,*,#7370,.T.);
#9661=ORIENTED_EDGE('',*,*,#7370,.F.);
#9662=ORIENTED_EDGE('',*,*,#7364,.F.);
#9663=ORIENTED_EDGE('',*,*,#7371,.F.);
#9664=ORIENTED_EDGE('',*,*,#7352,.F.);
#9665=ORIENTED_EDGE('',*,*,#7353,.T.);
#9666=ORIENTED_EDGE('',*,*,#7371,.T.);
#9667=ORIENTED_EDGE('',*,*,#7363,.T.);
#9668=ORIENTED_EDGE('',*,*,#7372,.T.);
#9669=ORIENTED_EDGE('',*,*,#7372,.F.);
#9670=ORIENTED_EDGE('',*,*,#7362,.F.);
#9671=ORIENTED_EDGE('',*,*,#7368,.T.);
#9672=ORIENTED_EDGE('',*,*,#7354,.F.);
#9673=ORIENTED_EDGE('',*,*,#7369,.F.);
#9674=ORIENTED_EDGE('',*,*,#7349,.F.);
#9675=ORIENTED_EDGE('',*,*,#7358,.F.);
#9676=ORIENTED_EDGE('',*,*,#7367,.F.);
#9677=ORIENTED_EDGE('',*,*,#7373,.F.);
#9678=ORIENTED_EDGE('',*,*,#7374,.F.);
#9679=ORIENTED_EDGE('',*,*,#7375,.F.);
#9680=ORIENTED_EDGE('',*,*,#7376,.F.);
#9681=ORIENTED_EDGE('',*,*,#7377,.F.);
#9682=ORIENTED_EDGE('',*,*,#7378,.F.);
#9683=ORIENTED_EDGE('',*,*,#7379,.F.);
#9684=ORIENTED_EDGE('',*,*,#7380,.F.);
#9685=ORIENTED_EDGE('',*,*,#7381,.F.);
#9686=ORIENTED_EDGE('',*,*,#7382,.F.);
#9687=ORIENTED_EDGE('',*,*,#7383,.F.);
#9688=ORIENTED_EDGE('',*,*,#7384,.F.);
#9689=ORIENTED_EDGE('',*,*,#7379,.T.);
#9690=ORIENTED_EDGE('',*,*,#7385,.F.);
#9691=ORIENTED_EDGE('',*,*,#7373,.T.);
#9692=ORIENTED_EDGE('',*,*,#7386,.T.);
#9693=ORIENTED_EDGE('',*,*,#7384,.T.);
#9694=ORIENTED_EDGE('',*,*,#7387,.F.);
#9695=ORIENTED_EDGE('',*,*,#7374,.T.);
#9696=ORIENTED_EDGE('',*,*,#7385,.T.);
#9697=ORIENTED_EDGE('',*,*,#7383,.T.);
#9698=ORIENTED_EDGE('',*,*,#7388,.F.);
#9699=ORIENTED_EDGE('',*,*,#7375,.T.);
#9700=ORIENTED_EDGE('',*,*,#7387,.T.);
#9701=ORIENTED_EDGE('',*,*,#7382,.T.);
#9702=ORIENTED_EDGE('',*,*,#7389,.F.);
#9703=ORIENTED_EDGE('',*,*,#7376,.T.);
#9704=ORIENTED_EDGE('',*,*,#7388,.T.);
#9705=ORIENTED_EDGE('',*,*,#7381,.T.);
#9706=ORIENTED_EDGE('',*,*,#7390,.F.);
#9707=ORIENTED_EDGE('',*,*,#7377,.T.);
#9708=ORIENTED_EDGE('',*,*,#7389,.T.);
#9709=ORIENTED_EDGE('',*,*,#7380,.T.);
#9710=ORIENTED_EDGE('',*,*,#7386,.F.);
#9711=ORIENTED_EDGE('',*,*,#7378,.T.);
#9712=ORIENTED_EDGE('',*,*,#7390,.T.);
#9713=ORIENTED_EDGE('',*,*,#7391,.F.);
#9714=ORIENTED_EDGE('',*,*,#7392,.T.);
#9715=ORIENTED_EDGE('',*,*,#7393,.F.);
#9716=ORIENTED_EDGE('',*,*,#7394,.T.);
#9717=ORIENTED_EDGE('',*,*,#7395,.F.);
#9718=ORIENTED_EDGE('',*,*,#7394,.F.);
#9719=ORIENTED_EDGE('',*,*,#7396,.F.);
#9720=ORIENTED_EDGE('',*,*,#7397,.F.);
#9721=ORIENTED_EDGE('',*,*,#7398,.F.);
#9722=ORIENTED_EDGE('',*,*,#7397,.T.);
#9723=ORIENTED_EDGE('',*,*,#7399,.F.);
#9724=ORIENTED_EDGE('',*,*,#7400,.T.);
#9725=ORIENTED_EDGE('',*,*,#7401,.F.);
#9726=ORIENTED_EDGE('',*,*,#7400,.F.);
#9727=ORIENTED_EDGE('',*,*,#7402,.F.);
#9728=ORIENTED_EDGE('',*,*,#7392,.F.);
#9729=ORIENTED_EDGE('',*,*,#7403,.F.);
#9730=ORIENTED_EDGE('',*,*,#7404,.T.);
#9731=ORIENTED_EDGE('',*,*,#7405,.F.);
#9732=ORIENTED_EDGE('',*,*,#7406,.T.);
#9733=ORIENTED_EDGE('',*,*,#7407,.F.);
#9734=ORIENTED_EDGE('',*,*,#7406,.F.);
#9735=ORIENTED_EDGE('',*,*,#7408,.F.);
#9736=ORIENTED_EDGE('',*,*,#7409,.F.);
#9737=ORIENTED_EDGE('',*,*,#7410,.F.);
#9738=ORIENTED_EDGE('',*,*,#7409,.T.);
#9739=ORIENTED_EDGE('',*,*,#7411,.F.);
#9740=ORIENTED_EDGE('',*,*,#7412,.T.);
#9741=ORIENTED_EDGE('',*,*,#7413,.F.);
#9742=ORIENTED_EDGE('',*,*,#7412,.F.);
#9743=ORIENTED_EDGE('',*,*,#7414,.F.);
#9744=ORIENTED_EDGE('',*,*,#7404,.F.);
#9745=ORIENTED_EDGE('',*,*,#7415,.F.);
#9746=ORIENTED_EDGE('',*,*,#7416,.T.);
#9747=ORIENTED_EDGE('',*,*,#7417,.F.);
#9748=ORIENTED_EDGE('',*,*,#7418,.T.);
#9749=ORIENTED_EDGE('',*,*,#7419,.F.);
#9750=ORIENTED_EDGE('',*,*,#7418,.F.);
#9751=ORIENTED_EDGE('',*,*,#7420,.F.);
#9752=ORIENTED_EDGE('',*,*,#7421,.F.);
#9753=ORIENTED_EDGE('',*,*,#7422,.F.);
#9754=ORIENTED_EDGE('',*,*,#7421,.T.);
#9755=ORIENTED_EDGE('',*,*,#7423,.F.);
#9756=ORIENTED_EDGE('',*,*,#7424,.T.);
#9757=ORIENTED_EDGE('',*,*,#7425,.F.);
#9758=ORIENTED_EDGE('',*,*,#7424,.F.);
#9759=ORIENTED_EDGE('',*,*,#7426,.F.);
#9760=ORIENTED_EDGE('',*,*,#7416,.F.);
#9761=ORIENTED_EDGE('',*,*,#7427,.F.);
#9762=ORIENTED_EDGE('',*,*,#7428,.T.);
#9763=ORIENTED_EDGE('',*,*,#7429,.F.);
#9764=ORIENTED_EDGE('',*,*,#7430,.T.);
#9765=ORIENTED_EDGE('',*,*,#7431,.F.);
#9766=ORIENTED_EDGE('',*,*,#7430,.F.);
#9767=ORIENTED_EDGE('',*,*,#7432,.F.);
#9768=ORIENTED_EDGE('',*,*,#7433,.F.);
#9769=ORIENTED_EDGE('',*,*,#7434,.F.);
#9770=ORIENTED_EDGE('',*,*,#7433,.T.);
#9771=ORIENTED_EDGE('',*,*,#7435,.F.);
#9772=ORIENTED_EDGE('',*,*,#7436,.T.);
#9773=ORIENTED_EDGE('',*,*,#7437,.F.);
#9774=ORIENTED_EDGE('',*,*,#7436,.F.);
#9775=ORIENTED_EDGE('',*,*,#7438,.F.);
#9776=ORIENTED_EDGE('',*,*,#7428,.F.);
#9777=ORIENTED_EDGE('',*,*,#7439,.F.);
#9778=ORIENTED_EDGE('',*,*,#7440,.T.);
#9779=ORIENTED_EDGE('',*,*,#7441,.F.);
#9780=ORIENTED_EDGE('',*,*,#7442,.T.);
#9781=ORIENTED_EDGE('',*,*,#7443,.F.);
#9782=ORIENTED_EDGE('',*,*,#7442,.F.);
#9783=ORIENTED_EDGE('',*,*,#7444,.F.);
#9784=ORIENTED_EDGE('',*,*,#7445,.F.);
#9785=ORIENTED_EDGE('',*,*,#7446,.F.);
#9786=ORIENTED_EDGE('',*,*,#7445,.T.);
#9787=ORIENTED_EDGE('',*,*,#7447,.F.);
#9788=ORIENTED_EDGE('',*,*,#7448,.T.);
#9789=ORIENTED_EDGE('',*,*,#7449,.F.);
#9790=ORIENTED_EDGE('',*,*,#7448,.F.);
#9791=ORIENTED_EDGE('',*,*,#7450,.F.);
#9792=ORIENTED_EDGE('',*,*,#7440,.F.);
#9793=ORIENTED_EDGE('',*,*,#7451,.F.);
#9794=ORIENTED_EDGE('',*,*,#7452,.F.);
#9795=ORIENTED_EDGE('',*,*,#7453,.F.);
#9796=ORIENTED_EDGE('',*,*,#7454,.F.);
#9797=ORIENTED_EDGE('',*,*,#7455,.F.);
#9798=ORIENTED_EDGE('',*,*,#7456,.F.);
#9799=ORIENTED_EDGE('',*,*,#7457,.F.);
#9800=ORIENTED_EDGE('',*,*,#7458,.F.);
#9801=ORIENTED_EDGE('',*,*,#7452,.T.);
#9802=ORIENTED_EDGE('',*,*,#7459,.F.);
#9803=ORIENTED_EDGE('',*,*,#7458,.T.);
#9804=ORIENTED_EDGE('',*,*,#7460,.T.);
#9805=ORIENTED_EDGE('',*,*,#7453,.T.);
#9806=ORIENTED_EDGE('',*,*,#7460,.F.);
#9807=ORIENTED_EDGE('',*,*,#7457,.T.);
#9808=ORIENTED_EDGE('',*,*,#7461,.T.);
#9809=ORIENTED_EDGE('',*,*,#7398,.T.);
#9810=ORIENTED_EDGE('',*,*,#7401,.T.);
#9811=ORIENTED_EDGE('',*,*,#7391,.T.);
#9812=ORIENTED_EDGE('',*,*,#7395,.T.);
#9813=ORIENTED_EDGE('',*,*,#7410,.T.);
#9814=ORIENTED_EDGE('',*,*,#7413,.T.);
#9815=ORIENTED_EDGE('',*,*,#7403,.T.);
#9816=ORIENTED_EDGE('',*,*,#7407,.T.);
#9817=ORIENTED_EDGE('',*,*,#7422,.T.);
#9818=ORIENTED_EDGE('',*,*,#7425,.T.);
#9819=ORIENTED_EDGE('',*,*,#7415,.T.);
#9820=ORIENTED_EDGE('',*,*,#7419,.T.);
#9821=ORIENTED_EDGE('',*,*,#7434,.T.);
#9822=ORIENTED_EDGE('',*,*,#7437,.T.);
#9823=ORIENTED_EDGE('',*,*,#7427,.T.);
#9824=ORIENTED_EDGE('',*,*,#7431,.T.);
#9825=ORIENTED_EDGE('',*,*,#7446,.T.);
#9826=ORIENTED_EDGE('',*,*,#7449,.T.);
#9827=ORIENTED_EDGE('',*,*,#7439,.T.);
#9828=ORIENTED_EDGE('',*,*,#7443,.T.);
#9829=ORIENTED_EDGE('',*,*,#7451,.T.);
#9830=ORIENTED_EDGE('',*,*,#7462,.F.);
#9831=ORIENTED_EDGE('',*,*,#7455,.T.);
#9832=ORIENTED_EDGE('',*,*,#7459,.T.);
#9833=ORIENTED_EDGE('',*,*,#7399,.T.);
#9834=ORIENTED_EDGE('',*,*,#7396,.T.);
#9835=ORIENTED_EDGE('',*,*,#7393,.T.);
#9836=ORIENTED_EDGE('',*,*,#7402,.T.);
#9837=ORIENTED_EDGE('',*,*,#7411,.T.);
#9838=ORIENTED_EDGE('',*,*,#7408,.T.);
#9839=ORIENTED_EDGE('',*,*,#7405,.T.);
#9840=ORIENTED_EDGE('',*,*,#7414,.T.);
#9841=ORIENTED_EDGE('',*,*,#7423,.T.);
#9842=ORIENTED_EDGE('',*,*,#7420,.T.);
#9843=ORIENTED_EDGE('',*,*,#7417,.T.);
#9844=ORIENTED_EDGE('',*,*,#7426,.T.);
#9845=ORIENTED_EDGE('',*,*,#7435,.T.);
#9846=ORIENTED_EDGE('',*,*,#7432,.T.);
#9847=ORIENTED_EDGE('',*,*,#7429,.T.);
#9848=ORIENTED_EDGE('',*,*,#7438,.T.);
#9849=ORIENTED_EDGE('',*,*,#7447,.T.);
#9850=ORIENTED_EDGE('',*,*,#7444,.T.);
#9851=ORIENTED_EDGE('',*,*,#7441,.T.);
#9852=ORIENTED_EDGE('',*,*,#7450,.T.);
#9853=ORIENTED_EDGE('',*,*,#7454,.T.);
#9854=ORIENTED_EDGE('',*,*,#7461,.F.);
#9855=ORIENTED_EDGE('',*,*,#7456,.T.);
#9856=ORIENTED_EDGE('',*,*,#7462,.T.);
#9857=ORIENTED_EDGE('',*,*,#7463,.T.);
#9858=ORIENTED_EDGE('',*,*,#7463,.F.);
#9859=ORIENTED_EDGE('',*,*,#7464,.F.);
#9860=ORIENTED_EDGE('',*,*,#7465,.F.);
#9861=ORIENTED_EDGE('',*,*,#7466,.F.);
#9862=ORIENTED_EDGE('',*,*,#7467,.T.);
#9863=ORIENTED_EDGE('',*,*,#7468,.F.);
#9864=ORIENTED_EDGE('',*,*,#7469,.F.);
#9865=ORIENTED_EDGE('',*,*,#7470,.F.);
#9866=ORIENTED_EDGE('',*,*,#7464,.T.);
#9867=ORIENTED_EDGE('',*,*,#7471,.T.);
#9868=ORIENTED_EDGE('',*,*,#7472,.T.);
#9869=ORIENTED_EDGE('',*,*,#7473,.F.);
#9870=ORIENTED_EDGE('',*,*,#7474,.F.);
#9871=ORIENTED_EDGE('',*,*,#7468,.T.);
#9872=ORIENTED_EDGE('',*,*,#7475,.T.);
#9873=ORIENTED_EDGE('',*,*,#7476,.F.);
#9874=ORIENTED_EDGE('',*,*,#7477,.F.);
#9875=ORIENTED_EDGE('',*,*,#7478,.F.);
#9876=ORIENTED_EDGE('',*,*,#7473,.T.);
#9877=ORIENTED_EDGE('',*,*,#7479,.T.);
#9878=ORIENTED_EDGE('',*,*,#7480,.T.);
#9879=ORIENTED_EDGE('',*,*,#7481,.F.);
#9880=ORIENTED_EDGE('',*,*,#7482,.F.);
#9881=ORIENTED_EDGE('',*,*,#7476,.T.);
#9882=ORIENTED_EDGE('',*,*,#7483,.T.);
#9883=ORIENTED_EDGE('',*,*,#7484,.F.);
#9884=ORIENTED_EDGE('',*,*,#7485,.F.);
#9885=ORIENTED_EDGE('',*,*,#7486,.F.);
#9886=ORIENTED_EDGE('',*,*,#7481,.T.);
#9887=ORIENTED_EDGE('',*,*,#7487,.T.);
#9888=ORIENTED_EDGE('',*,*,#7488,.T.);
#9889=ORIENTED_EDGE('',*,*,#7489,.F.);
#9890=ORIENTED_EDGE('',*,*,#7490,.F.);
#9891=ORIENTED_EDGE('',*,*,#7484,.T.);
#9892=ORIENTED_EDGE('',*,*,#7491,.T.);
#9893=ORIENTED_EDGE('',*,*,#7492,.F.);
#9894=ORIENTED_EDGE('',*,*,#7493,.F.);
#9895=ORIENTED_EDGE('',*,*,#7494,.F.);
#9896=ORIENTED_EDGE('',*,*,#7489,.T.);
#9897=ORIENTED_EDGE('',*,*,#7495,.T.);
#9898=ORIENTED_EDGE('',*,*,#7496,.T.);
#9899=ORIENTED_EDGE('',*,*,#7497,.F.);
#9900=ORIENTED_EDGE('',*,*,#7498,.F.);
#9901=ORIENTED_EDGE('',*,*,#7492,.T.);
#9902=ORIENTED_EDGE('',*,*,#7499,.T.);
#9903=ORIENTED_EDGE('',*,*,#7500,.T.);
#9904=ORIENTED_EDGE('',*,*,#7501,.F.);
#9905=ORIENTED_EDGE('',*,*,#7502,.F.);
#9906=ORIENTED_EDGE('',*,*,#7503,.F.);
#9907=ORIENTED_EDGE('',*,*,#7497,.T.);
#9908=ORIENTED_EDGE('',*,*,#7504,.T.);
#9909=ORIENTED_EDGE('',*,*,#7505,.T.);
#9910=ORIENTED_EDGE('',*,*,#7506,.F.);
#9911=ORIENTED_EDGE('',*,*,#7507,.F.);
#9912=ORIENTED_EDGE('',*,*,#7508,.F.);
#9913=ORIENTED_EDGE('',*,*,#7501,.T.);
#9914=ORIENTED_EDGE('',*,*,#7509,.T.);
#9915=ORIENTED_EDGE('',*,*,#7510,.F.);
#9916=ORIENTED_EDGE('',*,*,#7511,.F.);
#9917=ORIENTED_EDGE('',*,*,#7512,.F.);
#9918=ORIENTED_EDGE('',*,*,#7506,.T.);
#9919=ORIENTED_EDGE('',*,*,#7513,.T.);
#9920=ORIENTED_EDGE('',*,*,#7514,.T.);
#9921=ORIENTED_EDGE('',*,*,#7515,.F.);
#9922=ORIENTED_EDGE('',*,*,#7516,.F.);
#9923=ORIENTED_EDGE('',*,*,#7510,.T.);
#9924=ORIENTED_EDGE('',*,*,#7517,.T.);
#9925=ORIENTED_EDGE('',*,*,#7518,.F.);
#9926=ORIENTED_EDGE('',*,*,#7519,.F.);
#9927=ORIENTED_EDGE('',*,*,#7520,.F.);
#9928=ORIENTED_EDGE('',*,*,#7515,.T.);
#9929=ORIENTED_EDGE('',*,*,#7521,.T.);
#9930=ORIENTED_EDGE('',*,*,#7522,.T.);
#9931=ORIENTED_EDGE('',*,*,#7523,.F.);
#9932=ORIENTED_EDGE('',*,*,#7524,.F.);
#9933=ORIENTED_EDGE('',*,*,#7518,.T.);
#9934=ORIENTED_EDGE('',*,*,#7525,.T.);
#9935=ORIENTED_EDGE('',*,*,#7526,.F.);
#9936=ORIENTED_EDGE('',*,*,#7527,.F.);
#9937=ORIENTED_EDGE('',*,*,#7528,.F.);
#9938=ORIENTED_EDGE('',*,*,#7523,.T.);
#9939=ORIENTED_EDGE('',*,*,#7529,.T.);
#9940=ORIENTED_EDGE('',*,*,#7530,.T.);
#9941=ORIENTED_EDGE('',*,*,#7531,.F.);
#9942=ORIENTED_EDGE('',*,*,#7532,.F.);
#9943=ORIENTED_EDGE('',*,*,#7526,.T.);
#9944=ORIENTED_EDGE('',*,*,#7533,.T.);
#9945=ORIENTED_EDGE('',*,*,#7534,.F.);
#9946=ORIENTED_EDGE('',*,*,#7535,.F.);
#9947=ORIENTED_EDGE('',*,*,#7536,.F.);
#9948=ORIENTED_EDGE('',*,*,#7531,.T.);
#9949=ORIENTED_EDGE('',*,*,#7537,.T.);
#9950=ORIENTED_EDGE('',*,*,#7538,.T.);
#9951=ORIENTED_EDGE('',*,*,#7539,.F.);
#9952=ORIENTED_EDGE('',*,*,#7540,.F.);
#9953=ORIENTED_EDGE('',*,*,#7534,.T.);
#9954=ORIENTED_EDGE('',*,*,#7541,.T.);
#9955=ORIENTED_EDGE('',*,*,#7542,.T.);
#9956=ORIENTED_EDGE('',*,*,#7543,.F.);
#9957=ORIENTED_EDGE('',*,*,#7544,.T.);
#9958=ORIENTED_EDGE('',*,*,#7545,.T.);
#9959=ORIENTED_EDGE('',*,*,#7546,.T.);
#9960=ORIENTED_EDGE('',*,*,#7547,.T.);
#9961=ORIENTED_EDGE('',*,*,#7548,.T.);
#9962=ORIENTED_EDGE('',*,*,#7549,.T.);
#9963=ORIENTED_EDGE('',*,*,#7550,.T.);
#9964=ORIENTED_EDGE('',*,*,#7551,.T.);
#9965=ORIENTED_EDGE('',*,*,#7552,.T.);
#9966=ORIENTED_EDGE('',*,*,#7553,.T.);
#9967=ORIENTED_EDGE('',*,*,#7554,.T.);
#9968=ORIENTED_EDGE('',*,*,#7555,.T.);
#9969=ORIENTED_EDGE('',*,*,#7556,.T.);
#9970=ORIENTED_EDGE('',*,*,#7557,.T.);
#9971=ORIENTED_EDGE('',*,*,#7558,.T.);
#9972=ORIENTED_EDGE('',*,*,#7559,.T.);
#9973=ORIENTED_EDGE('',*,*,#7560,.T.);
#9974=ORIENTED_EDGE('',*,*,#7561,.T.);
#9975=ORIENTED_EDGE('',*,*,#7562,.T.);
#9976=ORIENTED_EDGE('',*,*,#7563,.T.);
#9977=ORIENTED_EDGE('',*,*,#7564,.T.);
#9978=ORIENTED_EDGE('',*,*,#7565,.F.);
#9979=ORIENTED_EDGE('',*,*,#7566,.F.);
#9980=ORIENTED_EDGE('',*,*,#7567,.T.);
#9981=ORIENTED_EDGE('',*,*,#7568,.T.);
#9982=ORIENTED_EDGE('',*,*,#7569,.T.);
#9983=ORIENTED_EDGE('',*,*,#7570,.T.);
#9984=ORIENTED_EDGE('',*,*,#7571,.T.);
#9985=ORIENTED_EDGE('',*,*,#7572,.T.);
#9986=ORIENTED_EDGE('',*,*,#7573,.T.);
#9987=ORIENTED_EDGE('',*,*,#7574,.T.);
#9988=ORIENTED_EDGE('',*,*,#7575,.T.);
#9989=ORIENTED_EDGE('',*,*,#7576,.T.);
#9990=ORIENTED_EDGE('',*,*,#7577,.T.);
#9991=ORIENTED_EDGE('',*,*,#7578,.T.);
#9992=ORIENTED_EDGE('',*,*,#7579,.T.);
#9993=ORIENTED_EDGE('',*,*,#7580,.T.);
#9994=ORIENTED_EDGE('',*,*,#7581,.T.);
#9995=ORIENTED_EDGE('',*,*,#7582,.T.);
#9996=ORIENTED_EDGE('',*,*,#7583,.T.);
#9997=ORIENTED_EDGE('',*,*,#7584,.T.);
#9998=ORIENTED_EDGE('',*,*,#7585,.T.);
#9999=ORIENTED_EDGE('',*,*,#7539,.T.);
#10000=ORIENTED_EDGE('',*,*,#7586,.T.);
#10001=ORIENTED_EDGE('',*,*,#7587,.T.);
#10002=ORIENTED_EDGE('',*,*,#7588,.F.);
#10003=ORIENTED_EDGE('',*,*,#7589,.F.);
#10004=ORIENTED_EDGE('',*,*,#7590,.F.);
#10005=ORIENTED_EDGE('',*,*,#7591,.F.);
#10006=ORIENTED_EDGE('',*,*,#7592,.T.);
#10007=ORIENTED_EDGE('',*,*,#7588,.T.);
#10008=ORIENTED_EDGE('',*,*,#7593,.T.);
#10009=ORIENTED_EDGE('',*,*,#7592,.F.);
#10010=ORIENTED_EDGE('',*,*,#7594,.F.);
#10011=ORIENTED_EDGE('',*,*,#7564,.F.);
#10012=ORIENTED_EDGE('',*,*,#7563,.F.);
#10013=ORIENTED_EDGE('',*,*,#7562,.F.);
#10014=ORIENTED_EDGE('',*,*,#7561,.F.);
#10015=ORIENTED_EDGE('',*,*,#7560,.F.);
#10016=ORIENTED_EDGE('',*,*,#7559,.F.);
#10017=ORIENTED_EDGE('',*,*,#7558,.F.);
#10018=ORIENTED_EDGE('',*,*,#7557,.F.);
#10019=ORIENTED_EDGE('',*,*,#7556,.F.);
#10020=ORIENTED_EDGE('',*,*,#7555,.F.);
#10021=ORIENTED_EDGE('',*,*,#7554,.F.);
#10022=ORIENTED_EDGE('',*,*,#7553,.F.);
#10023=ORIENTED_EDGE('',*,*,#7552,.F.);
#10024=ORIENTED_EDGE('',*,*,#7551,.F.);
#10025=ORIENTED_EDGE('',*,*,#7550,.F.);
#10026=ORIENTED_EDGE('',*,*,#7549,.F.);
#10027=ORIENTED_EDGE('',*,*,#7548,.F.);
#10028=ORIENTED_EDGE('',*,*,#7547,.F.);
#10029=ORIENTED_EDGE('',*,*,#7546,.F.);
#10030=ORIENTED_EDGE('',*,*,#7545,.F.);
#10031=ORIENTED_EDGE('',*,*,#7544,.F.);
#10032=ORIENTED_EDGE('',*,*,#7595,.F.);
#10033=ORIENTED_EDGE('',*,*,#7465,.T.);
#10034=ORIENTED_EDGE('',*,*,#7470,.T.);
#10035=ORIENTED_EDGE('',*,*,#7469,.T.);
#10036=ORIENTED_EDGE('',*,*,#7474,.T.);
#10037=ORIENTED_EDGE('',*,*,#7478,.T.);
#10038=ORIENTED_EDGE('',*,*,#7477,.T.);
#10039=ORIENTED_EDGE('',*,*,#7482,.T.);
#10040=ORIENTED_EDGE('',*,*,#7486,.T.);
#10041=ORIENTED_EDGE('',*,*,#7485,.T.);
#10042=ORIENTED_EDGE('',*,*,#7490,.T.);
#10043=ORIENTED_EDGE('',*,*,#7494,.T.);
#10044=ORIENTED_EDGE('',*,*,#7493,.T.);
#10045=ORIENTED_EDGE('',*,*,#7498,.T.);
#10046=ORIENTED_EDGE('',*,*,#7503,.T.);
#10047=ORIENTED_EDGE('',*,*,#7502,.T.);
#10048=ORIENTED_EDGE('',*,*,#7508,.T.);
#10049=ORIENTED_EDGE('',*,*,#7507,.T.);
#10050=ORIENTED_EDGE('',*,*,#7512,.T.);
#10051=ORIENTED_EDGE('',*,*,#7511,.T.);
#10052=ORIENTED_EDGE('',*,*,#7516,.T.);
#10053=ORIENTED_EDGE('',*,*,#7520,.T.);
#10054=ORIENTED_EDGE('',*,*,#7519,.T.);
#10055=ORIENTED_EDGE('',*,*,#7524,.T.);
#10056=ORIENTED_EDGE('',*,*,#7528,.T.);
#10057=ORIENTED_EDGE('',*,*,#7527,.T.);
#10058=ORIENTED_EDGE('',*,*,#7532,.T.);
#10059=ORIENTED_EDGE('',*,*,#7536,.T.);
#10060=ORIENTED_EDGE('',*,*,#7535,.T.);
#10061=ORIENTED_EDGE('',*,*,#7540,.T.);
#10062=ORIENTED_EDGE('',*,*,#7590,.T.);
#10063=ORIENTED_EDGE('',*,*,#7589,.T.);
#10064=ORIENTED_EDGE('',*,*,#7596,.F.);
#10065=ORIENTED_EDGE('',*,*,#7597,.T.);
#10066=ORIENTED_EDGE('',*,*,#7466,.T.);
#10067=ORIENTED_EDGE('',*,*,#7595,.T.);
#10068=ORIENTED_EDGE('',*,*,#7598,.F.);
#10069=ORIENTED_EDGE('',*,*,#7593,.F.);
#10070=ORIENTED_EDGE('',*,*,#7587,.F.);
#10071=ORIENTED_EDGE('',*,*,#7586,.F.);
#10072=ORIENTED_EDGE('',*,*,#7541,.F.);
#10073=ORIENTED_EDGE('',*,*,#7538,.F.);
#10074=ORIENTED_EDGE('',*,*,#7537,.F.);
#10075=ORIENTED_EDGE('',*,*,#7533,.F.);
#10076=ORIENTED_EDGE('',*,*,#7530,.F.);
#10077=ORIENTED_EDGE('',*,*,#7529,.F.);
#10078=ORIENTED_EDGE('',*,*,#7525,.F.);
#10079=ORIENTED_EDGE('',*,*,#7522,.F.);
#10080=ORIENTED_EDGE('',*,*,#7521,.F.);
#10081=ORIENTED_EDGE('',*,*,#7517,.F.);
#10082=ORIENTED_EDGE('',*,*,#7514,.F.);
#10083=ORIENTED_EDGE('',*,*,#7513,.F.);
#10084=ORIENTED_EDGE('',*,*,#7509,.F.);
#10085=ORIENTED_EDGE('',*,*,#7505,.F.);
#10086=ORIENTED_EDGE('',*,*,#7504,.F.);
#10087=ORIENTED_EDGE('',*,*,#7500,.F.);
#10088=ORIENTED_EDGE('',*,*,#7499,.F.);
#10089=ORIENTED_EDGE('',*,*,#7496,.F.);
#10090=ORIENTED_EDGE('',*,*,#7495,.F.);
#10091=ORIENTED_EDGE('',*,*,#7491,.F.);
#10092=ORIENTED_EDGE('',*,*,#7488,.F.);
#10093=ORIENTED_EDGE('',*,*,#7487,.F.);
#10094=ORIENTED_EDGE('',*,*,#7483,.F.);
#10095=ORIENTED_EDGE('',*,*,#7480,.F.);
#10096=ORIENTED_EDGE('',*,*,#7479,.F.);
#10097=ORIENTED_EDGE('',*,*,#7475,.F.);
#10098=ORIENTED_EDGE('',*,*,#7472,.F.);
#10099=ORIENTED_EDGE('',*,*,#7471,.F.);
#10100=ORIENTED_EDGE('',*,*,#7467,.F.);
#10101=ORIENTED_EDGE('',*,*,#7597,.F.);
#10102=ORIENTED_EDGE('',*,*,#7599,.F.);
#10103=ORIENTED_EDGE('',*,*,#7542,.F.);
#10104=ORIENTED_EDGE('',*,*,#7585,.F.);
#10105=ORIENTED_EDGE('',*,*,#7584,.F.);
#10106=ORIENTED_EDGE('',*,*,#7583,.F.);
#10107=ORIENTED_EDGE('',*,*,#7582,.F.);
#10108=ORIENTED_EDGE('',*,*,#7581,.F.);
#10109=ORIENTED_EDGE('',*,*,#7580,.F.);
#10110=ORIENTED_EDGE('',*,*,#7579,.F.);
#10111=ORIENTED_EDGE('',*,*,#7578,.F.);
#10112=ORIENTED_EDGE('',*,*,#7577,.F.);
#10113=ORIENTED_EDGE('',*,*,#7576,.F.);
#10114=ORIENTED_EDGE('',*,*,#7575,.F.);
#10115=ORIENTED_EDGE('',*,*,#7574,.F.);
#10116=ORIENTED_EDGE('',*,*,#7573,.F.);
#10117=ORIENTED_EDGE('',*,*,#7572,.F.);
#10118=ORIENTED_EDGE('',*,*,#7571,.F.);
#10119=ORIENTED_EDGE('',*,*,#7570,.F.);
#10120=ORIENTED_EDGE('',*,*,#7569,.F.);
#10121=ORIENTED_EDGE('',*,*,#7568,.F.);
#10122=ORIENTED_EDGE('',*,*,#7567,.F.);
#10123=ORIENTED_EDGE('',*,*,#7600,.T.);
#10124=ORIENTED_EDGE('',*,*,#7601,.T.);
#10125=ORIENTED_EDGE('',*,*,#7598,.T.);
#10126=ORIENTED_EDGE('',*,*,#7543,.T.);
#10127=ORIENTED_EDGE('',*,*,#7599,.T.);
#10128=ORIENTED_EDGE('',*,*,#7596,.T.);
#10129=ORIENTED_EDGE('',*,*,#7601,.F.);
#10130=ORIENTED_EDGE('',*,*,#7602,.F.);
#10131=ORIENTED_EDGE('',*,*,#7600,.F.);
#10132=ORIENTED_EDGE('',*,*,#7566,.T.);
#10133=ORIENTED_EDGE('',*,*,#7603,.T.);
#10134=ORIENTED_EDGE('',*,*,#7604,.T.);
#10135=ORIENTED_EDGE('',*,*,#7603,.F.);
#10136=ORIENTED_EDGE('',*,*,#7565,.T.);
#10137=ORIENTED_EDGE('',*,*,#7594,.T.);
#10138=ORIENTED_EDGE('',*,*,#7591,.T.);
#10139=ORIENTED_EDGE('',*,*,#7604,.F.);
#10140=ORIENTED_EDGE('',*,*,#7605,.F.);
#10141=ORIENTED_EDGE('',*,*,#7606,.T.);
#10142=ORIENTED_EDGE('',*,*,#7607,.F.);
#10143=ORIENTED_EDGE('',*,*,#7608,.F.);
#10144=ORIENTED_EDGE('',*,*,#7609,.F.);
#10145=ORIENTED_EDGE('',*,*,#7610,.F.);
#10146=ORIENTED_EDGE('',*,*,#7607,.T.);
#10147=ORIENTED_EDGE('',*,*,#7611,.T.);
#10148=ORIENTED_EDGE('',*,*,#7612,.F.);
#10149=ORIENTED_EDGE('',*,*,#7611,.F.);
#10150=ORIENTED_EDGE('',*,*,#7606,.F.);
#10151=ORIENTED_EDGE('',*,*,#7613,.T.);
#10152=ORIENTED_EDGE('',*,*,#7614,.T.);
#10153=ORIENTED_EDGE('',*,*,#7615,.T.);
#10154=ORIENTED_EDGE('',*,*,#7616,.T.);
#10155=ORIENTED_EDGE('',*,*,#7617,.T.);
#10156=ORIENTED_EDGE('',*,*,#7618,.T.);
#10157=ORIENTED_EDGE('',*,*,#7619,.T.);
#10158=ORIENTED_EDGE('',*,*,#7620,.T.);
#10159=ORIENTED_EDGE('',*,*,#7621,.T.);
#10160=ORIENTED_EDGE('',*,*,#7622,.T.);
#10161=ORIENTED_EDGE('',*,*,#7623,.T.);
#10162=ORIENTED_EDGE('',*,*,#7624,.T.);
#10163=ORIENTED_EDGE('',*,*,#7625,.T.);
#10164=ORIENTED_EDGE('',*,*,#7626,.T.);
#10165=ORIENTED_EDGE('',*,*,#7627,.T.);
#10166=ORIENTED_EDGE('',*,*,#7628,.T.);
#10167=ORIENTED_EDGE('',*,*,#7629,.T.);
#10168=ORIENTED_EDGE('',*,*,#7630,.T.);
#10169=ORIENTED_EDGE('',*,*,#7631,.T.);
#10170=ORIENTED_EDGE('',*,*,#7632,.T.);
#10171=ORIENTED_EDGE('',*,*,#7633,.T.);
#10172=ORIENTED_EDGE('',*,*,#7634,.T.);
#10173=ORIENTED_EDGE('',*,*,#7635,.T.);
#10174=ORIENTED_EDGE('',*,*,#7636,.T.);
#10175=ORIENTED_EDGE('',*,*,#7637,.T.);
#10176=ORIENTED_EDGE('',*,*,#7638,.T.);
#10177=ORIENTED_EDGE('',*,*,#7639,.T.);
#10178=ORIENTED_EDGE('',*,*,#7640,.T.);
#10179=ORIENTED_EDGE('',*,*,#7641,.T.);
#10180=ORIENTED_EDGE('',*,*,#7642,.T.);
#10181=ORIENTED_EDGE('',*,*,#7643,.T.);
#10182=ORIENTED_EDGE('',*,*,#7644,.T.);
#10183=ORIENTED_EDGE('',*,*,#7645,.T.);
#10184=ORIENTED_EDGE('',*,*,#7646,.T.);
#10185=ORIENTED_EDGE('',*,*,#7647,.T.);
#10186=ORIENTED_EDGE('',*,*,#7648,.T.);
#10187=ORIENTED_EDGE('',*,*,#7649,.T.);
#10188=ORIENTED_EDGE('',*,*,#7650,.T.);
#10189=ORIENTED_EDGE('',*,*,#7651,.T.);
#10190=ORIENTED_EDGE('',*,*,#7652,.T.);
#10191=ORIENTED_EDGE('',*,*,#7653,.T.);
#10192=ORIENTED_EDGE('',*,*,#7654,.T.);
#10193=ORIENTED_EDGE('',*,*,#7655,.T.);
#10194=ORIENTED_EDGE('',*,*,#7656,.T.);
#10195=ORIENTED_EDGE('',*,*,#7657,.T.);
#10196=ORIENTED_EDGE('',*,*,#7658,.T.);
#10197=ORIENTED_EDGE('',*,*,#7659,.T.);
#10198=ORIENTED_EDGE('',*,*,#7660,.T.);
#10199=ORIENTED_EDGE('',*,*,#7661,.T.);
#10200=ORIENTED_EDGE('',*,*,#7662,.T.);
#10201=ORIENTED_EDGE('',*,*,#7663,.T.);
#10202=ORIENTED_EDGE('',*,*,#7664,.T.);
#10203=ORIENTED_EDGE('',*,*,#7665,.T.);
#10204=ORIENTED_EDGE('',*,*,#7666,.T.);
#10205=ORIENTED_EDGE('',*,*,#7667,.T.);
#10206=ORIENTED_EDGE('',*,*,#7668,.T.);
#10207=ORIENTED_EDGE('',*,*,#7608,.T.);
#10208=ORIENTED_EDGE('',*,*,#7610,.T.);
#10209=ORIENTED_EDGE('',*,*,#7669,.T.);
#10210=ORIENTED_EDGE('',*,*,#7670,.T.);
#10211=ORIENTED_EDGE('',*,*,#7671,.T.);
#10212=ORIENTED_EDGE('',*,*,#7672,.T.);
#10213=ORIENTED_EDGE('',*,*,#7673,.T.);
#10214=ORIENTED_EDGE('',*,*,#7674,.T.);
#10215=ORIENTED_EDGE('',*,*,#7675,.T.);
#10216=ORIENTED_EDGE('',*,*,#7676,.T.);
#10217=ORIENTED_EDGE('',*,*,#7677,.T.);
#10218=ORIENTED_EDGE('',*,*,#7678,.T.);
#10219=ORIENTED_EDGE('',*,*,#7679,.T.);
#10220=ORIENTED_EDGE('',*,*,#7680,.T.);
#10221=ORIENTED_EDGE('',*,*,#7681,.T.);
#10222=ORIENTED_EDGE('',*,*,#7682,.T.);
#10223=ORIENTED_EDGE('',*,*,#7683,.T.);
#10224=ORIENTED_EDGE('',*,*,#7684,.T.);
#10225=ORIENTED_EDGE('',*,*,#7685,.T.);
#10226=ORIENTED_EDGE('',*,*,#7686,.T.);
#10227=ORIENTED_EDGE('',*,*,#7687,.T.);
#10228=ORIENTED_EDGE('',*,*,#7688,.T.);
#10229=ORIENTED_EDGE('',*,*,#7689,.T.);
#10230=ORIENTED_EDGE('',*,*,#7690,.T.);
#10231=ORIENTED_EDGE('',*,*,#7691,.T.);
#10232=ORIENTED_EDGE('',*,*,#7692,.T.);
#10233=ORIENTED_EDGE('',*,*,#7693,.T.);
#10234=ORIENTED_EDGE('',*,*,#7694,.T.);
#10235=ORIENTED_EDGE('',*,*,#7695,.T.);
#10236=ORIENTED_EDGE('',*,*,#7696,.T.);
#10237=ORIENTED_EDGE('',*,*,#7697,.T.);
#10238=ORIENTED_EDGE('',*,*,#7698,.T.);
#10239=ORIENTED_EDGE('',*,*,#7699,.T.);
#10240=ORIENTED_EDGE('',*,*,#7700,.T.);
#10241=ORIENTED_EDGE('',*,*,#7701,.T.);
#10242=ORIENTED_EDGE('',*,*,#7702,.T.);
#10243=ORIENTED_EDGE('',*,*,#7703,.T.);
#10244=ORIENTED_EDGE('',*,*,#7704,.T.);
#10245=ORIENTED_EDGE('',*,*,#7705,.T.);
#10246=ORIENTED_EDGE('',*,*,#7706,.T.);
#10247=ORIENTED_EDGE('',*,*,#7707,.T.);
#10248=ORIENTED_EDGE('',*,*,#7708,.T.);
#10249=ORIENTED_EDGE('',*,*,#7709,.T.);
#10250=ORIENTED_EDGE('',*,*,#7710,.T.);
#10251=ORIENTED_EDGE('',*,*,#7711,.T.);
#10252=ORIENTED_EDGE('',*,*,#7712,.T.);
#10253=ORIENTED_EDGE('',*,*,#7713,.T.);
#10254=ORIENTED_EDGE('',*,*,#7714,.T.);
#10255=ORIENTED_EDGE('',*,*,#7715,.T.);
#10256=ORIENTED_EDGE('',*,*,#7716,.T.);
#10257=ORIENTED_EDGE('',*,*,#7717,.T.);
#10258=ORIENTED_EDGE('',*,*,#7718,.T.);
#10259=ORIENTED_EDGE('',*,*,#7719,.T.);
#10260=ORIENTED_EDGE('',*,*,#7720,.T.);
#10261=ORIENTED_EDGE('',*,*,#7719,.F.);
#10262=ORIENTED_EDGE('',*,*,#7721,.F.);
#10263=ORIENTED_EDGE('',*,*,#7722,.T.);
#10264=ORIENTED_EDGE('',*,*,#7723,.F.);
#10265=ORIENTED_EDGE('',*,*,#7670,.F.);
#10266=ORIENTED_EDGE('',*,*,#7724,.F.);
#10267=ORIENTED_EDGE('',*,*,#7671,.F.);
#10268=ORIENTED_EDGE('',*,*,#7723,.T.);
#10269=ORIENTED_EDGE('',*,*,#7725,.T.);
#10270=ORIENTED_EDGE('',*,*,#7726,.F.);
#10271=ORIENTED_EDGE('',*,*,#7725,.F.);
#10272=ORIENTED_EDGE('',*,*,#7722,.F.);
#10273=ORIENTED_EDGE('',*,*,#7727,.F.);
#10274=ORIENTED_EDGE('',*,*,#7728,.T.);
#10275=ORIENTED_EDGE('',*,*,#7729,.F.);
#10276=ORIENTED_EDGE('',*,*,#7673,.F.);
#10277=ORIENTED_EDGE('',*,*,#7730,.F.);
#10278=ORIENTED_EDGE('',*,*,#7674,.F.);
#10279=ORIENTED_EDGE('',*,*,#7729,.T.);
#10280=ORIENTED_EDGE('',*,*,#7731,.T.);
#10281=ORIENTED_EDGE('',*,*,#7732,.F.);
#10282=ORIENTED_EDGE('',*,*,#7731,.F.);
#10283=ORIENTED_EDGE('',*,*,#7728,.F.);
#10284=ORIENTED_EDGE('',*,*,#7733,.F.);
#10285=ORIENTED_EDGE('',*,*,#7734,.T.);
#10286=ORIENTED_EDGE('',*,*,#7735,.F.);
#10287=ORIENTED_EDGE('',*,*,#7676,.F.);
#10288=ORIENTED_EDGE('',*,*,#7736,.F.);
#10289=ORIENTED_EDGE('',*,*,#7677,.F.);
#10290=ORIENTED_EDGE('',*,*,#7735,.T.);
#10291=ORIENTED_EDGE('',*,*,#7737,.T.);
#10292=ORIENTED_EDGE('',*,*,#7738,.F.);
#10293=ORIENTED_EDGE('',*,*,#7737,.F.);
#10294=ORIENTED_EDGE('',*,*,#7734,.F.);
#10295=ORIENTED_EDGE('',*,*,#7739,.F.);
#10296=ORIENTED_EDGE('',*,*,#7740,.T.);
#10297=ORIENTED_EDGE('',*,*,#7741,.F.);
#10298=ORIENTED_EDGE('',*,*,#7679,.F.);
#10299=ORIENTED_EDGE('',*,*,#7742,.F.);
#10300=ORIENTED_EDGE('',*,*,#7680,.F.);
#10301=ORIENTED_EDGE('',*,*,#7741,.T.);
#10302=ORIENTED_EDGE('',*,*,#7743,.T.);
#10303=ORIENTED_EDGE('',*,*,#7744,.F.);
#10304=ORIENTED_EDGE('',*,*,#7743,.F.);
#10305=ORIENTED_EDGE('',*,*,#7740,.F.);
#10306=ORIENTED_EDGE('',*,*,#7745,.F.);
#10307=ORIENTED_EDGE('',*,*,#7746,.T.);
#10308=ORIENTED_EDGE('',*,*,#7747,.F.);
#10309=ORIENTED_EDGE('',*,*,#7682,.F.);
#10310=ORIENTED_EDGE('',*,*,#7748,.F.);
#10311=ORIENTED_EDGE('',*,*,#7683,.F.);
#10312=ORIENTED_EDGE('',*,*,#7747,.T.);
#10313=ORIENTED_EDGE('',*,*,#7749,.T.);
#10314=ORIENTED_EDGE('',*,*,#7750,.F.);
#10315=ORIENTED_EDGE('',*,*,#7749,.F.);
#10316=ORIENTED_EDGE('',*,*,#7746,.F.);
#10317=ORIENTED_EDGE('',*,*,#7751,.F.);
#10318=ORIENTED_EDGE('',*,*,#7752,.T.);
#10319=ORIENTED_EDGE('',*,*,#7753,.F.);
#10320=ORIENTED_EDGE('',*,*,#7685,.F.);
#10321=ORIENTED_EDGE('',*,*,#7754,.F.);
#10322=ORIENTED_EDGE('',*,*,#7686,.F.);
#10323=ORIENTED_EDGE('',*,*,#7753,.T.);
#10324=ORIENTED_EDGE('',*,*,#7755,.T.);
#10325=ORIENTED_EDGE('',*,*,#7756,.F.);
#10326=ORIENTED_EDGE('',*,*,#7755,.F.);
#10327=ORIENTED_EDGE('',*,*,#7752,.F.);
#10328=ORIENTED_EDGE('',*,*,#7757,.F.);
#10329=ORIENTED_EDGE('',*,*,#7758,.T.);
#10330=ORIENTED_EDGE('',*,*,#7759,.F.);
#10331=ORIENTED_EDGE('',*,*,#7688,.F.);
#10332=ORIENTED_EDGE('',*,*,#7760,.F.);
#10333=ORIENTED_EDGE('',*,*,#7689,.F.);
#10334=ORIENTED_EDGE('',*,*,#7759,.T.);
#10335=ORIENTED_EDGE('',*,*,#7761,.T.);
#10336=ORIENTED_EDGE('',*,*,#7762,.F.);
#10337=ORIENTED_EDGE('',*,*,#7761,.F.);
#10338=ORIENTED_EDGE('',*,*,#7758,.F.);
#10339=ORIENTED_EDGE('',*,*,#7763,.F.);
#10340=ORIENTED_EDGE('',*,*,#7764,.T.);
#10341=ORIENTED_EDGE('',*,*,#7765,.F.);
#10342=ORIENTED_EDGE('',*,*,#7691,.F.);
#10343=ORIENTED_EDGE('',*,*,#7766,.F.);
#10344=ORIENTED_EDGE('',*,*,#7692,.F.);
#10345=ORIENTED_EDGE('',*,*,#7765,.T.);
#10346=ORIENTED_EDGE('',*,*,#7767,.T.);
#10347=ORIENTED_EDGE('',*,*,#7768,.F.);
#10348=ORIENTED_EDGE('',*,*,#7767,.F.);
#10349=ORIENTED_EDGE('',*,*,#7764,.F.);
#10350=ORIENTED_EDGE('',*,*,#7769,.F.);
#10351=ORIENTED_EDGE('',*,*,#7770,.T.);
#10352=ORIENTED_EDGE('',*,*,#7771,.F.);
#10353=ORIENTED_EDGE('',*,*,#7694,.F.);
#10354=ORIENTED_EDGE('',*,*,#7772,.F.);
#10355=ORIENTED_EDGE('',*,*,#7695,.F.);
#10356=ORIENTED_EDGE('',*,*,#7771,.T.);
#10357=ORIENTED_EDGE('',*,*,#7773,.T.);
#10358=ORIENTED_EDGE('',*,*,#7774,.F.);
#10359=ORIENTED_EDGE('',*,*,#7773,.F.);
#10360=ORIENTED_EDGE('',*,*,#7770,.F.);
#10361=ORIENTED_EDGE('',*,*,#7775,.F.);
#10362=ORIENTED_EDGE('',*,*,#7776,.T.);
#10363=ORIENTED_EDGE('',*,*,#7777,.F.);
#10364=ORIENTED_EDGE('',*,*,#7697,.F.);
#10365=ORIENTED_EDGE('',*,*,#7778,.F.);
#10366=ORIENTED_EDGE('',*,*,#7698,.F.);
#10367=ORIENTED_EDGE('',*,*,#7777,.T.);
#10368=ORIENTED_EDGE('',*,*,#7779,.T.);
#10369=ORIENTED_EDGE('',*,*,#7780,.F.);
#10370=ORIENTED_EDGE('',*,*,#7779,.F.);
#10371=ORIENTED_EDGE('',*,*,#7776,.F.);
#10372=ORIENTED_EDGE('',*,*,#7781,.F.);
#10373=ORIENTED_EDGE('',*,*,#7782,.T.);
#10374=ORIENTED_EDGE('',*,*,#7783,.F.);
#10375=ORIENTED_EDGE('',*,*,#7700,.F.);
#10376=ORIENTED_EDGE('',*,*,#7784,.F.);
#10377=ORIENTED_EDGE('',*,*,#7701,.F.);
#10378=ORIENTED_EDGE('',*,*,#7783,.T.);
#10379=ORIENTED_EDGE('',*,*,#7785,.T.);
#10380=ORIENTED_EDGE('',*,*,#7786,.F.);
#10381=ORIENTED_EDGE('',*,*,#7785,.F.);
#10382=ORIENTED_EDGE('',*,*,#7782,.F.);
#10383=ORIENTED_EDGE('',*,*,#7787,.F.);
#10384=ORIENTED_EDGE('',*,*,#7788,.T.);
#10385=ORIENTED_EDGE('',*,*,#7789,.F.);
#10386=ORIENTED_EDGE('',*,*,#7703,.F.);
#10387=ORIENTED_EDGE('',*,*,#7790,.F.);
#10388=ORIENTED_EDGE('',*,*,#7704,.F.);
#10389=ORIENTED_EDGE('',*,*,#7789,.T.);
#10390=ORIENTED_EDGE('',*,*,#7791,.T.);
#10391=ORIENTED_EDGE('',*,*,#7792,.F.);
#10392=ORIENTED_EDGE('',*,*,#7791,.F.);
#10393=ORIENTED_EDGE('',*,*,#7788,.F.);
#10394=ORIENTED_EDGE('',*,*,#7793,.F.);
#10395=ORIENTED_EDGE('',*,*,#7794,.T.);
#10396=ORIENTED_EDGE('',*,*,#7795,.F.);
#10397=ORIENTED_EDGE('',*,*,#7706,.F.);
#10398=ORIENTED_EDGE('',*,*,#7796,.F.);
#10399=ORIENTED_EDGE('',*,*,#7707,.F.);
#10400=ORIENTED_EDGE('',*,*,#7795,.T.);
#10401=ORIENTED_EDGE('',*,*,#7797,.T.);
#10402=ORIENTED_EDGE('',*,*,#7798,.F.);
#10403=ORIENTED_EDGE('',*,*,#7797,.F.);
#10404=ORIENTED_EDGE('',*,*,#7794,.F.);
#10405=ORIENTED_EDGE('',*,*,#7799,.F.);
#10406=ORIENTED_EDGE('',*,*,#7800,.T.);
#10407=ORIENTED_EDGE('',*,*,#7801,.F.);
#10408=ORIENTED_EDGE('',*,*,#7709,.F.);
#10409=ORIENTED_EDGE('',*,*,#7802,.F.);
#10410=ORIENTED_EDGE('',*,*,#7710,.F.);
#10411=ORIENTED_EDGE('',*,*,#7801,.T.);
#10412=ORIENTED_EDGE('',*,*,#7803,.T.);
#10413=ORIENTED_EDGE('',*,*,#7804,.F.);
#10414=ORIENTED_EDGE('',*,*,#7803,.F.);
#10415=ORIENTED_EDGE('',*,*,#7800,.F.);
#10416=ORIENTED_EDGE('',*,*,#7805,.F.);
#10417=ORIENTED_EDGE('',*,*,#7806,.T.);
#10418=ORIENTED_EDGE('',*,*,#7807,.F.);
#10419=ORIENTED_EDGE('',*,*,#7712,.F.);
#10420=ORIENTED_EDGE('',*,*,#7808,.F.);
#10421=ORIENTED_EDGE('',*,*,#7713,.F.);
#10422=ORIENTED_EDGE('',*,*,#7807,.T.);
#10423=ORIENTED_EDGE('',*,*,#7809,.T.);
#10424=ORIENTED_EDGE('',*,*,#7810,.F.);
#10425=ORIENTED_EDGE('',*,*,#7809,.F.);
#10426=ORIENTED_EDGE('',*,*,#7806,.F.);
#10427=ORIENTED_EDGE('',*,*,#7811,.F.);
#10428=ORIENTED_EDGE('',*,*,#7812,.T.);
#10429=ORIENTED_EDGE('',*,*,#7813,.F.);
#10430=ORIENTED_EDGE('',*,*,#7715,.F.);
#10431=ORIENTED_EDGE('',*,*,#7814,.F.);
#10432=ORIENTED_EDGE('',*,*,#7716,.F.);
#10433=ORIENTED_EDGE('',*,*,#7813,.T.);
#10434=ORIENTED_EDGE('',*,*,#7815,.T.);
#10435=ORIENTED_EDGE('',*,*,#7816,.F.);
#10436=ORIENTED_EDGE('',*,*,#7815,.F.);
#10437=ORIENTED_EDGE('',*,*,#7812,.F.);
#10438=ORIENTED_EDGE('',*,*,#7817,.F.);
#10439=ORIENTED_EDGE('',*,*,#7818,.T.);
#10440=ORIENTED_EDGE('',*,*,#7819,.F.);
#10441=ORIENTED_EDGE('',*,*,#7718,.F.);
#10442=ORIENTED_EDGE('',*,*,#7820,.F.);
#10443=ORIENTED_EDGE('',*,*,#7613,.F.);
#10444=ORIENTED_EDGE('',*,*,#7819,.T.);
#10445=ORIENTED_EDGE('',*,*,#7821,.T.);
#10446=ORIENTED_EDGE('',*,*,#7822,.F.);
#10447=ORIENTED_EDGE('',*,*,#7821,.F.);
#10448=ORIENTED_EDGE('',*,*,#7818,.F.);
#10449=ORIENTED_EDGE('',*,*,#7823,.F.);
#10450=ORIENTED_EDGE('',*,*,#7824,.F.);
#10451=ORIENTED_EDGE('',*,*,#7825,.T.);
#10452=ORIENTED_EDGE('',*,*,#7826,.F.);
#10453=ORIENTED_EDGE('',*,*,#7615,.F.);
#10454=ORIENTED_EDGE('',*,*,#7827,.F.);
#10455=ORIENTED_EDGE('',*,*,#7616,.F.);
#10456=ORIENTED_EDGE('',*,*,#7826,.T.);
#10457=ORIENTED_EDGE('',*,*,#7828,.T.);
#10458=ORIENTED_EDGE('',*,*,#7829,.F.);
#10459=ORIENTED_EDGE('',*,*,#7828,.F.);
#10460=ORIENTED_EDGE('',*,*,#7825,.F.);
#10461=ORIENTED_EDGE('',*,*,#7830,.F.);
#10462=ORIENTED_EDGE('',*,*,#7831,.T.);
#10463=ORIENTED_EDGE('',*,*,#7832,.F.);
#10464=ORIENTED_EDGE('',*,*,#7618,.F.);
#10465=ORIENTED_EDGE('',*,*,#7833,.F.);
#10466=ORIENTED_EDGE('',*,*,#7619,.F.);
#10467=ORIENTED_EDGE('',*,*,#7832,.T.);
#10468=ORIENTED_EDGE('',*,*,#7834,.T.);
#10469=ORIENTED_EDGE('',*,*,#7835,.F.);
#10470=ORIENTED_EDGE('',*,*,#7834,.F.);
#10471=ORIENTED_EDGE('',*,*,#7831,.F.);
#10472=ORIENTED_EDGE('',*,*,#7836,.F.);
#10473=ORIENTED_EDGE('',*,*,#7837,.T.);
#10474=ORIENTED_EDGE('',*,*,#7838,.F.);
#10475=ORIENTED_EDGE('',*,*,#7621,.F.);
#10476=ORIENTED_EDGE('',*,*,#7839,.F.);
#10477=ORIENTED_EDGE('',*,*,#7622,.F.);
#10478=ORIENTED_EDGE('',*,*,#7838,.T.);
#10479=ORIENTED_EDGE('',*,*,#7840,.T.);
#10480=ORIENTED_EDGE('',*,*,#7841,.F.);
#10481=ORIENTED_EDGE('',*,*,#7840,.F.);
#10482=ORIENTED_EDGE('',*,*,#7837,.F.);
#10483=ORIENTED_EDGE('',*,*,#7842,.F.);
#10484=ORIENTED_EDGE('',*,*,#7843,.T.);
#10485=ORIENTED_EDGE('',*,*,#7844,.F.);
#10486=ORIENTED_EDGE('',*,*,#7624,.F.);
#10487=ORIENTED_EDGE('',*,*,#7845,.F.);
#10488=ORIENTED_EDGE('',*,*,#7625,.F.);
#10489=ORIENTED_EDGE('',*,*,#7844,.T.);
#10490=ORIENTED_EDGE('',*,*,#7846,.T.);
#10491=ORIENTED_EDGE('',*,*,#7847,.F.);
#10492=ORIENTED_EDGE('',*,*,#7846,.F.);
#10493=ORIENTED_EDGE('',*,*,#7843,.F.);
#10494=ORIENTED_EDGE('',*,*,#7848,.F.);
#10495=ORIENTED_EDGE('',*,*,#7849,.T.);
#10496=ORIENTED_EDGE('',*,*,#7850,.F.);
#10497=ORIENTED_EDGE('',*,*,#7627,.F.);
#10498=ORIENTED_EDGE('',*,*,#7851,.F.);
#10499=ORIENTED_EDGE('',*,*,#7628,.F.);
#10500=ORIENTED_EDGE('',*,*,#7850,.T.);
#10501=ORIENTED_EDGE('',*,*,#7852,.T.);
#10502=ORIENTED_EDGE('',*,*,#7853,.F.);
#10503=ORIENTED_EDGE('',*,*,#7852,.F.);
#10504=ORIENTED_EDGE('',*,*,#7849,.F.);
#10505=ORIENTED_EDGE('',*,*,#7854,.F.);
#10506=ORIENTED_EDGE('',*,*,#7855,.T.);
#10507=ORIENTED_EDGE('',*,*,#7856,.F.);
#10508=ORIENTED_EDGE('',*,*,#7630,.F.);
#10509=ORIENTED_EDGE('',*,*,#7857,.F.);
#10510=ORIENTED_EDGE('',*,*,#7631,.F.);
#10511=ORIENTED_EDGE('',*,*,#7856,.T.);
#10512=ORIENTED_EDGE('',*,*,#7858,.T.);
#10513=ORIENTED_EDGE('',*,*,#7859,.F.);
#10514=ORIENTED_EDGE('',*,*,#7858,.F.);
#10515=ORIENTED_EDGE('',*,*,#7855,.F.);
#10516=ORIENTED_EDGE('',*,*,#7860,.F.);
#10517=ORIENTED_EDGE('',*,*,#7861,.T.);
#10518=ORIENTED_EDGE('',*,*,#7862,.F.);
#10519=ORIENTED_EDGE('',*,*,#7633,.F.);
#10520=ORIENTED_EDGE('',*,*,#7863,.F.);
#10521=ORIENTED_EDGE('',*,*,#7634,.F.);
#10522=ORIENTED_EDGE('',*,*,#7862,.T.);
#10523=ORIENTED_EDGE('',*,*,#7864,.T.);
#10524=ORIENTED_EDGE('',*,*,#7865,.F.);
#10525=ORIENTED_EDGE('',*,*,#7864,.F.);
#10526=ORIENTED_EDGE('',*,*,#7861,.F.);
#10527=ORIENTED_EDGE('',*,*,#7866,.F.);
#10528=ORIENTED_EDGE('',*,*,#7867,.T.);
#10529=ORIENTED_EDGE('',*,*,#7868,.F.);
#10530=ORIENTED_EDGE('',*,*,#7636,.F.);
#10531=ORIENTED_EDGE('',*,*,#7869,.F.);
#10532=ORIENTED_EDGE('',*,*,#7637,.F.);
#10533=ORIENTED_EDGE('',*,*,#7868,.T.);
#10534=ORIENTED_EDGE('',*,*,#7870,.T.);
#10535=ORIENTED_EDGE('',*,*,#7871,.F.);
#10536=ORIENTED_EDGE('',*,*,#7870,.F.);
#10537=ORIENTED_EDGE('',*,*,#7867,.F.);
#10538=ORIENTED_EDGE('',*,*,#7872,.F.);
#10539=ORIENTED_EDGE('',*,*,#7873,.T.);
#10540=ORIENTED_EDGE('',*,*,#7874,.F.);
#10541=ORIENTED_EDGE('',*,*,#7639,.F.);
#10542=ORIENTED_EDGE('',*,*,#7875,.F.);
#10543=ORIENTED_EDGE('',*,*,#7640,.F.);
#10544=ORIENTED_EDGE('',*,*,#7874,.T.);
#10545=ORIENTED_EDGE('',*,*,#7876,.T.);
#10546=ORIENTED_EDGE('',*,*,#7877,.F.);
#10547=ORIENTED_EDGE('',*,*,#7876,.F.);
#10548=ORIENTED_EDGE('',*,*,#7873,.F.);
#10549=ORIENTED_EDGE('',*,*,#7878,.F.);
#10550=ORIENTED_EDGE('',*,*,#7879,.T.);
#10551=ORIENTED_EDGE('',*,*,#7880,.F.);
#10552=ORIENTED_EDGE('',*,*,#7642,.F.);
#10553=ORIENTED_EDGE('',*,*,#7881,.F.);
#10554=ORIENTED_EDGE('',*,*,#7643,.F.);
#10555=ORIENTED_EDGE('',*,*,#7880,.T.);
#10556=ORIENTED_EDGE('',*,*,#7882,.T.);
#10557=ORIENTED_EDGE('',*,*,#7883,.F.);
#10558=ORIENTED_EDGE('',*,*,#7882,.F.);
#10559=ORIENTED_EDGE('',*,*,#7879,.F.);
#10560=ORIENTED_EDGE('',*,*,#7884,.F.);
#10561=ORIENTED_EDGE('',*,*,#7885,.T.);
#10562=ORIENTED_EDGE('',*,*,#7886,.F.);
#10563=ORIENTED_EDGE('',*,*,#7645,.F.);
#10564=ORIENTED_EDGE('',*,*,#7887,.F.);
#10565=ORIENTED_EDGE('',*,*,#7646,.F.);
#10566=ORIENTED_EDGE('',*,*,#7886,.T.);
#10567=ORIENTED_EDGE('',*,*,#7888,.T.);
#10568=ORIENTED_EDGE('',*,*,#7889,.F.);
#10569=ORIENTED_EDGE('',*,*,#7888,.F.);
#10570=ORIENTED_EDGE('',*,*,#7885,.F.);
#10571=ORIENTED_EDGE('',*,*,#7890,.F.);
#10572=ORIENTED_EDGE('',*,*,#7891,.T.);
#10573=ORIENTED_EDGE('',*,*,#7892,.F.);
#10574=ORIENTED_EDGE('',*,*,#7648,.F.);
#10575=ORIENTED_EDGE('',*,*,#7893,.F.);
#10576=ORIENTED_EDGE('',*,*,#7649,.F.);
#10577=ORIENTED_EDGE('',*,*,#7892,.T.);
#10578=ORIENTED_EDGE('',*,*,#7894,.T.);
#10579=ORIENTED_EDGE('',*,*,#7895,.F.);
#10580=ORIENTED_EDGE('',*,*,#7894,.F.);
#10581=ORIENTED_EDGE('',*,*,#7891,.F.);
#10582=ORIENTED_EDGE('',*,*,#7896,.F.);
#10583=ORIENTED_EDGE('',*,*,#7897,.T.);
#10584=ORIENTED_EDGE('',*,*,#7898,.F.);
#10585=ORIENTED_EDGE('',*,*,#7651,.F.);
#10586=ORIENTED_EDGE('',*,*,#7899,.F.);
#10587=ORIENTED_EDGE('',*,*,#7652,.F.);
#10588=ORIENTED_EDGE('',*,*,#7898,.T.);
#10589=ORIENTED_EDGE('',*,*,#7900,.T.);
#10590=ORIENTED_EDGE('',*,*,#7901,.F.);
#10591=ORIENTED_EDGE('',*,*,#7900,.F.);
#10592=ORIENTED_EDGE('',*,*,#7897,.F.);
#10593=ORIENTED_EDGE('',*,*,#7902,.F.);
#10594=ORIENTED_EDGE('',*,*,#7903,.T.);
#10595=ORIENTED_EDGE('',*,*,#7904,.F.);
#10596=ORIENTED_EDGE('',*,*,#7654,.F.);
#10597=ORIENTED_EDGE('',*,*,#7905,.F.);
#10598=ORIENTED_EDGE('',*,*,#7655,.F.);
#10599=ORIENTED_EDGE('',*,*,#7904,.T.);
#10600=ORIENTED_EDGE('',*,*,#7906,.T.);
#10601=ORIENTED_EDGE('',*,*,#7907,.F.);
#10602=ORIENTED_EDGE('',*,*,#7906,.F.);
#10603=ORIENTED_EDGE('',*,*,#7903,.F.);
#10604=ORIENTED_EDGE('',*,*,#7908,.F.);
#10605=ORIENTED_EDGE('',*,*,#7909,.T.);
#10606=ORIENTED_EDGE('',*,*,#7910,.F.);
#10607=ORIENTED_EDGE('',*,*,#7657,.F.);
#10608=ORIENTED_EDGE('',*,*,#7911,.F.);
#10609=ORIENTED_EDGE('',*,*,#7658,.F.);
#10610=ORIENTED_EDGE('',*,*,#7910,.T.);
#10611=ORIENTED_EDGE('',*,*,#7912,.T.);
#10612=ORIENTED_EDGE('',*,*,#7913,.F.);
#10613=ORIENTED_EDGE('',*,*,#7912,.F.);
#10614=ORIENTED_EDGE('',*,*,#7909,.F.);
#10615=ORIENTED_EDGE('',*,*,#7914,.F.);
#10616=ORIENTED_EDGE('',*,*,#7915,.T.);
#10617=ORIENTED_EDGE('',*,*,#7916,.F.);
#10618=ORIENTED_EDGE('',*,*,#7660,.F.);
#10619=ORIENTED_EDGE('',*,*,#7917,.F.);
#10620=ORIENTED_EDGE('',*,*,#7661,.F.);
#10621=ORIENTED_EDGE('',*,*,#7916,.T.);
#10622=ORIENTED_EDGE('',*,*,#7918,.T.);
#10623=ORIENTED_EDGE('',*,*,#7919,.F.);
#10624=ORIENTED_EDGE('',*,*,#7918,.F.);
#10625=ORIENTED_EDGE('',*,*,#7915,.F.);
#10626=ORIENTED_EDGE('',*,*,#7920,.F.);
#10627=ORIENTED_EDGE('',*,*,#7921,.T.);
#10628=ORIENTED_EDGE('',*,*,#7922,.F.);
#10629=ORIENTED_EDGE('',*,*,#7663,.F.);
#10630=ORIENTED_EDGE('',*,*,#7923,.F.);
#10631=ORIENTED_EDGE('',*,*,#7664,.F.);
#10632=ORIENTED_EDGE('',*,*,#7922,.T.);
#10633=ORIENTED_EDGE('',*,*,#7924,.T.);
#10634=ORIENTED_EDGE('',*,*,#7925,.F.);
#10635=ORIENTED_EDGE('',*,*,#7924,.F.);
#10636=ORIENTED_EDGE('',*,*,#7921,.F.);
#10637=ORIENTED_EDGE('',*,*,#7926,.F.);
#10638=ORIENTED_EDGE('',*,*,#7927,.T.);
#10639=ORIENTED_EDGE('',*,*,#7928,.F.);
#10640=ORIENTED_EDGE('',*,*,#7666,.F.);
#10641=ORIENTED_EDGE('',*,*,#7929,.F.);
#10642=ORIENTED_EDGE('',*,*,#7667,.F.);
#10643=ORIENTED_EDGE('',*,*,#7928,.T.);
#10644=ORIENTED_EDGE('',*,*,#7930,.T.);
#10645=ORIENTED_EDGE('',*,*,#7931,.F.);
#10646=ORIENTED_EDGE('',*,*,#7930,.F.);
#10647=ORIENTED_EDGE('',*,*,#7927,.F.);
#10648=ORIENTED_EDGE('',*,*,#7822,.T.);
#10649=ORIENTED_EDGE('',*,*,#7932,.T.);
#10650=ORIENTED_EDGE('',*,*,#7602,.T.);
#10651=ORIENTED_EDGE('',*,*,#7932,.F.);
#10652=ORIENTED_EDGE('',*,*,#7823,.T.);
#10653=ORIENTED_EDGE('',*,*,#7817,.T.);
#10654=ORIENTED_EDGE('',*,*,#7717,.F.);
#10655=ORIENTED_EDGE('',*,*,#7814,.T.);
#10656=ORIENTED_EDGE('',*,*,#7816,.T.);
#10657=ORIENTED_EDGE('',*,*,#7811,.T.);
#10658=ORIENTED_EDGE('',*,*,#7714,.F.);
#10659=ORIENTED_EDGE('',*,*,#7808,.T.);
#10660=ORIENTED_EDGE('',*,*,#7810,.T.);
#10661=ORIENTED_EDGE('',*,*,#7805,.T.);
#10662=ORIENTED_EDGE('',*,*,#7711,.F.);
#10663=ORIENTED_EDGE('',*,*,#7802,.T.);
#10664=ORIENTED_EDGE('',*,*,#7804,.T.);
#10665=ORIENTED_EDGE('',*,*,#7799,.T.);
#10666=ORIENTED_EDGE('',*,*,#7708,.F.);
#10667=ORIENTED_EDGE('',*,*,#7796,.T.);
#10668=ORIENTED_EDGE('',*,*,#7798,.T.);
#10669=ORIENTED_EDGE('',*,*,#7793,.T.);
#10670=ORIENTED_EDGE('',*,*,#7705,.F.);
#10671=ORIENTED_EDGE('',*,*,#7790,.T.);
#10672=ORIENTED_EDGE('',*,*,#7792,.T.);
#10673=ORIENTED_EDGE('',*,*,#7787,.T.);
#10674=ORIENTED_EDGE('',*,*,#7702,.F.);
#10675=ORIENTED_EDGE('',*,*,#7784,.T.);
#10676=ORIENTED_EDGE('',*,*,#7786,.T.);
#10677=ORIENTED_EDGE('',*,*,#7781,.T.);
#10678=ORIENTED_EDGE('',*,*,#7699,.F.);
#10679=ORIENTED_EDGE('',*,*,#7778,.T.);
#10680=ORIENTED_EDGE('',*,*,#7780,.T.);
#10681=ORIENTED_EDGE('',*,*,#7775,.T.);
#10682=ORIENTED_EDGE('',*,*,#7696,.F.);
#10683=ORIENTED_EDGE('',*,*,#7772,.T.);
#10684=ORIENTED_EDGE('',*,*,#7774,.T.);
#10685=ORIENTED_EDGE('',*,*,#7769,.T.);
#10686=ORIENTED_EDGE('',*,*,#7693,.F.);
#10687=ORIENTED_EDGE('',*,*,#7766,.T.);
#10688=ORIENTED_EDGE('',*,*,#7768,.T.);
#10689=ORIENTED_EDGE('',*,*,#7763,.T.);
#10690=ORIENTED_EDGE('',*,*,#7690,.F.);
#10691=ORIENTED_EDGE('',*,*,#7760,.T.);
#10692=ORIENTED_EDGE('',*,*,#7762,.T.);
#10693=ORIENTED_EDGE('',*,*,#7757,.T.);
#10694=ORIENTED_EDGE('',*,*,#7687,.F.);
#10695=ORIENTED_EDGE('',*,*,#7754,.T.);
#10696=ORIENTED_EDGE('',*,*,#7756,.T.);
#10697=ORIENTED_EDGE('',*,*,#7751,.T.);
#10698=ORIENTED_EDGE('',*,*,#7684,.F.);
#10699=ORIENTED_EDGE('',*,*,#7748,.T.);
#10700=ORIENTED_EDGE('',*,*,#7750,.T.);
#10701=ORIENTED_EDGE('',*,*,#7745,.T.);
#10702=ORIENTED_EDGE('',*,*,#7681,.F.);
#10703=ORIENTED_EDGE('',*,*,#7742,.T.);
#10704=ORIENTED_EDGE('',*,*,#7744,.T.);
#10705=ORIENTED_EDGE('',*,*,#7739,.T.);
#10706=ORIENTED_EDGE('',*,*,#7678,.F.);
#10707=ORIENTED_EDGE('',*,*,#7736,.T.);
#10708=ORIENTED_EDGE('',*,*,#7738,.T.);
#10709=ORIENTED_EDGE('',*,*,#7733,.T.);
#10710=ORIENTED_EDGE('',*,*,#7675,.F.);
#10711=ORIENTED_EDGE('',*,*,#7730,.T.);
#10712=ORIENTED_EDGE('',*,*,#7732,.T.);
#10713=ORIENTED_EDGE('',*,*,#7727,.T.);
#10714=ORIENTED_EDGE('',*,*,#7672,.F.);
#10715=ORIENTED_EDGE('',*,*,#7724,.T.);
#10716=ORIENTED_EDGE('',*,*,#7726,.T.);
#10717=ORIENTED_EDGE('',*,*,#7721,.T.);
#10718=ORIENTED_EDGE('',*,*,#7669,.F.);
#10719=ORIENTED_EDGE('',*,*,#7609,.T.);
#10720=ORIENTED_EDGE('',*,*,#7612,.T.);
#10721=ORIENTED_EDGE('',*,*,#7605,.T.);
#10722=ORIENTED_EDGE('',*,*,#7668,.F.);
#10723=ORIENTED_EDGE('',*,*,#7929,.T.);
#10724=ORIENTED_EDGE('',*,*,#7931,.T.);
#10725=ORIENTED_EDGE('',*,*,#7926,.T.);
#10726=ORIENTED_EDGE('',*,*,#7665,.F.);
#10727=ORIENTED_EDGE('',*,*,#7923,.T.);
#10728=ORIENTED_EDGE('',*,*,#7925,.T.);
#10729=ORIENTED_EDGE('',*,*,#7920,.T.);
#10730=ORIENTED_EDGE('',*,*,#7662,.F.);
#10731=ORIENTED_EDGE('',*,*,#7917,.T.);
#10732=ORIENTED_EDGE('',*,*,#7919,.T.);
#10733=ORIENTED_EDGE('',*,*,#7914,.T.);
#10734=ORIENTED_EDGE('',*,*,#7659,.F.);
#10735=ORIENTED_EDGE('',*,*,#7911,.T.);
#10736=ORIENTED_EDGE('',*,*,#7913,.T.);
#10737=ORIENTED_EDGE('',*,*,#7908,.T.);
#10738=ORIENTED_EDGE('',*,*,#7656,.F.);
#10739=ORIENTED_EDGE('',*,*,#7905,.T.);
#10740=ORIENTED_EDGE('',*,*,#7907,.T.);
#10741=ORIENTED_EDGE('',*,*,#7902,.T.);
#10742=ORIENTED_EDGE('',*,*,#7653,.F.);
#10743=ORIENTED_EDGE('',*,*,#7899,.T.);
#10744=ORIENTED_EDGE('',*,*,#7901,.T.);
#10745=ORIENTED_EDGE('',*,*,#7896,.T.);
#10746=ORIENTED_EDGE('',*,*,#7650,.F.);
#10747=ORIENTED_EDGE('',*,*,#7893,.T.);
#10748=ORIENTED_EDGE('',*,*,#7895,.T.);
#10749=ORIENTED_EDGE('',*,*,#7890,.T.);
#10750=ORIENTED_EDGE('',*,*,#7647,.F.);
#10751=ORIENTED_EDGE('',*,*,#7887,.T.);
#10752=ORIENTED_EDGE('',*,*,#7889,.T.);
#10753=ORIENTED_EDGE('',*,*,#7884,.T.);
#10754=ORIENTED_EDGE('',*,*,#7644,.F.);
#10755=ORIENTED_EDGE('',*,*,#7881,.T.);
#10756=ORIENTED_EDGE('',*,*,#7883,.T.);
#10757=ORIENTED_EDGE('',*,*,#7878,.T.);
#10758=ORIENTED_EDGE('',*,*,#7641,.F.);
#10759=ORIENTED_EDGE('',*,*,#7875,.T.);
#10760=ORIENTED_EDGE('',*,*,#7877,.T.);
#10761=ORIENTED_EDGE('',*,*,#7872,.T.);
#10762=ORIENTED_EDGE('',*,*,#7638,.F.);
#10763=ORIENTED_EDGE('',*,*,#7869,.T.);
#10764=ORIENTED_EDGE('',*,*,#7871,.T.);
#10765=ORIENTED_EDGE('',*,*,#7866,.T.);
#10766=ORIENTED_EDGE('',*,*,#7635,.F.);
#10767=ORIENTED_EDGE('',*,*,#7863,.T.);
#10768=ORIENTED_EDGE('',*,*,#7865,.T.);
#10769=ORIENTED_EDGE('',*,*,#7860,.T.);
#10770=ORIENTED_EDGE('',*,*,#7632,.F.);
#10771=ORIENTED_EDGE('',*,*,#7857,.T.);
#10772=ORIENTED_EDGE('',*,*,#7859,.T.);
#10773=ORIENTED_EDGE('',*,*,#7854,.T.);
#10774=ORIENTED_EDGE('',*,*,#7629,.F.);
#10775=ORIENTED_EDGE('',*,*,#7851,.T.);
#10776=ORIENTED_EDGE('',*,*,#7853,.T.);
#10777=ORIENTED_EDGE('',*,*,#7848,.T.);
#10778=ORIENTED_EDGE('',*,*,#7626,.F.);
#10779=ORIENTED_EDGE('',*,*,#7845,.T.);
#10780=ORIENTED_EDGE('',*,*,#7847,.T.);
#10781=ORIENTED_EDGE('',*,*,#7842,.T.);
#10782=ORIENTED_EDGE('',*,*,#7623,.F.);
#10783=ORIENTED_EDGE('',*,*,#7839,.T.);
#10784=ORIENTED_EDGE('',*,*,#7841,.T.);
#10785=ORIENTED_EDGE('',*,*,#7836,.T.);
#10786=ORIENTED_EDGE('',*,*,#7620,.F.);
#10787=ORIENTED_EDGE('',*,*,#7833,.T.);
#10788=ORIENTED_EDGE('',*,*,#7835,.T.);
#10789=ORIENTED_EDGE('',*,*,#7830,.T.);
#10790=ORIENTED_EDGE('',*,*,#7617,.F.);
#10791=ORIENTED_EDGE('',*,*,#7827,.T.);
#10792=ORIENTED_EDGE('',*,*,#7829,.T.);
#10793=ORIENTED_EDGE('',*,*,#7824,.T.);
#10794=ORIENTED_EDGE('',*,*,#7614,.F.);
#10795=ORIENTED_EDGE('',*,*,#7820,.T.);
#10796=ORIENTED_EDGE('',*,*,#7720,.F.);
#10797=ORIENTED_EDGE('',*,*,#7933,.T.);
#10798=ORIENTED_EDGE('',*,*,#7934,.T.);
#10799=ORIENTED_EDGE('',*,*,#7935,.T.);
#10800=ORIENTED_EDGE('',*,*,#7936,.T.);
#10801=ORIENTED_EDGE('',*,*,#7937,.T.);
#10802=ORIENTED_EDGE('',*,*,#7938,.T.);
#10803=ORIENTED_EDGE('',*,*,#7939,.F.);
#10804=ORIENTED_EDGE('',*,*,#7940,.T.);
#10805=ORIENTED_EDGE('',*,*,#7941,.F.);
#10806=ORIENTED_EDGE('',*,*,#7942,.T.);
#10807=ORIENTED_EDGE('',*,*,#7943,.F.);
#10808=ORIENTED_EDGE('',*,*,#7944,.T.);
#10809=ORIENTED_EDGE('',*,*,#7945,.F.);
#10810=ORIENTED_EDGE('',*,*,#7946,.T.);
#10811=ORIENTED_EDGE('',*,*,#7947,.F.);
#10812=ORIENTED_EDGE('',*,*,#7948,.T.);
#10813=ORIENTED_EDGE('',*,*,#7949,.F.);
#10814=ORIENTED_EDGE('',*,*,#7950,.T.);
#10815=ORIENTED_EDGE('',*,*,#7951,.T.);
#10816=ORIENTED_EDGE('',*,*,#7950,.F.);
#10817=ORIENTED_EDGE('',*,*,#7948,.F.);
#10818=ORIENTED_EDGE('',*,*,#7946,.F.);
#10819=ORIENTED_EDGE('',*,*,#7944,.F.);
#10820=ORIENTED_EDGE('',*,*,#7942,.F.);
#10821=ORIENTED_EDGE('',*,*,#7940,.F.);
#10822=ORIENTED_EDGE('',*,*,#7951,.F.);
#10823=ORIENTED_EDGE('',*,*,#7933,.F.);
#10824=ORIENTED_EDGE('',*,*,#7952,.T.);
#10825=ORIENTED_EDGE('',*,*,#7939,.T.);
#10826=ORIENTED_EDGE('',*,*,#7953,.F.);
#10827=ORIENTED_EDGE('',*,*,#7938,.F.);
#10828=ORIENTED_EDGE('',*,*,#7954,.T.);
#10829=ORIENTED_EDGE('',*,*,#7949,.T.);
#10830=ORIENTED_EDGE('',*,*,#7952,.F.);
#10831=ORIENTED_EDGE('',*,*,#7937,.F.);
#10832=ORIENTED_EDGE('',*,*,#7955,.T.);
#10833=ORIENTED_EDGE('',*,*,#7947,.T.);
#10834=ORIENTED_EDGE('',*,*,#7954,.F.);
#10835=ORIENTED_EDGE('',*,*,#7936,.F.);
#10836=ORIENTED_EDGE('',*,*,#7956,.T.);
#10837=ORIENTED_EDGE('',*,*,#7945,.T.);
#10838=ORIENTED_EDGE('',*,*,#7955,.F.);
#10839=ORIENTED_EDGE('',*,*,#7935,.F.);
#10840=ORIENTED_EDGE('',*,*,#7957,.T.);
#10841=ORIENTED_EDGE('',*,*,#7943,.T.);
#10842=ORIENTED_EDGE('',*,*,#7956,.F.);
#10843=ORIENTED_EDGE('',*,*,#7934,.F.);
#10844=ORIENTED_EDGE('',*,*,#7953,.T.);
#10845=ORIENTED_EDGE('',*,*,#7941,.T.);
#10846=ORIENTED_EDGE('',*,*,#7957,.F.);
#10847=ORIENTED_EDGE('',*,*,#7958,.F.);
#10848=ORIENTED_EDGE('',*,*,#7959,.F.);
#10849=ORIENTED_EDGE('',*,*,#7960,.F.);
#10850=ORIENTED_EDGE('',*,*,#7961,.T.);
#10851=ORIENTED_EDGE('',*,*,#7962,.F.);
#10852=ORIENTED_EDGE('',*,*,#7963,.F.);
#10853=ORIENTED_EDGE('',*,*,#7964,.F.);
#10854=ORIENTED_EDGE('',*,*,#7958,.T.);
#10855=ORIENTED_EDGE('',*,*,#7965,.T.);
#10856=ORIENTED_EDGE('',*,*,#7966,.T.);
#10857=ORIENTED_EDGE('',*,*,#7967,.F.);
#10858=ORIENTED_EDGE('',*,*,#7968,.F.);
#10859=ORIENTED_EDGE('',*,*,#7969,.F.);
#10860=ORIENTED_EDGE('',*,*,#7962,.T.);
#10861=ORIENTED_EDGE('',*,*,#7970,.T.);
#10862=ORIENTED_EDGE('',*,*,#7971,.F.);
#10863=ORIENTED_EDGE('',*,*,#7972,.F.);
#10864=ORIENTED_EDGE('',*,*,#7967,.T.);
#10865=ORIENTED_EDGE('',*,*,#7973,.T.);
#10866=ORIENTED_EDGE('',*,*,#7974,.T.);
#10867=ORIENTED_EDGE('',*,*,#7975,.F.);
#10868=ORIENTED_EDGE('',*,*,#7976,.F.);
#10869=ORIENTED_EDGE('',*,*,#7977,.F.);
#10870=ORIENTED_EDGE('',*,*,#7971,.T.);
#10871=ORIENTED_EDGE('',*,*,#7978,.T.);
#10872=ORIENTED_EDGE('',*,*,#7979,.F.);
#10873=ORIENTED_EDGE('',*,*,#7980,.F.);
#10874=ORIENTED_EDGE('',*,*,#7975,.T.);
#10875=ORIENTED_EDGE('',*,*,#7981,.T.);
#10876=ORIENTED_EDGE('',*,*,#7982,.T.);
#10877=ORIENTED_EDGE('',*,*,#7983,.F.);
#10878=ORIENTED_EDGE('',*,*,#7984,.F.);
#10879=ORIENTED_EDGE('',*,*,#7985,.F.);
#10880=ORIENTED_EDGE('',*,*,#7979,.T.);
#10881=ORIENTED_EDGE('',*,*,#7986,.T.);
#10882=ORIENTED_EDGE('',*,*,#7987,.F.);
#10883=ORIENTED_EDGE('',*,*,#7988,.F.);
#10884=ORIENTED_EDGE('',*,*,#7983,.T.);
#10885=ORIENTED_EDGE('',*,*,#7989,.T.);
#10886=ORIENTED_EDGE('',*,*,#7990,.T.);
#10887=ORIENTED_EDGE('',*,*,#7991,.F.);
#10888=ORIENTED_EDGE('',*,*,#7992,.F.);
#10889=ORIENTED_EDGE('',*,*,#7993,.F.);
#10890=ORIENTED_EDGE('',*,*,#7987,.T.);
#10891=ORIENTED_EDGE('',*,*,#7994,.T.);
#10892=ORIENTED_EDGE('',*,*,#7995,.F.);
#10893=ORIENTED_EDGE('',*,*,#7996,.F.);
#10894=ORIENTED_EDGE('',*,*,#7991,.T.);
#10895=ORIENTED_EDGE('',*,*,#7997,.T.);
#10896=ORIENTED_EDGE('',*,*,#7998,.T.);
#10897=ORIENTED_EDGE('',*,*,#7999,.F.);
#10898=ORIENTED_EDGE('',*,*,#8000,.F.);
#10899=ORIENTED_EDGE('',*,*,#8001,.F.);
#10900=ORIENTED_EDGE('',*,*,#7995,.T.);
#10901=ORIENTED_EDGE('',*,*,#8002,.T.);
#10902=ORIENTED_EDGE('',*,*,#8003,.F.);
#10903=ORIENTED_EDGE('',*,*,#8004,.F.);
#10904=ORIENTED_EDGE('',*,*,#7999,.T.);
#10905=ORIENTED_EDGE('',*,*,#8005,.T.);
#10906=ORIENTED_EDGE('',*,*,#8006,.T.);
#10907=ORIENTED_EDGE('',*,*,#8007,.F.);
#10908=ORIENTED_EDGE('',*,*,#8008,.F.);
#10909=ORIENTED_EDGE('',*,*,#8009,.F.);
#10910=ORIENTED_EDGE('',*,*,#8003,.T.);
#10911=ORIENTED_EDGE('',*,*,#8010,.T.);
#10912=ORIENTED_EDGE('',*,*,#8011,.F.);
#10913=ORIENTED_EDGE('',*,*,#8012,.F.);
#10914=ORIENTED_EDGE('',*,*,#8007,.T.);
#10915=ORIENTED_EDGE('',*,*,#8013,.T.);
#10916=ORIENTED_EDGE('',*,*,#8014,.T.);
#10917=ORIENTED_EDGE('',*,*,#8015,.F.);
#10918=ORIENTED_EDGE('',*,*,#8016,.F.);
#10919=ORIENTED_EDGE('',*,*,#8017,.F.);
#10920=ORIENTED_EDGE('',*,*,#8011,.T.);
#10921=ORIENTED_EDGE('',*,*,#8018,.T.);
#10922=ORIENTED_EDGE('',*,*,#8019,.F.);
#10923=ORIENTED_EDGE('',*,*,#8020,.F.);
#10924=ORIENTED_EDGE('',*,*,#8015,.T.);
#10925=ORIENTED_EDGE('',*,*,#8021,.T.);
#10926=ORIENTED_EDGE('',*,*,#8022,.T.);
#10927=ORIENTED_EDGE('',*,*,#8023,.F.);
#10928=ORIENTED_EDGE('',*,*,#8024,.F.);
#10929=ORIENTED_EDGE('',*,*,#8025,.F.);
#10930=ORIENTED_EDGE('',*,*,#8019,.T.);
#10931=ORIENTED_EDGE('',*,*,#8026,.T.);
#10932=ORIENTED_EDGE('',*,*,#8027,.F.);
#10933=ORIENTED_EDGE('',*,*,#8028,.F.);
#10934=ORIENTED_EDGE('',*,*,#8023,.T.);
#10935=ORIENTED_EDGE('',*,*,#8029,.T.);
#10936=ORIENTED_EDGE('',*,*,#8030,.T.);
#10937=ORIENTED_EDGE('',*,*,#8031,.F.);
#10938=ORIENTED_EDGE('',*,*,#8032,.F.);
#10939=ORIENTED_EDGE('',*,*,#8033,.F.);
#10940=ORIENTED_EDGE('',*,*,#8027,.T.);
#10941=ORIENTED_EDGE('',*,*,#8034,.T.);
#10942=ORIENTED_EDGE('',*,*,#8035,.F.);
#10943=ORIENTED_EDGE('',*,*,#8036,.F.);
#10944=ORIENTED_EDGE('',*,*,#8031,.T.);
#10945=ORIENTED_EDGE('',*,*,#8037,.T.);
#10946=ORIENTED_EDGE('',*,*,#8038,.T.);
#10947=ORIENTED_EDGE('',*,*,#8039,.F.);
#10948=ORIENTED_EDGE('',*,*,#8040,.F.);
#10949=ORIENTED_EDGE('',*,*,#8041,.F.);
#10950=ORIENTED_EDGE('',*,*,#8035,.T.);
#10951=ORIENTED_EDGE('',*,*,#8042,.T.);
#10952=ORIENTED_EDGE('',*,*,#8043,.F.);
#10953=ORIENTED_EDGE('',*,*,#8044,.F.);
#10954=ORIENTED_EDGE('',*,*,#8045,.F.);
#10955=ORIENTED_EDGE('',*,*,#8039,.T.);
#10956=ORIENTED_EDGE('',*,*,#8046,.T.);
#10957=ORIENTED_EDGE('',*,*,#8047,.T.);
#10958=ORIENTED_EDGE('',*,*,#8048,.F.);
#10959=ORIENTED_EDGE('',*,*,#8049,.F.);
#10960=ORIENTED_EDGE('',*,*,#8043,.T.);
#10961=ORIENTED_EDGE('',*,*,#8050,.T.);
#10962=ORIENTED_EDGE('',*,*,#8051,.F.);
#10963=ORIENTED_EDGE('',*,*,#8052,.F.);
#10964=ORIENTED_EDGE('',*,*,#8053,.F.);
#10965=ORIENTED_EDGE('',*,*,#8048,.T.);
#10966=ORIENTED_EDGE('',*,*,#8054,.T.);
#10967=ORIENTED_EDGE('',*,*,#8055,.T.);
#10968=ORIENTED_EDGE('',*,*,#8056,.F.);
#10969=ORIENTED_EDGE('',*,*,#8057,.F.);
#10970=ORIENTED_EDGE('',*,*,#8051,.T.);
#10971=ORIENTED_EDGE('',*,*,#8058,.T.);
#10972=ORIENTED_EDGE('',*,*,#8059,.T.);
#10973=ORIENTED_EDGE('',*,*,#8060,.F.);
#10974=ORIENTED_EDGE('',*,*,#8061,.F.);
#10975=ORIENTED_EDGE('',*,*,#8062,.F.);
#10976=ORIENTED_EDGE('',*,*,#8056,.T.);
#10977=ORIENTED_EDGE('',*,*,#8063,.T.);
#10978=ORIENTED_EDGE('',*,*,#8064,.F.);
#10979=ORIENTED_EDGE('',*,*,#8065,.F.);
#10980=ORIENTED_EDGE('',*,*,#8060,.T.);
#10981=ORIENTED_EDGE('',*,*,#8066,.T.);
#10982=ORIENTED_EDGE('',*,*,#8067,.T.);
#10983=ORIENTED_EDGE('',*,*,#8068,.T.);
#10984=ORIENTED_EDGE('',*,*,#8069,.F.);
#10985=ORIENTED_EDGE('',*,*,#8070,.T.);
#10986=ORIENTED_EDGE('',*,*,#8071,.T.);
#10987=ORIENTED_EDGE('',*,*,#8072,.T.);
#10988=ORIENTED_EDGE('',*,*,#8073,.T.);
#10989=ORIENTED_EDGE('',*,*,#8074,.T.);
#10990=ORIENTED_EDGE('',*,*,#8075,.T.);
#10991=ORIENTED_EDGE('',*,*,#8076,.T.);
#10992=ORIENTED_EDGE('',*,*,#8077,.T.);
#10993=ORIENTED_EDGE('',*,*,#8078,.T.);
#10994=ORIENTED_EDGE('',*,*,#8079,.T.);
#10995=ORIENTED_EDGE('',*,*,#8080,.T.);
#10996=ORIENTED_EDGE('',*,*,#8081,.T.);
#10997=ORIENTED_EDGE('',*,*,#8082,.T.);
#10998=ORIENTED_EDGE('',*,*,#8083,.T.);
#10999=ORIENTED_EDGE('',*,*,#8084,.T.);
#11000=ORIENTED_EDGE('',*,*,#8085,.T.);
#11001=ORIENTED_EDGE('',*,*,#8086,.T.);
#11002=ORIENTED_EDGE('',*,*,#8087,.T.);
#11003=ORIENTED_EDGE('',*,*,#8088,.T.);
#11004=ORIENTED_EDGE('',*,*,#8089,.T.);
#11005=ORIENTED_EDGE('',*,*,#8090,.T.);
#11006=ORIENTED_EDGE('',*,*,#8091,.T.);
#11007=ORIENTED_EDGE('',*,*,#8092,.T.);
#11008=ORIENTED_EDGE('',*,*,#8093,.T.);
#11009=ORIENTED_EDGE('',*,*,#8094,.T.);
#11010=ORIENTED_EDGE('',*,*,#8095,.T.);
#11011=ORIENTED_EDGE('',*,*,#8096,.T.);
#11012=ORIENTED_EDGE('',*,*,#8097,.T.);
#11013=ORIENTED_EDGE('',*,*,#8098,.T.);
#11014=ORIENTED_EDGE('',*,*,#8099,.F.);
#11015=ORIENTED_EDGE('',*,*,#8100,.F.);
#11016=ORIENTED_EDGE('',*,*,#8101,.T.);
#11017=ORIENTED_EDGE('',*,*,#8102,.T.);
#11018=ORIENTED_EDGE('',*,*,#8103,.T.);
#11019=ORIENTED_EDGE('',*,*,#8104,.T.);
#11020=ORIENTED_EDGE('',*,*,#8105,.T.);
#11021=ORIENTED_EDGE('',*,*,#8106,.T.);
#11022=ORIENTED_EDGE('',*,*,#8107,.T.);
#11023=ORIENTED_EDGE('',*,*,#8108,.T.);
#11024=ORIENTED_EDGE('',*,*,#8109,.T.);
#11025=ORIENTED_EDGE('',*,*,#8110,.T.);
#11026=ORIENTED_EDGE('',*,*,#8111,.T.);
#11027=ORIENTED_EDGE('',*,*,#8112,.T.);
#11028=ORIENTED_EDGE('',*,*,#8113,.T.);
#11029=ORIENTED_EDGE('',*,*,#8114,.T.);
#11030=ORIENTED_EDGE('',*,*,#8115,.T.);
#11031=ORIENTED_EDGE('',*,*,#8116,.T.);
#11032=ORIENTED_EDGE('',*,*,#8117,.T.);
#11033=ORIENTED_EDGE('',*,*,#8118,.T.);
#11034=ORIENTED_EDGE('',*,*,#8119,.T.);
#11035=ORIENTED_EDGE('',*,*,#8120,.T.);
#11036=ORIENTED_EDGE('',*,*,#8121,.T.);
#11037=ORIENTED_EDGE('',*,*,#8122,.T.);
#11038=ORIENTED_EDGE('',*,*,#8123,.T.);
#11039=ORIENTED_EDGE('',*,*,#8124,.T.);
#11040=ORIENTED_EDGE('',*,*,#8125,.T.);
#11041=ORIENTED_EDGE('',*,*,#8126,.T.);
#11042=ORIENTED_EDGE('',*,*,#8127,.T.);
#11043=ORIENTED_EDGE('',*,*,#8064,.T.);
#11044=ORIENTED_EDGE('',*,*,#8128,.T.);
#11045=ORIENTED_EDGE('',*,*,#8129,.T.);
#11046=ORIENTED_EDGE('',*,*,#8130,.F.);
#11047=ORIENTED_EDGE('',*,*,#8131,.F.);
#11048=ORIENTED_EDGE('',*,*,#8132,.F.);
#11049=ORIENTED_EDGE('',*,*,#8133,.F.);
#11050=ORIENTED_EDGE('',*,*,#8134,.T.);
#11051=ORIENTED_EDGE('',*,*,#8130,.T.);
#11052=ORIENTED_EDGE('',*,*,#8135,.T.);
#11053=ORIENTED_EDGE('',*,*,#8134,.F.);
#11054=ORIENTED_EDGE('',*,*,#8136,.F.);
#11055=ORIENTED_EDGE('',*,*,#8098,.F.);
#11056=ORIENTED_EDGE('',*,*,#8097,.F.);
#11057=ORIENTED_EDGE('',*,*,#8096,.F.);
#11058=ORIENTED_EDGE('',*,*,#8095,.F.);
#11059=ORIENTED_EDGE('',*,*,#8094,.F.);
#11060=ORIENTED_EDGE('',*,*,#8093,.F.);
#11061=ORIENTED_EDGE('',*,*,#8092,.F.);
#11062=ORIENTED_EDGE('',*,*,#8091,.F.);
#11063=ORIENTED_EDGE('',*,*,#8090,.F.);
#11064=ORIENTED_EDGE('',*,*,#8089,.F.);
#11065=ORIENTED_EDGE('',*,*,#8088,.F.);
#11066=ORIENTED_EDGE('',*,*,#8087,.F.);
#11067=ORIENTED_EDGE('',*,*,#8086,.F.);
#11068=ORIENTED_EDGE('',*,*,#8085,.F.);
#11069=ORIENTED_EDGE('',*,*,#8084,.F.);
#11070=ORIENTED_EDGE('',*,*,#8083,.F.);
#11071=ORIENTED_EDGE('',*,*,#8082,.F.);
#11072=ORIENTED_EDGE('',*,*,#8081,.F.);
#11073=ORIENTED_EDGE('',*,*,#8080,.F.);
#11074=ORIENTED_EDGE('',*,*,#8079,.F.);
#11075=ORIENTED_EDGE('',*,*,#8078,.F.);
#11076=ORIENTED_EDGE('',*,*,#8077,.F.);
#11077=ORIENTED_EDGE('',*,*,#8076,.F.);
#11078=ORIENTED_EDGE('',*,*,#8075,.F.);
#11079=ORIENTED_EDGE('',*,*,#8074,.F.);
#11080=ORIENTED_EDGE('',*,*,#8073,.F.);
#11081=ORIENTED_EDGE('',*,*,#8072,.F.);
#11082=ORIENTED_EDGE('',*,*,#8071,.F.);
#11083=ORIENTED_EDGE('',*,*,#8070,.F.);
#11084=ORIENTED_EDGE('',*,*,#8137,.F.);
#11085=ORIENTED_EDGE('',*,*,#7959,.T.);
#11086=ORIENTED_EDGE('',*,*,#7964,.T.);
#11087=ORIENTED_EDGE('',*,*,#7963,.T.);
#11088=ORIENTED_EDGE('',*,*,#7969,.T.);
#11089=ORIENTED_EDGE('',*,*,#7968,.T.);
#11090=ORIENTED_EDGE('',*,*,#7972,.T.);
#11091=ORIENTED_EDGE('',*,*,#7977,.T.);
#11092=ORIENTED_EDGE('',*,*,#7976,.T.);
#11093=ORIENTED_EDGE('',*,*,#7980,.T.);
#11094=ORIENTED_EDGE('',*,*,#7985,.T.);
#11095=ORIENTED_EDGE('',*,*,#7984,.T.);
#11096=ORIENTED_EDGE('',*,*,#7988,.T.);
#11097=ORIENTED_EDGE('',*,*,#7993,.T.);
#11098=ORIENTED_EDGE('',*,*,#7992,.T.);
#11099=ORIENTED_EDGE('',*,*,#7996,.T.);
#11100=ORIENTED_EDGE('',*,*,#8001,.T.);
#11101=ORIENTED_EDGE('',*,*,#8000,.T.);
#11102=ORIENTED_EDGE('',*,*,#8004,.T.);
#11103=ORIENTED_EDGE('',*,*,#8009,.T.);
#11104=ORIENTED_EDGE('',*,*,#8008,.T.);
#11105=ORIENTED_EDGE('',*,*,#8012,.T.);
#11106=ORIENTED_EDGE('',*,*,#8017,.T.);
#11107=ORIENTED_EDGE('',*,*,#8016,.T.);
#11108=ORIENTED_EDGE('',*,*,#8020,.T.);
#11109=ORIENTED_EDGE('',*,*,#8025,.T.);
#11110=ORIENTED_EDGE('',*,*,#8024,.T.);
#11111=ORIENTED_EDGE('',*,*,#8028,.T.);
#11112=ORIENTED_EDGE('',*,*,#8033,.T.);
#11113=ORIENTED_EDGE('',*,*,#8032,.T.);
#11114=ORIENTED_EDGE('',*,*,#8036,.T.);
#11115=ORIENTED_EDGE('',*,*,#8041,.T.);
#11116=ORIENTED_EDGE('',*,*,#8040,.T.);
#11117=ORIENTED_EDGE('',*,*,#8045,.T.);
#11118=ORIENTED_EDGE('',*,*,#8044,.T.);
#11119=ORIENTED_EDGE('',*,*,#8049,.T.);
#11120=ORIENTED_EDGE('',*,*,#8053,.T.);
#11121=ORIENTED_EDGE('',*,*,#8052,.T.);
#11122=ORIENTED_EDGE('',*,*,#8057,.T.);
#11123=ORIENTED_EDGE('',*,*,#8062,.T.);
#11124=ORIENTED_EDGE('',*,*,#8061,.T.);
#11125=ORIENTED_EDGE('',*,*,#8065,.T.);
#11126=ORIENTED_EDGE('',*,*,#8132,.T.);
#11127=ORIENTED_EDGE('',*,*,#8131,.T.);
#11128=ORIENTED_EDGE('',*,*,#8138,.F.);
#11129=ORIENTED_EDGE('',*,*,#8139,.T.);
#11130=ORIENTED_EDGE('',*,*,#7960,.T.);
#11131=ORIENTED_EDGE('',*,*,#8137,.T.);
#11132=ORIENTED_EDGE('',*,*,#8140,.F.);
#11133=ORIENTED_EDGE('',*,*,#8135,.F.);
#11134=ORIENTED_EDGE('',*,*,#8129,.F.);
#11135=ORIENTED_EDGE('',*,*,#8128,.F.);
#11136=ORIENTED_EDGE('',*,*,#8067,.F.);
#11137=ORIENTED_EDGE('',*,*,#8066,.F.);
#11138=ORIENTED_EDGE('',*,*,#8063,.F.);
#11139=ORIENTED_EDGE('',*,*,#8059,.F.);
#11140=ORIENTED_EDGE('',*,*,#8058,.F.);
#11141=ORIENTED_EDGE('',*,*,#8055,.F.);
#11142=ORIENTED_EDGE('',*,*,#8054,.F.);
#11143=ORIENTED_EDGE('',*,*,#8050,.F.);
#11144=ORIENTED_EDGE('',*,*,#8047,.F.);
#11145=ORIENTED_EDGE('',*,*,#8046,.F.);
#11146=ORIENTED_EDGE('',*,*,#8042,.F.);
#11147=ORIENTED_EDGE('',*,*,#8038,.F.);
#11148=ORIENTED_EDGE('',*,*,#8037,.F.);
#11149=ORIENTED_EDGE('',*,*,#8034,.F.);
#11150=ORIENTED_EDGE('',*,*,#8030,.F.);
#11151=ORIENTED_EDGE('',*,*,#8029,.F.);
#11152=ORIENTED_EDGE('',*,*,#8026,.F.);
#11153=ORIENTED_EDGE('',*,*,#8022,.F.);
#11154=ORIENTED_EDGE('',*,*,#8021,.F.);
#11155=ORIENTED_EDGE('',*,*,#8018,.F.);
#11156=ORIENTED_EDGE('',*,*,#8014,.F.);
#11157=ORIENTED_EDGE('',*,*,#8013,.F.);
#11158=ORIENTED_EDGE('',*,*,#8010,.F.);
#11159=ORIENTED_EDGE('',*,*,#8006,.F.);
#11160=ORIENTED_EDGE('',*,*,#8005,.F.);
#11161=ORIENTED_EDGE('',*,*,#8002,.F.);
#11162=ORIENTED_EDGE('',*,*,#7998,.F.);
#11163=ORIENTED_EDGE('',*,*,#7997,.F.);
#11164=ORIENTED_EDGE('',*,*,#7994,.F.);
#11165=ORIENTED_EDGE('',*,*,#7990,.F.);
#11166=ORIENTED_EDGE('',*,*,#7989,.F.);
#11167=ORIENTED_EDGE('',*,*,#7986,.F.);
#11168=ORIENTED_EDGE('',*,*,#7982,.F.);
#11169=ORIENTED_EDGE('',*,*,#7981,.F.);
#11170=ORIENTED_EDGE('',*,*,#7978,.F.);
#11171=ORIENTED_EDGE('',*,*,#7974,.F.);
#11172=ORIENTED_EDGE('',*,*,#7973,.F.);
#11173=ORIENTED_EDGE('',*,*,#7970,.F.);
#11174=ORIENTED_EDGE('',*,*,#7966,.F.);
#11175=ORIENTED_EDGE('',*,*,#7965,.F.);
#11176=ORIENTED_EDGE('',*,*,#7961,.F.);
#11177=ORIENTED_EDGE('',*,*,#8139,.F.);
#11178=ORIENTED_EDGE('',*,*,#8141,.F.);
#11179=ORIENTED_EDGE('',*,*,#8068,.F.);
#11180=ORIENTED_EDGE('',*,*,#8127,.F.);
#11181=ORIENTED_EDGE('',*,*,#8126,.F.);
#11182=ORIENTED_EDGE('',*,*,#8125,.F.);
#11183=ORIENTED_EDGE('',*,*,#8124,.F.);
#11184=ORIENTED_EDGE('',*,*,#8123,.F.);
#11185=ORIENTED_EDGE('',*,*,#8122,.F.);
#11186=ORIENTED_EDGE('',*,*,#8121,.F.);
#11187=ORIENTED_EDGE('',*,*,#8120,.F.);
#11188=ORIENTED_EDGE('',*,*,#8119,.F.);
#11189=ORIENTED_EDGE('',*,*,#8118,.F.);
#11190=ORIENTED_EDGE('',*,*,#8117,.F.);
#11191=ORIENTED_EDGE('',*,*,#8116,.F.);
#11192=ORIENTED_EDGE('',*,*,#8115,.F.);
#11193=ORIENTED_EDGE('',*,*,#8114,.F.);
#11194=ORIENTED_EDGE('',*,*,#8113,.F.);
#11195=ORIENTED_EDGE('',*,*,#8112,.F.);
#11196=ORIENTED_EDGE('',*,*,#8111,.F.);
#11197=ORIENTED_EDGE('',*,*,#8110,.F.);
#11198=ORIENTED_EDGE('',*,*,#8109,.F.);
#11199=ORIENTED_EDGE('',*,*,#8108,.F.);
#11200=ORIENTED_EDGE('',*,*,#8107,.F.);
#11201=ORIENTED_EDGE('',*,*,#8106,.F.);
#11202=ORIENTED_EDGE('',*,*,#8105,.F.);
#11203=ORIENTED_EDGE('',*,*,#8104,.F.);
#11204=ORIENTED_EDGE('',*,*,#8103,.F.);
#11205=ORIENTED_EDGE('',*,*,#8102,.F.);
#11206=ORIENTED_EDGE('',*,*,#8101,.F.);
#11207=ORIENTED_EDGE('',*,*,#8142,.T.);
#11208=ORIENTED_EDGE('',*,*,#8143,.T.);
#11209=ORIENTED_EDGE('',*,*,#8140,.T.);
#11210=ORIENTED_EDGE('',*,*,#8069,.T.);
#11211=ORIENTED_EDGE('',*,*,#8141,.T.);
#11212=ORIENTED_EDGE('',*,*,#8138,.T.);
#11213=ORIENTED_EDGE('',*,*,#8143,.F.);
#11214=ORIENTED_EDGE('',*,*,#8144,.T.);
#11215=ORIENTED_EDGE('',*,*,#8142,.F.);
#11216=ORIENTED_EDGE('',*,*,#8100,.T.);
#11217=ORIENTED_EDGE('',*,*,#8145,.T.);
#11218=ORIENTED_EDGE('',*,*,#8146,.T.);
#11219=ORIENTED_EDGE('',*,*,#8145,.F.);
#11220=ORIENTED_EDGE('',*,*,#8099,.T.);
#11221=ORIENTED_EDGE('',*,*,#8136,.T.);
#11222=ORIENTED_EDGE('',*,*,#8133,.T.);
#11223=ORIENTED_EDGE('',*,*,#8146,.F.);
#11224=ORIENTED_EDGE('',*,*,#8147,.F.);
#11225=ORIENTED_EDGE('',*,*,#8148,.T.);
#11226=ORIENTED_EDGE('',*,*,#8149,.F.);
#11227=ORIENTED_EDGE('',*,*,#8150,.F.);
#11228=ORIENTED_EDGE('',*,*,#8151,.F.);
#11229=ORIENTED_EDGE('',*,*,#8149,.T.);
#11230=ORIENTED_EDGE('',*,*,#8152,.T.);
#11231=ORIENTED_EDGE('',*,*,#8153,.F.);
#11232=ORIENTED_EDGE('',*,*,#8154,.F.);
#11233=ORIENTED_EDGE('',*,*,#8152,.F.);
#11234=ORIENTED_EDGE('',*,*,#8148,.F.);
#11235=ORIENTED_EDGE('',*,*,#8155,.T.);
#11236=ORIENTED_EDGE('',*,*,#8156,.T.);
#11237=ORIENTED_EDGE('',*,*,#8157,.T.);
#11238=ORIENTED_EDGE('',*,*,#8158,.T.);
#11239=ORIENTED_EDGE('',*,*,#8159,.T.);
#11240=ORIENTED_EDGE('',*,*,#8160,.T.);
#11241=ORIENTED_EDGE('',*,*,#8161,.T.);
#11242=ORIENTED_EDGE('',*,*,#8162,.T.);
#11243=ORIENTED_EDGE('',*,*,#8163,.T.);
#11244=ORIENTED_EDGE('',*,*,#8164,.T.);
#11245=ORIENTED_EDGE('',*,*,#8165,.T.);
#11246=ORIENTED_EDGE('',*,*,#8166,.T.);
#11247=ORIENTED_EDGE('',*,*,#8167,.T.);
#11248=ORIENTED_EDGE('',*,*,#8168,.T.);
#11249=ORIENTED_EDGE('',*,*,#8169,.T.);
#11250=ORIENTED_EDGE('',*,*,#8170,.T.);
#11251=ORIENTED_EDGE('',*,*,#8171,.T.);
#11252=ORIENTED_EDGE('',*,*,#8172,.T.);
#11253=ORIENTED_EDGE('',*,*,#8173,.T.);
#11254=ORIENTED_EDGE('',*,*,#8174,.T.);
#11255=ORIENTED_EDGE('',*,*,#8175,.T.);
#11256=ORIENTED_EDGE('',*,*,#8176,.T.);
#11257=ORIENTED_EDGE('',*,*,#8177,.T.);
#11258=ORIENTED_EDGE('',*,*,#8178,.T.);
#11259=ORIENTED_EDGE('',*,*,#8179,.T.);
#11260=ORIENTED_EDGE('',*,*,#8180,.T.);
#11261=ORIENTED_EDGE('',*,*,#8181,.T.);
#11262=ORIENTED_EDGE('',*,*,#8182,.T.);
#11263=ORIENTED_EDGE('',*,*,#8183,.T.);
#11264=ORIENTED_EDGE('',*,*,#8184,.T.);
#11265=ORIENTED_EDGE('',*,*,#8185,.T.);
#11266=ORIENTED_EDGE('',*,*,#8186,.T.);
#11267=ORIENTED_EDGE('',*,*,#8187,.T.);
#11268=ORIENTED_EDGE('',*,*,#8188,.T.);
#11269=ORIENTED_EDGE('',*,*,#8189,.T.);
#11270=ORIENTED_EDGE('',*,*,#8190,.T.);
#11271=ORIENTED_EDGE('',*,*,#8191,.T.);
#11272=ORIENTED_EDGE('',*,*,#8192,.T.);
#11273=ORIENTED_EDGE('',*,*,#8193,.T.);
#11274=ORIENTED_EDGE('',*,*,#8194,.T.);
#11275=ORIENTED_EDGE('',*,*,#8195,.T.);
#11276=ORIENTED_EDGE('',*,*,#8196,.T.);
#11277=ORIENTED_EDGE('',*,*,#8197,.T.);
#11278=ORIENTED_EDGE('',*,*,#8198,.T.);
#11279=ORIENTED_EDGE('',*,*,#8199,.T.);
#11280=ORIENTED_EDGE('',*,*,#8200,.T.);
#11281=ORIENTED_EDGE('',*,*,#8201,.T.);
#11282=ORIENTED_EDGE('',*,*,#8202,.T.);
#11283=ORIENTED_EDGE('',*,*,#8203,.T.);
#11284=ORIENTED_EDGE('',*,*,#8204,.T.);
#11285=ORIENTED_EDGE('',*,*,#8205,.T.);
#11286=ORIENTED_EDGE('',*,*,#8206,.T.);
#11287=ORIENTED_EDGE('',*,*,#8207,.T.);
#11288=ORIENTED_EDGE('',*,*,#8208,.T.);
#11289=ORIENTED_EDGE('',*,*,#8209,.T.);
#11290=ORIENTED_EDGE('',*,*,#8210,.T.);
#11291=ORIENTED_EDGE('',*,*,#8150,.T.);
#11292=ORIENTED_EDGE('',*,*,#8151,.T.);
#11293=ORIENTED_EDGE('',*,*,#8211,.T.);
#11294=ORIENTED_EDGE('',*,*,#8212,.T.);
#11295=ORIENTED_EDGE('',*,*,#8213,.T.);
#11296=ORIENTED_EDGE('',*,*,#8214,.T.);
#11297=ORIENTED_EDGE('',*,*,#8215,.T.);
#11298=ORIENTED_EDGE('',*,*,#8216,.T.);
#11299=ORIENTED_EDGE('',*,*,#8217,.T.);
#11300=ORIENTED_EDGE('',*,*,#8218,.T.);
#11301=ORIENTED_EDGE('',*,*,#8219,.T.);
#11302=ORIENTED_EDGE('',*,*,#8220,.T.);
#11303=ORIENTED_EDGE('',*,*,#8221,.T.);
#11304=ORIENTED_EDGE('',*,*,#8222,.T.);
#11305=ORIENTED_EDGE('',*,*,#8223,.T.);
#11306=ORIENTED_EDGE('',*,*,#8224,.T.);
#11307=ORIENTED_EDGE('',*,*,#8225,.T.);
#11308=ORIENTED_EDGE('',*,*,#8226,.T.);
#11309=ORIENTED_EDGE('',*,*,#8227,.T.);
#11310=ORIENTED_EDGE('',*,*,#8228,.T.);
#11311=ORIENTED_EDGE('',*,*,#8229,.T.);
#11312=ORIENTED_EDGE('',*,*,#8230,.T.);
#11313=ORIENTED_EDGE('',*,*,#8231,.T.);
#11314=ORIENTED_EDGE('',*,*,#8232,.T.);
#11315=ORIENTED_EDGE('',*,*,#8233,.T.);
#11316=ORIENTED_EDGE('',*,*,#8234,.T.);
#11317=ORIENTED_EDGE('',*,*,#8235,.T.);
#11318=ORIENTED_EDGE('',*,*,#8236,.T.);
#11319=ORIENTED_EDGE('',*,*,#8237,.T.);
#11320=ORIENTED_EDGE('',*,*,#8238,.T.);
#11321=ORIENTED_EDGE('',*,*,#8239,.T.);
#11322=ORIENTED_EDGE('',*,*,#8240,.T.);
#11323=ORIENTED_EDGE('',*,*,#8241,.T.);
#11324=ORIENTED_EDGE('',*,*,#8242,.T.);
#11325=ORIENTED_EDGE('',*,*,#8243,.T.);
#11326=ORIENTED_EDGE('',*,*,#8244,.T.);
#11327=ORIENTED_EDGE('',*,*,#8245,.T.);
#11328=ORIENTED_EDGE('',*,*,#8246,.T.);
#11329=ORIENTED_EDGE('',*,*,#8247,.T.);
#11330=ORIENTED_EDGE('',*,*,#8248,.T.);
#11331=ORIENTED_EDGE('',*,*,#8249,.T.);
#11332=ORIENTED_EDGE('',*,*,#8250,.T.);
#11333=ORIENTED_EDGE('',*,*,#8251,.T.);
#11334=ORIENTED_EDGE('',*,*,#8252,.T.);
#11335=ORIENTED_EDGE('',*,*,#8253,.T.);
#11336=ORIENTED_EDGE('',*,*,#8254,.T.);
#11337=ORIENTED_EDGE('',*,*,#8255,.T.);
#11338=ORIENTED_EDGE('',*,*,#8256,.T.);
#11339=ORIENTED_EDGE('',*,*,#8257,.T.);
#11340=ORIENTED_EDGE('',*,*,#8258,.T.);
#11341=ORIENTED_EDGE('',*,*,#8259,.T.);
#11342=ORIENTED_EDGE('',*,*,#8260,.T.);
#11343=ORIENTED_EDGE('',*,*,#8261,.T.);
#11344=ORIENTED_EDGE('',*,*,#8262,.T.);
#11345=ORIENTED_EDGE('',*,*,#8261,.F.);
#11346=ORIENTED_EDGE('',*,*,#8263,.F.);
#11347=ORIENTED_EDGE('',*,*,#8264,.F.);
#11348=ORIENTED_EDGE('',*,*,#8265,.F.);
#11349=ORIENTED_EDGE('',*,*,#8266,.F.);
#11350=ORIENTED_EDGE('',*,*,#8265,.T.);
#11351=ORIENTED_EDGE('',*,*,#8267,.F.);
#11352=ORIENTED_EDGE('',*,*,#8212,.F.);
#11353=ORIENTED_EDGE('',*,*,#8268,.F.);
#11354=ORIENTED_EDGE('',*,*,#8213,.F.);
#11355=ORIENTED_EDGE('',*,*,#8267,.T.);
#11356=ORIENTED_EDGE('',*,*,#8264,.T.);
#11357=ORIENTED_EDGE('',*,*,#8269,.T.);
#11358=ORIENTED_EDGE('',*,*,#8270,.T.);
#11359=ORIENTED_EDGE('',*,*,#8144,.F.);
#11360=ORIENTED_EDGE('',*,*,#8270,.F.);
#11361=ORIENTED_EDGE('',*,*,#8271,.T.);
#11362=ORIENTED_EDGE('',*,*,#8272,.T.);
#11363=ORIENTED_EDGE('',*,*,#8259,.F.);
#11364=ORIENTED_EDGE('',*,*,#8273,.T.);
#11365=ORIENTED_EDGE('',*,*,#8274,.T.);
#11366=ORIENTED_EDGE('',*,*,#8275,.T.);
#11367=ORIENTED_EDGE('',*,*,#8256,.F.);
#11368=ORIENTED_EDGE('',*,*,#8276,.T.);
#11369=ORIENTED_EDGE('',*,*,#8277,.T.);
#11370=ORIENTED_EDGE('',*,*,#8278,.T.);
#11371=ORIENTED_EDGE('',*,*,#8253,.F.);
#11372=ORIENTED_EDGE('',*,*,#8279,.T.);
#11373=ORIENTED_EDGE('',*,*,#8280,.T.);
#11374=ORIENTED_EDGE('',*,*,#8281,.T.);
#11375=ORIENTED_EDGE('',*,*,#8250,.F.);
#11376=ORIENTED_EDGE('',*,*,#8282,.T.);
#11377=ORIENTED_EDGE('',*,*,#8283,.T.);
#11378=ORIENTED_EDGE('',*,*,#8284,.T.);
#11379=ORIENTED_EDGE('',*,*,#8247,.F.);
#11380=ORIENTED_EDGE('',*,*,#8285,.T.);
#11381=ORIENTED_EDGE('',*,*,#8286,.T.);
#11382=ORIENTED_EDGE('',*,*,#8287,.T.);
#11383=ORIENTED_EDGE('',*,*,#8244,.F.);
#11384=ORIENTED_EDGE('',*,*,#8288,.T.);
#11385=ORIENTED_EDGE('',*,*,#8289,.T.);
#11386=ORIENTED_EDGE('',*,*,#8290,.T.);
#11387=ORIENTED_EDGE('',*,*,#8241,.F.);
#11388=ORIENTED_EDGE('',*,*,#8291,.T.);
#11389=ORIENTED_EDGE('',*,*,#8292,.T.);
#11390=ORIENTED_EDGE('',*,*,#8293,.T.);
#11391=ORIENTED_EDGE('',*,*,#8238,.F.);
#11392=ORIENTED_EDGE('',*,*,#8294,.T.);
#11393=ORIENTED_EDGE('',*,*,#8295,.T.);
#11394=ORIENTED_EDGE('',*,*,#8296,.T.);
#11395=ORIENTED_EDGE('',*,*,#8235,.F.);
#11396=ORIENTED_EDGE('',*,*,#8297,.T.);
#11397=ORIENTED_EDGE('',*,*,#8298,.T.);
#11398=ORIENTED_EDGE('',*,*,#8299,.T.);
#11399=ORIENTED_EDGE('',*,*,#8232,.F.);
#11400=ORIENTED_EDGE('',*,*,#8300,.T.);
#11401=ORIENTED_EDGE('',*,*,#8301,.T.);
#11402=ORIENTED_EDGE('',*,*,#8302,.T.);
#11403=ORIENTED_EDGE('',*,*,#8229,.F.);
#11404=ORIENTED_EDGE('',*,*,#8303,.T.);
#11405=ORIENTED_EDGE('',*,*,#8304,.T.);
#11406=ORIENTED_EDGE('',*,*,#8305,.T.);
#11407=ORIENTED_EDGE('',*,*,#8226,.F.);
#11408=ORIENTED_EDGE('',*,*,#8306,.T.);
#11409=ORIENTED_EDGE('',*,*,#8307,.T.);
#11410=ORIENTED_EDGE('',*,*,#8308,.T.);
#11411=ORIENTED_EDGE('',*,*,#8223,.F.);
#11412=ORIENTED_EDGE('',*,*,#8309,.T.);
#11413=ORIENTED_EDGE('',*,*,#8310,.T.);
#11414=ORIENTED_EDGE('',*,*,#8311,.T.);
#11415=ORIENTED_EDGE('',*,*,#8220,.F.);
#11416=ORIENTED_EDGE('',*,*,#8312,.T.);
#11417=ORIENTED_EDGE('',*,*,#8313,.T.);
#11418=ORIENTED_EDGE('',*,*,#8314,.T.);
#11419=ORIENTED_EDGE('',*,*,#8217,.F.);
#11420=ORIENTED_EDGE('',*,*,#8315,.T.);
#11421=ORIENTED_EDGE('',*,*,#8316,.T.);
#11422=ORIENTED_EDGE('',*,*,#8317,.T.);
#11423=ORIENTED_EDGE('',*,*,#8214,.F.);
#11424=ORIENTED_EDGE('',*,*,#8268,.T.);
#11425=ORIENTED_EDGE('',*,*,#8263,.T.);
#11426=ORIENTED_EDGE('',*,*,#8266,.T.);
#11427=ORIENTED_EDGE('',*,*,#8211,.F.);
#11428=ORIENTED_EDGE('',*,*,#8153,.T.);
#11429=ORIENTED_EDGE('',*,*,#8154,.T.);
#11430=ORIENTED_EDGE('',*,*,#8147,.T.);
#11431=ORIENTED_EDGE('',*,*,#8210,.F.);
#11432=ORIENTED_EDGE('',*,*,#8318,.T.);
#11433=ORIENTED_EDGE('',*,*,#8319,.T.);
#11434=ORIENTED_EDGE('',*,*,#8320,.T.);
#11435=ORIENTED_EDGE('',*,*,#8207,.F.);
#11436=ORIENTED_EDGE('',*,*,#8321,.T.);
#11437=ORIENTED_EDGE('',*,*,#8322,.T.);
#11438=ORIENTED_EDGE('',*,*,#8323,.T.);
#11439=ORIENTED_EDGE('',*,*,#8204,.F.);
#11440=ORIENTED_EDGE('',*,*,#8324,.T.);
#11441=ORIENTED_EDGE('',*,*,#8325,.T.);
#11442=ORIENTED_EDGE('',*,*,#8326,.T.);
#11443=ORIENTED_EDGE('',*,*,#8201,.F.);
#11444=ORIENTED_EDGE('',*,*,#8327,.T.);
#11445=ORIENTED_EDGE('',*,*,#8328,.T.);
#11446=ORIENTED_EDGE('',*,*,#8329,.T.);
#11447=ORIENTED_EDGE('',*,*,#8198,.F.);
#11448=ORIENTED_EDGE('',*,*,#8330,.T.);
#11449=ORIENTED_EDGE('',*,*,#8331,.T.);
#11450=ORIENTED_EDGE('',*,*,#8332,.T.);
#11451=ORIENTED_EDGE('',*,*,#8195,.F.);
#11452=ORIENTED_EDGE('',*,*,#8333,.T.);
#11453=ORIENTED_EDGE('',*,*,#8334,.T.);
#11454=ORIENTED_EDGE('',*,*,#8335,.T.);
#11455=ORIENTED_EDGE('',*,*,#8192,.F.);
#11456=ORIENTED_EDGE('',*,*,#8336,.T.);
#11457=ORIENTED_EDGE('',*,*,#8337,.T.);
#11458=ORIENTED_EDGE('',*,*,#8338,.T.);
#11459=ORIENTED_EDGE('',*,*,#8189,.F.);
#11460=ORIENTED_EDGE('',*,*,#8339,.T.);
#11461=ORIENTED_EDGE('',*,*,#8340,.T.);
#11462=ORIENTED_EDGE('',*,*,#8341,.T.);
#11463=ORIENTED_EDGE('',*,*,#8186,.F.);
#11464=ORIENTED_EDGE('',*,*,#8342,.T.);
#11465=ORIENTED_EDGE('',*,*,#8343,.T.);
#11466=ORIENTED_EDGE('',*,*,#8344,.T.);
#11467=ORIENTED_EDGE('',*,*,#8183,.F.);
#11468=ORIENTED_EDGE('',*,*,#8345,.T.);
#11469=ORIENTED_EDGE('',*,*,#8346,.T.);
#11470=ORIENTED_EDGE('',*,*,#8347,.T.);
#11471=ORIENTED_EDGE('',*,*,#8180,.F.);
#11472=ORIENTED_EDGE('',*,*,#8348,.T.);
#11473=ORIENTED_EDGE('',*,*,#8349,.T.);
#11474=ORIENTED_EDGE('',*,*,#8350,.T.);
#11475=ORIENTED_EDGE('',*,*,#8177,.F.);
#11476=ORIENTED_EDGE('',*,*,#8351,.T.);
#11477=ORIENTED_EDGE('',*,*,#8352,.T.);
#11478=ORIENTED_EDGE('',*,*,#8353,.T.);
#11479=ORIENTED_EDGE('',*,*,#8174,.F.);
#11480=ORIENTED_EDGE('',*,*,#8354,.T.);
#11481=ORIENTED_EDGE('',*,*,#8355,.T.);
#11482=ORIENTED_EDGE('',*,*,#8356,.T.);
#11483=ORIENTED_EDGE('',*,*,#8171,.F.);
#11484=ORIENTED_EDGE('',*,*,#8357,.T.);
#11485=ORIENTED_EDGE('',*,*,#8358,.T.);
#11486=ORIENTED_EDGE('',*,*,#8359,.T.);
#11487=ORIENTED_EDGE('',*,*,#8168,.F.);
#11488=ORIENTED_EDGE('',*,*,#8360,.T.);
#11489=ORIENTED_EDGE('',*,*,#8361,.T.);
#11490=ORIENTED_EDGE('',*,*,#8362,.T.);
#11491=ORIENTED_EDGE('',*,*,#8165,.F.);
#11492=ORIENTED_EDGE('',*,*,#8363,.T.);
#11493=ORIENTED_EDGE('',*,*,#8364,.T.);
#11494=ORIENTED_EDGE('',*,*,#8365,.T.);
#11495=ORIENTED_EDGE('',*,*,#8162,.F.);
#11496=ORIENTED_EDGE('',*,*,#8366,.T.);
#11497=ORIENTED_EDGE('',*,*,#8367,.T.);
#11498=ORIENTED_EDGE('',*,*,#8368,.T.);
#11499=ORIENTED_EDGE('',*,*,#8159,.F.);
#11500=ORIENTED_EDGE('',*,*,#8369,.T.);
#11501=ORIENTED_EDGE('',*,*,#8370,.T.);
#11502=ORIENTED_EDGE('',*,*,#8371,.T.);
#11503=ORIENTED_EDGE('',*,*,#8156,.F.);
#11504=ORIENTED_EDGE('',*,*,#8372,.T.);
#11505=ORIENTED_EDGE('',*,*,#8317,.F.);
#11506=ORIENTED_EDGE('',*,*,#8373,.T.);
#11507=ORIENTED_EDGE('',*,*,#8374,.F.);
#11508=ORIENTED_EDGE('',*,*,#8215,.F.);
#11509=ORIENTED_EDGE('',*,*,#8216,.F.);
#11510=ORIENTED_EDGE('',*,*,#8374,.T.);
#11511=ORIENTED_EDGE('',*,*,#8375,.T.);
#11512=ORIENTED_EDGE('',*,*,#8315,.F.);
#11513=ORIENTED_EDGE('',*,*,#8316,.F.);
#11514=ORIENTED_EDGE('',*,*,#8375,.F.);
#11515=ORIENTED_EDGE('',*,*,#8373,.F.);
#11516=ORIENTED_EDGE('',*,*,#8313,.F.);
#11517=ORIENTED_EDGE('',*,*,#8376,.F.);
#11518=ORIENTED_EDGE('',*,*,#8377,.F.);
#11519=ORIENTED_EDGE('',*,*,#8314,.F.);
#11520=ORIENTED_EDGE('',*,*,#8377,.T.);
#11521=ORIENTED_EDGE('',*,*,#8378,.F.);
#11522=ORIENTED_EDGE('',*,*,#8218,.F.);
#11523=ORIENTED_EDGE('',*,*,#8312,.F.);
#11524=ORIENTED_EDGE('',*,*,#8219,.F.);
#11525=ORIENTED_EDGE('',*,*,#8378,.T.);
#11526=ORIENTED_EDGE('',*,*,#8376,.T.);
#11527=ORIENTED_EDGE('',*,*,#8311,.F.);
#11528=ORIENTED_EDGE('',*,*,#8379,.T.);
#11529=ORIENTED_EDGE('',*,*,#8380,.F.);
#11530=ORIENTED_EDGE('',*,*,#8221,.F.);
#11531=ORIENTED_EDGE('',*,*,#8222,.F.);
#11532=ORIENTED_EDGE('',*,*,#8380,.T.);
#11533=ORIENTED_EDGE('',*,*,#8381,.T.);
#11534=ORIENTED_EDGE('',*,*,#8309,.F.);
#11535=ORIENTED_EDGE('',*,*,#8310,.F.);
#11536=ORIENTED_EDGE('',*,*,#8381,.F.);
#11537=ORIENTED_EDGE('',*,*,#8379,.F.);
#11538=ORIENTED_EDGE('',*,*,#8307,.F.);
#11539=ORIENTED_EDGE('',*,*,#8382,.F.);
#11540=ORIENTED_EDGE('',*,*,#8383,.F.);
#11541=ORIENTED_EDGE('',*,*,#8308,.F.);
#11542=ORIENTED_EDGE('',*,*,#8383,.T.);
#11543=ORIENTED_EDGE('',*,*,#8384,.F.);
#11544=ORIENTED_EDGE('',*,*,#8224,.F.);
#11545=ORIENTED_EDGE('',*,*,#8306,.F.);
#11546=ORIENTED_EDGE('',*,*,#8225,.F.);
#11547=ORIENTED_EDGE('',*,*,#8384,.T.);
#11548=ORIENTED_EDGE('',*,*,#8382,.T.);
#11549=ORIENTED_EDGE('',*,*,#8305,.F.);
#11550=ORIENTED_EDGE('',*,*,#8385,.T.);
#11551=ORIENTED_EDGE('',*,*,#8386,.F.);
#11552=ORIENTED_EDGE('',*,*,#8227,.F.);
#11553=ORIENTED_EDGE('',*,*,#8228,.F.);
#11554=ORIENTED_EDGE('',*,*,#8386,.T.);
#11555=ORIENTED_EDGE('',*,*,#8387,.T.);
#11556=ORIENTED_EDGE('',*,*,#8303,.F.);
#11557=ORIENTED_EDGE('',*,*,#8304,.F.);
#11558=ORIENTED_EDGE('',*,*,#8387,.F.);
#11559=ORIENTED_EDGE('',*,*,#8385,.F.);
#11560=ORIENTED_EDGE('',*,*,#8301,.F.);
#11561=ORIENTED_EDGE('',*,*,#8388,.F.);
#11562=ORIENTED_EDGE('',*,*,#8389,.F.);
#11563=ORIENTED_EDGE('',*,*,#8302,.F.);
#11564=ORIENTED_EDGE('',*,*,#8389,.T.);
#11565=ORIENTED_EDGE('',*,*,#8390,.F.);
#11566=ORIENTED_EDGE('',*,*,#8230,.F.);
#11567=ORIENTED_EDGE('',*,*,#8300,.F.);
#11568=ORIENTED_EDGE('',*,*,#8231,.F.);
#11569=ORIENTED_EDGE('',*,*,#8390,.T.);
#11570=ORIENTED_EDGE('',*,*,#8388,.T.);
#11571=ORIENTED_EDGE('',*,*,#8299,.F.);
#11572=ORIENTED_EDGE('',*,*,#8391,.T.);
#11573=ORIENTED_EDGE('',*,*,#8392,.F.);
#11574=ORIENTED_EDGE('',*,*,#8233,.F.);
#11575=ORIENTED_EDGE('',*,*,#8234,.F.);
#11576=ORIENTED_EDGE('',*,*,#8392,.T.);
#11577=ORIENTED_EDGE('',*,*,#8393,.T.);
#11578=ORIENTED_EDGE('',*,*,#8297,.F.);
#11579=ORIENTED_EDGE('',*,*,#8298,.F.);
#11580=ORIENTED_EDGE('',*,*,#8393,.F.);
#11581=ORIENTED_EDGE('',*,*,#8391,.F.);
#11582=ORIENTED_EDGE('',*,*,#8295,.F.);
#11583=ORIENTED_EDGE('',*,*,#8394,.F.);
#11584=ORIENTED_EDGE('',*,*,#8395,.F.);
#11585=ORIENTED_EDGE('',*,*,#8296,.F.);
#11586=ORIENTED_EDGE('',*,*,#8395,.T.);
#11587=ORIENTED_EDGE('',*,*,#8396,.F.);
#11588=ORIENTED_EDGE('',*,*,#8236,.F.);
#11589=ORIENTED_EDGE('',*,*,#8294,.F.);
#11590=ORIENTED_EDGE('',*,*,#8237,.F.);
#11591=ORIENTED_EDGE('',*,*,#8396,.T.);
#11592=ORIENTED_EDGE('',*,*,#8394,.T.);
#11593=ORIENTED_EDGE('',*,*,#8293,.F.);
#11594=ORIENTED_EDGE('',*,*,#8397,.T.);
#11595=ORIENTED_EDGE('',*,*,#8398,.F.);
#11596=ORIENTED_EDGE('',*,*,#8239,.F.);
#11597=ORIENTED_EDGE('',*,*,#8240,.F.);
#11598=ORIENTED_EDGE('',*,*,#8398,.T.);
#11599=ORIENTED_EDGE('',*,*,#8399,.T.);
#11600=ORIENTED_EDGE('',*,*,#8291,.F.);
#11601=ORIENTED_EDGE('',*,*,#8292,.F.);
#11602=ORIENTED_EDGE('',*,*,#8399,.F.);
#11603=ORIENTED_EDGE('',*,*,#8397,.F.);
#11604=ORIENTED_EDGE('',*,*,#8289,.F.);
#11605=ORIENTED_EDGE('',*,*,#8400,.F.);
#11606=ORIENTED_EDGE('',*,*,#8401,.F.);
#11607=ORIENTED_EDGE('',*,*,#8290,.F.);
#11608=ORIENTED_EDGE('',*,*,#8401,.T.);
#11609=ORIENTED_EDGE('',*,*,#8402,.F.);
#11610=ORIENTED_EDGE('',*,*,#8242,.F.);
#11611=ORIENTED_EDGE('',*,*,#8288,.F.);
#11612=ORIENTED_EDGE('',*,*,#8243,.F.);
#11613=ORIENTED_EDGE('',*,*,#8402,.T.);
#11614=ORIENTED_EDGE('',*,*,#8400,.T.);
#11615=ORIENTED_EDGE('',*,*,#8287,.F.);
#11616=ORIENTED_EDGE('',*,*,#8403,.T.);
#11617=ORIENTED_EDGE('',*,*,#8404,.F.);
#11618=ORIENTED_EDGE('',*,*,#8245,.F.);
#11619=ORIENTED_EDGE('',*,*,#8246,.F.);
#11620=ORIENTED_EDGE('',*,*,#8404,.T.);
#11621=ORIENTED_EDGE('',*,*,#8405,.T.);
#11622=ORIENTED_EDGE('',*,*,#8285,.F.);
#11623=ORIENTED_EDGE('',*,*,#8286,.F.);
#11624=ORIENTED_EDGE('',*,*,#8405,.F.);
#11625=ORIENTED_EDGE('',*,*,#8403,.F.);
#11626=ORIENTED_EDGE('',*,*,#8283,.F.);
#11627=ORIENTED_EDGE('',*,*,#8406,.F.);
#11628=ORIENTED_EDGE('',*,*,#8407,.F.);
#11629=ORIENTED_EDGE('',*,*,#8284,.F.);
#11630=ORIENTED_EDGE('',*,*,#8407,.T.);
#11631=ORIENTED_EDGE('',*,*,#8408,.F.);
#11632=ORIENTED_EDGE('',*,*,#8248,.F.);
#11633=ORIENTED_EDGE('',*,*,#8282,.F.);
#11634=ORIENTED_EDGE('',*,*,#8249,.F.);
#11635=ORIENTED_EDGE('',*,*,#8408,.T.);
#11636=ORIENTED_EDGE('',*,*,#8406,.T.);
#11637=ORIENTED_EDGE('',*,*,#8281,.F.);
#11638=ORIENTED_EDGE('',*,*,#8409,.T.);
#11639=ORIENTED_EDGE('',*,*,#8410,.F.);
#11640=ORIENTED_EDGE('',*,*,#8251,.F.);
#11641=ORIENTED_EDGE('',*,*,#8252,.F.);
#11642=ORIENTED_EDGE('',*,*,#8410,.T.);
#11643=ORIENTED_EDGE('',*,*,#8411,.T.);
#11644=ORIENTED_EDGE('',*,*,#8279,.F.);
#11645=ORIENTED_EDGE('',*,*,#8280,.F.);
#11646=ORIENTED_EDGE('',*,*,#8411,.F.);
#11647=ORIENTED_EDGE('',*,*,#8409,.F.);
#11648=ORIENTED_EDGE('',*,*,#8277,.F.);
#11649=ORIENTED_EDGE('',*,*,#8412,.F.);
#11650=ORIENTED_EDGE('',*,*,#8413,.F.);
#11651=ORIENTED_EDGE('',*,*,#8278,.F.);
#11652=ORIENTED_EDGE('',*,*,#8413,.T.);
#11653=ORIENTED_EDGE('',*,*,#8414,.F.);
#11654=ORIENTED_EDGE('',*,*,#8254,.F.);
#11655=ORIENTED_EDGE('',*,*,#8276,.F.);
#11656=ORIENTED_EDGE('',*,*,#8255,.F.);
#11657=ORIENTED_EDGE('',*,*,#8414,.T.);
#11658=ORIENTED_EDGE('',*,*,#8412,.T.);
#11659=ORIENTED_EDGE('',*,*,#8275,.F.);
#11660=ORIENTED_EDGE('',*,*,#8415,.T.);
#11661=ORIENTED_EDGE('',*,*,#8416,.F.);
#11662=ORIENTED_EDGE('',*,*,#8257,.F.);
#11663=ORIENTED_EDGE('',*,*,#8258,.F.);
#11664=ORIENTED_EDGE('',*,*,#8416,.T.);
#11665=ORIENTED_EDGE('',*,*,#8417,.T.);
#11666=ORIENTED_EDGE('',*,*,#8273,.F.);
#11667=ORIENTED_EDGE('',*,*,#8274,.F.);
#11668=ORIENTED_EDGE('',*,*,#8417,.F.);
#11669=ORIENTED_EDGE('',*,*,#8415,.F.);
#11670=ORIENTED_EDGE('',*,*,#8269,.F.);
#11671=ORIENTED_EDGE('',*,*,#8418,.F.);
#11672=ORIENTED_EDGE('',*,*,#8419,.F.);
#11673=ORIENTED_EDGE('',*,*,#8271,.F.);
#11674=ORIENTED_EDGE('',*,*,#8272,.F.);
#11675=ORIENTED_EDGE('',*,*,#8419,.T.);
#11676=ORIENTED_EDGE('',*,*,#8420,.F.);
#11677=ORIENTED_EDGE('',*,*,#8260,.F.);
#11678=ORIENTED_EDGE('',*,*,#8372,.F.);
#11679=ORIENTED_EDGE('',*,*,#8155,.F.);
#11680=ORIENTED_EDGE('',*,*,#8420,.T.);
#11681=ORIENTED_EDGE('',*,*,#8418,.T.);
#11682=ORIENTED_EDGE('',*,*,#8371,.F.);
#11683=ORIENTED_EDGE('',*,*,#8421,.T.);
#11684=ORIENTED_EDGE('',*,*,#8422,.F.);
#11685=ORIENTED_EDGE('',*,*,#8157,.F.);
#11686=ORIENTED_EDGE('',*,*,#8158,.F.);
#11687=ORIENTED_EDGE('',*,*,#8422,.T.);
#11688=ORIENTED_EDGE('',*,*,#8423,.T.);
#11689=ORIENTED_EDGE('',*,*,#8369,.F.);
#11690=ORIENTED_EDGE('',*,*,#8370,.F.);
#11691=ORIENTED_EDGE('',*,*,#8423,.F.);
#11692=ORIENTED_EDGE('',*,*,#8421,.F.);
#11693=ORIENTED_EDGE('',*,*,#8367,.F.);
#11694=ORIENTED_EDGE('',*,*,#8424,.F.);
#11695=ORIENTED_EDGE('',*,*,#8425,.F.);
#11696=ORIENTED_EDGE('',*,*,#8368,.F.);
#11697=ORIENTED_EDGE('',*,*,#8425,.T.);
#11698=ORIENTED_EDGE('',*,*,#8426,.F.);
#11699=ORIENTED_EDGE('',*,*,#8160,.F.);
#11700=ORIENTED_EDGE('',*,*,#8366,.F.);
#11701=ORIENTED_EDGE('',*,*,#8161,.F.);
#11702=ORIENTED_EDGE('',*,*,#8426,.T.);
#11703=ORIENTED_EDGE('',*,*,#8424,.T.);
#11704=ORIENTED_EDGE('',*,*,#8365,.F.);
#11705=ORIENTED_EDGE('',*,*,#8427,.T.);
#11706=ORIENTED_EDGE('',*,*,#8428,.F.);
#11707=ORIENTED_EDGE('',*,*,#8163,.F.);
#11708=ORIENTED_EDGE('',*,*,#8164,.F.);
#11709=ORIENTED_EDGE('',*,*,#8428,.T.);
#11710=ORIENTED_EDGE('',*,*,#8429,.T.);
#11711=ORIENTED_EDGE('',*,*,#8363,.F.);
#11712=ORIENTED_EDGE('',*,*,#8364,.F.);
#11713=ORIENTED_EDGE('',*,*,#8429,.F.);
#11714=ORIENTED_EDGE('',*,*,#8427,.F.);
#11715=ORIENTED_EDGE('',*,*,#8361,.F.);
#11716=ORIENTED_EDGE('',*,*,#8430,.F.);
#11717=ORIENTED_EDGE('',*,*,#8431,.F.);
#11718=ORIENTED_EDGE('',*,*,#8362,.F.);
#11719=ORIENTED_EDGE('',*,*,#8431,.T.);
#11720=ORIENTED_EDGE('',*,*,#8432,.F.);
#11721=ORIENTED_EDGE('',*,*,#8166,.F.);
#11722=ORIENTED_EDGE('',*,*,#8360,.F.);
#11723=ORIENTED_EDGE('',*,*,#8167,.F.);
#11724=ORIENTED_EDGE('',*,*,#8432,.T.);
#11725=ORIENTED_EDGE('',*,*,#8430,.T.);
#11726=ORIENTED_EDGE('',*,*,#8359,.F.);
#11727=ORIENTED_EDGE('',*,*,#8433,.T.);
#11728=ORIENTED_EDGE('',*,*,#8434,.F.);
#11729=ORIENTED_EDGE('',*,*,#8169,.F.);
#11730=ORIENTED_EDGE('',*,*,#8170,.F.);
#11731=ORIENTED_EDGE('',*,*,#8434,.T.);
#11732=ORIENTED_EDGE('',*,*,#8435,.T.);
#11733=ORIENTED_EDGE('',*,*,#8357,.F.);
#11734=ORIENTED_EDGE('',*,*,#8358,.F.);
#11735=ORIENTED_EDGE('',*,*,#8435,.F.);
#11736=ORIENTED_EDGE('',*,*,#8433,.F.);
#11737=ORIENTED_EDGE('',*,*,#8355,.F.);
#11738=ORIENTED_EDGE('',*,*,#8436,.F.);
#11739=ORIENTED_EDGE('',*,*,#8437,.F.);
#11740=ORIENTED_EDGE('',*,*,#8356,.F.);
#11741=ORIENTED_EDGE('',*,*,#8437,.T.);
#11742=ORIENTED_EDGE('',*,*,#8438,.F.);
#11743=ORIENTED_EDGE('',*,*,#8172,.F.);
#11744=ORIENTED_EDGE('',*,*,#8354,.F.);
#11745=ORIENTED_EDGE('',*,*,#8173,.F.);
#11746=ORIENTED_EDGE('',*,*,#8438,.T.);
#11747=ORIENTED_EDGE('',*,*,#8436,.T.);
#11748=ORIENTED_EDGE('',*,*,#8353,.F.);
#11749=ORIENTED_EDGE('',*,*,#8439,.T.);
#11750=ORIENTED_EDGE('',*,*,#8440,.F.);
#11751=ORIENTED_EDGE('',*,*,#8175,.F.);
#11752=ORIENTED_EDGE('',*,*,#8176,.F.);
#11753=ORIENTED_EDGE('',*,*,#8440,.T.);
#11754=ORIENTED_EDGE('',*,*,#8441,.T.);
#11755=ORIENTED_EDGE('',*,*,#8351,.F.);
#11756=ORIENTED_EDGE('',*,*,#8352,.F.);
#11757=ORIENTED_EDGE('',*,*,#8441,.F.);
#11758=ORIENTED_EDGE('',*,*,#8439,.F.);
#11759=ORIENTED_EDGE('',*,*,#8349,.F.);
#11760=ORIENTED_EDGE('',*,*,#8442,.F.);
#11761=ORIENTED_EDGE('',*,*,#8443,.F.);
#11762=ORIENTED_EDGE('',*,*,#8350,.F.);
#11763=ORIENTED_EDGE('',*,*,#8443,.T.);
#11764=ORIENTED_EDGE('',*,*,#8444,.F.);
#11765=ORIENTED_EDGE('',*,*,#8178,.F.);
#11766=ORIENTED_EDGE('',*,*,#8348,.F.);
#11767=ORIENTED_EDGE('',*,*,#8179,.F.);
#11768=ORIENTED_EDGE('',*,*,#8444,.T.);
#11769=ORIENTED_EDGE('',*,*,#8442,.T.);
#11770=ORIENTED_EDGE('',*,*,#8347,.F.);
#11771=ORIENTED_EDGE('',*,*,#8445,.T.);
#11772=ORIENTED_EDGE('',*,*,#8446,.F.);
#11773=ORIENTED_EDGE('',*,*,#8181,.F.);
#11774=ORIENTED_EDGE('',*,*,#8182,.F.);
#11775=ORIENTED_EDGE('',*,*,#8446,.T.);
#11776=ORIENTED_EDGE('',*,*,#8447,.T.);
#11777=ORIENTED_EDGE('',*,*,#8345,.F.);
#11778=ORIENTED_EDGE('',*,*,#8346,.F.);
#11779=ORIENTED_EDGE('',*,*,#8447,.F.);
#11780=ORIENTED_EDGE('',*,*,#8445,.F.);
#11781=ORIENTED_EDGE('',*,*,#8343,.F.);
#11782=ORIENTED_EDGE('',*,*,#8448,.F.);
#11783=ORIENTED_EDGE('',*,*,#8449,.F.);
#11784=ORIENTED_EDGE('',*,*,#8344,.F.);
#11785=ORIENTED_EDGE('',*,*,#8449,.T.);
#11786=ORIENTED_EDGE('',*,*,#8450,.F.);
#11787=ORIENTED_EDGE('',*,*,#8184,.F.);
#11788=ORIENTED_EDGE('',*,*,#8342,.F.);
#11789=ORIENTED_EDGE('',*,*,#8185,.F.);
#11790=ORIENTED_EDGE('',*,*,#8450,.T.);
#11791=ORIENTED_EDGE('',*,*,#8448,.T.);
#11792=ORIENTED_EDGE('',*,*,#8341,.F.);
#11793=ORIENTED_EDGE('',*,*,#8451,.T.);
#11794=ORIENTED_EDGE('',*,*,#8452,.F.);
#11795=ORIENTED_EDGE('',*,*,#8187,.F.);
#11796=ORIENTED_EDGE('',*,*,#8188,.F.);
#11797=ORIENTED_EDGE('',*,*,#8452,.T.);
#11798=ORIENTED_EDGE('',*,*,#8453,.T.);
#11799=ORIENTED_EDGE('',*,*,#8339,.F.);
#11800=ORIENTED_EDGE('',*,*,#8340,.F.);
#11801=ORIENTED_EDGE('',*,*,#8453,.F.);
#11802=ORIENTED_EDGE('',*,*,#8451,.F.);
#11803=ORIENTED_EDGE('',*,*,#8337,.F.);
#11804=ORIENTED_EDGE('',*,*,#8454,.F.);
#11805=ORIENTED_EDGE('',*,*,#8455,.F.);
#11806=ORIENTED_EDGE('',*,*,#8338,.F.);
#11807=ORIENTED_EDGE('',*,*,#8455,.T.);
#11808=ORIENTED_EDGE('',*,*,#8456,.F.);
#11809=ORIENTED_EDGE('',*,*,#8190,.F.);
#11810=ORIENTED_EDGE('',*,*,#8336,.F.);
#11811=ORIENTED_EDGE('',*,*,#8191,.F.);
#11812=ORIENTED_EDGE('',*,*,#8456,.T.);
#11813=ORIENTED_EDGE('',*,*,#8454,.T.);
#11814=ORIENTED_EDGE('',*,*,#8335,.F.);
#11815=ORIENTED_EDGE('',*,*,#8457,.T.);
#11816=ORIENTED_EDGE('',*,*,#8458,.F.);
#11817=ORIENTED_EDGE('',*,*,#8193,.F.);
#11818=ORIENTED_EDGE('',*,*,#8194,.F.);
#11819=ORIENTED_EDGE('',*,*,#8458,.T.);
#11820=ORIENTED_EDGE('',*,*,#8459,.T.);
#11821=ORIENTED_EDGE('',*,*,#8333,.F.);
#11822=ORIENTED_EDGE('',*,*,#8334,.F.);
#11823=ORIENTED_EDGE('',*,*,#8459,.F.);
#11824=ORIENTED_EDGE('',*,*,#8457,.F.);
#11825=ORIENTED_EDGE('',*,*,#8331,.F.);
#11826=ORIENTED_EDGE('',*,*,#8460,.F.);
#11827=ORIENTED_EDGE('',*,*,#8461,.F.);
#11828=ORIENTED_EDGE('',*,*,#8332,.F.);
#11829=ORIENTED_EDGE('',*,*,#8461,.T.);
#11830=ORIENTED_EDGE('',*,*,#8462,.F.);
#11831=ORIENTED_EDGE('',*,*,#8196,.F.);
#11832=ORIENTED_EDGE('',*,*,#8330,.F.);
#11833=ORIENTED_EDGE('',*,*,#8197,.F.);
#11834=ORIENTED_EDGE('',*,*,#8462,.T.);
#11835=ORIENTED_EDGE('',*,*,#8460,.T.);
#11836=ORIENTED_EDGE('',*,*,#8329,.F.);
#11837=ORIENTED_EDGE('',*,*,#8463,.T.);
#11838=ORIENTED_EDGE('',*,*,#8464,.F.);
#11839=ORIENTED_EDGE('',*,*,#8199,.F.);
#11840=ORIENTED_EDGE('',*,*,#8200,.F.);
#11841=ORIENTED_EDGE('',*,*,#8464,.T.);
#11842=ORIENTED_EDGE('',*,*,#8465,.T.);
#11843=ORIENTED_EDGE('',*,*,#8327,.F.);
#11844=ORIENTED_EDGE('',*,*,#8328,.F.);
#11845=ORIENTED_EDGE('',*,*,#8465,.F.);
#11846=ORIENTED_EDGE('',*,*,#8463,.F.);
#11847=ORIENTED_EDGE('',*,*,#8325,.F.);
#11848=ORIENTED_EDGE('',*,*,#8466,.F.);
#11849=ORIENTED_EDGE('',*,*,#8467,.F.);
#11850=ORIENTED_EDGE('',*,*,#8326,.F.);
#11851=ORIENTED_EDGE('',*,*,#8467,.T.);
#11852=ORIENTED_EDGE('',*,*,#8468,.F.);
#11853=ORIENTED_EDGE('',*,*,#8202,.F.);
#11854=ORIENTED_EDGE('',*,*,#8324,.F.);
#11855=ORIENTED_EDGE('',*,*,#8203,.F.);
#11856=ORIENTED_EDGE('',*,*,#8468,.T.);
#11857=ORIENTED_EDGE('',*,*,#8466,.T.);
#11858=ORIENTED_EDGE('',*,*,#8323,.F.);
#11859=ORIENTED_EDGE('',*,*,#8469,.T.);
#11860=ORIENTED_EDGE('',*,*,#8470,.F.);
#11861=ORIENTED_EDGE('',*,*,#8205,.F.);
#11862=ORIENTED_EDGE('',*,*,#8206,.F.);
#11863=ORIENTED_EDGE('',*,*,#8470,.T.);
#11864=ORIENTED_EDGE('',*,*,#8471,.T.);
#11865=ORIENTED_EDGE('',*,*,#8321,.F.);
#11866=ORIENTED_EDGE('',*,*,#8322,.F.);
#11867=ORIENTED_EDGE('',*,*,#8471,.F.);
#11868=ORIENTED_EDGE('',*,*,#8469,.F.);
#11869=ORIENTED_EDGE('',*,*,#8319,.F.);
#11870=ORIENTED_EDGE('',*,*,#8472,.F.);
#11871=ORIENTED_EDGE('',*,*,#8473,.F.);
#11872=ORIENTED_EDGE('',*,*,#8320,.F.);
#11873=ORIENTED_EDGE('',*,*,#8473,.T.);
#11874=ORIENTED_EDGE('',*,*,#8474,.F.);
#11875=ORIENTED_EDGE('',*,*,#8208,.F.);
#11876=ORIENTED_EDGE('',*,*,#8318,.F.);
#11877=ORIENTED_EDGE('',*,*,#8209,.F.);
#11878=ORIENTED_EDGE('',*,*,#8474,.T.);
#11879=ORIENTED_EDGE('',*,*,#8472,.T.);
#11880=ORIENTED_EDGE('',*,*,#8262,.F.);
#11881=ORIENTED_EDGE('',*,*,#8475,.T.);
#11882=ORIENTED_EDGE('',*,*,#8476,.T.);
#11883=ORIENTED_EDGE('',*,*,#8477,.T.);
#11884=ORIENTED_EDGE('',*,*,#8478,.T.);
#11885=ORIENTED_EDGE('',*,*,#8479,.T.);
#11886=ORIENTED_EDGE('',*,*,#8480,.T.);
#11887=ORIENTED_EDGE('',*,*,#8481,.F.);
#11888=ORIENTED_EDGE('',*,*,#8482,.F.);
#11889=ORIENTED_EDGE('',*,*,#8483,.F.);
#11890=ORIENTED_EDGE('',*,*,#8484,.F.);
#11891=ORIENTED_EDGE('',*,*,#8485,.F.);
#11892=ORIENTED_EDGE('',*,*,#8486,.F.);
#11893=ORIENTED_EDGE('',*,*,#8487,.F.);
#11894=ORIENTED_EDGE('',*,*,#8488,.F.);
#11895=ORIENTED_EDGE('',*,*,#8489,.F.);
#11896=ORIENTED_EDGE('',*,*,#8490,.F.);
#11897=ORIENTED_EDGE('',*,*,#8491,.F.);
#11898=ORIENTED_EDGE('',*,*,#8492,.F.);
#11899=ORIENTED_EDGE('',*,*,#8493,.T.);
#11900=ORIENTED_EDGE('',*,*,#8486,.T.);
#11901=ORIENTED_EDGE('',*,*,#8484,.T.);
#11902=ORIENTED_EDGE('',*,*,#8482,.T.);
#11903=ORIENTED_EDGE('',*,*,#8492,.T.);
#11904=ORIENTED_EDGE('',*,*,#8490,.T.);
#11905=ORIENTED_EDGE('',*,*,#8488,.T.);
#11906=ORIENTED_EDGE('',*,*,#8493,.F.);
#11907=ORIENTED_EDGE('',*,*,#8475,.F.);
#11908=ORIENTED_EDGE('',*,*,#8494,.T.);
#11909=ORIENTED_EDGE('',*,*,#8481,.T.);
#11910=ORIENTED_EDGE('',*,*,#8495,.F.);
#11911=ORIENTED_EDGE('',*,*,#8480,.F.);
#11912=ORIENTED_EDGE('',*,*,#8496,.T.);
#11913=ORIENTED_EDGE('',*,*,#8491,.T.);
#11914=ORIENTED_EDGE('',*,*,#8494,.F.);
#11915=ORIENTED_EDGE('',*,*,#8479,.F.);
#11916=ORIENTED_EDGE('',*,*,#8497,.T.);
#11917=ORIENTED_EDGE('',*,*,#8489,.T.);
#11918=ORIENTED_EDGE('',*,*,#8496,.F.);
#11919=ORIENTED_EDGE('',*,*,#8478,.F.);
#11920=ORIENTED_EDGE('',*,*,#8498,.T.);
#11921=ORIENTED_EDGE('',*,*,#8487,.T.);
#11922=ORIENTED_EDGE('',*,*,#8497,.F.);
#11923=ORIENTED_EDGE('',*,*,#8477,.F.);
#11924=ORIENTED_EDGE('',*,*,#8499,.T.);
#11925=ORIENTED_EDGE('',*,*,#8485,.T.);
#11926=ORIENTED_EDGE('',*,*,#8498,.F.);
#11927=ORIENTED_EDGE('',*,*,#8476,.F.);
#11928=ORIENTED_EDGE('',*,*,#8495,.T.);
#11929=ORIENTED_EDGE('',*,*,#8483,.T.);
#11930=ORIENTED_EDGE('',*,*,#8499,.F.);
#11931=ORIENTED_EDGE('',*,*,#8500,.F.);
#11932=ORIENTED_EDGE('',*,*,#8501,.F.);
#11933=ORIENTED_EDGE('',*,*,#8502,.F.);
#11934=ORIENTED_EDGE('',*,*,#8503,.T.);
#11935=ORIENTED_EDGE('',*,*,#8504,.F.);
#11936=ORIENTED_EDGE('',*,*,#8505,.F.);
#11937=ORIENTED_EDGE('',*,*,#8506,.F.);
#11938=ORIENTED_EDGE('',*,*,#8500,.T.);
#11939=ORIENTED_EDGE('',*,*,#8507,.T.);
#11940=ORIENTED_EDGE('',*,*,#8508,.T.);
#11941=ORIENTED_EDGE('',*,*,#8509,.F.);
#11942=ORIENTED_EDGE('',*,*,#8510,.F.);
#11943=ORIENTED_EDGE('',*,*,#8504,.T.);
#11944=ORIENTED_EDGE('',*,*,#8511,.T.);
#11945=ORIENTED_EDGE('',*,*,#8512,.T.);
#11946=ORIENTED_EDGE('',*,*,#8513,.F.);
#11947=ORIENTED_EDGE('',*,*,#8514,.F.);
#11948=ORIENTED_EDGE('',*,*,#8515,.F.);
#11949=ORIENTED_EDGE('',*,*,#8509,.T.);
#11950=ORIENTED_EDGE('',*,*,#8516,.T.);
#11951=ORIENTED_EDGE('',*,*,#8517,.T.);
#11952=ORIENTED_EDGE('',*,*,#8518,.F.);
#11953=ORIENTED_EDGE('',*,*,#8519,.F.);
#11954=ORIENTED_EDGE('',*,*,#8520,.F.);
#11955=ORIENTED_EDGE('',*,*,#8513,.T.);
#11956=ORIENTED_EDGE('',*,*,#8521,.T.);
#11957=ORIENTED_EDGE('',*,*,#8522,.F.);
#11958=ORIENTED_EDGE('',*,*,#8523,.F.);
#11959=ORIENTED_EDGE('',*,*,#8518,.T.);
#11960=ORIENTED_EDGE('',*,*,#8524,.T.);
#11961=ORIENTED_EDGE('',*,*,#8525,.T.);
#11962=ORIENTED_EDGE('',*,*,#8526,.F.);
#11963=ORIENTED_EDGE('',*,*,#8527,.F.);
#11964=ORIENTED_EDGE('',*,*,#8528,.F.);
#11965=ORIENTED_EDGE('',*,*,#8522,.T.);
#11966=ORIENTED_EDGE('',*,*,#8529,.T.);
#11967=ORIENTED_EDGE('',*,*,#8530,.F.);
#11968=ORIENTED_EDGE('',*,*,#8531,.F.);
#11969=ORIENTED_EDGE('',*,*,#8526,.T.);
#11970=ORIENTED_EDGE('',*,*,#8532,.T.);
#11971=ORIENTED_EDGE('',*,*,#8533,.T.);
#11972=ORIENTED_EDGE('',*,*,#8534,.F.);
#11973=ORIENTED_EDGE('',*,*,#8535,.F.);
#11974=ORIENTED_EDGE('',*,*,#8536,.F.);
#11975=ORIENTED_EDGE('',*,*,#8530,.T.);
#11976=ORIENTED_EDGE('',*,*,#8537,.T.);
#11977=ORIENTED_EDGE('',*,*,#8538,.F.);
#11978=ORIENTED_EDGE('',*,*,#8539,.F.);
#11979=ORIENTED_EDGE('',*,*,#8534,.T.);
#11980=ORIENTED_EDGE('',*,*,#8540,.T.);
#11981=ORIENTED_EDGE('',*,*,#8541,.T.);
#11982=ORIENTED_EDGE('',*,*,#8542,.F.);
#11983=ORIENTED_EDGE('',*,*,#8543,.F.);
#11984=ORIENTED_EDGE('',*,*,#8544,.F.);
#11985=ORIENTED_EDGE('',*,*,#8538,.T.);
#11986=ORIENTED_EDGE('',*,*,#8545,.T.);
#11987=ORIENTED_EDGE('',*,*,#8546,.T.);
#11988=ORIENTED_EDGE('',*,*,#8547,.F.);
#11989=ORIENTED_EDGE('',*,*,#8548,.F.);
#11990=ORIENTED_EDGE('',*,*,#8549,.F.);
#11991=ORIENTED_EDGE('',*,*,#8542,.T.);
#11992=ORIENTED_EDGE('',*,*,#8550,.T.);
#11993=ORIENTED_EDGE('',*,*,#8551,.F.);
#11994=ORIENTED_EDGE('',*,*,#8552,.F.);
#11995=ORIENTED_EDGE('',*,*,#8553,.F.);
#11996=ORIENTED_EDGE('',*,*,#8547,.T.);
#11997=ORIENTED_EDGE('',*,*,#8554,.T.);
#11998=ORIENTED_EDGE('',*,*,#8555,.F.);
#11999=ORIENTED_EDGE('',*,*,#8556,.F.);
#12000=ORIENTED_EDGE('',*,*,#8551,.T.);
#12001=ORIENTED_EDGE('',*,*,#8557,.T.);
#12002=ORIENTED_EDGE('',*,*,#8558,.T.);
#12003=ORIENTED_EDGE('',*,*,#8559,.F.);
#12004=ORIENTED_EDGE('',*,*,#8560,.T.);
#12005=ORIENTED_EDGE('',*,*,#8561,.T.);
#12006=ORIENTED_EDGE('',*,*,#8562,.T.);
#12007=ORIENTED_EDGE('',*,*,#8563,.T.);
#12008=ORIENTED_EDGE('',*,*,#8564,.T.);
#12009=ORIENTED_EDGE('',*,*,#8565,.T.);
#12010=ORIENTED_EDGE('',*,*,#8566,.T.);
#12011=ORIENTED_EDGE('',*,*,#8567,.T.);
#12012=ORIENTED_EDGE('',*,*,#8568,.T.);
#12013=ORIENTED_EDGE('',*,*,#8569,.T.);
#12014=ORIENTED_EDGE('',*,*,#8570,.T.);
#12015=ORIENTED_EDGE('',*,*,#8571,.T.);
#12016=ORIENTED_EDGE('',*,*,#8572,.T.);
#12017=ORIENTED_EDGE('',*,*,#8573,.T.);
#12018=ORIENTED_EDGE('',*,*,#8574,.T.);
#12019=ORIENTED_EDGE('',*,*,#8575,.T.);
#12020=ORIENTED_EDGE('',*,*,#8576,.F.);
#12021=ORIENTED_EDGE('',*,*,#8577,.T.);
#12022=ORIENTED_EDGE('',*,*,#8578,.T.);
#12023=ORIENTED_EDGE('',*,*,#8579,.T.);
#12024=ORIENTED_EDGE('',*,*,#8580,.T.);
#12025=ORIENTED_EDGE('',*,*,#8581,.T.);
#12026=ORIENTED_EDGE('',*,*,#8582,.T.);
#12027=ORIENTED_EDGE('',*,*,#8583,.T.);
#12028=ORIENTED_EDGE('',*,*,#8584,.T.);
#12029=ORIENTED_EDGE('',*,*,#8585,.T.);
#12030=ORIENTED_EDGE('',*,*,#8586,.T.);
#12031=ORIENTED_EDGE('',*,*,#8587,.T.);
#12032=ORIENTED_EDGE('',*,*,#8588,.T.);
#12033=ORIENTED_EDGE('',*,*,#8589,.T.);
#12034=ORIENTED_EDGE('',*,*,#8590,.T.);
#12035=ORIENTED_EDGE('',*,*,#8591,.T.);
#12036=ORIENTED_EDGE('',*,*,#8555,.T.);
#12037=ORIENTED_EDGE('',*,*,#8592,.T.);
#12038=ORIENTED_EDGE('',*,*,#8593,.F.);
#12039=ORIENTED_EDGE('',*,*,#8594,.F.);
#12040=ORIENTED_EDGE('',*,*,#8595,.F.);
#12041=ORIENTED_EDGE('',*,*,#8596,.F.);
#12042=ORIENTED_EDGE('',*,*,#8597,.T.);
#12043=ORIENTED_EDGE('',*,*,#8593,.T.);
#12044=ORIENTED_EDGE('',*,*,#8598,.T.);
#12045=ORIENTED_EDGE('',*,*,#8599,.T.);
#12046=ORIENTED_EDGE('',*,*,#8600,.F.);
#12047=ORIENTED_EDGE('',*,*,#8597,.F.);
#12048=ORIENTED_EDGE('',*,*,#8601,.F.);
#12049=ORIENTED_EDGE('',*,*,#8575,.F.);
#12050=ORIENTED_EDGE('',*,*,#8574,.F.);
#12051=ORIENTED_EDGE('',*,*,#8573,.F.);
#12052=ORIENTED_EDGE('',*,*,#8572,.F.);
#12053=ORIENTED_EDGE('',*,*,#8571,.F.);
#12054=ORIENTED_EDGE('',*,*,#8570,.F.);
#12055=ORIENTED_EDGE('',*,*,#8569,.F.);
#12056=ORIENTED_EDGE('',*,*,#8568,.F.);
#12057=ORIENTED_EDGE('',*,*,#8567,.F.);
#12058=ORIENTED_EDGE('',*,*,#8566,.F.);
#12059=ORIENTED_EDGE('',*,*,#8565,.F.);
#12060=ORIENTED_EDGE('',*,*,#8564,.F.);
#12061=ORIENTED_EDGE('',*,*,#8563,.F.);
#12062=ORIENTED_EDGE('',*,*,#8562,.F.);
#12063=ORIENTED_EDGE('',*,*,#8561,.F.);
#12064=ORIENTED_EDGE('',*,*,#8560,.F.);
#12065=ORIENTED_EDGE('',*,*,#8602,.F.);
#12066=ORIENTED_EDGE('',*,*,#8501,.T.);
#12067=ORIENTED_EDGE('',*,*,#8506,.T.);
#12068=ORIENTED_EDGE('',*,*,#8505,.T.);
#12069=ORIENTED_EDGE('',*,*,#8510,.T.);
#12070=ORIENTED_EDGE('',*,*,#8515,.T.);
#12071=ORIENTED_EDGE('',*,*,#8514,.T.);
#12072=ORIENTED_EDGE('',*,*,#8520,.T.);
#12073=ORIENTED_EDGE('',*,*,#8519,.T.);
#12074=ORIENTED_EDGE('',*,*,#8523,.T.);
#12075=ORIENTED_EDGE('',*,*,#8528,.T.);
#12076=ORIENTED_EDGE('',*,*,#8527,.T.);
#12077=ORIENTED_EDGE('',*,*,#8531,.T.);
#12078=ORIENTED_EDGE('',*,*,#8536,.T.);
#12079=ORIENTED_EDGE('',*,*,#8535,.T.);
#12080=ORIENTED_EDGE('',*,*,#8539,.T.);
#12081=ORIENTED_EDGE('',*,*,#8544,.T.);
#12082=ORIENTED_EDGE('',*,*,#8543,.T.);
#12083=ORIENTED_EDGE('',*,*,#8549,.T.);
#12084=ORIENTED_EDGE('',*,*,#8548,.T.);
#12085=ORIENTED_EDGE('',*,*,#8553,.T.);
#12086=ORIENTED_EDGE('',*,*,#8552,.T.);
#12087=ORIENTED_EDGE('',*,*,#8556,.T.);
#12088=ORIENTED_EDGE('',*,*,#8595,.T.);
#12089=ORIENTED_EDGE('',*,*,#8594,.T.);
#12090=ORIENTED_EDGE('',*,*,#8603,.F.);
#12091=ORIENTED_EDGE('',*,*,#8604,.T.);
#12092=ORIENTED_EDGE('',*,*,#8502,.T.);
#12093=ORIENTED_EDGE('',*,*,#8602,.T.);
#12094=ORIENTED_EDGE('',*,*,#8605,.F.);
#12095=ORIENTED_EDGE('',*,*,#8599,.F.);
#12096=ORIENTED_EDGE('',*,*,#8598,.F.);
#12097=ORIENTED_EDGE('',*,*,#8592,.F.);
#12098=ORIENTED_EDGE('',*,*,#8557,.F.);
#12099=ORIENTED_EDGE('',*,*,#8554,.F.);
#12100=ORIENTED_EDGE('',*,*,#8550,.F.);
#12101=ORIENTED_EDGE('',*,*,#8546,.F.);
#12102=ORIENTED_EDGE('',*,*,#8545,.F.);
#12103=ORIENTED_EDGE('',*,*,#8541,.F.);
#12104=ORIENTED_EDGE('',*,*,#8540,.F.);
#12105=ORIENTED_EDGE('',*,*,#8537,.F.);
#12106=ORIENTED_EDGE('',*,*,#8533,.F.);
#12107=ORIENTED_EDGE('',*,*,#8532,.F.);
#12108=ORIENTED_EDGE('',*,*,#8529,.F.);
#12109=ORIENTED_EDGE('',*,*,#8525,.F.);
#12110=ORIENTED_EDGE('',*,*,#8524,.F.);
#12111=ORIENTED_EDGE('',*,*,#8521,.F.);
#12112=ORIENTED_EDGE('',*,*,#8517,.F.);
#12113=ORIENTED_EDGE('',*,*,#8516,.F.);
#12114=ORIENTED_EDGE('',*,*,#8512,.F.);
#12115=ORIENTED_EDGE('',*,*,#8511,.F.);
#12116=ORIENTED_EDGE('',*,*,#8508,.F.);
#12117=ORIENTED_EDGE('',*,*,#8507,.F.);
#12118=ORIENTED_EDGE('',*,*,#8503,.F.);
#12119=ORIENTED_EDGE('',*,*,#8604,.F.);
#12120=ORIENTED_EDGE('',*,*,#8606,.F.);
#12121=ORIENTED_EDGE('',*,*,#8558,.F.);
#12122=ORIENTED_EDGE('',*,*,#8591,.F.);
#12123=ORIENTED_EDGE('',*,*,#8590,.F.);
#12124=ORIENTED_EDGE('',*,*,#8589,.F.);
#12125=ORIENTED_EDGE('',*,*,#8588,.F.);
#12126=ORIENTED_EDGE('',*,*,#8587,.F.);
#12127=ORIENTED_EDGE('',*,*,#8586,.F.);
#12128=ORIENTED_EDGE('',*,*,#8585,.F.);
#12129=ORIENTED_EDGE('',*,*,#8584,.F.);
#12130=ORIENTED_EDGE('',*,*,#8583,.F.);
#12131=ORIENTED_EDGE('',*,*,#8582,.F.);
#12132=ORIENTED_EDGE('',*,*,#8581,.F.);
#12133=ORIENTED_EDGE('',*,*,#8580,.F.);
#12134=ORIENTED_EDGE('',*,*,#8579,.F.);
#12135=ORIENTED_EDGE('',*,*,#8578,.F.);
#12136=ORIENTED_EDGE('',*,*,#8577,.F.);
#12137=ORIENTED_EDGE('',*,*,#8607,.T.);
#12138=ORIENTED_EDGE('',*,*,#8608,.T.);
#12139=ORIENTED_EDGE('',*,*,#8605,.T.);
#12140=ORIENTED_EDGE('',*,*,#8559,.T.);
#12141=ORIENTED_EDGE('',*,*,#8606,.T.);
#12142=ORIENTED_EDGE('',*,*,#8603,.T.);
#12143=ORIENTED_EDGE('',*,*,#8608,.F.);
#12144=ORIENTED_EDGE('',*,*,#8609,.F.);
#12145=ORIENTED_EDGE('',*,*,#8607,.F.);
#12146=ORIENTED_EDGE('',*,*,#8596,.T.);
#12147=ORIENTED_EDGE('',*,*,#8610,.T.);
#12148=ORIENTED_EDGE('',*,*,#8611,.T.);
#12149=ORIENTED_EDGE('',*,*,#8610,.F.);
#12150=ORIENTED_EDGE('',*,*,#8600,.T.);
#12151=ORIENTED_EDGE('',*,*,#8576,.T.);
#12152=ORIENTED_EDGE('',*,*,#8601,.T.);
#12153=ORIENTED_EDGE('',*,*,#8611,.F.);
#12154=ORIENTED_EDGE('',*,*,#8612,.F.);
#12155=ORIENTED_EDGE('',*,*,#8613,.T.);
#12156=ORIENTED_EDGE('',*,*,#8614,.F.);
#12157=ORIENTED_EDGE('',*,*,#8615,.F.);
#12158=ORIENTED_EDGE('',*,*,#8616,.F.);
#12159=ORIENTED_EDGE('',*,*,#8617,.F.);
#12160=ORIENTED_EDGE('',*,*,#8614,.T.);
#12161=ORIENTED_EDGE('',*,*,#8618,.T.);
#12162=ORIENTED_EDGE('',*,*,#8619,.F.);
#12163=ORIENTED_EDGE('',*,*,#8618,.F.);
#12164=ORIENTED_EDGE('',*,*,#8613,.F.);
#12165=ORIENTED_EDGE('',*,*,#8620,.T.);
#12166=ORIENTED_EDGE('',*,*,#8621,.T.);
#12167=ORIENTED_EDGE('',*,*,#8622,.T.);
#12168=ORIENTED_EDGE('',*,*,#8623,.T.);
#12169=ORIENTED_EDGE('',*,*,#8624,.T.);
#12170=ORIENTED_EDGE('',*,*,#8625,.T.);
#12171=ORIENTED_EDGE('',*,*,#8626,.T.);
#12172=ORIENTED_EDGE('',*,*,#8627,.T.);
#12173=ORIENTED_EDGE('',*,*,#8628,.T.);
#12174=ORIENTED_EDGE('',*,*,#8629,.T.);
#12175=ORIENTED_EDGE('',*,*,#8630,.T.);
#12176=ORIENTED_EDGE('',*,*,#8631,.T.);
#12177=ORIENTED_EDGE('',*,*,#8632,.T.);
#12178=ORIENTED_EDGE('',*,*,#8633,.T.);
#12179=ORIENTED_EDGE('',*,*,#8634,.T.);
#12180=ORIENTED_EDGE('',*,*,#8635,.T.);
#12181=ORIENTED_EDGE('',*,*,#8636,.T.);
#12182=ORIENTED_EDGE('',*,*,#8637,.T.);
#12183=ORIENTED_EDGE('',*,*,#8638,.T.);
#12184=ORIENTED_EDGE('',*,*,#8639,.T.);
#12185=ORIENTED_EDGE('',*,*,#8640,.T.);
#12186=ORIENTED_EDGE('',*,*,#8641,.T.);
#12187=ORIENTED_EDGE('',*,*,#8642,.T.);
#12188=ORIENTED_EDGE('',*,*,#8643,.T.);
#12189=ORIENTED_EDGE('',*,*,#8644,.T.);
#12190=ORIENTED_EDGE('',*,*,#8645,.T.);
#12191=ORIENTED_EDGE('',*,*,#8646,.T.);
#12192=ORIENTED_EDGE('',*,*,#8647,.T.);
#12193=ORIENTED_EDGE('',*,*,#8648,.T.);
#12194=ORIENTED_EDGE('',*,*,#8649,.T.);
#12195=ORIENTED_EDGE('',*,*,#8650,.T.);
#12196=ORIENTED_EDGE('',*,*,#8651,.T.);
#12197=ORIENTED_EDGE('',*,*,#8652,.T.);
#12198=ORIENTED_EDGE('',*,*,#8653,.T.);
#12199=ORIENTED_EDGE('',*,*,#8654,.T.);
#12200=ORIENTED_EDGE('',*,*,#8655,.T.);
#12201=ORIENTED_EDGE('',*,*,#8656,.T.);
#12202=ORIENTED_EDGE('',*,*,#8657,.T.);
#12203=ORIENTED_EDGE('',*,*,#8658,.T.);
#12204=ORIENTED_EDGE('',*,*,#8659,.T.);
#12205=ORIENTED_EDGE('',*,*,#8660,.T.);
#12206=ORIENTED_EDGE('',*,*,#8661,.T.);
#12207=ORIENTED_EDGE('',*,*,#8662,.T.);
#12208=ORIENTED_EDGE('',*,*,#8663,.T.);
#12209=ORIENTED_EDGE('',*,*,#8664,.T.);
#12210=ORIENTED_EDGE('',*,*,#8665,.T.);
#12211=ORIENTED_EDGE('',*,*,#8666,.T.);
#12212=ORIENTED_EDGE('',*,*,#8667,.T.);
#12213=ORIENTED_EDGE('',*,*,#8668,.T.);
#12214=ORIENTED_EDGE('',*,*,#8669,.T.);
#12215=ORIENTED_EDGE('',*,*,#8670,.T.);
#12216=ORIENTED_EDGE('',*,*,#8671,.T.);
#12217=ORIENTED_EDGE('',*,*,#8672,.T.);
#12218=ORIENTED_EDGE('',*,*,#8673,.T.);
#12219=ORIENTED_EDGE('',*,*,#8674,.T.);
#12220=ORIENTED_EDGE('',*,*,#8675,.T.);
#12221=ORIENTED_EDGE('',*,*,#8615,.T.);
#12222=ORIENTED_EDGE('',*,*,#8617,.T.);
#12223=ORIENTED_EDGE('',*,*,#8676,.T.);
#12224=ORIENTED_EDGE('',*,*,#8677,.T.);
#12225=ORIENTED_EDGE('',*,*,#8678,.T.);
#12226=ORIENTED_EDGE('',*,*,#8679,.T.);
#12227=ORIENTED_EDGE('',*,*,#8680,.T.);
#12228=ORIENTED_EDGE('',*,*,#8681,.T.);
#12229=ORIENTED_EDGE('',*,*,#8682,.T.);
#12230=ORIENTED_EDGE('',*,*,#8683,.T.);
#12231=ORIENTED_EDGE('',*,*,#8684,.T.);
#12232=ORIENTED_EDGE('',*,*,#8685,.T.);
#12233=ORIENTED_EDGE('',*,*,#8686,.T.);
#12234=ORIENTED_EDGE('',*,*,#8687,.T.);
#12235=ORIENTED_EDGE('',*,*,#8688,.T.);
#12236=ORIENTED_EDGE('',*,*,#8689,.T.);
#12237=ORIENTED_EDGE('',*,*,#8690,.T.);
#12238=ORIENTED_EDGE('',*,*,#8691,.T.);
#12239=ORIENTED_EDGE('',*,*,#8692,.T.);
#12240=ORIENTED_EDGE('',*,*,#8693,.T.);
#12241=ORIENTED_EDGE('',*,*,#8694,.T.);
#12242=ORIENTED_EDGE('',*,*,#8695,.T.);
#12243=ORIENTED_EDGE('',*,*,#8696,.T.);
#12244=ORIENTED_EDGE('',*,*,#8697,.T.);
#12245=ORIENTED_EDGE('',*,*,#8698,.T.);
#12246=ORIENTED_EDGE('',*,*,#8699,.T.);
#12247=ORIENTED_EDGE('',*,*,#8700,.T.);
#12248=ORIENTED_EDGE('',*,*,#8701,.T.);
#12249=ORIENTED_EDGE('',*,*,#8702,.T.);
#12250=ORIENTED_EDGE('',*,*,#8703,.T.);
#12251=ORIENTED_EDGE('',*,*,#8704,.T.);
#12252=ORIENTED_EDGE('',*,*,#8705,.T.);
#12253=ORIENTED_EDGE('',*,*,#8706,.T.);
#12254=ORIENTED_EDGE('',*,*,#8707,.T.);
#12255=ORIENTED_EDGE('',*,*,#8708,.T.);
#12256=ORIENTED_EDGE('',*,*,#8709,.T.);
#12257=ORIENTED_EDGE('',*,*,#8710,.T.);
#12258=ORIENTED_EDGE('',*,*,#8711,.T.);
#12259=ORIENTED_EDGE('',*,*,#8712,.T.);
#12260=ORIENTED_EDGE('',*,*,#8713,.T.);
#12261=ORIENTED_EDGE('',*,*,#8714,.T.);
#12262=ORIENTED_EDGE('',*,*,#8715,.T.);
#12263=ORIENTED_EDGE('',*,*,#8716,.T.);
#12264=ORIENTED_EDGE('',*,*,#8717,.T.);
#12265=ORIENTED_EDGE('',*,*,#8718,.T.);
#12266=ORIENTED_EDGE('',*,*,#8719,.T.);
#12267=ORIENTED_EDGE('',*,*,#8720,.T.);
#12268=ORIENTED_EDGE('',*,*,#8721,.T.);
#12269=ORIENTED_EDGE('',*,*,#8722,.T.);
#12270=ORIENTED_EDGE('',*,*,#8723,.T.);
#12271=ORIENTED_EDGE('',*,*,#8724,.T.);
#12272=ORIENTED_EDGE('',*,*,#8725,.T.);
#12273=ORIENTED_EDGE('',*,*,#8726,.T.);
#12274=ORIENTED_EDGE('',*,*,#8727,.T.);
#12275=ORIENTED_EDGE('',*,*,#8726,.F.);
#12276=ORIENTED_EDGE('',*,*,#8728,.F.);
#12277=ORIENTED_EDGE('',*,*,#8729,.T.);
#12278=ORIENTED_EDGE('',*,*,#8730,.F.);
#12279=ORIENTED_EDGE('',*,*,#8677,.F.);
#12280=ORIENTED_EDGE('',*,*,#8731,.F.);
#12281=ORIENTED_EDGE('',*,*,#8678,.F.);
#12282=ORIENTED_EDGE('',*,*,#8730,.T.);
#12283=ORIENTED_EDGE('',*,*,#8732,.T.);
#12284=ORIENTED_EDGE('',*,*,#8733,.F.);
#12285=ORIENTED_EDGE('',*,*,#8732,.F.);
#12286=ORIENTED_EDGE('',*,*,#8729,.F.);
#12287=ORIENTED_EDGE('',*,*,#8734,.F.);
#12288=ORIENTED_EDGE('',*,*,#8735,.T.);
#12289=ORIENTED_EDGE('',*,*,#8736,.F.);
#12290=ORIENTED_EDGE('',*,*,#8680,.F.);
#12291=ORIENTED_EDGE('',*,*,#8737,.F.);
#12292=ORIENTED_EDGE('',*,*,#8681,.F.);
#12293=ORIENTED_EDGE('',*,*,#8736,.T.);
#12294=ORIENTED_EDGE('',*,*,#8738,.T.);
#12295=ORIENTED_EDGE('',*,*,#8739,.F.);
#12296=ORIENTED_EDGE('',*,*,#8738,.F.);
#12297=ORIENTED_EDGE('',*,*,#8735,.F.);
#12298=ORIENTED_EDGE('',*,*,#8740,.F.);
#12299=ORIENTED_EDGE('',*,*,#8741,.T.);
#12300=ORIENTED_EDGE('',*,*,#8742,.F.);
#12301=ORIENTED_EDGE('',*,*,#8683,.F.);
#12302=ORIENTED_EDGE('',*,*,#8743,.F.);
#12303=ORIENTED_EDGE('',*,*,#8684,.F.);
#12304=ORIENTED_EDGE('',*,*,#8742,.T.);
#12305=ORIENTED_EDGE('',*,*,#8744,.T.);
#12306=ORIENTED_EDGE('',*,*,#8745,.F.);
#12307=ORIENTED_EDGE('',*,*,#8744,.F.);
#12308=ORIENTED_EDGE('',*,*,#8741,.F.);
#12309=ORIENTED_EDGE('',*,*,#8746,.F.);
#12310=ORIENTED_EDGE('',*,*,#8747,.T.);
#12311=ORIENTED_EDGE('',*,*,#8748,.F.);
#12312=ORIENTED_EDGE('',*,*,#8686,.F.);
#12313=ORIENTED_EDGE('',*,*,#8749,.F.);
#12314=ORIENTED_EDGE('',*,*,#8687,.F.);
#12315=ORIENTED_EDGE('',*,*,#8748,.T.);
#12316=ORIENTED_EDGE('',*,*,#8750,.T.);
#12317=ORIENTED_EDGE('',*,*,#8751,.F.);
#12318=ORIENTED_EDGE('',*,*,#8750,.F.);
#12319=ORIENTED_EDGE('',*,*,#8747,.F.);
#12320=ORIENTED_EDGE('',*,*,#8752,.F.);
#12321=ORIENTED_EDGE('',*,*,#8753,.T.);
#12322=ORIENTED_EDGE('',*,*,#8754,.F.);
#12323=ORIENTED_EDGE('',*,*,#8689,.F.);
#12324=ORIENTED_EDGE('',*,*,#8755,.F.);
#12325=ORIENTED_EDGE('',*,*,#8690,.F.);
#12326=ORIENTED_EDGE('',*,*,#8754,.T.);
#12327=ORIENTED_EDGE('',*,*,#8756,.T.);
#12328=ORIENTED_EDGE('',*,*,#8757,.F.);
#12329=ORIENTED_EDGE('',*,*,#8756,.F.);
#12330=ORIENTED_EDGE('',*,*,#8753,.F.);
#12331=ORIENTED_EDGE('',*,*,#8758,.F.);
#12332=ORIENTED_EDGE('',*,*,#8759,.T.);
#12333=ORIENTED_EDGE('',*,*,#8760,.F.);
#12334=ORIENTED_EDGE('',*,*,#8692,.F.);
#12335=ORIENTED_EDGE('',*,*,#8761,.F.);
#12336=ORIENTED_EDGE('',*,*,#8693,.F.);
#12337=ORIENTED_EDGE('',*,*,#8760,.T.);
#12338=ORIENTED_EDGE('',*,*,#8762,.T.);
#12339=ORIENTED_EDGE('',*,*,#8763,.F.);
#12340=ORIENTED_EDGE('',*,*,#8762,.F.);
#12341=ORIENTED_EDGE('',*,*,#8759,.F.);
#12342=ORIENTED_EDGE('',*,*,#8764,.F.);
#12343=ORIENTED_EDGE('',*,*,#8765,.T.);
#12344=ORIENTED_EDGE('',*,*,#8766,.F.);
#12345=ORIENTED_EDGE('',*,*,#8695,.F.);
#12346=ORIENTED_EDGE('',*,*,#8767,.F.);
#12347=ORIENTED_EDGE('',*,*,#8696,.F.);
#12348=ORIENTED_EDGE('',*,*,#8766,.T.);
#12349=ORIENTED_EDGE('',*,*,#8768,.T.);
#12350=ORIENTED_EDGE('',*,*,#8769,.F.);
#12351=ORIENTED_EDGE('',*,*,#8768,.F.);
#12352=ORIENTED_EDGE('',*,*,#8765,.F.);
#12353=ORIENTED_EDGE('',*,*,#8770,.F.);
#12354=ORIENTED_EDGE('',*,*,#8771,.T.);
#12355=ORIENTED_EDGE('',*,*,#8772,.F.);
#12356=ORIENTED_EDGE('',*,*,#8698,.F.);
#12357=ORIENTED_EDGE('',*,*,#8773,.F.);
#12358=ORIENTED_EDGE('',*,*,#8699,.F.);
#12359=ORIENTED_EDGE('',*,*,#8772,.T.);
#12360=ORIENTED_EDGE('',*,*,#8774,.T.);
#12361=ORIENTED_EDGE('',*,*,#8775,.F.);
#12362=ORIENTED_EDGE('',*,*,#8774,.F.);
#12363=ORIENTED_EDGE('',*,*,#8771,.F.);
#12364=ORIENTED_EDGE('',*,*,#8776,.F.);
#12365=ORIENTED_EDGE('',*,*,#8777,.T.);
#12366=ORIENTED_EDGE('',*,*,#8778,.F.);
#12367=ORIENTED_EDGE('',*,*,#8701,.F.);
#12368=ORIENTED_EDGE('',*,*,#8779,.F.);
#12369=ORIENTED_EDGE('',*,*,#8702,.F.);
#12370=ORIENTED_EDGE('',*,*,#8778,.T.);
#12371=ORIENTED_EDGE('',*,*,#8780,.T.);
#12372=ORIENTED_EDGE('',*,*,#8781,.F.);
#12373=ORIENTED_EDGE('',*,*,#8780,.F.);
#12374=ORIENTED_EDGE('',*,*,#8777,.F.);
#12375=ORIENTED_EDGE('',*,*,#8782,.F.);
#12376=ORIENTED_EDGE('',*,*,#8783,.T.);
#12377=ORIENTED_EDGE('',*,*,#8784,.F.);
#12378=ORIENTED_EDGE('',*,*,#8704,.F.);
#12379=ORIENTED_EDGE('',*,*,#8785,.F.);
#12380=ORIENTED_EDGE('',*,*,#8705,.F.);
#12381=ORIENTED_EDGE('',*,*,#8784,.T.);
#12382=ORIENTED_EDGE('',*,*,#8786,.T.);
#12383=ORIENTED_EDGE('',*,*,#8787,.F.);
#12384=ORIENTED_EDGE('',*,*,#8786,.F.);
#12385=ORIENTED_EDGE('',*,*,#8783,.F.);
#12386=ORIENTED_EDGE('',*,*,#8788,.F.);
#12387=ORIENTED_EDGE('',*,*,#8789,.T.);
#12388=ORIENTED_EDGE('',*,*,#8790,.F.);
#12389=ORIENTED_EDGE('',*,*,#8707,.F.);
#12390=ORIENTED_EDGE('',*,*,#8791,.F.);
#12391=ORIENTED_EDGE('',*,*,#8708,.F.);
#12392=ORIENTED_EDGE('',*,*,#8790,.T.);
#12393=ORIENTED_EDGE('',*,*,#8792,.T.);
#12394=ORIENTED_EDGE('',*,*,#8793,.F.);
#12395=ORIENTED_EDGE('',*,*,#8792,.F.);
#12396=ORIENTED_EDGE('',*,*,#8789,.F.);
#12397=ORIENTED_EDGE('',*,*,#8794,.F.);
#12398=ORIENTED_EDGE('',*,*,#8795,.T.);
#12399=ORIENTED_EDGE('',*,*,#8796,.F.);
#12400=ORIENTED_EDGE('',*,*,#8710,.F.);
#12401=ORIENTED_EDGE('',*,*,#8797,.F.);
#12402=ORIENTED_EDGE('',*,*,#8711,.F.);
#12403=ORIENTED_EDGE('',*,*,#8796,.T.);
#12404=ORIENTED_EDGE('',*,*,#8798,.T.);
#12405=ORIENTED_EDGE('',*,*,#8799,.F.);
#12406=ORIENTED_EDGE('',*,*,#8798,.F.);
#12407=ORIENTED_EDGE('',*,*,#8795,.F.);
#12408=ORIENTED_EDGE('',*,*,#8800,.F.);
#12409=ORIENTED_EDGE('',*,*,#8801,.T.);
#12410=ORIENTED_EDGE('',*,*,#8802,.F.);
#12411=ORIENTED_EDGE('',*,*,#8713,.F.);
#12412=ORIENTED_EDGE('',*,*,#8803,.F.);
#12413=ORIENTED_EDGE('',*,*,#8714,.F.);
#12414=ORIENTED_EDGE('',*,*,#8802,.T.);
#12415=ORIENTED_EDGE('',*,*,#8804,.T.);
#12416=ORIENTED_EDGE('',*,*,#8805,.F.);
#12417=ORIENTED_EDGE('',*,*,#8804,.F.);
#12418=ORIENTED_EDGE('',*,*,#8801,.F.);
#12419=ORIENTED_EDGE('',*,*,#8806,.F.);
#12420=ORIENTED_EDGE('',*,*,#8807,.T.);
#12421=ORIENTED_EDGE('',*,*,#8808,.F.);
#12422=ORIENTED_EDGE('',*,*,#8716,.F.);
#12423=ORIENTED_EDGE('',*,*,#8809,.F.);
#12424=ORIENTED_EDGE('',*,*,#8717,.F.);
#12425=ORIENTED_EDGE('',*,*,#8808,.T.);
#12426=ORIENTED_EDGE('',*,*,#8810,.T.);
#12427=ORIENTED_EDGE('',*,*,#8811,.F.);
#12428=ORIENTED_EDGE('',*,*,#8810,.F.);
#12429=ORIENTED_EDGE('',*,*,#8807,.F.);
#12430=ORIENTED_EDGE('',*,*,#8812,.F.);
#12431=ORIENTED_EDGE('',*,*,#8813,.T.);
#12432=ORIENTED_EDGE('',*,*,#8814,.F.);
#12433=ORIENTED_EDGE('',*,*,#8719,.F.);
#12434=ORIENTED_EDGE('',*,*,#8815,.F.);
#12435=ORIENTED_EDGE('',*,*,#8720,.F.);
#12436=ORIENTED_EDGE('',*,*,#8814,.T.);
#12437=ORIENTED_EDGE('',*,*,#8816,.T.);
#12438=ORIENTED_EDGE('',*,*,#8817,.F.);
#12439=ORIENTED_EDGE('',*,*,#8816,.F.);
#12440=ORIENTED_EDGE('',*,*,#8813,.F.);
#12441=ORIENTED_EDGE('',*,*,#8818,.F.);
#12442=ORIENTED_EDGE('',*,*,#8819,.T.);
#12443=ORIENTED_EDGE('',*,*,#8820,.F.);
#12444=ORIENTED_EDGE('',*,*,#8722,.F.);
#12445=ORIENTED_EDGE('',*,*,#8821,.F.);
#12446=ORIENTED_EDGE('',*,*,#8723,.F.);
#12447=ORIENTED_EDGE('',*,*,#8820,.T.);
#12448=ORIENTED_EDGE('',*,*,#8822,.T.);
#12449=ORIENTED_EDGE('',*,*,#8823,.F.);
#12450=ORIENTED_EDGE('',*,*,#8822,.F.);
#12451=ORIENTED_EDGE('',*,*,#8819,.F.);
#12452=ORIENTED_EDGE('',*,*,#8824,.F.);
#12453=ORIENTED_EDGE('',*,*,#8825,.T.);
#12454=ORIENTED_EDGE('',*,*,#8826,.F.);
#12455=ORIENTED_EDGE('',*,*,#8725,.F.);
#12456=ORIENTED_EDGE('',*,*,#8827,.F.);
#12457=ORIENTED_EDGE('',*,*,#8620,.F.);
#12458=ORIENTED_EDGE('',*,*,#8826,.T.);
#12459=ORIENTED_EDGE('',*,*,#8828,.T.);
#12460=ORIENTED_EDGE('',*,*,#8829,.F.);
#12461=ORIENTED_EDGE('',*,*,#8828,.F.);
#12462=ORIENTED_EDGE('',*,*,#8825,.F.);
#12463=ORIENTED_EDGE('',*,*,#8830,.F.);
#12464=ORIENTED_EDGE('',*,*,#8831,.F.);
#12465=ORIENTED_EDGE('',*,*,#8832,.T.);
#12466=ORIENTED_EDGE('',*,*,#8833,.F.);
#12467=ORIENTED_EDGE('',*,*,#8622,.F.);
#12468=ORIENTED_EDGE('',*,*,#8834,.F.);
#12469=ORIENTED_EDGE('',*,*,#8623,.F.);
#12470=ORIENTED_EDGE('',*,*,#8833,.T.);
#12471=ORIENTED_EDGE('',*,*,#8835,.T.);
#12472=ORIENTED_EDGE('',*,*,#8836,.F.);
#12473=ORIENTED_EDGE('',*,*,#8835,.F.);
#12474=ORIENTED_EDGE('',*,*,#8832,.F.);
#12475=ORIENTED_EDGE('',*,*,#8837,.F.);
#12476=ORIENTED_EDGE('',*,*,#8838,.T.);
#12477=ORIENTED_EDGE('',*,*,#8839,.F.);
#12478=ORIENTED_EDGE('',*,*,#8625,.F.);
#12479=ORIENTED_EDGE('',*,*,#8840,.F.);
#12480=ORIENTED_EDGE('',*,*,#8626,.F.);
#12481=ORIENTED_EDGE('',*,*,#8839,.T.);
#12482=ORIENTED_EDGE('',*,*,#8841,.T.);
#12483=ORIENTED_EDGE('',*,*,#8842,.F.);
#12484=ORIENTED_EDGE('',*,*,#8841,.F.);
#12485=ORIENTED_EDGE('',*,*,#8838,.F.);
#12486=ORIENTED_EDGE('',*,*,#8843,.F.);
#12487=ORIENTED_EDGE('',*,*,#8844,.T.);
#12488=ORIENTED_EDGE('',*,*,#8845,.F.);
#12489=ORIENTED_EDGE('',*,*,#8628,.F.);
#12490=ORIENTED_EDGE('',*,*,#8846,.F.);
#12491=ORIENTED_EDGE('',*,*,#8629,.F.);
#12492=ORIENTED_EDGE('',*,*,#8845,.T.);
#12493=ORIENTED_EDGE('',*,*,#8847,.T.);
#12494=ORIENTED_EDGE('',*,*,#8848,.F.);
#12495=ORIENTED_EDGE('',*,*,#8847,.F.);
#12496=ORIENTED_EDGE('',*,*,#8844,.F.);
#12497=ORIENTED_EDGE('',*,*,#8849,.F.);
#12498=ORIENTED_EDGE('',*,*,#8850,.T.);
#12499=ORIENTED_EDGE('',*,*,#8851,.F.);
#12500=ORIENTED_EDGE('',*,*,#8631,.F.);
#12501=ORIENTED_EDGE('',*,*,#8852,.F.);
#12502=ORIENTED_EDGE('',*,*,#8632,.F.);
#12503=ORIENTED_EDGE('',*,*,#8851,.T.);
#12504=ORIENTED_EDGE('',*,*,#8853,.T.);
#12505=ORIENTED_EDGE('',*,*,#8854,.F.);
#12506=ORIENTED_EDGE('',*,*,#8853,.F.);
#12507=ORIENTED_EDGE('',*,*,#8850,.F.);
#12508=ORIENTED_EDGE('',*,*,#8855,.F.);
#12509=ORIENTED_EDGE('',*,*,#8856,.T.);
#12510=ORIENTED_EDGE('',*,*,#8857,.F.);
#12511=ORIENTED_EDGE('',*,*,#8634,.F.);
#12512=ORIENTED_EDGE('',*,*,#8858,.F.);
#12513=ORIENTED_EDGE('',*,*,#8635,.F.);
#12514=ORIENTED_EDGE('',*,*,#8857,.T.);
#12515=ORIENTED_EDGE('',*,*,#8859,.T.);
#12516=ORIENTED_EDGE('',*,*,#8860,.F.);
#12517=ORIENTED_EDGE('',*,*,#8859,.F.);
#12518=ORIENTED_EDGE('',*,*,#8856,.F.);
#12519=ORIENTED_EDGE('',*,*,#8861,.F.);
#12520=ORIENTED_EDGE('',*,*,#8862,.T.);
#12521=ORIENTED_EDGE('',*,*,#8863,.F.);
#12522=ORIENTED_EDGE('',*,*,#8637,.F.);
#12523=ORIENTED_EDGE('',*,*,#8864,.F.);
#12524=ORIENTED_EDGE('',*,*,#8638,.F.);
#12525=ORIENTED_EDGE('',*,*,#8863,.T.);
#12526=ORIENTED_EDGE('',*,*,#8865,.T.);
#12527=ORIENTED_EDGE('',*,*,#8866,.F.);
#12528=ORIENTED_EDGE('',*,*,#8865,.F.);
#12529=ORIENTED_EDGE('',*,*,#8862,.F.);
#12530=ORIENTED_EDGE('',*,*,#8867,.F.);
#12531=ORIENTED_EDGE('',*,*,#8868,.T.);
#12532=ORIENTED_EDGE('',*,*,#8869,.F.);
#12533=ORIENTED_EDGE('',*,*,#8640,.F.);
#12534=ORIENTED_EDGE('',*,*,#8870,.F.);
#12535=ORIENTED_EDGE('',*,*,#8641,.F.);
#12536=ORIENTED_EDGE('',*,*,#8869,.T.);
#12537=ORIENTED_EDGE('',*,*,#8871,.T.);
#12538=ORIENTED_EDGE('',*,*,#8872,.F.);
#12539=ORIENTED_EDGE('',*,*,#8871,.F.);
#12540=ORIENTED_EDGE('',*,*,#8868,.F.);
#12541=ORIENTED_EDGE('',*,*,#8873,.F.);
#12542=ORIENTED_EDGE('',*,*,#8874,.T.);
#12543=ORIENTED_EDGE('',*,*,#8875,.F.);
#12544=ORIENTED_EDGE('',*,*,#8643,.F.);
#12545=ORIENTED_EDGE('',*,*,#8876,.F.);
#12546=ORIENTED_EDGE('',*,*,#8644,.F.);
#12547=ORIENTED_EDGE('',*,*,#8875,.T.);
#12548=ORIENTED_EDGE('',*,*,#8877,.T.);
#12549=ORIENTED_EDGE('',*,*,#8878,.F.);
#12550=ORIENTED_EDGE('',*,*,#8877,.F.);
#12551=ORIENTED_EDGE('',*,*,#8874,.F.);
#12552=ORIENTED_EDGE('',*,*,#8879,.F.);
#12553=ORIENTED_EDGE('',*,*,#8880,.T.);
#12554=ORIENTED_EDGE('',*,*,#8881,.F.);
#12555=ORIENTED_EDGE('',*,*,#8646,.F.);
#12556=ORIENTED_EDGE('',*,*,#8882,.F.);
#12557=ORIENTED_EDGE('',*,*,#8647,.F.);
#12558=ORIENTED_EDGE('',*,*,#8881,.T.);
#12559=ORIENTED_EDGE('',*,*,#8883,.T.);
#12560=ORIENTED_EDGE('',*,*,#8884,.F.);
#12561=ORIENTED_EDGE('',*,*,#8883,.F.);
#12562=ORIENTED_EDGE('',*,*,#8880,.F.);
#12563=ORIENTED_EDGE('',*,*,#8885,.F.);
#12564=ORIENTED_EDGE('',*,*,#8886,.T.);
#12565=ORIENTED_EDGE('',*,*,#8887,.F.);
#12566=ORIENTED_EDGE('',*,*,#8649,.F.);
#12567=ORIENTED_EDGE('',*,*,#8888,.F.);
#12568=ORIENTED_EDGE('',*,*,#8650,.F.);
#12569=ORIENTED_EDGE('',*,*,#8887,.T.);
#12570=ORIENTED_EDGE('',*,*,#8889,.T.);
#12571=ORIENTED_EDGE('',*,*,#8890,.F.);
#12572=ORIENTED_EDGE('',*,*,#8889,.F.);
#12573=ORIENTED_EDGE('',*,*,#8886,.F.);
#12574=ORIENTED_EDGE('',*,*,#8891,.F.);
#12575=ORIENTED_EDGE('',*,*,#8892,.T.);
#12576=ORIENTED_EDGE('',*,*,#8893,.F.);
#12577=ORIENTED_EDGE('',*,*,#8652,.F.);
#12578=ORIENTED_EDGE('',*,*,#8894,.F.);
#12579=ORIENTED_EDGE('',*,*,#8653,.F.);
#12580=ORIENTED_EDGE('',*,*,#8893,.T.);
#12581=ORIENTED_EDGE('',*,*,#8895,.T.);
#12582=ORIENTED_EDGE('',*,*,#8896,.F.);
#12583=ORIENTED_EDGE('',*,*,#8895,.F.);
#12584=ORIENTED_EDGE('',*,*,#8892,.F.);
#12585=ORIENTED_EDGE('',*,*,#8897,.F.);
#12586=ORIENTED_EDGE('',*,*,#8898,.T.);
#12587=ORIENTED_EDGE('',*,*,#8899,.F.);
#12588=ORIENTED_EDGE('',*,*,#8655,.F.);
#12589=ORIENTED_EDGE('',*,*,#8900,.F.);
#12590=ORIENTED_EDGE('',*,*,#8656,.F.);
#12591=ORIENTED_EDGE('',*,*,#8899,.T.);
#12592=ORIENTED_EDGE('',*,*,#8901,.T.);
#12593=ORIENTED_EDGE('',*,*,#8902,.F.);
#12594=ORIENTED_EDGE('',*,*,#8901,.F.);
#12595=ORIENTED_EDGE('',*,*,#8898,.F.);
#12596=ORIENTED_EDGE('',*,*,#8903,.F.);
#12597=ORIENTED_EDGE('',*,*,#8904,.T.);
#12598=ORIENTED_EDGE('',*,*,#8905,.F.);
#12599=ORIENTED_EDGE('',*,*,#8658,.F.);
#12600=ORIENTED_EDGE('',*,*,#8906,.F.);
#12601=ORIENTED_EDGE('',*,*,#8659,.F.);
#12602=ORIENTED_EDGE('',*,*,#8905,.T.);
#12603=ORIENTED_EDGE('',*,*,#8907,.T.);
#12604=ORIENTED_EDGE('',*,*,#8908,.F.);
#12605=ORIENTED_EDGE('',*,*,#8907,.F.);
#12606=ORIENTED_EDGE('',*,*,#8904,.F.);
#12607=ORIENTED_EDGE('',*,*,#8909,.F.);
#12608=ORIENTED_EDGE('',*,*,#8910,.T.);
#12609=ORIENTED_EDGE('',*,*,#8911,.F.);
#12610=ORIENTED_EDGE('',*,*,#8661,.F.);
#12611=ORIENTED_EDGE('',*,*,#8912,.F.);
#12612=ORIENTED_EDGE('',*,*,#8662,.F.);
#12613=ORIENTED_EDGE('',*,*,#8911,.T.);
#12614=ORIENTED_EDGE('',*,*,#8913,.T.);
#12615=ORIENTED_EDGE('',*,*,#8914,.F.);
#12616=ORIENTED_EDGE('',*,*,#8913,.F.);
#12617=ORIENTED_EDGE('',*,*,#8910,.F.);
#12618=ORIENTED_EDGE('',*,*,#8915,.F.);
#12619=ORIENTED_EDGE('',*,*,#8916,.T.);
#12620=ORIENTED_EDGE('',*,*,#8917,.F.);
#12621=ORIENTED_EDGE('',*,*,#8664,.F.);
#12622=ORIENTED_EDGE('',*,*,#8918,.F.);
#12623=ORIENTED_EDGE('',*,*,#8665,.F.);
#12624=ORIENTED_EDGE('',*,*,#8917,.T.);
#12625=ORIENTED_EDGE('',*,*,#8919,.T.);
#12626=ORIENTED_EDGE('',*,*,#8920,.F.);
#12627=ORIENTED_EDGE('',*,*,#8919,.F.);
#12628=ORIENTED_EDGE('',*,*,#8916,.F.);
#12629=ORIENTED_EDGE('',*,*,#8921,.F.);
#12630=ORIENTED_EDGE('',*,*,#8922,.T.);
#12631=ORIENTED_EDGE('',*,*,#8923,.F.);
#12632=ORIENTED_EDGE('',*,*,#8667,.F.);
#12633=ORIENTED_EDGE('',*,*,#8924,.F.);
#12634=ORIENTED_EDGE('',*,*,#8668,.F.);
#12635=ORIENTED_EDGE('',*,*,#8923,.T.);
#12636=ORIENTED_EDGE('',*,*,#8925,.T.);
#12637=ORIENTED_EDGE('',*,*,#8926,.F.);
#12638=ORIENTED_EDGE('',*,*,#8925,.F.);
#12639=ORIENTED_EDGE('',*,*,#8922,.F.);
#12640=ORIENTED_EDGE('',*,*,#8927,.F.);
#12641=ORIENTED_EDGE('',*,*,#8928,.T.);
#12642=ORIENTED_EDGE('',*,*,#8929,.F.);
#12643=ORIENTED_EDGE('',*,*,#8670,.F.);
#12644=ORIENTED_EDGE('',*,*,#8930,.F.);
#12645=ORIENTED_EDGE('',*,*,#8671,.F.);
#12646=ORIENTED_EDGE('',*,*,#8929,.T.);
#12647=ORIENTED_EDGE('',*,*,#8931,.T.);
#12648=ORIENTED_EDGE('',*,*,#8932,.F.);
#12649=ORIENTED_EDGE('',*,*,#8931,.F.);
#12650=ORIENTED_EDGE('',*,*,#8928,.F.);
#12651=ORIENTED_EDGE('',*,*,#8933,.F.);
#12652=ORIENTED_EDGE('',*,*,#8934,.T.);
#12653=ORIENTED_EDGE('',*,*,#8935,.F.);
#12654=ORIENTED_EDGE('',*,*,#8673,.F.);
#12655=ORIENTED_EDGE('',*,*,#8936,.F.);
#12656=ORIENTED_EDGE('',*,*,#8674,.F.);
#12657=ORIENTED_EDGE('',*,*,#8935,.T.);
#12658=ORIENTED_EDGE('',*,*,#8937,.T.);
#12659=ORIENTED_EDGE('',*,*,#8938,.F.);
#12660=ORIENTED_EDGE('',*,*,#8937,.F.);
#12661=ORIENTED_EDGE('',*,*,#8934,.F.);
#12662=ORIENTED_EDGE('',*,*,#8829,.T.);
#12663=ORIENTED_EDGE('',*,*,#8939,.T.);
#12664=ORIENTED_EDGE('',*,*,#8609,.T.);
#12665=ORIENTED_EDGE('',*,*,#8939,.F.);
#12666=ORIENTED_EDGE('',*,*,#8830,.T.);
#12667=ORIENTED_EDGE('',*,*,#8824,.T.);
#12668=ORIENTED_EDGE('',*,*,#8724,.F.);
#12669=ORIENTED_EDGE('',*,*,#8821,.T.);
#12670=ORIENTED_EDGE('',*,*,#8823,.T.);
#12671=ORIENTED_EDGE('',*,*,#8818,.T.);
#12672=ORIENTED_EDGE('',*,*,#8721,.F.);
#12673=ORIENTED_EDGE('',*,*,#8815,.T.);
#12674=ORIENTED_EDGE('',*,*,#8817,.T.);
#12675=ORIENTED_EDGE('',*,*,#8812,.T.);
#12676=ORIENTED_EDGE('',*,*,#8718,.F.);
#12677=ORIENTED_EDGE('',*,*,#8809,.T.);
#12678=ORIENTED_EDGE('',*,*,#8811,.T.);
#12679=ORIENTED_EDGE('',*,*,#8806,.T.);
#12680=ORIENTED_EDGE('',*,*,#8715,.F.);
#12681=ORIENTED_EDGE('',*,*,#8803,.T.);
#12682=ORIENTED_EDGE('',*,*,#8805,.T.);
#12683=ORIENTED_EDGE('',*,*,#8800,.T.);
#12684=ORIENTED_EDGE('',*,*,#8712,.F.);
#12685=ORIENTED_EDGE('',*,*,#8797,.T.);
#12686=ORIENTED_EDGE('',*,*,#8799,.T.);
#12687=ORIENTED_EDGE('',*,*,#8794,.T.);
#12688=ORIENTED_EDGE('',*,*,#8709,.F.);
#12689=ORIENTED_EDGE('',*,*,#8791,.T.);
#12690=ORIENTED_EDGE('',*,*,#8793,.T.);
#12691=ORIENTED_EDGE('',*,*,#8788,.T.);
#12692=ORIENTED_EDGE('',*,*,#8706,.F.);
#12693=ORIENTED_EDGE('',*,*,#8785,.T.);
#12694=ORIENTED_EDGE('',*,*,#8787,.T.);
#12695=ORIENTED_EDGE('',*,*,#8782,.T.);
#12696=ORIENTED_EDGE('',*,*,#8703,.F.);
#12697=ORIENTED_EDGE('',*,*,#8779,.T.);
#12698=ORIENTED_EDGE('',*,*,#8781,.T.);
#12699=ORIENTED_EDGE('',*,*,#8776,.T.);
#12700=ORIENTED_EDGE('',*,*,#8700,.F.);
#12701=ORIENTED_EDGE('',*,*,#8773,.T.);
#12702=ORIENTED_EDGE('',*,*,#8775,.T.);
#12703=ORIENTED_EDGE('',*,*,#8770,.T.);
#12704=ORIENTED_EDGE('',*,*,#8697,.F.);
#12705=ORIENTED_EDGE('',*,*,#8767,.T.);
#12706=ORIENTED_EDGE('',*,*,#8769,.T.);
#12707=ORIENTED_EDGE('',*,*,#8764,.T.);
#12708=ORIENTED_EDGE('',*,*,#8694,.F.);
#12709=ORIENTED_EDGE('',*,*,#8761,.T.);
#12710=ORIENTED_EDGE('',*,*,#8763,.T.);
#12711=ORIENTED_EDGE('',*,*,#8758,.T.);
#12712=ORIENTED_EDGE('',*,*,#8691,.F.);
#12713=ORIENTED_EDGE('',*,*,#8755,.T.);
#12714=ORIENTED_EDGE('',*,*,#8757,.T.);
#12715=ORIENTED_EDGE('',*,*,#8752,.T.);
#12716=ORIENTED_EDGE('',*,*,#8688,.F.);
#12717=ORIENTED_EDGE('',*,*,#8749,.T.);
#12718=ORIENTED_EDGE('',*,*,#8751,.T.);
#12719=ORIENTED_EDGE('',*,*,#8746,.T.);
#12720=ORIENTED_EDGE('',*,*,#8685,.F.);
#12721=ORIENTED_EDGE('',*,*,#8743,.T.);
#12722=ORIENTED_EDGE('',*,*,#8745,.T.);
#12723=ORIENTED_EDGE('',*,*,#8740,.T.);
#12724=ORIENTED_EDGE('',*,*,#8682,.F.);
#12725=ORIENTED_EDGE('',*,*,#8737,.T.);
#12726=ORIENTED_EDGE('',*,*,#8739,.T.);
#12727=ORIENTED_EDGE('',*,*,#8734,.T.);
#12728=ORIENTED_EDGE('',*,*,#8679,.F.);
#12729=ORIENTED_EDGE('',*,*,#8731,.T.);
#12730=ORIENTED_EDGE('',*,*,#8733,.T.);
#12731=ORIENTED_EDGE('',*,*,#8728,.T.);
#12732=ORIENTED_EDGE('',*,*,#8676,.F.);
#12733=ORIENTED_EDGE('',*,*,#8616,.T.);
#12734=ORIENTED_EDGE('',*,*,#8619,.T.);
#12735=ORIENTED_EDGE('',*,*,#8612,.T.);
#12736=ORIENTED_EDGE('',*,*,#8675,.F.);
#12737=ORIENTED_EDGE('',*,*,#8936,.T.);
#12738=ORIENTED_EDGE('',*,*,#8938,.T.);
#12739=ORIENTED_EDGE('',*,*,#8933,.T.);
#12740=ORIENTED_EDGE('',*,*,#8672,.F.);
#12741=ORIENTED_EDGE('',*,*,#8930,.T.);
#12742=ORIENTED_EDGE('',*,*,#8932,.T.);
#12743=ORIENTED_EDGE('',*,*,#8927,.T.);
#12744=ORIENTED_EDGE('',*,*,#8669,.F.);
#12745=ORIENTED_EDGE('',*,*,#8924,.T.);
#12746=ORIENTED_EDGE('',*,*,#8926,.T.);
#12747=ORIENTED_EDGE('',*,*,#8921,.T.);
#12748=ORIENTED_EDGE('',*,*,#8666,.F.);
#12749=ORIENTED_EDGE('',*,*,#8918,.T.);
#12750=ORIENTED_EDGE('',*,*,#8920,.T.);
#12751=ORIENTED_EDGE('',*,*,#8915,.T.);
#12752=ORIENTED_EDGE('',*,*,#8663,.F.);
#12753=ORIENTED_EDGE('',*,*,#8912,.T.);
#12754=ORIENTED_EDGE('',*,*,#8914,.T.);
#12755=ORIENTED_EDGE('',*,*,#8909,.T.);
#12756=ORIENTED_EDGE('',*,*,#8660,.F.);
#12757=ORIENTED_EDGE('',*,*,#8906,.T.);
#12758=ORIENTED_EDGE('',*,*,#8908,.T.);
#12759=ORIENTED_EDGE('',*,*,#8903,.T.);
#12760=ORIENTED_EDGE('',*,*,#8657,.F.);
#12761=ORIENTED_EDGE('',*,*,#8900,.T.);
#12762=ORIENTED_EDGE('',*,*,#8902,.T.);
#12763=ORIENTED_EDGE('',*,*,#8897,.T.);
#12764=ORIENTED_EDGE('',*,*,#8654,.F.);
#12765=ORIENTED_EDGE('',*,*,#8894,.T.);
#12766=ORIENTED_EDGE('',*,*,#8896,.T.);
#12767=ORIENTED_EDGE('',*,*,#8891,.T.);
#12768=ORIENTED_EDGE('',*,*,#8651,.F.);
#12769=ORIENTED_EDGE('',*,*,#8888,.T.);
#12770=ORIENTED_EDGE('',*,*,#8890,.T.);
#12771=ORIENTED_EDGE('',*,*,#8885,.T.);
#12772=ORIENTED_EDGE('',*,*,#8648,.F.);
#12773=ORIENTED_EDGE('',*,*,#8882,.T.);
#12774=ORIENTED_EDGE('',*,*,#8884,.T.);
#12775=ORIENTED_EDGE('',*,*,#8879,.T.);
#12776=ORIENTED_EDGE('',*,*,#8645,.F.);
#12777=ORIENTED_EDGE('',*,*,#8876,.T.);
#12778=ORIENTED_EDGE('',*,*,#8878,.T.);
#12779=ORIENTED_EDGE('',*,*,#8873,.T.);
#12780=ORIENTED_EDGE('',*,*,#8642,.F.);
#12781=ORIENTED_EDGE('',*,*,#8870,.T.);
#12782=ORIENTED_EDGE('',*,*,#8872,.T.);
#12783=ORIENTED_EDGE('',*,*,#8867,.T.);
#12784=ORIENTED_EDGE('',*,*,#8639,.F.);
#12785=ORIENTED_EDGE('',*,*,#8864,.T.);
#12786=ORIENTED_EDGE('',*,*,#8866,.T.);
#12787=ORIENTED_EDGE('',*,*,#8861,.T.);
#12788=ORIENTED_EDGE('',*,*,#8636,.F.);
#12789=ORIENTED_EDGE('',*,*,#8858,.T.);
#12790=ORIENTED_EDGE('',*,*,#8860,.T.);
#12791=ORIENTED_EDGE('',*,*,#8855,.T.);
#12792=ORIENTED_EDGE('',*,*,#8633,.F.);
#12793=ORIENTED_EDGE('',*,*,#8852,.T.);
#12794=ORIENTED_EDGE('',*,*,#8854,.T.);
#12795=ORIENTED_EDGE('',*,*,#8849,.T.);
#12796=ORIENTED_EDGE('',*,*,#8630,.F.);
#12797=ORIENTED_EDGE('',*,*,#8846,.T.);
#12798=ORIENTED_EDGE('',*,*,#8848,.T.);
#12799=ORIENTED_EDGE('',*,*,#8843,.T.);
#12800=ORIENTED_EDGE('',*,*,#8627,.F.);
#12801=ORIENTED_EDGE('',*,*,#8840,.T.);
#12802=ORIENTED_EDGE('',*,*,#8842,.T.);
#12803=ORIENTED_EDGE('',*,*,#8837,.T.);
#12804=ORIENTED_EDGE('',*,*,#8624,.F.);
#12805=ORIENTED_EDGE('',*,*,#8834,.T.);
#12806=ORIENTED_EDGE('',*,*,#8836,.T.);
#12807=ORIENTED_EDGE('',*,*,#8831,.T.);
#12808=ORIENTED_EDGE('',*,*,#8621,.F.);
#12809=ORIENTED_EDGE('',*,*,#8827,.T.);
#12810=ORIENTED_EDGE('',*,*,#8727,.F.);
#12811=ORIENTED_EDGE('',*,*,#8940,.T.);
#12812=ORIENTED_EDGE('',*,*,#8941,.T.);
#12813=ORIENTED_EDGE('',*,*,#8942,.T.);
#12814=ORIENTED_EDGE('',*,*,#8943,.T.);
#12815=ORIENTED_EDGE('',*,*,#8944,.T.);
#12816=ORIENTED_EDGE('',*,*,#8945,.T.);
#12817=ORIENTED_EDGE('',*,*,#8946,.F.);
#12818=ORIENTED_EDGE('',*,*,#8947,.T.);
#12819=ORIENTED_EDGE('',*,*,#8948,.F.);
#12820=ORIENTED_EDGE('',*,*,#8949,.T.);
#12821=ORIENTED_EDGE('',*,*,#8950,.F.);
#12822=ORIENTED_EDGE('',*,*,#8951,.T.);
#12823=ORIENTED_EDGE('',*,*,#8952,.F.);
#12824=ORIENTED_EDGE('',*,*,#8953,.T.);
#12825=ORIENTED_EDGE('',*,*,#8954,.F.);
#12826=ORIENTED_EDGE('',*,*,#8955,.T.);
#12827=ORIENTED_EDGE('',*,*,#8956,.F.);
#12828=ORIENTED_EDGE('',*,*,#8957,.T.);
#12829=ORIENTED_EDGE('',*,*,#8958,.T.);
#12830=ORIENTED_EDGE('',*,*,#8957,.F.);
#12831=ORIENTED_EDGE('',*,*,#8955,.F.);
#12832=ORIENTED_EDGE('',*,*,#8953,.F.);
#12833=ORIENTED_EDGE('',*,*,#8951,.F.);
#12834=ORIENTED_EDGE('',*,*,#8949,.F.);
#12835=ORIENTED_EDGE('',*,*,#8947,.F.);
#12836=ORIENTED_EDGE('',*,*,#8958,.F.);
#12837=ORIENTED_EDGE('',*,*,#8940,.F.);
#12838=ORIENTED_EDGE('',*,*,#8959,.T.);
#12839=ORIENTED_EDGE('',*,*,#8946,.T.);
#12840=ORIENTED_EDGE('',*,*,#8960,.F.);
#12841=ORIENTED_EDGE('',*,*,#8945,.F.);
#12842=ORIENTED_EDGE('',*,*,#8961,.T.);
#12843=ORIENTED_EDGE('',*,*,#8956,.T.);
#12844=ORIENTED_EDGE('',*,*,#8959,.F.);
#12845=ORIENTED_EDGE('',*,*,#8944,.F.);
#12846=ORIENTED_EDGE('',*,*,#8962,.T.);
#12847=ORIENTED_EDGE('',*,*,#8954,.T.);
#12848=ORIENTED_EDGE('',*,*,#8961,.F.);
#12849=ORIENTED_EDGE('',*,*,#8943,.F.);
#12850=ORIENTED_EDGE('',*,*,#8963,.T.);
#12851=ORIENTED_EDGE('',*,*,#8952,.T.);
#12852=ORIENTED_EDGE('',*,*,#8962,.F.);
#12853=ORIENTED_EDGE('',*,*,#8942,.F.);
#12854=ORIENTED_EDGE('',*,*,#8964,.T.);
#12855=ORIENTED_EDGE('',*,*,#8950,.T.);
#12856=ORIENTED_EDGE('',*,*,#8963,.F.);
#12857=ORIENTED_EDGE('',*,*,#8941,.F.);
#12858=ORIENTED_EDGE('',*,*,#8960,.T.);
#12859=ORIENTED_EDGE('',*,*,#8948,.T.);
#12860=ORIENTED_EDGE('',*,*,#8964,.F.);
#12861=CYLINDRICAL_SURFACE('',#13758,4.25);
#12862=CYLINDRICAL_SURFACE('',#13763,2.6);
#12863=CYLINDRICAL_SURFACE('',#13764,4.25);
#12864=CYLINDRICAL_SURFACE('',#13769,2.6);
#12865=CYLINDRICAL_SURFACE('',#13770,4.25);
#12866=CYLINDRICAL_SURFACE('',#13775,2.6);
#12867=CYLINDRICAL_SURFACE('',#13776,4.25);
#12868=CYLINDRICAL_SURFACE('',#13781,2.6);
#12869=CYLINDRICAL_SURFACE('',#13782,4.25);
#12870=CYLINDRICAL_SURFACE('',#13787,2.6);
#12871=CYLINDRICAL_SURFACE('',#13788,4.25);
#12872=CYLINDRICAL_SURFACE('',#13793,2.6);
#12873=CYLINDRICAL_SURFACE('',#13801,5.35);
#12874=CYLINDRICAL_SURFACE('',#13805,5.35);
#12875=CYLINDRICAL_SURFACE('',#13809,5.35);
#12876=CYLINDRICAL_SURFACE('',#13813,5.35);
#12877=CYLINDRICAL_SURFACE('',#13823,3.55600000000001);
#12878=CYLINDRICAL_SURFACE('',#13825,3.556);
#12879=CYLINDRICAL_SURFACE('',#13827,3.556);
#12880=CYLINDRICAL_SURFACE('',#13829,3.55600000000001);
#12881=CYLINDRICAL_SURFACE('',#13841,6.35);
#12882=CYLINDRICAL_SURFACE('',#13847,6.35);
#12883=CYLINDRICAL_SURFACE('',#13876,4.25000000000001);
#12884=CYLINDRICAL_SURFACE('',#13882,4.25);
#12885=CYLINDRICAL_SURFACE('',#13888,4.25);
#12886=CYLINDRICAL_SURFACE('',#13892,4.25000000000001);
#12887=CYLINDRICAL_SURFACE('',#13896,4.25000000000001);
#12888=CYLINDRICAL_SURFACE('',#13905,4.25);
#12889=CYLINDRICAL_SURFACE('',#13912,4.25);
#12890=CYLINDRICAL_SURFACE('',#13919,4.25000000000001);
#12891=CYLINDRICAL_SURFACE('',#13936,2.6);
#12892=CYLINDRICAL_SURFACE('',#13938,2.6);
#12893=CYLINDRICAL_SURFACE('',#13940,2.6);
#12894=CYLINDRICAL_SURFACE('',#13942,2.6);
#12895=CYLINDRICAL_SURFACE('',#13944,2.6);
#12896=CYLINDRICAL_SURFACE('',#13946,2.6);
#12897=CYLINDRICAL_SURFACE('',#13948,2.6);
#12898=CYLINDRICAL_SURFACE('',#13950,2.6);
#12899=CYLINDRICAL_SURFACE('',#13954,3.225);
#12900=CYLINDRICAL_SURFACE('',#13958,3.225);
#12901=CYLINDRICAL_SURFACE('',#13960,3.225);
#12902=CYLINDRICAL_SURFACE('',#13962,3.225);
#12903=CYLINDRICAL_SURFACE('',#13964,3.225);
#12904=CYLINDRICAL_SURFACE('',#13966,3.225);
#12905=CYLINDRICAL_SURFACE('',#13970,3.225);
#12906=CYLINDRICAL_SURFACE('',#13974,3.225);
#12907=CYLINDRICAL_SURFACE('',#13994,2.464);
#12908=CYLINDRICAL_SURFACE('',#13997,2.464);
#12909=CYLINDRICAL_SURFACE('',#14000,2.464);
#12910=CYLINDRICAL_SURFACE('',#14007,6.35);
#12911=CYLINDRICAL_SURFACE('',#14018,2.464);
#12912=CYLINDRICAL_SURFACE('',#14023,2.464);
#12913=CYLINDRICAL_SURFACE('',#14027,11.1);
#12914=CYLINDRICAL_SURFACE('',#14053,8.75);
#12915=CYLINDRICAL_SURFACE('',#14059,11.1);
#12916=CYLINDRICAL_SURFACE('',#14106,8.75);
#12917=CYLINDRICAL_SURFACE('',#14108,6.45);
#12918=CYLINDRICAL_SURFACE('',#14115,1.92913);
#12919=CYLINDRICAL_SURFACE('',#14117,1.92913);
#12920=CYLINDRICAL_SURFACE('',#14118,1.92913);
#12921=CYLINDRICAL_SURFACE('',#14119,1.92913);
#12922=CYLINDRICAL_SURFACE('',#14120,1.92913);
#12923=CYLINDRICAL_SURFACE('',#14121,1.92913);
#12924=CYLINDRICAL_SURFACE('',#14122,1.92913);
#12925=CYLINDRICAL_SURFACE('',#14123,1.92913);
#12926=CYLINDRICAL_SURFACE('',#14124,1.92913);
#12927=CYLINDRICAL_SURFACE('',#14125,1.92913);
#12928=CYLINDRICAL_SURFACE('',#14126,1.92913);
#12929=CYLINDRICAL_SURFACE('',#14127,1.92913);
#12930=CYLINDRICAL_SURFACE('',#14128,1.92913);
#12931=CYLINDRICAL_SURFACE('',#14129,1.92913);
#12932=CYLINDRICAL_SURFACE('',#14130,1.92913);
#12933=CYLINDRICAL_SURFACE('',#14131,1.92913);
#12934=CYLINDRICAL_SURFACE('',#14132,1.92913);
#12935=CYLINDRICAL_SURFACE('',#14133,1.92913);
#12936=CYLINDRICAL_SURFACE('',#14134,1.92913);
#12937=CYLINDRICAL_SURFACE('',#14135,2.36347);
#12938=CYLINDRICAL_SURFACE('',#14139,1.92913);
#12939=CYLINDRICAL_SURFACE('',#14337,3.9624);
#12940=CYLINDRICAL_SURFACE('',#14359,1.92913);
#12941=CYLINDRICAL_SURFACE('',#14361,1.92913);
#12942=CYLINDRICAL_SURFACE('',#14362,1.92913);
#12943=CYLINDRICAL_SURFACE('',#14363,1.92913);
#12944=CYLINDRICAL_SURFACE('',#14364,1.92913);
#12945=CYLINDRICAL_SURFACE('',#14365,1.92913);
#12946=CYLINDRICAL_SURFACE('',#14366,1.92913);
#12947=CYLINDRICAL_SURFACE('',#14367,1.92913);
#12948=CYLINDRICAL_SURFACE('',#14368,1.92913);
#12949=CYLINDRICAL_SURFACE('',#14369,1.92913);
#12950=CYLINDRICAL_SURFACE('',#14370,1.92913);
#12951=CYLINDRICAL_SURFACE('',#14371,1.92913);
#12952=CYLINDRICAL_SURFACE('',#14372,1.92913);
#12953=CYLINDRICAL_SURFACE('',#14373,1.92913);
#12954=CYLINDRICAL_SURFACE('',#14374,1.92913);
#12955=CYLINDRICAL_SURFACE('',#14375,1.92913);
#12956=CYLINDRICAL_SURFACE('',#14376,1.92913);
#12957=CYLINDRICAL_SURFACE('',#14377,1.92913);
#12958=CYLINDRICAL_SURFACE('',#14378,1.92913);
#12959=CYLINDRICAL_SURFACE('',#14379,1.92913);
#12960=CYLINDRICAL_SURFACE('',#14380,1.92913);
#12961=CYLINDRICAL_SURFACE('',#14381,1.92913);
#12962=CYLINDRICAL_SURFACE('',#14382,1.92913);
#12963=CYLINDRICAL_SURFACE('',#14383,1.92913);
#12964=CYLINDRICAL_SURFACE('',#14384,1.92913);
#12965=CYLINDRICAL_SURFACE('',#14385,1.92913);
#12966=CYLINDRICAL_SURFACE('',#14386,1.92913);
#12967=CYLINDRICAL_SURFACE('',#14387,2.36347);
#12968=CYLINDRICAL_SURFACE('',#14391,1.92913);
#12969=CYLINDRICAL_SURFACE('',#14452,3.9624);
#12970=CYLINDRICAL_SURFACE('',#14611,2.40538);
#12971=CYLINDRICAL_SURFACE('',#14613,2.40538);
#12972=CYLINDRICAL_SURFACE('',#14614,2.40538);
#12973=CYLINDRICAL_SURFACE('',#14615,2.40538);
#12974=CYLINDRICAL_SURFACE('',#14616,2.40538);
#12975=CYLINDRICAL_SURFACE('',#14617,2.40538);
#12976=CYLINDRICAL_SURFACE('',#14618,2.40538);
#12977=CYLINDRICAL_SURFACE('',#14619,2.40538);
#12978=CYLINDRICAL_SURFACE('',#14620,2.40538);
#12979=CYLINDRICAL_SURFACE('',#14621,2.40538);
#12980=CYLINDRICAL_SURFACE('',#14622,2.40538);
#12981=CYLINDRICAL_SURFACE('',#14623,2.40538);
#12982=CYLINDRICAL_SURFACE('',#14624,2.40538);
#12983=CYLINDRICAL_SURFACE('',#14625,2.40538);
#12984=CYLINDRICAL_SURFACE('',#14626,3.11023);
#12985=CYLINDRICAL_SURFACE('',#14629,2.40538);
#12986=CYLINDRICAL_SURFACE('',#14828,4.7625);
#12987=ADVANCED_FACE('',(#2027),#12861,.F.);
#12988=ADVANCED_FACE('',(#2028,#1484),#1565,.F.);
#12989=ADVANCED_FACE('',(#2029),#12862,.F.);
#12990=ADVANCED_FACE('',(#2030),#12863,.F.);
#12991=ADVANCED_FACE('',(#2031,#1485),#1566,.F.);
#12992=ADVANCED_FACE('',(#2032),#12864,.F.);
#12993=ADVANCED_FACE('',(#2033),#12865,.F.);
#12994=ADVANCED_FACE('',(#2034,#1486),#1567,.F.);
#12995=ADVANCED_FACE('',(#2035),#12866,.F.);
#12996=ADVANCED_FACE('',(#2036),#12867,.F.);
#12997=ADVANCED_FACE('',(#2037,#1487),#1568,.F.);
#12998=ADVANCED_FACE('',(#2038),#12868,.F.);
#12999=ADVANCED_FACE('',(#2039),#12869,.F.);
#13000=ADVANCED_FACE('',(#2040,#1488),#1569,.F.);
#13001=ADVANCED_FACE('',(#2041),#12870,.F.);
#13002=ADVANCED_FACE('',(#2042),#12871,.F.);
#13003=ADVANCED_FACE('',(#2043,#1489),#1570,.F.);
#13004=ADVANCED_FACE('',(#2044),#12872,.F.);
#13005=ADVANCED_FACE('',(#2045),#1053,.F.);
#13006=ADVANCED_FACE('',(#2046,#1490,#1491,#1492,#1493),#1571,.T.);
#13007=ADVANCED_FACE('',(#2047),#12873,.F.);
#13008=ADVANCED_FACE('',(#2048),#1054,.F.);
#13009=ADVANCED_FACE('',(#2049),#12874,.F.);
#13010=ADVANCED_FACE('',(#2050),#1055,.F.);
#13011=ADVANCED_FACE('',(#2051),#12875,.F.);
#13012=ADVANCED_FACE('',(#2052),#1056,.F.);
#13013=ADVANCED_FACE('',(#2053),#12876,.F.);
#13014=ADVANCED_FACE('',(#2054,#1494),#1572,.T.);
#13015=ADVANCED_FACE('',(#2055,#1495),#1573,.T.);
#13016=ADVANCED_FACE('',(#2056,#1496),#1574,.T.);
#13017=ADVANCED_FACE('',(#2057,#1497),#1575,.T.);
#13018=ADVANCED_FACE('',(#2058),#12877,.F.);
#13019=ADVANCED_FACE('',(#2059),#12878,.F.);
#13020=ADVANCED_FACE('',(#2060),#12879,.F.);
#13021=ADVANCED_FACE('',(#2061),#12880,.F.);
#13022=ADVANCED_FACE('',(#2062),#1576,.T.);
#13023=ADVANCED_FACE('',(#2063),#1577,.T.);
#13024=ADVANCED_FACE('',(#2064),#1578,.F.);
#13025=ADVANCED_FACE('',(#2065),#1579,.T.);
#13026=ADVANCED_FACE('',(#2066),#1580,.T.);
#13027=ADVANCED_FACE('',(#2067),#1581,.T.);
#13028=ADVANCED_FACE('',(#2068,#1498,#1499,#1500,#1501,#1502,#1503,#1504,
#1505,#1506,#1507),#1582,.T.);
#13029=ADVANCED_FACE('',(#2069),#1583,.T.);
#13030=ADVANCED_FACE('',(#2070,#1508,#1509,#1510),#12881,.F.);
#13031=ADVANCED_FACE('',(#2071),#1584,.T.);
#13032=ADVANCED_FACE('',(#2072),#1585,.T.);
#13033=ADVANCED_FACE('',(#2073),#1586,.T.);
#13034=ADVANCED_FACE('',(#2074),#1587,.T.);
#13035=ADVANCED_FACE('',(#2075,#1511,#1512,#1513),#12882,.F.);
#13036=ADVANCED_FACE('',(#2076),#1588,.T.);
#13037=ADVANCED_FACE('',(#2077),#1589,.T.);
#13038=ADVANCED_FACE('',(#2078),#1590,.T.);
#13039=ADVANCED_FACE('',(#2079),#1591,.T.);
#13040=ADVANCED_FACE('',(#2080),#1592,.T.);
#13041=ADVANCED_FACE('',(#2081),#1057,.F.);
#13042=ADVANCED_FACE('',(#2082,#1514,#1515,#1516,#1517,#1518,#1519,#1520,
#1521,#1522,#1523,#1524,#1525),#1593,.T.);
#13043=ADVANCED_FACE('',(#2083),#1058,.F.);
#13044=ADVANCED_FACE('',(#2084),#12883,.F.);
#13045=ADVANCED_FACE('',(#2085),#1059,.F.);
#13046=ADVANCED_FACE('',(#2086),#1060,.F.);
#13047=ADVANCED_FACE('',(#2087),#12884,.F.);
#13048=ADVANCED_FACE('',(#2088),#1061,.F.);
#13049=ADVANCED_FACE('',(#2089),#1062,.F.);
#13050=ADVANCED_FACE('',(#2090),#12885,.F.);
#13051=ADVANCED_FACE('',(#2091),#1063,.F.);
#13052=ADVANCED_FACE('',(#2092),#12886,.F.);
#13053=ADVANCED_FACE('',(#2093),#1064,.F.);
#13054=ADVANCED_FACE('',(#2094),#12887,.F.);
#13055=ADVANCED_FACE('',(#2095,#1526),#1594,.T.);
#13056=ADVANCED_FACE('',(#2096,#1527),#1595,.T.);
#13057=ADVANCED_FACE('',(#2097,#1528),#1596,.T.);
#13058=ADVANCED_FACE('',(#2098),#12888,.F.);
#13059=ADVANCED_FACE('',(#2099,#1529),#1597,.T.);
#13060=ADVANCED_FACE('',(#2100,#1530),#1598,.T.);
#13061=ADVANCED_FACE('',(#2101),#12889,.F.);
#13062=ADVANCED_FACE('',(#2102,#1531),#1599,.T.);
#13063=ADVANCED_FACE('',(#2103,#1532),#1600,.T.);
#13064=ADVANCED_FACE('',(#2104),#12890,.F.);
#13065=ADVANCED_FACE('',(#2105,#1533),#1601,.T.);
#13066=ADVANCED_FACE('',(#2106),#1065,.F.);
#13067=ADVANCED_FACE('',(#2107),#1066,.F.);
#13068=ADVANCED_FACE('',(#2108),#1067,.F.);
#13069=ADVANCED_FACE('',(#2109),#1068,.F.);
#13070=ADVANCED_FACE('',(#2110),#12891,.F.);
#13071=ADVANCED_FACE('',(#2111),#12892,.F.);
#13072=ADVANCED_FACE('',(#2112),#12893,.F.);
#13073=ADVANCED_FACE('',(#2113),#12894,.F.);
#13074=ADVANCED_FACE('',(#2114),#12895,.F.);
#13075=ADVANCED_FACE('',(#2115),#12896,.F.);
#13076=ADVANCED_FACE('',(#2116),#12897,.F.);
#13077=ADVANCED_FACE('',(#2117),#12898,.F.);
#13078=ADVANCED_FACE('',(#2118),#1069,.F.);
#13079=ADVANCED_FACE('',(#2119),#12899,.F.);
#13080=ADVANCED_FACE('',(#2120),#1070,.F.);
#13081=ADVANCED_FACE('',(#2121),#12900,.F.);
#13082=ADVANCED_FACE('',(#2122),#12901,.F.);
#13083=ADVANCED_FACE('',(#2123),#12902,.F.);
#13084=ADVANCED_FACE('',(#2124),#12903,.F.);
#13085=ADVANCED_FACE('',(#2125),#12904,.F.);
#13086=ADVANCED_FACE('',(#2126),#1071,.F.);
#13087=ADVANCED_FACE('',(#2127),#12905,.F.);
#13088=ADVANCED_FACE('',(#2128),#1072,.F.);
#13089=ADVANCED_FACE('',(#2129),#12906,.F.);
#13090=ADVANCED_FACE('',(#2130),#1073,.F.);
#13091=ADVANCED_FACE('',(#2131),#1074,.F.);
#13092=ADVANCED_FACE('',(#2132),#1075,.F.);
#13093=ADVANCED_FACE('',(#2133),#1076,.F.);
#13094=ADVANCED_FACE('',(#2134),#1077,.F.);
#13095=ADVANCED_FACE('',(#2135),#1078,.F.);
#13096=ADVANCED_FACE('',(#2136),#1079,.F.);
#13097=ADVANCED_FACE('',(#2137),#1080,.F.);
#13098=ADVANCED_FACE('',(#2138),#1602,.T.);
#13099=ADVANCED_FACE('',(#2139),#1603,.T.);
#13100=ADVANCED_FACE('',(#2140),#1604,.T.);
#13101=ADVANCED_FACE('',(#2141),#1605,.T.);
#13102=ADVANCED_FACE('',(#2142),#1606,.T.);
#13103=ADVANCED_FACE('',(#2143),#1607,.T.);
#13104=ADVANCED_FACE('',(#2144),#1608,.T.);
#13105=ADVANCED_FACE('',(#2145),#1609,.T.);
#13106=ADVANCED_FACE('',(#2146,#1534,#1535,#1536,#1537,#1538,#1539,#1540,
#1541),#1610,.F.);
#13107=ADVANCED_FACE('',(#2147),#12907,.F.);
#13108=ADVANCED_FACE('',(#2148),#1081,.F.);
#13109=ADVANCED_FACE('',(#2149),#12908,.F.);
#13110=ADVANCED_FACE('',(#2150),#1082,.F.);
#13111=ADVANCED_FACE('',(#2151),#12909,.F.);
#13112=ADVANCED_FACE('',(#2152),#1083,.F.);
#13113=ADVANCED_FACE('',(#2153),#1611,.T.);
#13114=ADVANCED_FACE('',(#2154),#1084,.T.);
#13115=ADVANCED_FACE('',(#2155,#1542,#1543,#1544),#12910,.T.);
#13116=ADVANCED_FACE('',(#2156),#1085,.T.);
#13117=ADVANCED_FACE('',(#2157),#1612,.T.);
#13118=ADVANCED_FACE('',(#2158),#1086,.F.);
#13119=ADVANCED_FACE('',(#2159,#1545,#1546),#1613,.T.);
#13120=ADVANCED_FACE('',(#2160),#12911,.F.);
#13121=ADVANCED_FACE('',(#2161),#1087,.F.);
#13122=ADVANCED_FACE('',(#2162),#12912,.F.);
#13123=ADVANCED_FACE('',(#2163),#1088,.F.);
#13124=ADVANCED_FACE('',(#2164,#1547,#1548),#12913,.F.);
#13125=ADVANCED_FACE('',(#2165),#1089,.F.);
#13126=ADVANCED_FACE('',(#2166),#1090,.F.);
#13127=ADVANCED_FACE('',(#2167),#1614,.T.);
#13128=ADVANCED_FACE('',(#2168),#1615,.T.);
#13129=ADVANCED_FACE('',(#2169),#1091,.F.);
#13130=ADVANCED_FACE('',(#2170),#1616,.F.);
#13131=ADVANCED_FACE('',(#2171),#1617,.T.);
#13132=ADVANCED_FACE('',(#2172),#1618,.T.);
#13133=ADVANCED_FACE('',(#2173),#1619,.T.);
#13134=ADVANCED_FACE('',(#2174),#1620,.T.);
#13135=ADVANCED_FACE('',(#2175),#1621,.T.);
#13136=ADVANCED_FACE('',(#2176),#1622,.T.);
#13137=ADVANCED_FACE('',(#2177),#1623,.T.);
#13138=ADVANCED_FACE('',(#2178),#1624,.F.);
#13139=ADVANCED_FACE('',(#2179),#1625,.F.);
#13140=ADVANCED_FACE('',(#2180),#1092,.T.);
#13141=ADVANCED_FACE('',(#2181),#1626,.T.);
#13142=ADVANCED_FACE('',(#2182),#12914,.F.);
#13143=ADVANCED_FACE('',(#2183),#1627,.T.);
#13144=ADVANCED_FACE('',(#2184),#1093,.T.);
#13145=ADVANCED_FACE('',(#2185),#12915,.T.);
#13146=ADVANCED_FACE('',(#2186),#1628,.F.);
#13147=ADVANCED_FACE('',(#2187),#1629,.T.);
#13148=ADVANCED_FACE('',(#2188),#1630,.F.);
#13149=ADVANCED_FACE('',(#2189),#1631,.F.);
#13150=ADVANCED_FACE('',(#2190),#1632,.F.);
#13151=ADVANCED_FACE('',(#2191),#1633,.T.);
#13152=ADVANCED_FACE('',(#2192),#1634,.F.);
#13153=ADVANCED_FACE('',(#2193),#1635,.F.);
#13154=ADVANCED_FACE('',(#2194),#1636,.F.);
#13155=ADVANCED_FACE('',(#2195),#1637,.T.);
#13156=ADVANCED_FACE('',(#2196),#1638,.F.);
#13157=ADVANCED_FACE('',(#2197),#1639,.F.);
#13158=ADVANCED_FACE('',(#2198),#1640,.F.);
#13159=ADVANCED_FACE('',(#2199),#1641,.T.);
#13160=ADVANCED_FACE('',(#2200),#1642,.F.);
#13161=ADVANCED_FACE('',(#2201),#1643,.F.);
#13162=ADVANCED_FACE('',(#2202),#1644,.F.);
#13163=ADVANCED_FACE('',(#2203),#1645,.T.);
#13164=ADVANCED_FACE('',(#2204),#1646,.F.);
#13165=ADVANCED_FACE('',(#2205),#1647,.F.);
#13166=ADVANCED_FACE('',(#2206),#1648,.F.);
#13167=ADVANCED_FACE('',(#2207),#1649,.F.);
#13168=ADVANCED_FACE('',(#2208),#1650,.T.);
#13169=ADVANCED_FACE('',(#2209,#1549,#1550,#1551,#1552,#1553),#12916,.T.);
#13170=ADVANCED_FACE('',(#2210,#1554,#1555,#1556,#1557,#1558),#12917,.F.);
#13171=ADVANCED_FACE('',(#2211),#1651,.T.);
#13172=ADVANCED_FACE('',(#2212),#1012,.T.);
#13173=ADVANCED_FACE('',(#2213),#12918,.T.);
#13174=ADVANCED_FACE('',(#2214),#12919,.T.);
#13175=ADVANCED_FACE('',(#2215),#12920,.T.);
#13176=ADVANCED_FACE('',(#2216),#12921,.T.);
#13177=ADVANCED_FACE('',(#2217),#12922,.T.);
#13178=ADVANCED_FACE('',(#2218),#12923,.T.);
#13179=ADVANCED_FACE('',(#2219),#12924,.T.);
#13180=ADVANCED_FACE('',(#2220),#12925,.T.);
#13181=ADVANCED_FACE('',(#2221),#12926,.T.);
#13182=ADVANCED_FACE('',(#2222),#12927,.T.);
#13183=ADVANCED_FACE('',(#2223),#12928,.T.);
#13184=ADVANCED_FACE('',(#2224),#12929,.T.);
#13185=ADVANCED_FACE('',(#2225),#12930,.T.);
#13186=ADVANCED_FACE('',(#2226),#12931,.T.);
#13187=ADVANCED_FACE('',(#2227),#12932,.T.);
#13188=ADVANCED_FACE('',(#2228),#12933,.T.);
#13189=ADVANCED_FACE('',(#2229),#12934,.T.);
#13190=ADVANCED_FACE('',(#2230),#12935,.T.);
#13191=ADVANCED_FACE('',(#2231),#12936,.T.);
#13192=ADVANCED_FACE('',(#2232),#12937,.T.);
#13193=ADVANCED_FACE('',(#2233),#12938,.T.);
#13194=ADVANCED_FACE('',(#2234),#1652,.T.);
#13195=ADVANCED_FACE('',(#2235),#1006,.F.);
#13196=ADVANCED_FACE('',(#2236),#1653,.F.);
#13197=ADVANCED_FACE('',(#2237),#1007,.F.);
#13198=ADVANCED_FACE('',(#2238),#1003,.F.);
#13199=ADVANCED_FACE('',(#2239,#1559),#1654,.F.);
#13200=ADVANCED_FACE('',(#2240),#1094,.T.);
#13201=ADVANCED_FACE('',(#2241),#1655,.F.);
#13202=ADVANCED_FACE('',(#2242),#1656,.F.);
#13203=ADVANCED_FACE('',(#2243),#1657,.F.);
#13204=ADVANCED_FACE('',(#2244),#1658,.F.);
#13205=ADVANCED_FACE('',(#2245),#1095,.T.);
#13206=ADVANCED_FACE('',(#2246),#1659,.F.);
#13207=ADVANCED_FACE('',(#2247),#1660,.F.);
#13208=ADVANCED_FACE('',(#2248),#1661,.F.);
#13209=ADVANCED_FACE('',(#2249),#1662,.F.);
#13210=ADVANCED_FACE('',(#2250),#1663,.F.);
#13211=ADVANCED_FACE('',(#2251),#1664,.F.);
#13212=ADVANCED_FACE('',(#2252),#1665,.F.);
#13213=ADVANCED_FACE('',(#2253),#1666,.F.);
#13214=ADVANCED_FACE('',(#2254),#1667,.F.);
#13215=ADVANCED_FACE('',(#2255),#1668,.F.);
#13216=ADVANCED_FACE('',(#2256),#1669,.F.);
#13217=ADVANCED_FACE('',(#2257),#1670,.F.);
#13218=ADVANCED_FACE('',(#2258),#1671,.F.);
#13219=ADVANCED_FACE('',(#2259),#1672,.F.);
#13220=ADVANCED_FACE('',(#2260),#1673,.F.);
#13221=ADVANCED_FACE('',(#2261),#1674,.F.);
#13222=ADVANCED_FACE('',(#2262),#1675,.F.);
#13223=ADVANCED_FACE('',(#2263),#1676,.F.);
#13224=ADVANCED_FACE('',(#2264),#1677,.F.);
#13225=ADVANCED_FACE('',(#2265),#1678,.F.);
#13226=ADVANCED_FACE('',(#2266),#1679,.F.);
#13227=ADVANCED_FACE('',(#2267),#1680,.F.);
#13228=ADVANCED_FACE('',(#2268),#1681,.F.);
#13229=ADVANCED_FACE('',(#2269),#1682,.F.);
#13230=ADVANCED_FACE('',(#2270),#1683,.F.);
#13231=ADVANCED_FACE('',(#2271),#1684,.F.);
#13232=ADVANCED_FACE('',(#2272),#1685,.F.);
#13233=ADVANCED_FACE('',(#2273),#1686,.F.);
#13234=ADVANCED_FACE('',(#2274),#1687,.F.);
#13235=ADVANCED_FACE('',(#2275),#1688,.F.);
#13236=ADVANCED_FACE('',(#2276),#1689,.F.);
#13237=ADVANCED_FACE('',(#2277),#1690,.F.);
#13238=ADVANCED_FACE('',(#2278),#1691,.F.);
#13239=ADVANCED_FACE('',(#2279),#1692,.F.);
#13240=ADVANCED_FACE('',(#2280),#1693,.F.);
#13241=ADVANCED_FACE('',(#2281),#1694,.F.);
#13242=ADVANCED_FACE('',(#2282),#1695,.F.);
#13243=ADVANCED_FACE('',(#2283),#1696,.F.);
#13244=ADVANCED_FACE('',(#2284),#1697,.F.);
#13245=ADVANCED_FACE('',(#2285),#1698,.F.);
#13246=ADVANCED_FACE('',(#2286),#1699,.F.);
#13247=ADVANCED_FACE('',(#2287),#1700,.F.);
#13248=ADVANCED_FACE('',(#2288),#1701,.F.);
#13249=ADVANCED_FACE('',(#2289),#1702,.F.);
#13250=ADVANCED_FACE('',(#2290),#1703,.F.);
#13251=ADVANCED_FACE('',(#2291),#1704,.F.);
#13252=ADVANCED_FACE('',(#2292),#1705,.F.);
#13253=ADVANCED_FACE('',(#2293),#1706,.F.);
#13254=ADVANCED_FACE('',(#2294),#1707,.F.);
#13255=ADVANCED_FACE('',(#2295),#1708,.F.);
#13256=ADVANCED_FACE('',(#2296),#1709,.F.);
#13257=ADVANCED_FACE('',(#2297),#1710,.F.);
#13258=ADVANCED_FACE('',(#2298),#1711,.F.);
#13259=ADVANCED_FACE('',(#2299),#1712,.F.);
#13260=ADVANCED_FACE('',(#2300),#1713,.F.);
#13261=ADVANCED_FACE('',(#2301),#1714,.F.);
#13262=ADVANCED_FACE('',(#2302),#1715,.F.);
#13263=ADVANCED_FACE('',(#2303),#1716,.F.);
#13264=ADVANCED_FACE('',(#2304),#1717,.F.);
#13265=ADVANCED_FACE('',(#2305),#1718,.F.);
#13266=ADVANCED_FACE('',(#2306),#1719,.F.);
#13267=ADVANCED_FACE('',(#2307),#1720,.F.);
#13268=ADVANCED_FACE('',(#2308),#1721,.F.);
#13269=ADVANCED_FACE('',(#2309),#1722,.F.);
#13270=ADVANCED_FACE('',(#2310),#1723,.F.);
#13271=ADVANCED_FACE('',(#2311),#1724,.F.);
#13272=ADVANCED_FACE('',(#2312),#1725,.F.);
#13273=ADVANCED_FACE('',(#2313),#1726,.F.);
#13274=ADVANCED_FACE('',(#2314),#1727,.F.);
#13275=ADVANCED_FACE('',(#2315),#1728,.F.);
#13276=ADVANCED_FACE('',(#2316),#1729,.F.);
#13277=ADVANCED_FACE('',(#2317),#1730,.F.);
#13278=ADVANCED_FACE('',(#2318),#1731,.F.);
#13279=ADVANCED_FACE('',(#2319),#1732,.F.);
#13280=ADVANCED_FACE('',(#2320),#1733,.F.);
#13281=ADVANCED_FACE('',(#2321),#1734,.F.);
#13282=ADVANCED_FACE('',(#2322),#1735,.F.);
#13283=ADVANCED_FACE('',(#2323),#1736,.F.);
#13284=ADVANCED_FACE('',(#2324),#1737,.F.);
#13285=ADVANCED_FACE('',(#2325),#1738,.F.);
#13286=ADVANCED_FACE('',(#2326),#1739,.F.);
#13287=ADVANCED_FACE('',(#2327),#1740,.F.);
#13288=ADVANCED_FACE('',(#2328),#1741,.F.);
#13289=ADVANCED_FACE('',(#2329),#1742,.F.);
#13290=ADVANCED_FACE('',(#2330),#1743,.F.);
#13291=ADVANCED_FACE('',(#2331),#1744,.F.);
#13292=ADVANCED_FACE('',(#2332),#1745,.F.);
#13293=ADVANCED_FACE('',(#2333),#1746,.F.);
#13294=ADVANCED_FACE('',(#2334),#1747,.F.);
#13295=ADVANCED_FACE('',(#2335),#1748,.F.);
#13296=ADVANCED_FACE('',(#2336),#1749,.F.);
#13297=ADVANCED_FACE('',(#2337),#1750,.F.);
#13298=ADVANCED_FACE('',(#2338),#1751,.F.);
#13299=ADVANCED_FACE('',(#2339),#1752,.F.);
#13300=ADVANCED_FACE('',(#2340),#1753,.F.);
#13301=ADVANCED_FACE('',(#2341),#1754,.F.);
#13302=ADVANCED_FACE('',(#2342),#1755,.F.);
#13303=ADVANCED_FACE('',(#2343),#1756,.F.);
#13304=ADVANCED_FACE('',(#2344),#1757,.F.);
#13305=ADVANCED_FACE('',(#2345),#1758,.F.);
#13306=ADVANCED_FACE('',(#2346),#1759,.F.);
#13307=ADVANCED_FACE('',(#2347),#1760,.F.);
#13308=ADVANCED_FACE('',(#2348),#1761,.F.);
#13309=ADVANCED_FACE('',(#2349),#1762,.F.);
#13310=ADVANCED_FACE('',(#2350),#1763,.F.);
#13311=ADVANCED_FACE('',(#2351),#12939,.T.);
#13312=ADVANCED_FACE('',(#2352,#1560),#1764,.T.);
#13313=ADVANCED_FACE('',(#2353),#1765,.F.);
#13314=ADVANCED_FACE('',(#2354),#1766,.F.);
#13315=ADVANCED_FACE('',(#2355),#1767,.F.);
#13316=ADVANCED_FACE('',(#2356),#1768,.F.);
#13317=ADVANCED_FACE('',(#2357),#1769,.F.);
#13318=ADVANCED_FACE('',(#2358),#1770,.F.);
#13319=ADVANCED_FACE('',(#2359),#1096,.F.);
#13320=ADVANCED_FACE('',(#2360),#1771,.F.);
#13321=ADVANCED_FACE('',(#2361),#1772,.F.);
#13322=ADVANCED_FACE('',(#2362),#1773,.F.);
#13323=ADVANCED_FACE('',(#2363),#1774,.F.);
#13324=ADVANCED_FACE('',(#2364),#1775,.F.);
#13325=ADVANCED_FACE('',(#2365),#1776,.F.);
#13326=ADVANCED_FACE('',(#2366),#12940,.T.);
#13327=ADVANCED_FACE('',(#2367),#12941,.T.);
#13328=ADVANCED_FACE('',(#2368),#12942,.T.);
#13329=ADVANCED_FACE('',(#2369),#12943,.T.);
#13330=ADVANCED_FACE('',(#2370),#12944,.T.);
#13331=ADVANCED_FACE('',(#2371),#12945,.T.);
#13332=ADVANCED_FACE('',(#2372),#12946,.T.);
#13333=ADVANCED_FACE('',(#2373),#12947,.T.);
#13334=ADVANCED_FACE('',(#2374),#12948,.T.);
#13335=ADVANCED_FACE('',(#2375),#12949,.T.);
#13336=ADVANCED_FACE('',(#2376),#12950,.T.);
#13337=ADVANCED_FACE('',(#2377),#12951,.T.);
#13338=ADVANCED_FACE('',(#2378),#12952,.T.);
#13339=ADVANCED_FACE('',(#2379),#12953,.T.);
#13340=ADVANCED_FACE('',(#2380),#12954,.T.);
#13341=ADVANCED_FACE('',(#2381),#12955,.T.);
#13342=ADVANCED_FACE('',(#2382),#12956,.T.);
#13343=ADVANCED_FACE('',(#2383),#12957,.T.);
#13344=ADVANCED_FACE('',(#2384),#12958,.T.);
#13345=ADVANCED_FACE('',(#2385),#12959,.T.);
#13346=ADVANCED_FACE('',(#2386),#12960,.T.);
#13347=ADVANCED_FACE('',(#2387),#12961,.T.);
#13348=ADVANCED_FACE('',(#2388),#12962,.T.);
#13349=ADVANCED_FACE('',(#2389),#12963,.T.);
#13350=ADVANCED_FACE('',(#2390),#12964,.T.);
#13351=ADVANCED_FACE('',(#2391),#12965,.T.);
#13352=ADVANCED_FACE('',(#2392),#12966,.T.);
#13353=ADVANCED_FACE('',(#2393),#12967,.T.);
#13354=ADVANCED_FACE('',(#2394),#12968,.T.);
#13355=ADVANCED_FACE('',(#2395),#1777,.F.);
#13356=ADVANCED_FACE('',(#2396),#1008,.F.);
#13357=ADVANCED_FACE('',(#2397),#1778,.T.);
#13358=ADVANCED_FACE('',(#2398),#1009,.F.);
#13359=ADVANCED_FACE('',(#2399),#1004,.F.);
#13360=ADVANCED_FACE('',(#2400,#1561),#1779,.T.);
#13361=ADVANCED_FACE('',(#2401),#1097,.T.);
#13362=ADVANCED_FACE('',(#2402),#1780,.T.);
#13363=ADVANCED_FACE('',(#2403),#1781,.F.);
#13364=ADVANCED_FACE('',(#2404),#1782,.F.);
#13365=ADVANCED_FACE('',(#2405),#1783,.F.);
#13366=ADVANCED_FACE('',(#2406),#1098,.T.);
#13367=ADVANCED_FACE('',(#2407),#1784,.F.);
#13368=ADVANCED_FACE('',(#2408),#1785,.F.);
#13369=ADVANCED_FACE('',(#2409),#1786,.F.);
#13370=ADVANCED_FACE('',(#2410),#12969,.T.);
#13371=ADVANCED_FACE('',(#2411),#1787,.F.);
#13372=ADVANCED_FACE('',(#2412),#1788,.F.);
#13373=ADVANCED_FACE('',(#2413),#1789,.F.);
#13374=ADVANCED_FACE('',(#2414),#1790,.F.);
#13375=ADVANCED_FACE('',(#2415),#1791,.F.);
#13376=ADVANCED_FACE('',(#2416),#1792,.F.);
#13377=ADVANCED_FACE('',(#2417),#1793,.F.);
#13378=ADVANCED_FACE('',(#2418),#1794,.F.);
#13379=ADVANCED_FACE('',(#2419),#1795,.F.);
#13380=ADVANCED_FACE('',(#2420),#1796,.F.);
#13381=ADVANCED_FACE('',(#2421),#1797,.F.);
#13382=ADVANCED_FACE('',(#2422),#1798,.F.);
#13383=ADVANCED_FACE('',(#2423),#1799,.F.);
#13384=ADVANCED_FACE('',(#2424),#1800,.F.);
#13385=ADVANCED_FACE('',(#2425),#1801,.F.);
#13386=ADVANCED_FACE('',(#2426),#1802,.F.);
#13387=ADVANCED_FACE('',(#2427),#1803,.F.);
#13388=ADVANCED_FACE('',(#2428),#1804,.F.);
#13389=ADVANCED_FACE('',(#2429),#1805,.F.);
#13390=ADVANCED_FACE('',(#2430),#1806,.F.);
#13391=ADVANCED_FACE('',(#2431),#1807,.F.);
#13392=ADVANCED_FACE('',(#2432),#1808,.F.);
#13393=ADVANCED_FACE('',(#2433),#1809,.F.);
#13394=ADVANCED_FACE('',(#2434),#1810,.F.);
#13395=ADVANCED_FACE('',(#2435),#1811,.F.);
#13396=ADVANCED_FACE('',(#2436),#1812,.F.);
#13397=ADVANCED_FACE('',(#2437),#1813,.F.);
#13398=ADVANCED_FACE('',(#2438),#1814,.F.);
#13399=ADVANCED_FACE('',(#2439),#1815,.F.);
#13400=ADVANCED_FACE('',(#2440),#1816,.F.);
#13401=ADVANCED_FACE('',(#2441),#1817,.F.);
#13402=ADVANCED_FACE('',(#2442),#1818,.F.);
#13403=ADVANCED_FACE('',(#2443),#1819,.F.);
#13404=ADVANCED_FACE('',(#2444),#1820,.F.);
#13405=ADVANCED_FACE('',(#2445),#1821,.F.);
#13406=ADVANCED_FACE('',(#2446),#1822,.F.);
#13407=ADVANCED_FACE('',(#2447),#1823,.F.);
#13408=ADVANCED_FACE('',(#2448),#1824,.F.);
#13409=ADVANCED_FACE('',(#2449),#1825,.F.);
#13410=ADVANCED_FACE('',(#2450),#1826,.F.);
#13411=ADVANCED_FACE('',(#2451),#1827,.F.);
#13412=ADVANCED_FACE('',(#2452),#1828,.F.);
#13413=ADVANCED_FACE('',(#2453),#1829,.F.);
#13414=ADVANCED_FACE('',(#2454),#1830,.F.);
#13415=ADVANCED_FACE('',(#2455),#1831,.F.);
#13416=ADVANCED_FACE('',(#2456),#1832,.F.);
#13417=ADVANCED_FACE('',(#2457),#1833,.F.);
#13418=ADVANCED_FACE('',(#2458),#1834,.F.);
#13419=ADVANCED_FACE('',(#2459),#1835,.F.);
#13420=ADVANCED_FACE('',(#2460),#1836,.F.);
#13421=ADVANCED_FACE('',(#2461),#1837,.F.);
#13422=ADVANCED_FACE('',(#2462),#1838,.F.);
#13423=ADVANCED_FACE('',(#2463),#1839,.F.);
#13424=ADVANCED_FACE('',(#2464),#1840,.F.);
#13425=ADVANCED_FACE('',(#2465),#1841,.F.);
#13426=ADVANCED_FACE('',(#2466),#1842,.F.);
#13427=ADVANCED_FACE('',(#2467),#1843,.F.);
#13428=ADVANCED_FACE('',(#2468),#1844,.F.);
#13429=ADVANCED_FACE('',(#2469),#1845,.F.);
#13430=ADVANCED_FACE('',(#2470),#1846,.F.);
#13431=ADVANCED_FACE('',(#2471),#1847,.F.);
#13432=ADVANCED_FACE('',(#2472),#1848,.F.);
#13433=ADVANCED_FACE('',(#2473),#1849,.F.);
#13434=ADVANCED_FACE('',(#2474),#1850,.F.);
#13435=ADVANCED_FACE('',(#2475),#1851,.F.);
#13436=ADVANCED_FACE('',(#2476),#1852,.F.);
#13437=ADVANCED_FACE('',(#2477),#1853,.F.);
#13438=ADVANCED_FACE('',(#2478),#1854,.F.);
#13439=ADVANCED_FACE('',(#2479),#1855,.F.);
#13440=ADVANCED_FACE('',(#2480),#1856,.F.);
#13441=ADVANCED_FACE('',(#2481),#1857,.F.);
#13442=ADVANCED_FACE('',(#2482),#1858,.F.);
#13443=ADVANCED_FACE('',(#2483),#1859,.F.);
#13444=ADVANCED_FACE('',(#2484),#1860,.F.);
#13445=ADVANCED_FACE('',(#2485),#1861,.F.);
#13446=ADVANCED_FACE('',(#2486),#1862,.F.);
#13447=ADVANCED_FACE('',(#2487),#1863,.F.);
#13448=ADVANCED_FACE('',(#2488),#1864,.F.);
#13449=ADVANCED_FACE('',(#2489),#1865,.F.);
#13450=ADVANCED_FACE('',(#2490),#1866,.F.);
#13451=ADVANCED_FACE('',(#2491),#1867,.F.);
#13452=ADVANCED_FACE('',(#2492),#1868,.F.);
#13453=ADVANCED_FACE('',(#2493),#1869,.F.);
#13454=ADVANCED_FACE('',(#2494),#1870,.F.);
#13455=ADVANCED_FACE('',(#2495),#1871,.F.);
#13456=ADVANCED_FACE('',(#2496),#1872,.F.);
#13457=ADVANCED_FACE('',(#2497),#1873,.F.);
#13458=ADVANCED_FACE('',(#2498),#1874,.F.);
#13459=ADVANCED_FACE('',(#2499),#1875,.F.);
#13460=ADVANCED_FACE('',(#2500),#1876,.F.);
#13461=ADVANCED_FACE('',(#2501),#1877,.F.);
#13462=ADVANCED_FACE('',(#2502),#1878,.F.);
#13463=ADVANCED_FACE('',(#2503),#1879,.F.);
#13464=ADVANCED_FACE('',(#2504),#1880,.F.);
#13465=ADVANCED_FACE('',(#2505),#1881,.F.);
#13466=ADVANCED_FACE('',(#2506),#1882,.F.);
#13467=ADVANCED_FACE('',(#2507),#1883,.F.);
#13468=ADVANCED_FACE('',(#2508),#1884,.F.);
#13469=ADVANCED_FACE('',(#2509),#1885,.F.);
#13470=ADVANCED_FACE('',(#2510),#1886,.F.);
#13471=ADVANCED_FACE('',(#2511),#1887,.F.);
#13472=ADVANCED_FACE('',(#2512),#1888,.F.);
#13473=ADVANCED_FACE('',(#2513,#1562),#1889,.F.);
#13474=ADVANCED_FACE('',(#2514),#1890,.F.);
#13475=ADVANCED_FACE('',(#2515),#1891,.F.);
#13476=ADVANCED_FACE('',(#2516),#1892,.F.);
#13477=ADVANCED_FACE('',(#2517),#1893,.F.);
#13478=ADVANCED_FACE('',(#2518),#1894,.F.);
#13479=ADVANCED_FACE('',(#2519),#1895,.F.);
#13480=ADVANCED_FACE('',(#2520),#1099,.F.);
#13481=ADVANCED_FACE('',(#2521),#1896,.F.);
#13482=ADVANCED_FACE('',(#2522),#1897,.F.);
#13483=ADVANCED_FACE('',(#2523),#1898,.F.);
#13484=ADVANCED_FACE('',(#2524),#1899,.F.);
#13485=ADVANCED_FACE('',(#2525),#1900,.F.);
#13486=ADVANCED_FACE('',(#2526),#1901,.F.);
#13487=ADVANCED_FACE('',(#2527),#12970,.T.);
#13488=ADVANCED_FACE('',(#2528),#12971,.T.);
#13489=ADVANCED_FACE('',(#2529),#12972,.T.);
#13490=ADVANCED_FACE('',(#2530),#12973,.T.);
#13491=ADVANCED_FACE('',(#2531),#12974,.T.);
#13492=ADVANCED_FACE('',(#2532),#12975,.T.);
#13493=ADVANCED_FACE('',(#2533),#12976,.T.);
#13494=ADVANCED_FACE('',(#2534),#12977,.T.);
#13495=ADVANCED_FACE('',(#2535),#12978,.T.);
#13496=ADVANCED_FACE('',(#2536),#12979,.T.);
#13497=ADVANCED_FACE('',(#2537),#12980,.T.);
#13498=ADVANCED_FACE('',(#2538),#12981,.T.);
#13499=ADVANCED_FACE('',(#2539),#12982,.T.);
#13500=ADVANCED_FACE('',(#2540),#12983,.T.);
#13501=ADVANCED_FACE('',(#2541),#12984,.T.);
#13502=ADVANCED_FACE('',(#2542),#12985,.T.);
#13503=ADVANCED_FACE('',(#2543),#1902,.T.);
#13504=ADVANCED_FACE('',(#2544),#1010,.F.);
#13505=ADVANCED_FACE('',(#2545),#1903,.F.);
#13506=ADVANCED_FACE('',(#2546),#1011,.F.);
#13507=ADVANCED_FACE('',(#2547),#1005,.F.);
#13508=ADVANCED_FACE('',(#2548,#1563),#1904,.F.);
#13509=ADVANCED_FACE('',(#2549),#1100,.T.);
#13510=ADVANCED_FACE('',(#2550),#1905,.F.);
#13511=ADVANCED_FACE('',(#2551),#1906,.F.);
#13512=ADVANCED_FACE('',(#2552),#1907,.F.);
#13513=ADVANCED_FACE('',(#2553),#1908,.F.);
#13514=ADVANCED_FACE('',(#2554),#1101,.T.);
#13515=ADVANCED_FACE('',(#2555),#1909,.F.);
#13516=ADVANCED_FACE('',(#2556),#1910,.F.);
#13517=ADVANCED_FACE('',(#2557),#1911,.F.);
#13518=ADVANCED_FACE('',(#2558),#1912,.F.);
#13519=ADVANCED_FACE('',(#2559),#1913,.F.);
#13520=ADVANCED_FACE('',(#2560),#1914,.F.);
#13521=ADVANCED_FACE('',(#2561),#1915,.F.);
#13522=ADVANCED_FACE('',(#2562),#1916,.F.);
#13523=ADVANCED_FACE('',(#2563),#1917,.F.);
#13524=ADVANCED_FACE('',(#2564),#1918,.F.);
#13525=ADVANCED_FACE('',(#2565),#1919,.F.);
#13526=ADVANCED_FACE('',(#2566),#1920,.F.);
#13527=ADVANCED_FACE('',(#2567),#1921,.F.);
#13528=ADVANCED_FACE('',(#2568),#1922,.F.);
#13529=ADVANCED_FACE('',(#2569),#1923,.F.);
#13530=ADVANCED_FACE('',(#2570),#1924,.F.);
#13531=ADVANCED_FACE('',(#2571),#1925,.F.);
#13532=ADVANCED_FACE('',(#2572),#1926,.F.);
#13533=ADVANCED_FACE('',(#2573),#1927,.F.);
#13534=ADVANCED_FACE('',(#2574),#1928,.F.);
#13535=ADVANCED_FACE('',(#2575),#1929,.F.);
#13536=ADVANCED_FACE('',(#2576),#1930,.F.);
#13537=ADVANCED_FACE('',(#2577),#1931,.F.);
#13538=ADVANCED_FACE('',(#2578),#1932,.F.);
#13539=ADVANCED_FACE('',(#2579),#1933,.F.);
#13540=ADVANCED_FACE('',(#2580),#1934,.F.);
#13541=ADVANCED_FACE('',(#2581),#1935,.F.);
#13542=ADVANCED_FACE('',(#2582),#1936,.F.);
#13543=ADVANCED_FACE('',(#2583),#1937,.F.);
#13544=ADVANCED_FACE('',(#2584),#1938,.F.);
#13545=ADVANCED_FACE('',(#2585),#1939,.F.);
#13546=ADVANCED_FACE('',(#2586),#1940,.F.);
#13547=ADVANCED_FACE('',(#2587),#1941,.F.);
#13548=ADVANCED_FACE('',(#2588),#1942,.F.);
#13549=ADVANCED_FACE('',(#2589),#1943,.F.);
#13550=ADVANCED_FACE('',(#2590),#1944,.F.);
#13551=ADVANCED_FACE('',(#2591),#1945,.F.);
#13552=ADVANCED_FACE('',(#2592),#1946,.F.);
#13553=ADVANCED_FACE('',(#2593),#1947,.F.);
#13554=ADVANCED_FACE('',(#2594),#1948,.F.);
#13555=ADVANCED_FACE('',(#2595),#1949,.F.);
#13556=ADVANCED_FACE('',(#2596),#1950,.F.);
#13557=ADVANCED_FACE('',(#2597),#1951,.F.);
#13558=ADVANCED_FACE('',(#2598),#1952,.F.);
#13559=ADVANCED_FACE('',(#2599),#1953,.F.);
#13560=ADVANCED_FACE('',(#2600),#1954,.F.);
#13561=ADVANCED_FACE('',(#2601),#1955,.F.);
#13562=ADVANCED_FACE('',(#2602),#1956,.F.);
#13563=ADVANCED_FACE('',(#2603),#1957,.F.);
#13564=ADVANCED_FACE('',(#2604),#1958,.F.);
#13565=ADVANCED_FACE('',(#2605),#1959,.F.);
#13566=ADVANCED_FACE('',(#2606),#1960,.F.);
#13567=ADVANCED_FACE('',(#2607),#1961,.F.);
#13568=ADVANCED_FACE('',(#2608),#1962,.F.);
#13569=ADVANCED_FACE('',(#2609),#1963,.F.);
#13570=ADVANCED_FACE('',(#2610),#1964,.F.);
#13571=ADVANCED_FACE('',(#2611),#1965,.F.);
#13572=ADVANCED_FACE('',(#2612),#1966,.F.);
#13573=ADVANCED_FACE('',(#2613),#1967,.F.);
#13574=ADVANCED_FACE('',(#2614),#1968,.F.);
#13575=ADVANCED_FACE('',(#2615),#1969,.F.);
#13576=ADVANCED_FACE('',(#2616),#1970,.F.);
#13577=ADVANCED_FACE('',(#2617),#1971,.F.);
#13578=ADVANCED_FACE('',(#2618),#1972,.F.);
#13579=ADVANCED_FACE('',(#2619),#1973,.F.);
#13580=ADVANCED_FACE('',(#2620),#1974,.F.);
#13581=ADVANCED_FACE('',(#2621),#1975,.F.);
#13582=ADVANCED_FACE('',(#2622),#1976,.F.);
#13583=ADVANCED_FACE('',(#2623),#1977,.F.);
#13584=ADVANCED_FACE('',(#2624),#1978,.F.);
#13585=ADVANCED_FACE('',(#2625),#1979,.F.);
#13586=ADVANCED_FACE('',(#2626),#1980,.F.);
#13587=ADVANCED_FACE('',(#2627),#1981,.F.);
#13588=ADVANCED_FACE('',(#2628),#1982,.F.);
#13589=ADVANCED_FACE('',(#2629),#1983,.F.);
#13590=ADVANCED_FACE('',(#2630),#1984,.F.);
#13591=ADVANCED_FACE('',(#2631),#1985,.F.);
#13592=ADVANCED_FACE('',(#2632),#1986,.F.);
#13593=ADVANCED_FACE('',(#2633),#1987,.F.);
#13594=ADVANCED_FACE('',(#2634),#1988,.F.);
#13595=ADVANCED_FACE('',(#2635),#1989,.F.);
#13596=ADVANCED_FACE('',(#2636),#1990,.F.);
#13597=ADVANCED_FACE('',(#2637),#1991,.F.);
#13598=ADVANCED_FACE('',(#2638),#1992,.F.);
#13599=ADVANCED_FACE('',(#2639),#1993,.F.);
#13600=ADVANCED_FACE('',(#2640),#1994,.F.);
#13601=ADVANCED_FACE('',(#2641),#1995,.F.);
#13602=ADVANCED_FACE('',(#2642),#1996,.F.);
#13603=ADVANCED_FACE('',(#2643),#1997,.F.);
#13604=ADVANCED_FACE('',(#2644),#1998,.F.);
#13605=ADVANCED_FACE('',(#2645),#1999,.F.);
#13606=ADVANCED_FACE('',(#2646),#2000,.F.);
#13607=ADVANCED_FACE('',(#2647),#2001,.F.);
#13608=ADVANCED_FACE('',(#2648),#2002,.F.);
#13609=ADVANCED_FACE('',(#2649),#2003,.F.);
#13610=ADVANCED_FACE('',(#2650),#2004,.F.);
#13611=ADVANCED_FACE('',(#2651),#2005,.F.);
#13612=ADVANCED_FACE('',(#2652),#2006,.F.);
#13613=ADVANCED_FACE('',(#2653),#2007,.F.);
#13614=ADVANCED_FACE('',(#2654),#2008,.F.);
#13615=ADVANCED_FACE('',(#2655),#2009,.F.);
#13616=ADVANCED_FACE('',(#2656),#2010,.F.);
#13617=ADVANCED_FACE('',(#2657),#2011,.F.);
#13618=ADVANCED_FACE('',(#2658),#2012,.F.);
#13619=ADVANCED_FACE('',(#2659),#2013,.F.);
#13620=ADVANCED_FACE('',(#2660),#12986,.T.);
#13621=ADVANCED_FACE('',(#2661,#1564),#2014,.T.);
#13622=ADVANCED_FACE('',(#2662),#2015,.F.);
#13623=ADVANCED_FACE('',(#2663),#2016,.F.);
#13624=ADVANCED_FACE('',(#2664),#2017,.F.);
#13625=ADVANCED_FACE('',(#2665),#2018,.F.);
#13626=ADVANCED_FACE('',(#2666),#2019,.F.);
#13627=ADVANCED_FACE('',(#2667),#2020,.F.);
#13628=ADVANCED_FACE('',(#2668),#1102,.F.);
#13629=ADVANCED_FACE('',(#2669),#2021,.F.);
#13630=ADVANCED_FACE('',(#2670),#2022,.F.);
#13631=ADVANCED_FACE('',(#2671),#2023,.F.);
#13632=ADVANCED_FACE('',(#2672),#2024,.F.);
#13633=ADVANCED_FACE('',(#2673),#2025,.F.);
#13634=ADVANCED_FACE('',(#2674),#2026,.F.);
#13635=CLOSED_SHELL('',(#12987,#12988,#12989,#12990,#12991,#12992,#12993,
#12994,#12995,#12996,#12997,#12998,#12999,#13000,#13001,#13002,#13003,#13004,
#13005,#13006,#13007,#13008,#13009,#13010,#13011,#13012,#13013,#13014,#13015,
#13016,#13017,#13018,#13019,#13020,#13021,#13022,#13023,#13024,#13025,#13026,
#13027,#13028,#13029,#13030,#13031,#13032,#13033,#13034,#13035,#13036,#13037,
#13038,#13039,#13040));
#13636=CLOSED_SHELL('',(#13041,#13042,#13043,#13044,#13045,#13046,#13047,
#13048,#13049,#13050,#13051,#13052,#13053,#13054,#13055,#13056,#13057,#13058,
#13059,#13060,#13061,#13062,#13063,#13064,#13065,#13066,#13067,#13068,#13069,
#13070,#13071,#13072,#13073,#13074,#13075,#13076,#13077,#13078,#13079,#13080,
#13081,#13082,#13083,#13084,#13085,#13086,#13087,#13088,#13089,#13090,#13091,
#13092,#13093,#13094,#13095,#13096,#13097,#13098,#13099,#13100,#13101,#13102,
#13103,#13104,#13105,#13106));
#13637=CLOSED_SHELL('',(#13107,#13108,#13109,#13110,#13111,#13112,#13113,
#13114,#13115,#13116,#13117));
#13638=CLOSED_SHELL('',(#13118,#13119,#13120,#13121,#13122,#13123,#13124,
#13125,#13126,#13127,#13128,#13129,#13130,#13131,#13132,#13133,#13134,#13135,
#13136,#13137));
#13639=CLOSED_SHELL('',(#13138,#13139,#13140,#13141,#13142,#13143,#13144,
#13145));
#13640=CLOSED_SHELL('',(#13146,#13147,#13148,#13149,#13150,#13151,#13152,
#13153,#13154,#13155,#13156,#13157,#13158,#13159,#13160,#13161,#13162,#13163,
#13164,#13165,#13166,#13167,#13168,#13169,#13170,#13171));
#13641=CLOSED_SHELL('',(#13172));
#13642=CLOSED_SHELL('',(#13173,#13174,#13175,#13176,#13177,#13178,#13179,
#13180,#13181,#13182,#13183,#13184,#13185,#13186,#13187,#13188,#13189,#13190,
#13191,#13192,#13193,#13194,#13195,#13196,#13197,#13198,#13199,#13200,#13201,
#13202,#13203,#13204,#13205,#13206,#13207,#13208,#13209,#13210,#13211,#13212,
#13213,#13214,#13215,#13216,#13217,#13218,#13219,#13220,#13221,#13222,#13223,
#13224,#13225,#13226,#13227,#13228,#13229,#13230,#13231,#13232,#13233,#13234,
#13235,#13236,#13237,#13238,#13239,#13240,#13241,#13242,#13243,#13244,#13245,
#13246,#13247,#13248,#13249,#13250,#13251,#13252,#13253,#13254,#13255,#13256,
#13257,#13258,#13259,#13260,#13261,#13262,#13263,#13264,#13265,#13266,#13267,
#13268,#13269,#13270,#13271,#13272,#13273,#13274,#13275,#13276,#13277,#13278,
#13279,#13280,#13281,#13282,#13283,#13284,#13285,#13286,#13287,#13288,#13289,
#13290,#13291,#13292,#13293,#13294,#13295,#13296,#13297,#13298,#13299,#13300,
#13301,#13302,#13303,#13304,#13305,#13306,#13307,#13308,#13309,#13310,#13311,
#13312,#13313,#13314,#13315,#13316,#13317,#13318,#13319,#13320,#13321,#13322,
#13323,#13324,#13325));
#13643=CLOSED_SHELL('',(#13326,#13327,#13328,#13329,#13330,#13331,#13332,
#13333,#13334,#13335,#13336,#13337,#13338,#13339,#13340,#13341,#13342,#13343,
#13344,#13345,#13346,#13347,#13348,#13349,#13350,#13351,#13352,#13353,#13354,
#13355,#13356,#13357,#13358,#13359,#13360,#13361,#13362,#13363,#13364,#13365,
#13366,#13367,#13368,#13369,#13370,#13371,#13372,#13373,#13374,#13375,#13376,
#13377,#13378,#13379,#13380,#13381,#13382,#13383,#13384,#13385,#13386,#13387,
#13388,#13389,#13390,#13391,#13392,#13393,#13394,#13395,#13396,#13397,#13398,
#13399,#13400,#13401,#13402,#13403,#13404,#13405,#13406,#13407,#13408,#13409,
#13410,#13411,#13412,#13413,#13414,#13415,#13416,#13417,#13418,#13419,#13420,
#13421,#13422,#13423,#13424,#13425,#13426,#13427,#13428,#13429,#13430,#13431,
#13432,#13433,#13434,#13435,#13436,#13437,#13438,#13439,#13440,#13441,#13442,
#13443,#13444,#13445,#13446,#13447,#13448,#13449,#13450,#13451,#13452,#13453,
#13454,#13455,#13456,#13457,#13458,#13459,#13460,#13461,#13462,#13463,#13464,
#13465,#13466,#13467,#13468,#13469,#13470,#13471,#13472,#13473,#13474,#13475,
#13476,#13477,#13478,#13479,#13480,#13481,#13482,#13483,#13484,#13485,#13486));
#13644=CLOSED_SHELL('',(#13487,#13488,#13489,#13490,#13491,#13492,#13493,
#13494,#13495,#13496,#13497,#13498,#13499,#13500,#13501,#13502,#13503,#13504,
#13505,#13506,#13507,#13508,#13509,#13510,#13511,#13512,#13513,#13514,#13515,
#13516,#13517,#13518,#13519,#13520,#13521,#13522,#13523,#13524,#13525,#13526,
#13527,#13528,#13529,#13530,#13531,#13532,#13533,#13534,#13535,#13536,#13537,
#13538,#13539,#13540,#13541,#13542,#13543,#13544,#13545,#13546,#13547,#13548,
#13549,#13550,#13551,#13552,#13553,#13554,#13555,#13556,#13557,#13558,#13559,
#13560,#13561,#13562,#13563,#13564,#13565,#13566,#13567,#13568,#13569,#13570,
#13571,#13572,#13573,#13574,#13575,#13576,#13577,#13578,#13579,#13580,#13581,
#13582,#13583,#13584,#13585,#13586,#13587,#13588,#13589,#13590,#13591,#13592,
#13593,#13594,#13595,#13596,#13597,#13598,#13599,#13600,#13601,#13602,#13603,
#13604,#13605,#13606,#13607,#13608,#13609,#13610,#13611,#13612,#13613,#13614,
#13615,#13616,#13617,#13618,#13619,#13620,#13621,#13622,#13623,#13624,#13625,
#13626,#13627,#13628,#13629,#13630,#13631,#13632,#13633,#13634));
#13645=DERIVED_UNIT_ELEMENT(#13665,1.);
#13646=DERIVED_UNIT_ELEMENT(#71797,-3.);
#13647=DERIVED_UNIT_ELEMENT(#13665,1.);
#13648=DERIVED_UNIT_ELEMENT(#71797,-3.);
#13649=DERIVED_UNIT_ELEMENT(#13665,1.);
#13650=DERIVED_UNIT_ELEMENT(#71797,-3.);
#13651=DERIVED_UNIT_ELEMENT(#13665,1.);
#13652=DERIVED_UNIT_ELEMENT(#71797,-3.);
#13653=DERIVED_UNIT_ELEMENT(#13665,1.);
#13654=DERIVED_UNIT_ELEMENT(#71797,-3.);
#13655=DERIVED_UNIT_ELEMENT(#13665,1.);
#13656=DERIVED_UNIT_ELEMENT(#71797,-3.);
#13657=DERIVED_UNIT_ELEMENT(#13665,1.);
#13658=DERIVED_UNIT_ELEMENT(#71797,-3.);
#13659=DERIVED_UNIT_ELEMENT(#13665,1.);
#13660=DERIVED_UNIT_ELEMENT(#71797,-3.);
#13661=DERIVED_UNIT_ELEMENT(#13665,1.);
#13662=DERIVED_UNIT_ELEMENT(#71797,-3.);
#13663=DERIVED_UNIT_ELEMENT(#13665,1.);
#13664=DERIVED_UNIT_ELEMENT(#71797,-3.);
#13665=(
MASS_UNIT()
NAMED_UNIT(*)
SI_UNIT(.KILO.,.GRAM.)
);
#13666=DERIVED_UNIT((#13645,#13646));
#13667=DERIVED_UNIT((#13647,#13648));
#13668=DERIVED_UNIT((#13649,#13650));
#13669=DERIVED_UNIT((#13651,#13652));
#13670=DERIVED_UNIT((#13653,#13654));
#13671=DERIVED_UNIT((#13655,#13656));
#13672=DERIVED_UNIT((#13657,#13658));
#13673=DERIVED_UNIT((#13659,#13660));
#13674=DERIVED_UNIT((#13661,#13662));
#13675=DERIVED_UNIT((#13663,#13664));
#13676=MEASURE_REPRESENTATION_ITEM('density measure',
POSITIVE_RATIO_MEASURE(7850.),#13666);
#13677=MEASURE_REPRESENTATION_ITEM('density measure',
POSITIVE_RATIO_MEASURE(7850.),#13667);
#13678=MEASURE_REPRESENTATION_ITEM('density measure',
POSITIVE_RATIO_MEASURE(7850.),#13668);
#13679=MEASURE_REPRESENTATION_ITEM('density measure',
POSITIVE_RATIO_MEASURE(7850.),#13669);
#13680=MEASURE_REPRESENTATION_ITEM('density measure',
POSITIVE_RATIO_MEASURE(7850.),#13670);
#13681=MEASURE_REPRESENTATION_ITEM('density measure',
POSITIVE_RATIO_MEASURE(7850.),#13671);
#13682=MEASURE_REPRESENTATION_ITEM('density measure',
POSITIVE_RATIO_MEASURE(7850.),#13672);
#13683=MEASURE_REPRESENTATION_ITEM('density measure',
POSITIVE_RATIO_MEASURE(7850.),#13673);
#13684=MEASURE_REPRESENTATION_ITEM('density measure',
POSITIVE_RATIO_MEASURE(7850.),#13674);
#13685=MEASURE_REPRESENTATION_ITEM('density measure',
POSITIVE_RATIO_MEASURE(7850.),#13675);
#13686=PROPERTY_DEFINITION_REPRESENTATION(#13736,#13706);
#13687=PROPERTY_DEFINITION_REPRESENTATION(#13737,#13707);
#13688=PROPERTY_DEFINITION_REPRESENTATION(#13738,#13708);
#13689=PROPERTY_DEFINITION_REPRESENTATION(#13739,#13709);
#13690=PROPERTY_DEFINITION_REPRESENTATION(#13740,#13710);
#13691=PROPERTY_DEFINITION_REPRESENTATION(#13741,#13711);
#13692=PROPERTY_DEFINITION_REPRESENTATION(#13742,#13712);
#13693=PROPERTY_DEFINITION_REPRESENTATION(#13743,#13713);
#13694=PROPERTY_DEFINITION_REPRESENTATION(#13744,#13714);
#13695=PROPERTY_DEFINITION_REPRESENTATION(#13745,#13715);
#13696=PROPERTY_DEFINITION_REPRESENTATION(#13746,#13716);
#13697=PROPERTY_DEFINITION_REPRESENTATION(#13747,#13717);
#13698=PROPERTY_DEFINITION_REPRESENTATION(#13748,#13718);
#13699=PROPERTY_DEFINITION_REPRESENTATION(#13749,#13719);
#13700=PROPERTY_DEFINITION_REPRESENTATION(#13750,#13720);
#13701=PROPERTY_DEFINITION_REPRESENTATION(#13751,#13721);
#13702=PROPERTY_DEFINITION_REPRESENTATION(#13752,#13722);
#13703=PROPERTY_DEFINITION_REPRESENTATION(#13753,#13723);
#13704=PROPERTY_DEFINITION_REPRESENTATION(#13754,#13724);
#13705=PROPERTY_DEFINITION_REPRESENTATION(#13755,#13725);
#13706=REPRESENTATION('material name',(#13726),#71785);
#13707=REPRESENTATION('density',(#13676),#71785);
#13708=REPRESENTATION('material name',(#13727),#71786);
#13709=REPRESENTATION('density',(#13677),#71786);
#13710=REPRESENTATION('material name',(#13728),#71787);
#13711=REPRESENTATION('density',(#13678),#71787);
#13712=REPRESENTATION('material name',(#13729),#71788);
#13713=REPRESENTATION('density',(#13679),#71788);
#13714=REPRESENTATION('material name',(#13730),#71789);
#13715=REPRESENTATION('density',(#13680),#71789);
#13716=REPRESENTATION('material name',(#13731),#71790);
#13717=REPRESENTATION('density',(#13681),#71790);
#13718=REPRESENTATION('material name',(#13732),#71791);
#13719=REPRESENTATION('density',(#13682),#71791);
#13720=REPRESENTATION('material name',(#13733),#71792);
#13721=REPRESENTATION('density',(#13683),#71792);
#13722=REPRESENTATION('material name',(#13734),#71793);
#13723=REPRESENTATION('density',(#13684),#71793);
#13724=REPRESENTATION('material name',(#13735),#71794);
#13725=REPRESENTATION('density',(#13685),#71794);
#13726=DESCRIPTIVE_REPRESENTATION_ITEM('Steel','Steel');
#13727=DESCRIPTIVE_REPRESENTATION_ITEM('Steel','Steel');
#13728=DESCRIPTIVE_REPRESENTATION_ITEM('Steel','Steel');
#13729=DESCRIPTIVE_REPRESENTATION_ITEM('Steel','Steel');
#13730=DESCRIPTIVE_REPRESENTATION_ITEM('Steel','Steel');
#13731=DESCRIPTIVE_REPRESENTATION_ITEM('Steel','Steel');
#13732=DESCRIPTIVE_REPRESENTATION_ITEM('Steel','Steel');
#13733=DESCRIPTIVE_REPRESENTATION_ITEM('Steel','Steel');
#13734=DESCRIPTIVE_REPRESENTATION_ITEM('Steel','Steel');
#13735=DESCRIPTIVE_REPRESENTATION_ITEM('Steel','Steel');
#13736=PROPERTY_DEFINITION('material property','material name',#72029);
#13737=PROPERTY_DEFINITION('material property','density of part',#72029);
#13738=PROPERTY_DEFINITION('material property','material name',#72030);
#13739=PROPERTY_DEFINITION('material property','density of part',#72030);
#13740=PROPERTY_DEFINITION('material property','material name',#72031);
#13741=PROPERTY_DEFINITION('material property','density of part',#72031);
#13742=PROPERTY_DEFINITION('material property','material name',#72032);
#13743=PROPERTY_DEFINITION('material property','density of part',#72032);
#13744=PROPERTY_DEFINITION('material property','material name',#72033);
#13745=PROPERTY_DEFINITION('material property','density of part',#72033);
#13746=PROPERTY_DEFINITION('material property','material name',#72034);
#13747=PROPERTY_DEFINITION('material property','density of part',#72034);
#13748=PROPERTY_DEFINITION('material property','material name',#72035);
#13749=PROPERTY_DEFINITION('material property','density of part',#72035);
#13750=PROPERTY_DEFINITION('material property','material name',#72036);
#13751=PROPERTY_DEFINITION('material property','density of part',#72036);
#13752=PROPERTY_DEFINITION('material property','material name',#72037);
#13753=PROPERTY_DEFINITION('material property','density of part',#72037);
#13754=PROPERTY_DEFINITION('material property','material name',#72038);
#13755=PROPERTY_DEFINITION('material property','density of part',#72038);
#13756=AXIS2_PLACEMENT_3D('',#18528,#15043,#15044);
#13757=AXIS2_PLACEMENT_3D('',#18529,#15045,#15046);
#13758=AXIS2_PLACEMENT_3D('',#18530,#15047,#15048);
#13759=AXIS2_PLACEMENT_3D('',#18532,#15049,#15050);
#13760=AXIS2_PLACEMENT_3D('',#18535,#15052,#15053);
#13761=AXIS2_PLACEMENT_3D('',#18536,#15054,#15055);
#13762=AXIS2_PLACEMENT_3D('',#18538,#15056,#15057);
#13763=AXIS2_PLACEMENT_3D('',#18539,#15058,#15059);
#13764=AXIS2_PLACEMENT_3D('',#18579,#15061,#15062);
#13765=AXIS2_PLACEMENT_3D('',#18581,#15063,#15064);
#13766=AXIS2_PLACEMENT_3D('',#18584,#15066,#15067);
#13767=AXIS2_PLACEMENT_3D('',#18585,#15068,#15069);
#13768=AXIS2_PLACEMENT_3D('',#18587,#15070,#15071);
#13769=AXIS2_PLACEMENT_3D('',#18588,#15072,#15073);
#13770=AXIS2_PLACEMENT_3D('',#18628,#15075,#15076);
#13771=AXIS2_PLACEMENT_3D('',#18630,#15077,#15078);
#13772=AXIS2_PLACEMENT_3D('',#18633,#15080,#15081);
#13773=AXIS2_PLACEMENT_3D('',#18634,#15082,#15083);
#13774=AXIS2_PLACEMENT_3D('',#18636,#15084,#15085);
#13775=AXIS2_PLACEMENT_3D('',#18637,#15086,#15087);
#13776=AXIS2_PLACEMENT_3D('',#18677,#15089,#15090);
#13777=AXIS2_PLACEMENT_3D('',#18679,#15091,#15092);
#13778=AXIS2_PLACEMENT_3D('',#18682,#15094,#15095);
#13779=AXIS2_PLACEMENT_3D('',#18683,#15096,#15097);
#13780=AXIS2_PLACEMENT_3D('',#18685,#15098,#15099);
#13781=AXIS2_PLACEMENT_3D('',#18686,#15100,#15101);
#13782=AXIS2_PLACEMENT_3D('',#18726,#15103,#15104);
#13783=AXIS2_PLACEMENT_3D('',#18728,#15105,#15106);
#13784=AXIS2_PLACEMENT_3D('',#18731,#15108,#15109);
#13785=AXIS2_PLACEMENT_3D('',#18732,#15110,#15111);
#13786=AXIS2_PLACEMENT_3D('',#18734,#15112,#15113);
#13787=AXIS2_PLACEMENT_3D('',#18735,#15114,#15115);
#13788=AXIS2_PLACEMENT_3D('',#18775,#15117,#15118);
#13789=AXIS2_PLACEMENT_3D('',#18777,#15119,#15120);
#13790=AXIS2_PLACEMENT_3D('',#18780,#15122,#15123);
#13791=AXIS2_PLACEMENT_3D('',#18781,#15124,#15125);
#13792=AXIS2_PLACEMENT_3D('',#18783,#15126,#15127);
#13793=AXIS2_PLACEMENT_3D('',#18784,#15128,#15129);
#13794=AXIS2_PLACEMENT_3D('',#18824,#15131,#15132);
#13795=AXIS2_PLACEMENT_3D('',#18826,#15133,#15134);
#13796=AXIS2_PLACEMENT_3D('',#18829,#15136,#15137);
#13797=AXIS2_PLACEMENT_3D('',#18830,#15138,#15139);
#13798=AXIS2_PLACEMENT_3D('',#18840,#15144,#15145);
#13799=AXIS2_PLACEMENT_3D('',#18842,#15146,#15147);
#13800=AXIS2_PLACEMENT_3D('',#18844,#15148,#15149);
#13801=AXIS2_PLACEMENT_3D('',#18845,#15150,#15151);
#13802=AXIS2_PLACEMENT_3D('',#18848,#15153,#15154);
#13803=AXIS2_PLACEMENT_3D('',#18849,#15155,#15156);
#13804=AXIS2_PLACEMENT_3D('',#18851,#15157,#15158);
#13805=AXIS2_PLACEMENT_3D('',#18853,#15160,#15161);
#13806=AXIS2_PLACEMENT_3D('',#18856,#15163,#15164);
#13807=AXIS2_PLACEMENT_3D('',#18857,#15165,#15166);
#13808=AXIS2_PLACEMENT_3D('',#18859,#15167,#15168);
#13809=AXIS2_PLACEMENT_3D('',#18861,#15170,#15171);
#13810=AXIS2_PLACEMENT_3D('',#18864,#15173,#15174);
#13811=AXIS2_PLACEMENT_3D('',#18865,#15175,#15176);
#13812=AXIS2_PLACEMENT_3D('',#18867,#15177,#15178);
#13813=AXIS2_PLACEMENT_3D('',#18869,#15180,#15181);
#13814=AXIS2_PLACEMENT_3D('',#18872,#15183,#15184);
#13815=AXIS2_PLACEMENT_3D('',#18873,#15185,#15186);
#13816=AXIS2_PLACEMENT_3D('',#18875,#15187,#15188);
#13817=AXIS2_PLACEMENT_3D('',#18876,#15189,#15190);
#13818=AXIS2_PLACEMENT_3D('',#18878,#15191,#15192);
#13819=AXIS2_PLACEMENT_3D('',#18879,#15193,#15194);
#13820=AXIS2_PLACEMENT_3D('',#18881,#15195,#15196);
#13821=AXIS2_PLACEMENT_3D('',#18882,#15197,#15198);
#13822=AXIS2_PLACEMENT_3D('',#18884,#15199,#15200);
#13823=AXIS2_PLACEMENT_3D('',#18885,#15201,#15202);
#13824=AXIS2_PLACEMENT_3D('',#18888,#15204,#15205);
#13825=AXIS2_PLACEMENT_3D('',#18889,#15206,#15207);
#13826=AXIS2_PLACEMENT_3D('',#18892,#15209,#15210);
#13827=AXIS2_PLACEMENT_3D('',#18893,#15211,#15212);
#13828=AXIS2_PLACEMENT_3D('',#18896,#15214,#15215);
#13829=AXIS2_PLACEMENT_3D('',#18897,#15216,#15217);
#13830=AXIS2_PLACEMENT_3D('',#18900,#15219,#15220);
#13831=AXIS2_PLACEMENT_3D('',#18901,#15221,#15222);
#13832=AXIS2_PLACEMENT_3D('',#18910,#15227,#15228);
#13833=AXIS2_PLACEMENT_3D('',#18913,#15231,#15232);
#13834=AXIS2_PLACEMENT_3D('',#18919,#15235,#15236);
#13835=AXIS2_PLACEMENT_3D('',#18935,#15244,#15245);
#13836=AXIS2_PLACEMENT_3D('',#18943,#15250,#15251);
#13837=AXIS2_PLACEMENT_3D('',#18949,#15255,#15256);
#13838=AXIS2_PLACEMENT_3D('',#18953,#15259,#15260);
#13839=AXIS2_PLACEMENT_3D('',#18959,#15264,#15265);
#13840=AXIS2_PLACEMENT_3D('',#18963,#15268,#15269);
#13841=AXIS2_PLACEMENT_3D('',#18967,#15272,#15273);
#13842=AXIS2_PLACEMENT_3D('',#18971,#15275,#15276);
#13843=AXIS2_PLACEMENT_3D('',#18973,#15278,#15279);
#13844=AXIS2_PLACEMENT_3D('',#18977,#15282,#15283);
#13845=AXIS2_PLACEMENT_3D('',#18979,#15285,#15286);
#13846=AXIS2_PLACEMENT_3D('',#18983,#15289,#15290);
#13847=AXIS2_PLACEMENT_3D('',#18987,#15293,#15294);
#13848=AXIS2_PLACEMENT_3D('',#18989,#15295,#15296);
#13849=AXIS2_PLACEMENT_3D('',#18991,#15298,#15299);
#13850=AXIS2_PLACEMENT_3D('',#18993,#15301,#15302);
#13851=AXIS2_PLACEMENT_3D('',#18995,#15304,#15305);
#13852=AXIS2_PLACEMENT_3D('',#18999,#15308,#15309);
#13853=AXIS2_PLACEMENT_3D('',#19001,#15311,#15312);
#13854=AXIS2_PLACEMENT_3D('',#19002,#15313,#15314);
#13855=AXIS2_PLACEMENT_3D('',#19003,#15315,#15316);
#13856=AXIS2_PLACEMENT_3D('',#19013,#15317,#15318);
#13857=AXIS2_PLACEMENT_3D('',#19021,#15319,#15320);
#13858=AXIS2_PLACEMENT_3D('',#19022,#15321,#15322);
#13859=AXIS2_PLACEMENT_3D('',#19032,#15327,#15328);
#13860=AXIS2_PLACEMENT_3D('',#19034,#15329,#15330);
#13861=AXIS2_PLACEMENT_3D('',#19036,#15331,#15332);
#13862=AXIS2_PLACEMENT_3D('',#19038,#15333,#15334);
#13863=AXIS2_PLACEMENT_3D('',#19041,#15335,#15336);
#13864=AXIS2_PLACEMENT_3D('',#19042,#15337,#15338);
#13865=AXIS2_PLACEMENT_3D('',#19043,#15339,#15340);
#13866=AXIS2_PLACEMENT_3D('',#19045,#15341,#15342);
#13867=AXIS2_PLACEMENT_3D('',#19047,#15343,#15344);
#13868=AXIS2_PLACEMENT_3D('',#19050,#15345,#15346);
#13869=AXIS2_PLACEMENT_3D('',#19051,#15347,#15348);
#13870=AXIS2_PLACEMENT_3D('',#19054,#15349,#15350);
#13871=AXIS2_PLACEMENT_3D('',#19055,#15351,#15352);
#13872=AXIS2_PLACEMENT_3D('',#19057,#15353,#15354);
#13873=AXIS2_PLACEMENT_3D('',#19059,#15355,#15356);
#13874=AXIS2_PLACEMENT_3D('',#19060,#15357,#15358);
#13875=AXIS2_PLACEMENT_3D('',#19062,#15359,#15360);
#13876=AXIS2_PLACEMENT_3D('',#19064,#15362,#15363);
#13877=AXIS2_PLACEMENT_3D('',#19067,#15365,#15366);
#13878=AXIS2_PLACEMENT_3D('',#19068,#15367,#15368);
#13879=AXIS2_PLACEMENT_3D('',#19083,#15369,#15370);
#13880=AXIS2_PLACEMENT_3D('',#19084,#15371,#15372);
#13881=AXIS2_PLACEMENT_3D('',#19086,#15373,#15374);
#13882=AXIS2_PLACEMENT_3D('',#19088,#15376,#15377);
#13883=AXIS2_PLACEMENT_3D('',#19091,#15379,#15380);
#13884=AXIS2_PLACEMENT_3D('',#19092,#15381,#15382);
#13885=AXIS2_PLACEMENT_3D('',#19107,#15383,#15384);
#13886=AXIS2_PLACEMENT_3D('',#19108,#15385,#15386);
#13887=AXIS2_PLACEMENT_3D('',#19110,#15387,#15388);
#13888=AXIS2_PLACEMENT_3D('',#19112,#15390,#15391);
#13889=AXIS2_PLACEMENT_3D('',#19115,#15393,#15394);
#13890=AXIS2_PLACEMENT_3D('',#19116,#15395,#15396);
#13891=AXIS2_PLACEMENT_3D('',#19118,#15397,#15398);
#13892=AXIS2_PLACEMENT_3D('',#19120,#15400,#15401);
#13893=AXIS2_PLACEMENT_3D('',#19123,#15403,#15404);
#13894=AXIS2_PLACEMENT_3D('',#19124,#15405,#15406);
#13895=AXIS2_PLACEMENT_3D('',#19139,#15407,#15408);
#13896=AXIS2_PLACEMENT_3D('',#19140,#15409,#15410);
#13897=AXIS2_PLACEMENT_3D('',#19149,#15412,#15413);
#13898=AXIS2_PLACEMENT_3D('',#19156,#15415,#15416);
#13899=AXIS2_PLACEMENT_3D('',#19157,#15417,#15418);
#13900=AXIS2_PLACEMENT_3D('',#19159,#15419,#15420);
#13901=AXIS2_PLACEMENT_3D('',#19160,#15421,#15422);
#13902=AXIS2_PLACEMENT_3D('',#19162,#15423,#15424);
#13903=AXIS2_PLACEMENT_3D('',#19163,#15425,#15426);
#13904=AXIS2_PLACEMENT_3D('',#19165,#15427,#15428);
#13905=AXIS2_PLACEMENT_3D('',#19166,#15429,#15430);
#13906=AXIS2_PLACEMENT_3D('',#19175,#15432,#15433);
#13907=AXIS2_PLACEMENT_3D('',#19182,#15435,#15436);
#13908=AXIS2_PLACEMENT_3D('',#19183,#15437,#15438);
#13909=AXIS2_PLACEMENT_3D('',#19185,#15439,#15440);
#13910=AXIS2_PLACEMENT_3D('',#19186,#15441,#15442);
#13911=AXIS2_PLACEMENT_3D('',#19188,#15443,#15444);
#13912=AXIS2_PLACEMENT_3D('',#19189,#15445,#15446);
#13913=AXIS2_PLACEMENT_3D('',#19198,#15448,#15449);
#13914=AXIS2_PLACEMENT_3D('',#19205,#15451,#15452);
#13915=AXIS2_PLACEMENT_3D('',#19206,#15453,#15454);
#13916=AXIS2_PLACEMENT_3D('',#19208,#15455,#15456);
#13917=AXIS2_PLACEMENT_3D('',#19209,#15457,#15458);
#13918=AXIS2_PLACEMENT_3D('',#19211,#15459,#15460);
#13919=AXIS2_PLACEMENT_3D('',#19212,#15461,#15462);
#13920=AXIS2_PLACEMENT_3D('',#19221,#15464,#15465);
#13921=AXIS2_PLACEMENT_3D('',#19228,#15467,#15468);
#13922=AXIS2_PLACEMENT_3D('',#19229,#15469,#15470);
#13923=AXIS2_PLACEMENT_3D('',#19231,#15471,#15472);
#13924=AXIS2_PLACEMENT_3D('',#19232,#15473,#15474);
#13925=AXIS2_PLACEMENT_3D('',#19234,#15475,#15476);
#13926=AXIS2_PLACEMENT_3D('',#19235,#15477,#15478);
#13927=AXIS2_PLACEMENT_3D('',#19236,#15479,#15480);
#13928=AXIS2_PLACEMENT_3D('',#19238,#15481,#15482);
#13929=AXIS2_PLACEMENT_3D('',#19239,#15483,#15484);
#13930=AXIS2_PLACEMENT_3D('',#19240,#15485,#15486);
#13931=AXIS2_PLACEMENT_3D('',#19242,#15487,#15488);
#13932=AXIS2_PLACEMENT_3D('',#19243,#15489,#15490);
#13933=AXIS2_PLACEMENT_3D('',#19244,#15491,#15492);
#13934=AXIS2_PLACEMENT_3D('',#19246,#15493,#15494);
#13935=AXIS2_PLACEMENT_3D('',#19247,#15495,#15496);
#13936=AXIS2_PLACEMENT_3D('',#19248,#15497,#15498);
#13937=AXIS2_PLACEMENT_3D('',#19251,#15500,#15501);
#13938=AXIS2_PLACEMENT_3D('',#19252,#15502,#15503);
#13939=AXIS2_PLACEMENT_3D('',#19255,#15505,#15506);
#13940=AXIS2_PLACEMENT_3D('',#19256,#15507,#15508);
#13941=AXIS2_PLACEMENT_3D('',#19259,#15510,#15511);
#13942=AXIS2_PLACEMENT_3D('',#19260,#15512,#15513);
#13943=AXIS2_PLACEMENT_3D('',#19263,#15515,#15516);
#13944=AXIS2_PLACEMENT_3D('',#19264,#15517,#15518);
#13945=AXIS2_PLACEMENT_3D('',#19267,#15520,#15521);
#13946=AXIS2_PLACEMENT_3D('',#19268,#15522,#15523);
#13947=AXIS2_PLACEMENT_3D('',#19271,#15525,#15526);
#13948=AXIS2_PLACEMENT_3D('',#19272,#15527,#15528);
#13949=AXIS2_PLACEMENT_3D('',#19275,#15530,#15531);
#13950=AXIS2_PLACEMENT_3D('',#19276,#15532,#15533);
#13951=AXIS2_PLACEMENT_3D('',#19279,#15535,#15536);
#13952=AXIS2_PLACEMENT_3D('',#19280,#15537,#15538);
#13953=AXIS2_PLACEMENT_3D('',#19282,#15539,#15540);
#13954=AXIS2_PLACEMENT_3D('',#19284,#15542,#15543);
#13955=AXIS2_PLACEMENT_3D('',#19287,#15545,#15546);
#13956=AXIS2_PLACEMENT_3D('',#19288,#15547,#15548);
#13957=AXIS2_PLACEMENT_3D('',#19290,#15549,#15550);
#13958=AXIS2_PLACEMENT_3D('',#19292,#15552,#15553);
#13959=AXIS2_PLACEMENT_3D('',#19295,#15555,#15556);
#13960=AXIS2_PLACEMENT_3D('',#19296,#15557,#15558);
#13961=AXIS2_PLACEMENT_3D('',#19299,#15560,#15561);
#13962=AXIS2_PLACEMENT_3D('',#19300,#15562,#15563);
#13963=AXIS2_PLACEMENT_3D('',#19303,#15565,#15566);
#13964=AXIS2_PLACEMENT_3D('',#19304,#15567,#15568);
#13965=AXIS2_PLACEMENT_3D('',#19307,#15570,#15571);
#13966=AXIS2_PLACEMENT_3D('',#19308,#15572,#15573);
#13967=AXIS2_PLACEMENT_3D('',#19311,#15575,#15576);
#13968=AXIS2_PLACEMENT_3D('',#19312,#15577,#15578);
#13969=AXIS2_PLACEMENT_3D('',#19314,#15579,#15580);
#13970=AXIS2_PLACEMENT_3D('',#19316,#15582,#15583);
#13971=AXIS2_PLACEMENT_3D('',#19319,#15585,#15586);
#13972=AXIS2_PLACEMENT_3D('',#19320,#15587,#15588);
#13973=AXIS2_PLACEMENT_3D('',#19322,#15589,#15590);
#13974=AXIS2_PLACEMENT_3D('',#19324,#15592,#15593);
#13975=AXIS2_PLACEMENT_3D('',#19327,#15595,#15596);
#13976=AXIS2_PLACEMENT_3D('',#19328,#15597,#15598);
#13977=AXIS2_PLACEMENT_3D('',#19331,#15600,#15601);
#13978=AXIS2_PLACEMENT_3D('',#19334,#15603,#15604);
#13979=AXIS2_PLACEMENT_3D('',#19337,#15606,#15607);
#13980=AXIS2_PLACEMENT_3D('',#19340,#15609,#15610);
#13981=AXIS2_PLACEMENT_3D('',#19343,#15612,#15613);
#13982=AXIS2_PLACEMENT_3D('',#19346,#15615,#15616);
#13983=AXIS2_PLACEMENT_3D('',#19349,#15618,#15619);
#13984=AXIS2_PLACEMENT_3D('',#19352,#15621,#15622);
#13985=AXIS2_PLACEMENT_3D('',#19358,#15626,#15627);
#13986=AXIS2_PLACEMENT_3D('',#19362,#15630,#15631);
#13987=AXIS2_PLACEMENT_3D('',#19366,#15634,#15635);
#13988=AXIS2_PLACEMENT_3D('',#19368,#15637,#15638);
#13989=AXIS2_PLACEMENT_3D('',#19374,#15642,#15643);
#13990=AXIS2_PLACEMENT_3D('',#19378,#15646,#15647);
#13991=AXIS2_PLACEMENT_3D('',#19382,#15650,#15651);
#13992=AXIS2_PLACEMENT_3D('',#19384,#15653,#15654);
#13993=AXIS2_PLACEMENT_3D('',#19385,#15655,#15656);
#13994=AXIS2_PLACEMENT_3D('',#19386,#15657,#15658);
#13995=AXIS2_PLACEMENT_3D('',#19427,#15660,#15661);
#13996=AXIS2_PLACEMENT_3D('',#19428,#15662,#15663);
#13997=AXIS2_PLACEMENT_3D('',#19431,#15665,#15666);
#13998=AXIS2_PLACEMENT_3D('',#19472,#15668,#15669);
#13999=AXIS2_PLACEMENT_3D('',#19473,#15670,#15671);
#14000=AXIS2_PLACEMENT_3D('',#19476,#15673,#15674);
#14001=AXIS2_PLACEMENT_3D('',#19517,#15676,#15677);
#14002=AXIS2_PLACEMENT_3D('',#19518,#15678,#15679);
#14003=AXIS2_PLACEMENT_3D('',#19521,#15681,#15682);
#14004=AXIS2_PLACEMENT_3D('',#19523,#15683,#15684);
#14005=AXIS2_PLACEMENT_3D('',#19524,#15685,#15686);
#14006=AXIS2_PLACEMENT_3D('',#19526,#15687,#15688);
#14007=AXIS2_PLACEMENT_3D('',#19528,#15690,#15691);
#14008=AXIS2_PLACEMENT_3D('',#19530,#15692,#15693);
#14009=AXIS2_PLACEMENT_3D('',#19532,#15695,#15696);
#14010=AXIS2_PLACEMENT_3D('',#19535,#15698,#15699);
#14011=AXIS2_PLACEMENT_3D('',#19536,#15700,#15701);
#14012=AXIS2_PLACEMENT_3D('',#19537,#15702,#15703);
#14013=AXIS2_PLACEMENT_3D('',#19538,#15704,#15705);
#14014=AXIS2_PLACEMENT_3D('',#19540,#15706,#15707);
#14015=AXIS2_PLACEMENT_3D('',#19543,#15709,#15710);
#14016=AXIS2_PLACEMENT_3D('',#19544,#15711,#15712);
#14017=AXIS2_PLACEMENT_3D('',#19554,#15717,#15718);
#14018=AXIS2_PLACEMENT_3D('',#19555,#15719,#15720);
#14019=AXIS2_PLACEMENT_3D('',#19559,#15722,#15723);
#14020=AXIS2_PLACEMENT_3D('',#19575,#15724,#15725);
#14021=AXIS2_PLACEMENT_3D('',#19576,#15726,#15727);
#14022=AXIS2_PLACEMENT_3D('',#19578,#15728,#15729);
#14023=AXIS2_PLACEMENT_3D('',#19580,#15731,#15732);
#14024=AXIS2_PLACEMENT_3D('',#19584,#15734,#15735);
#14025=AXIS2_PLACEMENT_3D('',#19600,#15736,#15737);
#14026=AXIS2_PLACEMENT_3D('',#19601,#15738,#15739);
#14027=AXIS2_PLACEMENT_3D('',#19618,#15741,#15742);
#14028=AXIS2_PLACEMENT_3D('',#19621,#15743,#15744);
#14029=AXIS2_PLACEMENT_3D('',#19625,#15746,#15747);
#14030=AXIS2_PLACEMENT_3D('',#19641,#15749,#15750);
#14031=AXIS2_PLACEMENT_3D('',#19644,#15752,#15753);
#14032=AXIS2_PLACEMENT_3D('',#19648,#15755,#15756);
#14033=AXIS2_PLACEMENT_3D('',#19650,#15758,#15759);
#14034=AXIS2_PLACEMENT_3D('',#19665,#15768,#15769);
#14035=AXIS2_PLACEMENT_3D('',#19671,#15773,#15774);
#14036=AXIS2_PLACEMENT_3D('',#19674,#15776,#15777);
#14037=AXIS2_PLACEMENT_3D('',#19675,#15778,#15779);
#14038=AXIS2_PLACEMENT_3D('',#19688,#15787,#15788);
#14039=AXIS2_PLACEMENT_3D('',#19690,#15790,#15791);
#14040=AXIS2_PLACEMENT_3D('',#19692,#15793,#15794);
#14041=AXIS2_PLACEMENT_3D('',#19694,#15796,#15797);
#14042=AXIS2_PLACEMENT_3D('',#19696,#15799,#15800);
#14043=AXIS2_PLACEMENT_3D('',#19698,#15802,#15803);
#14044=AXIS2_PLACEMENT_3D('',#19699,#15804,#15805);
#14045=AXIS2_PLACEMENT_3D('',#19700,#15806,#15807);
#14046=AXIS2_PLACEMENT_3D('',#19701,#15808,#15809);
#14047=AXIS2_PLACEMENT_3D('',#19714,#15816,#15817);
#14048=AXIS2_PLACEMENT_3D('',#19727,#15824,#15825);
#14049=AXIS2_PLACEMENT_3D('',#19728,#15826,#15827);
#14050=AXIS2_PLACEMENT_3D('',#19729,#15828,#15829);
#14051=AXIS2_PLACEMENT_3D('',#19730,#15830,#15831);
#14052=AXIS2_PLACEMENT_3D('',#19731,#15832,#15833);
#14053=AXIS2_PLACEMENT_3D('',#19732,#15834,#15835);
#14054=AXIS2_PLACEMENT_3D('',#19733,#15836,#15837);
#14055=AXIS2_PLACEMENT_3D('',#19734,#15838,#15839);
#14056=AXIS2_PLACEMENT_3D('',#19735,#15840,#15841);
#14057=AXIS2_PLACEMENT_3D('',#19736,#15842,#15843);
#14058=AXIS2_PLACEMENT_3D('',#19737,#15844,#15845);
#14059=AXIS2_PLACEMENT_3D('',#19738,#15846,#15847);
#14060=AXIS2_PLACEMENT_3D('',#19739,#15848,#15849);
#14061=AXIS2_PLACEMENT_3D('',#19740,#15850,#15851);
#14062=AXIS2_PLACEMENT_3D('',#19749,#15856,#15857);
#14063=AXIS2_PLACEMENT_3D('',#19751,#15858,#15859);
#14064=AXIS2_PLACEMENT_3D('',#19753,#15860,#15861);
#14065=AXIS2_PLACEMENT_3D('',#19755,#15863,#15864);
#14066=AXIS2_PLACEMENT_3D('',#19761,#15868,#15869);
#14067=AXIS2_PLACEMENT_3D('',#19762,#15870,#15871);
#14068=AXIS2_PLACEMENT_3D('',#19763,#15872,#15873);
#14069=AXIS2_PLACEMENT_3D('',#19764,#15874,#15875);
#14070=AXIS2_PLACEMENT_3D('',#19773,#15880,#15881);
#14071=AXIS2_PLACEMENT_3D('',#19775,#15882,#15883);
#14072=AXIS2_PLACEMENT_3D('',#19777,#15884,#15885);
#14073=AXIS2_PLACEMENT_3D('',#19779,#15887,#15888);
#14074=AXIS2_PLACEMENT_3D('',#19785,#15892,#15893);
#14075=AXIS2_PLACEMENT_3D('',#19786,#15894,#15895);
#14076=AXIS2_PLACEMENT_3D('',#19787,#15896,#15897);
#14077=AXIS2_PLACEMENT_3D('',#19788,#15898,#15899);
#14078=AXIS2_PLACEMENT_3D('',#19797,#15904,#15905);
#14079=AXIS2_PLACEMENT_3D('',#19799,#15906,#15907);
#14080=AXIS2_PLACEMENT_3D('',#19801,#15908,#15909);
#14081=AXIS2_PLACEMENT_3D('',#19803,#15911,#15912);
#14082=AXIS2_PLACEMENT_3D('',#19809,#15916,#15917);
#14083=AXIS2_PLACEMENT_3D('',#19810,#15918,#15919);
#14084=AXIS2_PLACEMENT_3D('',#19811,#15920,#15921);
#14085=AXIS2_PLACEMENT_3D('',#19812,#15922,#15923);
#14086=AXIS2_PLACEMENT_3D('',#19821,#15928,#15929);
#14087=AXIS2_PLACEMENT_3D('',#19823,#15930,#15931);
#14088=AXIS2_PLACEMENT_3D('',#19825,#15932,#15933);
#14089=AXIS2_PLACEMENT_3D('',#19827,#15935,#15936);
#14090=AXIS2_PLACEMENT_3D('',#19833,#15940,#15941);
#14091=AXIS2_PLACEMENT_3D('',#19834,#15942,#15943);
#14092=AXIS2_PLACEMENT_3D('',#19835,#15944,#15945);
#14093=AXIS2_PLACEMENT_3D('',#19836,#15946,#15947);
#14094=AXIS2_PLACEMENT_3D('',#19845,#15952,#15953);
#14095=AXIS2_PLACEMENT_3D('',#19847,#15954,#15955);
#14096=AXIS2_PLACEMENT_3D('',#19849,#15956,#15957);
#14097=AXIS2_PLACEMENT_3D('',#19851,#15959,#15960);
#14098=AXIS2_PLACEMENT_3D('',#19857,#15964,#15965);
#14099=AXIS2_PLACEMENT_3D('',#19858,#15966,#15967);
#14100=AXIS2_PLACEMENT_3D('',#19859,#15968,#15969);
#14101=AXIS2_PLACEMENT_3D('',#19860,#15970,#15971);
#14102=AXIS2_PLACEMENT_3D('',#19869,#15976,#15977);
#14103=AXIS2_PLACEMENT_3D('',#19878,#15982,#15983);
#14104=AXIS2_PLACEMENT_3D('',#19879,#15984,#15985);
#14105=AXIS2_PLACEMENT_3D('',#19880,#15986,#15987);
#14106=AXIS2_PLACEMENT_3D('',#19881,#15988,#15989);
#14107=AXIS2_PLACEMENT_3D('',#19882,#15990,#15991);
#14108=AXIS2_PLACEMENT_3D('',#19883,#15992,#15993);
#14109=AXIS2_PLACEMENT_3D('',#19884,#15994,#15995);
#14110=AXIS2_PLACEMENT_3D('',#19885,#15996,#15997);
#14111=AXIS2_PLACEMENT_3D('',#19886,#15998,#15999);
#14112=AXIS2_PLACEMENT_3D('',#19887,#16000,#16001);
#14113=AXIS2_PLACEMENT_3D('',#19890,#16002,#16003);
#14114=AXIS2_PLACEMENT_3D('',#19891,#16004,#16005);
#14115=AXIS2_PLACEMENT_3D('',#19892,#16006,#16007);
#14116=AXIS2_PLACEMENT_3D('',#20028,#16009,#16010);
#14117=AXIS2_PLACEMENT_3D('',#20114,#16011,#16012);
#14118=AXIS2_PLACEMENT_3D('',#20540,#16014,#16015);
#14119=AXIS2_PLACEMENT_3D('',#20962,#16017,#16018);
#14120=AXIS2_PLACEMENT_3D('',#21424,#16020,#16021);
#14121=AXIS2_PLACEMENT_3D('',#21844,#16023,#16024);
#14122=AXIS2_PLACEMENT_3D('',#22308,#16026,#16027);
#14123=AXIS2_PLACEMENT_3D('',#22730,#16029,#16030);
#14124=AXIS2_PLACEMENT_3D('',#23229,#16032,#16033);
#14125=AXIS2_PLACEMENT_3D('',#23489,#16035,#16036);
#14126=AXIS2_PLACEMENT_3D('',#23793,#16038,#16039);
#14127=AXIS2_PLACEMENT_3D('',#24182,#16041,#16042);
#14128=AXIS2_PLACEMENT_3D('',#24607,#16044,#16045);
#14129=AXIS2_PLACEMENT_3D('',#25043,#16047,#16048);
#14130=AXIS2_PLACEMENT_3D('',#25481,#16050,#16051);
#14131=AXIS2_PLACEMENT_3D('',#25909,#16053,#16054);
#14132=AXIS2_PLACEMENT_3D('',#26351,#16056,#16057);
#14133=AXIS2_PLACEMENT_3D('',#26783,#16059,#16060);
#14134=AXIS2_PLACEMENT_3D('',#27249,#16062,#16063);
#14135=AXIS2_PLACEMENT_3D('',#27667,#16065,#16066);
#14136=AXIS2_PLACEMENT_3D('',#27738,#16067,#16068);
#14137=AXIS2_PLACEMENT_3D('',#31404,#16069,#16070);
#14138=AXIS2_PLACEMENT_3D('',#31406,#16071,#16072);
#14139=AXIS2_PLACEMENT_3D('',#34869,#16073,#16074);
#14140=AXIS2_PLACEMENT_3D('',#35041,#16075,#16076);
#14141=AXIS2_PLACEMENT_3D('',#35170,#16077,#16078);
#14142=AXIS2_PLACEMENT_3D('',#35172,#16079,#16080);
#14143=AXIS2_PLACEMENT_3D('',#35918,#16081,#16082);
#14144=AXIS2_PLACEMENT_3D('',#35921,#16083,#16084);
#14145=AXIS2_PLACEMENT_3D('',#36001,#16085,#16086);
#14146=AXIS2_PLACEMENT_3D('',#36510,#16087,#16088);
#14147=AXIS2_PLACEMENT_3D('',#36512,#16089,#16090);
#14148=AXIS2_PLACEMENT_3D('',#36513,#16091,#16092);
#14149=AXIS2_PLACEMENT_3D('',#36514,#16093,#16094);
#14150=AXIS2_PLACEMENT_3D('',#36516,#16095,#16096);
#14151=AXIS2_PLACEMENT_3D('',#36517,#16097,#16098);
#14152=AXIS2_PLACEMENT_3D('',#36520,#16100,#16101);
#14153=AXIS2_PLACEMENT_3D('',#36521,#16102,#16103);
#14154=AXIS2_PLACEMENT_3D('',#36522,#16104,#16105);
#14155=AXIS2_PLACEMENT_3D('',#36533,#16109,#16110);
#14156=AXIS2_PLACEMENT_3D('',#36541,#16113,#16114);
#14157=AXIS2_PLACEMENT_3D('',#36542,#16115,#16116);
#14158=AXIS2_PLACEMENT_3D('',#36543,#16117,#16118);
#14159=AXIS2_PLACEMENT_3D('',#36550,#16119,#16120);
#14160=AXIS2_PLACEMENT_3D('',#36560,#16121,#16122);
#14161=AXIS2_PLACEMENT_3D('',#36570,#16123,#16124);
#14162=AXIS2_PLACEMENT_3D('',#36580,#16125,#16126);
#14163=AXIS2_PLACEMENT_3D('',#36590,#16127,#16128);
#14164=AXIS2_PLACEMENT_3D('',#36600,#16129,#16130);
#14165=AXIS2_PLACEMENT_3D('',#36610,#16131,#16132);
#14166=AXIS2_PLACEMENT_3D('',#36620,#16133,#16134);
#14167=AXIS2_PLACEMENT_3D('',#36630,#16135,#16136);
#14168=AXIS2_PLACEMENT_3D('',#36640,#16137,#16138);
#14169=AXIS2_PLACEMENT_3D('',#36650,#16139,#16140);
#14170=AXIS2_PLACEMENT_3D('',#36660,#16141,#16142);
#14171=AXIS2_PLACEMENT_3D('',#36670,#16143,#16144);
#14172=AXIS2_PLACEMENT_3D('',#36680,#16145,#16146);
#14173=AXIS2_PLACEMENT_3D('',#36690,#16147,#16148);
#14174=AXIS2_PLACEMENT_3D('',#36700,#16149,#16150);
#14175=AXIS2_PLACEMENT_3D('',#36710,#16151,#16152);
#14176=AXIS2_PLACEMENT_3D('',#36720,#16153,#16154);
#14177=AXIS2_PLACEMENT_3D('',#36729,#16155,#16156);
#14178=AXIS2_PLACEMENT_3D('',#36731,#16157,#16158);
#14179=AXIS2_PLACEMENT_3D('',#36741,#16159,#16160);
#14180=AXIS2_PLACEMENT_3D('',#36751,#16161,#16162);
#14181=AXIS2_PLACEMENT_3D('',#36761,#16163,#16164);
#14182=AXIS2_PLACEMENT_3D('',#36771,#16165,#16166);
#14183=AXIS2_PLACEMENT_3D('',#36781,#16167,#16168);
#14184=AXIS2_PLACEMENT_3D('',#36791,#16169,#16170);
#14185=AXIS2_PLACEMENT_3D('',#36801,#16171,#16172);
#14186=AXIS2_PLACEMENT_3D('',#36811,#16173,#16174);
#14187=AXIS2_PLACEMENT_3D('',#36821,#16175,#16176);
#14188=AXIS2_PLACEMENT_3D('',#36831,#16177,#16178);
#14189=AXIS2_PLACEMENT_3D('',#36841,#16179,#16180);
#14190=AXIS2_PLACEMENT_3D('',#36851,#16181,#16182);
#14191=AXIS2_PLACEMENT_3D('',#36861,#16183,#16184);
#14192=AXIS2_PLACEMENT_3D('',#36871,#16185,#16186);
#14193=AXIS2_PLACEMENT_3D('',#36881,#16187,#16188);
#14194=AXIS2_PLACEMENT_3D('',#36891,#16189,#16190);
#14195=AXIS2_PLACEMENT_3D('',#36897,#16192,#16193);
#14196=AXIS2_PLACEMENT_3D('',#36898,#16194,#16195);
#14197=AXIS2_PLACEMENT_3D('',#36904,#16199,#16200);
#14198=AXIS2_PLACEMENT_3D('',#36908,#16203,#16204);
#14199=AXIS2_PLACEMENT_3D('',#36909,#16205,#16206);
#14200=AXIS2_PLACEMENT_3D('',#36910,#16207,#16208);
#14201=AXIS2_PLACEMENT_3D('',#36916,#16212,#16213);
#14202=AXIS2_PLACEMENT_3D('',#36920,#16216,#16217);
#14203=AXIS2_PLACEMENT_3D('',#36921,#16218,#16219);
#14204=AXIS2_PLACEMENT_3D('',#36922,#16220,#16221);
#14205=AXIS2_PLACEMENT_3D('',#36928,#16225,#16226);
#14206=AXIS2_PLACEMENT_3D('',#36932,#16229,#16230);
#14207=AXIS2_PLACEMENT_3D('',#36933,#16231,#16232);
#14208=AXIS2_PLACEMENT_3D('',#36934,#16233,#16234);
#14209=AXIS2_PLACEMENT_3D('',#36940,#16238,#16239);
#14210=AXIS2_PLACEMENT_3D('',#36944,#16242,#16243);
#14211=AXIS2_PLACEMENT_3D('',#36945,#16244,#16245);
#14212=AXIS2_PLACEMENT_3D('',#36946,#16246,#16247);
#14213=AXIS2_PLACEMENT_3D('',#36952,#16251,#16252);
#14214=AXIS2_PLACEMENT_3D('',#36956,#16255,#16256);
#14215=AXIS2_PLACEMENT_3D('',#36957,#16257,#16258);
#14216=AXIS2_PLACEMENT_3D('',#36958,#16259,#16260);
#14217=AXIS2_PLACEMENT_3D('',#36964,#16264,#16265);
#14218=AXIS2_PLACEMENT_3D('',#36968,#16268,#16269);
#14219=AXIS2_PLACEMENT_3D('',#36969,#16270,#16271);
#14220=AXIS2_PLACEMENT_3D('',#36970,#16272,#16273);
#14221=AXIS2_PLACEMENT_3D('',#36976,#16277,#16278);
#14222=AXIS2_PLACEMENT_3D('',#36980,#16281,#16282);
#14223=AXIS2_PLACEMENT_3D('',#36981,#16283,#16284);
#14224=AXIS2_PLACEMENT_3D('',#36982,#16285,#16286);
#14225=AXIS2_PLACEMENT_3D('',#36988,#16290,#16291);
#14226=AXIS2_PLACEMENT_3D('',#36992,#16294,#16295);
#14227=AXIS2_PLACEMENT_3D('',#36993,#16296,#16297);
#14228=AXIS2_PLACEMENT_3D('',#36994,#16298,#16299);
#14229=AXIS2_PLACEMENT_3D('',#37000,#16303,#16304);
#14230=AXIS2_PLACEMENT_3D('',#37004,#16307,#16308);
#14231=AXIS2_PLACEMENT_3D('',#37005,#16309,#16310);
#14232=AXIS2_PLACEMENT_3D('',#37006,#16311,#16312);
#14233=AXIS2_PLACEMENT_3D('',#37012,#16316,#16317);
#14234=AXIS2_PLACEMENT_3D('',#37016,#16320,#16321);
#14235=AXIS2_PLACEMENT_3D('',#37017,#16322,#16323);
#14236=AXIS2_PLACEMENT_3D('',#37018,#16324,#16325);
#14237=AXIS2_PLACEMENT_3D('',#37024,#16329,#16330);
#14238=AXIS2_PLACEMENT_3D('',#37028,#16333,#16334);
#14239=AXIS2_PLACEMENT_3D('',#37029,#16335,#16336);
#14240=AXIS2_PLACEMENT_3D('',#37030,#16337,#16338);
#14241=AXIS2_PLACEMENT_3D('',#37036,#16342,#16343);
#14242=AXIS2_PLACEMENT_3D('',#37040,#16346,#16347);
#14243=AXIS2_PLACEMENT_3D('',#37041,#16348,#16349);
#14244=AXIS2_PLACEMENT_3D('',#37042,#16350,#16351);
#14245=AXIS2_PLACEMENT_3D('',#37048,#16355,#16356);
#14246=AXIS2_PLACEMENT_3D('',#37052,#16359,#16360);
#14247=AXIS2_PLACEMENT_3D('',#37053,#16361,#16362);
#14248=AXIS2_PLACEMENT_3D('',#37054,#16363,#16364);
#14249=AXIS2_PLACEMENT_3D('',#37060,#16368,#16369);
#14250=AXIS2_PLACEMENT_3D('',#37064,#16372,#16373);
#14251=AXIS2_PLACEMENT_3D('',#37065,#16374,#16375);
#14252=AXIS2_PLACEMENT_3D('',#37066,#16376,#16377);
#14253=AXIS2_PLACEMENT_3D('',#37072,#16381,#16382);
#14254=AXIS2_PLACEMENT_3D('',#37076,#16385,#16386);
#14255=AXIS2_PLACEMENT_3D('',#37077,#16387,#16388);
#14256=AXIS2_PLACEMENT_3D('',#37078,#16389,#16390);
#14257=AXIS2_PLACEMENT_3D('',#37084,#16394,#16395);
#14258=AXIS2_PLACEMENT_3D('',#37088,#16398,#16399);
#14259=AXIS2_PLACEMENT_3D('',#37089,#16400,#16401);
#14260=AXIS2_PLACEMENT_3D('',#37090,#16402,#16403);
#14261=AXIS2_PLACEMENT_3D('',#37096,#16407,#16408);
#14262=AXIS2_PLACEMENT_3D('',#37100,#16411,#16412);
#14263=AXIS2_PLACEMENT_3D('',#37102,#16413,#16414);
#14264=AXIS2_PLACEMENT_3D('',#37103,#16415,#16416);
#14265=AXIS2_PLACEMENT_3D('',#37104,#16417,#16418);
#14266=AXIS2_PLACEMENT_3D('',#37110,#16422,#16423);
#14267=AXIS2_PLACEMENT_3D('',#37114,#16426,#16427);
#14268=AXIS2_PLACEMENT_3D('',#37115,#16428,#16429);
#14269=AXIS2_PLACEMENT_3D('',#37116,#16430,#16431);
#14270=AXIS2_PLACEMENT_3D('',#37122,#16435,#16436);
#14271=AXIS2_PLACEMENT_3D('',#37126,#16439,#16440);
#14272=AXIS2_PLACEMENT_3D('',#37127,#16441,#16442);
#14273=AXIS2_PLACEMENT_3D('',#37128,#16443,#16444);
#14274=AXIS2_PLACEMENT_3D('',#37134,#16448,#16449);
#14275=AXIS2_PLACEMENT_3D('',#37138,#16452,#16453);
#14276=AXIS2_PLACEMENT_3D('',#37139,#16454,#16455);
#14277=AXIS2_PLACEMENT_3D('',#37140,#16456,#16457);
#14278=AXIS2_PLACEMENT_3D('',#37146,#16461,#16462);
#14279=AXIS2_PLACEMENT_3D('',#37150,#16465,#16466);
#14280=AXIS2_PLACEMENT_3D('',#37151,#16467,#16468);
#14281=AXIS2_PLACEMENT_3D('',#37152,#16469,#16470);
#14282=AXIS2_PLACEMENT_3D('',#37158,#16474,#16475);
#14283=AXIS2_PLACEMENT_3D('',#37162,#16478,#16479);
#14284=AXIS2_PLACEMENT_3D('',#37163,#16480,#16481);
#14285=AXIS2_PLACEMENT_3D('',#37164,#16482,#16483);
#14286=AXIS2_PLACEMENT_3D('',#37170,#16487,#16488);
#14287=AXIS2_PLACEMENT_3D('',#37174,#16491,#16492);
#14288=AXIS2_PLACEMENT_3D('',#37175,#16493,#16494);
#14289=AXIS2_PLACEMENT_3D('',#37176,#16495,#16496);
#14290=AXIS2_PLACEMENT_3D('',#37182,#16500,#16501);
#14291=AXIS2_PLACEMENT_3D('',#37186,#16504,#16505);
#14292=AXIS2_PLACEMENT_3D('',#37187,#16506,#16507);
#14293=AXIS2_PLACEMENT_3D('',#37188,#16508,#16509);
#14294=AXIS2_PLACEMENT_3D('',#37194,#16513,#16514);
#14295=AXIS2_PLACEMENT_3D('',#37198,#16517,#16518);
#14296=AXIS2_PLACEMENT_3D('',#37199,#16519,#16520);
#14297=AXIS2_PLACEMENT_3D('',#37200,#16521,#16522);
#14298=AXIS2_PLACEMENT_3D('',#37206,#16526,#16527);
#14299=AXIS2_PLACEMENT_3D('',#37210,#16530,#16531);
#14300=AXIS2_PLACEMENT_3D('',#37211,#16532,#16533);
#14301=AXIS2_PLACEMENT_3D('',#37212,#16534,#16535);
#14302=AXIS2_PLACEMENT_3D('',#37218,#16539,#16540);
#14303=AXIS2_PLACEMENT_3D('',#37222,#16543,#16544);
#14304=AXIS2_PLACEMENT_3D('',#37223,#16545,#16546);
#14305=AXIS2_PLACEMENT_3D('',#37224,#16547,#16548);
#14306=AXIS2_PLACEMENT_3D('',#37230,#16552,#16553);
#14307=AXIS2_PLACEMENT_3D('',#37234,#16556,#16557);
#14308=AXIS2_PLACEMENT_3D('',#37235,#16558,#16559);
#14309=AXIS2_PLACEMENT_3D('',#37236,#16560,#16561);
#14310=AXIS2_PLACEMENT_3D('',#37242,#16565,#16566);
#14311=AXIS2_PLACEMENT_3D('',#37246,#16569,#16570);
#14312=AXIS2_PLACEMENT_3D('',#37247,#16571,#16572);
#14313=AXIS2_PLACEMENT_3D('',#37248,#16573,#16574);
#14314=AXIS2_PLACEMENT_3D('',#37254,#16578,#16579);
#14315=AXIS2_PLACEMENT_3D('',#37258,#16582,#16583);
#14316=AXIS2_PLACEMENT_3D('',#37259,#16584,#16585);
#14317=AXIS2_PLACEMENT_3D('',#37260,#16586,#16587);
#14318=AXIS2_PLACEMENT_3D('',#37266,#16591,#16592);
#14319=AXIS2_PLACEMENT_3D('',#37270,#16595,#16596);
#14320=AXIS2_PLACEMENT_3D('',#37271,#16597,#16598);
#14321=AXIS2_PLACEMENT_3D('',#37272,#16599,#16600);
#14322=AXIS2_PLACEMENT_3D('',#37278,#16604,#16605);
#14323=AXIS2_PLACEMENT_3D('',#37282,#16608,#16609);
#14324=AXIS2_PLACEMENT_3D('',#37283,#16610,#16611);
#14325=AXIS2_PLACEMENT_3D('',#37284,#16612,#16613);
#14326=AXIS2_PLACEMENT_3D('',#37290,#16617,#16618);
#14327=AXIS2_PLACEMENT_3D('',#37294,#16621,#16622);
#14328=AXIS2_PLACEMENT_3D('',#37295,#16623,#16624);
#14329=AXIS2_PLACEMENT_3D('',#37296,#16625,#16626);
#14330=AXIS2_PLACEMENT_3D('',#37302,#16630,#16631);
#14331=AXIS2_PLACEMENT_3D('',#37306,#16634,#16635);
#14332=AXIS2_PLACEMENT_3D('',#37307,#16636,#16637);
#14333=AXIS2_PLACEMENT_3D('',#37308,#16638,#16639);
#14334=AXIS2_PLACEMENT_3D('',#37314,#16643,#16644);
#14335=AXIS2_PLACEMENT_3D('',#37318,#16647,#16648);
#14336=AXIS2_PLACEMENT_3D('',#37319,#16649,#16650);
#14337=AXIS2_PLACEMENT_3D('',#37320,#16651,#16652);
#14338=AXIS2_PLACEMENT_3D('',#37322,#16654,#16655);
#14339=AXIS2_PLACEMENT_3D('',#37335,#16662,#16663);
#14340=AXIS2_PLACEMENT_3D('',#37339,#16665,#16666);
#14341=AXIS2_PLACEMENT_3D('',#37340,#16667,#16668);
#14342=AXIS2_PLACEMENT_3D('',#37343,#16670,#16671);
#14343=AXIS2_PLACEMENT_3D('',#37344,#16672,#16673);
#14344=AXIS2_PLACEMENT_3D('',#37347,#16675,#16676);
#14345=AXIS2_PLACEMENT_3D('',#37348,#16677,#16678);
#14346=AXIS2_PLACEMENT_3D('',#37351,#16680,#16681);
#14347=AXIS2_PLACEMENT_3D('',#37352,#16682,#16683);
#14348=AXIS2_PLACEMENT_3D('',#37355,#16685,#16686);
#14349=AXIS2_PLACEMENT_3D('',#37356,#16687,#16688);
#14350=AXIS2_PLACEMENT_3D('',#37358,#16690,#16691);
#14351=AXIS2_PLACEMENT_3D('',#37359,#16692,#16693);
#14352=AXIS2_PLACEMENT_3D('',#37362,#16695,#16696);
#14353=AXIS2_PLACEMENT_3D('',#37365,#16699,#16700);
#14354=AXIS2_PLACEMENT_3D('',#37367,#16702,#16703);
#14355=AXIS2_PLACEMENT_3D('',#37369,#16705,#16706);
#14356=AXIS2_PLACEMENT_3D('',#37371,#16708,#16709);
#14357=AXIS2_PLACEMENT_3D('',#37373,#16711,#16712);
#14358=AXIS2_PLACEMENT_3D('',#37374,#16713,#16714);
#14359=AXIS2_PLACEMENT_3D('',#37375,#16715,#16716);
#14360=AXIS2_PLACEMENT_3D('',#37511,#16718,#16719);
#14361=AXIS2_PLACEMENT_3D('',#37597,#16720,#16721);
#14362=AXIS2_PLACEMENT_3D('',#38012,#16723,#16724);
#14363=AXIS2_PLACEMENT_3D('',#38448,#16726,#16727);
#14364=AXIS2_PLACEMENT_3D('',#38909,#16729,#16730);
#14365=AXIS2_PLACEMENT_3D('',#39448,#16732,#16733);
#14366=AXIS2_PLACEMENT_3D('',#39911,#16735,#16736);
#14367=AXIS2_PLACEMENT_3D('',#40414,#16738,#16739);
#14368=AXIS2_PLACEMENT_3D('',#40891,#16741,#16742);
#14369=AXIS2_PLACEMENT_3D('',#41350,#16744,#16745);
#14370=AXIS2_PLACEMENT_3D('',#41793,#16747,#16748);
#14371=AXIS2_PLACEMENT_3D('',#42252,#16750,#16751);
#14372=AXIS2_PLACEMENT_3D('',#42721,#16753,#16754);
#14373=AXIS2_PLACEMENT_3D('',#43178,#16756,#16757);
#14374=AXIS2_PLACEMENT_3D('',#43627,#16759,#16760);
#14375=AXIS2_PLACEMENT_3D('',#44090,#16762,#16763);
#14376=AXIS2_PLACEMENT_3D('',#44527,#16765,#16766);
#14377=AXIS2_PLACEMENT_3D('',#45008,#16768,#16769);
#14378=AXIS2_PLACEMENT_3D('',#45499,#16771,#16772);
#14379=AXIS2_PLACEMENT_3D('',#45944,#16774,#16775);
#14380=AXIS2_PLACEMENT_3D('',#46413,#16777,#16778);
#14381=AXIS2_PLACEMENT_3D('',#46839,#16780,#16781);
#14382=AXIS2_PLACEMENT_3D('',#47339,#16783,#16784);
#14383=AXIS2_PLACEMENT_3D('',#47791,#16786,#16787);
#14384=AXIS2_PLACEMENT_3D('',#48242,#16789,#16790);
#14385=AXIS2_PLACEMENT_3D('',#48694,#16792,#16793);
#14386=AXIS2_PLACEMENT_3D('',#49201,#16795,#16796);
#14387=AXIS2_PLACEMENT_3D('',#49635,#16798,#16799);
#14388=AXIS2_PLACEMENT_3D('',#49706,#16800,#16801);
#14389=AXIS2_PLACEMENT_3D('',#53294,#16802,#16803);
#14390=AXIS2_PLACEMENT_3D('',#53296,#16804,#16805);
#14391=AXIS2_PLACEMENT_3D('',#56848,#16806,#16807);
#14392=AXIS2_PLACEMENT_3D('',#57010,#16808,#16809);
#14393=AXIS2_PLACEMENT_3D('',#57139,#16810,#16811);
#14394=AXIS2_PLACEMENT_3D('',#57141,#16812,#16813);
#14395=AXIS2_PLACEMENT_3D('',#58094,#16814,#16815);
#14396=AXIS2_PLACEMENT_3D('',#58097,#16816,#16817);
#14397=AXIS2_PLACEMENT_3D('',#58180,#16818,#16819);
#14398=AXIS2_PLACEMENT_3D('',#58893,#16820,#16821);
#14399=AXIS2_PLACEMENT_3D('',#58895,#16822,#16823);
#14400=AXIS2_PLACEMENT_3D('',#58896,#16824,#16825);
#14401=AXIS2_PLACEMENT_3D('',#58897,#16826,#16827);
#14402=AXIS2_PLACEMENT_3D('',#58899,#16828,#16829);
#14403=AXIS2_PLACEMENT_3D('',#58900,#16830,#16831);
#14404=AXIS2_PLACEMENT_3D('',#58903,#16833,#16834);
#14405=AXIS2_PLACEMENT_3D('',#58904,#16835,#16836);
#14406=AXIS2_PLACEMENT_3D('',#58905,#16837,#16838);
#14407=AXIS2_PLACEMENT_3D('',#58916,#16842,#16843);
#14408=AXIS2_PLACEMENT_3D('',#58924,#16846,#16847);
#14409=AXIS2_PLACEMENT_3D('',#58925,#16848,#16849);
#14410=AXIS2_PLACEMENT_3D('',#58926,#16850,#16851);
#14411=AXIS2_PLACEMENT_3D('',#58933,#16852,#16853);
#14412=AXIS2_PLACEMENT_3D('',#58943,#16854,#16855);
#14413=AXIS2_PLACEMENT_3D('',#58953,#16856,#16857);
#14414=AXIS2_PLACEMENT_3D('',#58963,#16858,#16859);
#14415=AXIS2_PLACEMENT_3D('',#58973,#16860,#16861);
#14416=AXIS2_PLACEMENT_3D('',#58983,#16862,#16863);
#14417=AXIS2_PLACEMENT_3D('',#58993,#16864,#16865);
#14418=AXIS2_PLACEMENT_3D('',#59003,#16866,#16867);
#14419=AXIS2_PLACEMENT_3D('',#59013,#16868,#16869);
#14420=AXIS2_PLACEMENT_3D('',#59023,#16870,#16871);
#14421=AXIS2_PLACEMENT_3D('',#59033,#16872,#16873);
#14422=AXIS2_PLACEMENT_3D('',#59043,#16874,#16875);
#14423=AXIS2_PLACEMENT_3D('',#59053,#16876,#16877);
#14424=AXIS2_PLACEMENT_3D('',#59063,#16878,#16879);
#14425=AXIS2_PLACEMENT_3D('',#59073,#16880,#16881);
#14426=AXIS2_PLACEMENT_3D('',#59083,#16882,#16883);
#14427=AXIS2_PLACEMENT_3D('',#59093,#16884,#16885);
#14428=AXIS2_PLACEMENT_3D('',#59103,#16886,#16887);
#14429=AXIS2_PLACEMENT_3D('',#59112,#16888,#16889);
#14430=AXIS2_PLACEMENT_3D('',#59114,#16890,#16891);
#14431=AXIS2_PLACEMENT_3D('',#59124,#16892,#16893);
#14432=AXIS2_PLACEMENT_3D('',#59134,#16894,#16895);
#14433=AXIS2_PLACEMENT_3D('',#59144,#16896,#16897);
#14434=AXIS2_PLACEMENT_3D('',#59154,#16898,#16899);
#14435=AXIS2_PLACEMENT_3D('',#59164,#16900,#16901);
#14436=AXIS2_PLACEMENT_3D('',#59174,#16902,#16903);
#14437=AXIS2_PLACEMENT_3D('',#59184,#16904,#16905);
#14438=AXIS2_PLACEMENT_3D('',#59194,#16906,#16907);
#14439=AXIS2_PLACEMENT_3D('',#59204,#16908,#16909);
#14440=AXIS2_PLACEMENT_3D('',#59214,#16910,#16911);
#14441=AXIS2_PLACEMENT_3D('',#59224,#16912,#16913);
#14442=AXIS2_PLACEMENT_3D('',#59234,#16914,#16915);
#14443=AXIS2_PLACEMENT_3D('',#59244,#16916,#16917);
#14444=AXIS2_PLACEMENT_3D('',#59254,#16918,#16919);
#14445=AXIS2_PLACEMENT_3D('',#59264,#16920,#16921);
#14446=AXIS2_PLACEMENT_3D('',#59274,#16922,#16923);
#14447=AXIS2_PLACEMENT_3D('',#59280,#16925,#16926);
#14448=AXIS2_PLACEMENT_3D('',#59281,#16927,#16928);
#14449=AXIS2_PLACEMENT_3D('',#59284,#16929,#16930);
#14450=AXIS2_PLACEMENT_3D('',#59288,#16933,#16934);
#14451=AXIS2_PLACEMENT_3D('',#59291,#16937,#16938);
#14452=AXIS2_PLACEMENT_3D('',#59293,#16940,#16941);
#14453=AXIS2_PLACEMENT_3D('',#59296,#16942,#16943);
#14454=AXIS2_PLACEMENT_3D('',#59299,#16945,#16946);
#14455=AXIS2_PLACEMENT_3D('',#59304,#16949,#16950);
#14456=AXIS2_PLACEMENT_3D('',#59309,#16953,#16954);
#14457=AXIS2_PLACEMENT_3D('',#59314,#16957,#16958);
#14458=AXIS2_PLACEMENT_3D('',#59319,#16961,#16962);
#14459=AXIS2_PLACEMENT_3D('',#59324,#16965,#16966);
#14460=AXIS2_PLACEMENT_3D('',#59329,#16969,#16970);
#14461=AXIS2_PLACEMENT_3D('',#59334,#16973,#16974);
#14462=AXIS2_PLACEMENT_3D('',#59339,#16977,#16978);
#14463=AXIS2_PLACEMENT_3D('',#59344,#16981,#16982);
#14464=AXIS2_PLACEMENT_3D('',#59349,#16985,#16986);
#14465=AXIS2_PLACEMENT_3D('',#59354,#16989,#16990);
#14466=AXIS2_PLACEMENT_3D('',#59359,#16993,#16994);
#14467=AXIS2_PLACEMENT_3D('',#59364,#16997,#16998);
#14468=AXIS2_PLACEMENT_3D('',#59369,#17001,#17002);
#14469=AXIS2_PLACEMENT_3D('',#59374,#17005,#17006);
#14470=AXIS2_PLACEMENT_3D('',#59379,#17009,#17010);
#14471=AXIS2_PLACEMENT_3D('',#59384,#17013,#17014);
#14472=AXIS2_PLACEMENT_3D('',#59389,#17017,#17018);
#14473=AXIS2_PLACEMENT_3D('',#59394,#17021,#17022);
#14474=AXIS2_PLACEMENT_3D('',#59399,#17025,#17026);
#14475=AXIS2_PLACEMENT_3D('',#59404,#17029,#17030);
#14476=AXIS2_PLACEMENT_3D('',#59409,#17033,#17034);
#14477=AXIS2_PLACEMENT_3D('',#59414,#17037,#17038);
#14478=AXIS2_PLACEMENT_3D('',#59419,#17041,#17042);
#14479=AXIS2_PLACEMENT_3D('',#59424,#17045,#17046);
#14480=AXIS2_PLACEMENT_3D('',#59429,#17049,#17050);
#14481=AXIS2_PLACEMENT_3D('',#59434,#17053,#17054);
#14482=AXIS2_PLACEMENT_3D('',#59439,#17057,#17058);
#14483=AXIS2_PLACEMENT_3D('',#59444,#17061,#17062);
#14484=AXIS2_PLACEMENT_3D('',#59449,#17065,#17066);
#14485=AXIS2_PLACEMENT_3D('',#59454,#17069,#17070);
#14486=AXIS2_PLACEMENT_3D('',#59459,#17073,#17074);
#14487=AXIS2_PLACEMENT_3D('',#59464,#17077,#17078);
#14488=AXIS2_PLACEMENT_3D('',#59467,#17081,#17082);
#14489=AXIS2_PLACEMENT_3D('',#59471,#17085,#17086);
#14490=AXIS2_PLACEMENT_3D('',#59473,#17088,#17089);
#14491=AXIS2_PLACEMENT_3D('',#59474,#17090,#17091);
#14492=AXIS2_PLACEMENT_3D('',#59478,#17094,#17095);
#14493=AXIS2_PLACEMENT_3D('',#59480,#17097,#17098);
#14494=AXIS2_PLACEMENT_3D('',#59481,#17099,#17100);
#14495=AXIS2_PLACEMENT_3D('',#59485,#17103,#17104);
#14496=AXIS2_PLACEMENT_3D('',#59487,#17106,#17107);
#14497=AXIS2_PLACEMENT_3D('',#59488,#17108,#17109);
#14498=AXIS2_PLACEMENT_3D('',#59492,#17112,#17113);
#14499=AXIS2_PLACEMENT_3D('',#59494,#17115,#17116);
#14500=AXIS2_PLACEMENT_3D('',#59495,#17117,#17118);
#14501=AXIS2_PLACEMENT_3D('',#59499,#17121,#17122);
#14502=AXIS2_PLACEMENT_3D('',#59501,#17124,#17125);
#14503=AXIS2_PLACEMENT_3D('',#59502,#17126,#17127);
#14504=AXIS2_PLACEMENT_3D('',#59506,#17130,#17131);
#14505=AXIS2_PLACEMENT_3D('',#59508,#17133,#17134);
#14506=AXIS2_PLACEMENT_3D('',#59509,#17135,#17136);
#14507=AXIS2_PLACEMENT_3D('',#59513,#17139,#17140);
#14508=AXIS2_PLACEMENT_3D('',#59515,#17142,#17143);
#14509=AXIS2_PLACEMENT_3D('',#59516,#17144,#17145);
#14510=AXIS2_PLACEMENT_3D('',#59520,#17148,#17149);
#14511=AXIS2_PLACEMENT_3D('',#59522,#17151,#17152);
#14512=AXIS2_PLACEMENT_3D('',#59523,#17153,#17154);
#14513=AXIS2_PLACEMENT_3D('',#59527,#17157,#17158);
#14514=AXIS2_PLACEMENT_3D('',#59529,#17160,#17161);
#14515=AXIS2_PLACEMENT_3D('',#59530,#17162,#17163);
#14516=AXIS2_PLACEMENT_3D('',#59534,#17166,#17167);
#14517=AXIS2_PLACEMENT_3D('',#59536,#17169,#17170);
#14518=AXIS2_PLACEMENT_3D('',#59537,#17171,#17172);
#14519=AXIS2_PLACEMENT_3D('',#59541,#17175,#17176);
#14520=AXIS2_PLACEMENT_3D('',#59543,#17178,#17179);
#14521=AXIS2_PLACEMENT_3D('',#59544,#17180,#17181);
#14522=AXIS2_PLACEMENT_3D('',#59548,#17184,#17185);
#14523=AXIS2_PLACEMENT_3D('',#59550,#17187,#17188);
#14524=AXIS2_PLACEMENT_3D('',#59551,#17189,#17190);
#14525=AXIS2_PLACEMENT_3D('',#59555,#17193,#17194);
#14526=AXIS2_PLACEMENT_3D('',#59557,#17196,#17197);
#14527=AXIS2_PLACEMENT_3D('',#59558,#17198,#17199);
#14528=AXIS2_PLACEMENT_3D('',#59562,#17202,#17203);
#14529=AXIS2_PLACEMENT_3D('',#59564,#17205,#17206);
#14530=AXIS2_PLACEMENT_3D('',#59565,#17207,#17208);
#14531=AXIS2_PLACEMENT_3D('',#59569,#17211,#17212);
#14532=AXIS2_PLACEMENT_3D('',#59571,#17214,#17215);
#14533=AXIS2_PLACEMENT_3D('',#59572,#17216,#17217);
#14534=AXIS2_PLACEMENT_3D('',#59576,#17220,#17221);
#14535=AXIS2_PLACEMENT_3D('',#59578,#17223,#17224);
#14536=AXIS2_PLACEMENT_3D('',#59579,#17225,#17226);
#14537=AXIS2_PLACEMENT_3D('',#59583,#17229,#17230);
#14538=AXIS2_PLACEMENT_3D('',#59585,#17232,#17233);
#14539=AXIS2_PLACEMENT_3D('',#59586,#17234,#17235);
#14540=AXIS2_PLACEMENT_3D('',#59590,#17238,#17239);
#14541=AXIS2_PLACEMENT_3D('',#59592,#17241,#17242);
#14542=AXIS2_PLACEMENT_3D('',#59593,#17243,#17244);
#14543=AXIS2_PLACEMENT_3D('',#59597,#17247,#17248);
#14544=AXIS2_PLACEMENT_3D('',#59599,#17250,#17251);
#14545=AXIS2_PLACEMENT_3D('',#59600,#17252,#17253);
#14546=AXIS2_PLACEMENT_3D('',#59604,#17256,#17257);
#14547=AXIS2_PLACEMENT_3D('',#59606,#17259,#17260);
#14548=AXIS2_PLACEMENT_3D('',#59607,#17261,#17262);
#14549=AXIS2_PLACEMENT_3D('',#59611,#17265,#17266);
#14550=AXIS2_PLACEMENT_3D('',#59613,#17268,#17269);
#14551=AXIS2_PLACEMENT_3D('',#59614,#17270,#17271);
#14552=AXIS2_PLACEMENT_3D('',#59618,#17274,#17275);
#14553=AXIS2_PLACEMENT_3D('',#59620,#17277,#17278);
#14554=AXIS2_PLACEMENT_3D('',#59621,#17279,#17280);
#14555=AXIS2_PLACEMENT_3D('',#59625,#17283,#17284);
#14556=AXIS2_PLACEMENT_3D('',#59627,#17286,#17287);
#14557=AXIS2_PLACEMENT_3D('',#59628,#17288,#17289);
#14558=AXIS2_PLACEMENT_3D('',#59632,#17292,#17293);
#14559=AXIS2_PLACEMENT_3D('',#59634,#17295,#17296);
#14560=AXIS2_PLACEMENT_3D('',#59635,#17297,#17298);
#14561=AXIS2_PLACEMENT_3D('',#59639,#17301,#17302);
#14562=AXIS2_PLACEMENT_3D('',#59641,#17304,#17305);
#14563=AXIS2_PLACEMENT_3D('',#59642,#17306,#17307);
#14564=AXIS2_PLACEMENT_3D('',#59646,#17310,#17311);
#14565=AXIS2_PLACEMENT_3D('',#59648,#17313,#17314);
#14566=AXIS2_PLACEMENT_3D('',#59649,#17315,#17316);
#14567=AXIS2_PLACEMENT_3D('',#59653,#17319,#17320);
#14568=AXIS2_PLACEMENT_3D('',#59655,#17322,#17323);
#14569=AXIS2_PLACEMENT_3D('',#59656,#17324,#17325);
#14570=AXIS2_PLACEMENT_3D('',#59660,#17328,#17329);
#14571=AXIS2_PLACEMENT_3D('',#59662,#17331,#17332);
#14572=AXIS2_PLACEMENT_3D('',#59663,#17333,#17334);
#14573=AXIS2_PLACEMENT_3D('',#59667,#17337,#17338);
#14574=AXIS2_PLACEMENT_3D('',#59669,#17340,#17341);
#14575=AXIS2_PLACEMENT_3D('',#59670,#17342,#17343);
#14576=AXIS2_PLACEMENT_3D('',#59674,#17346,#17347);
#14577=AXIS2_PLACEMENT_3D('',#59676,#17349,#17350);
#14578=AXIS2_PLACEMENT_3D('',#59677,#17351,#17352);
#14579=AXIS2_PLACEMENT_3D('',#59681,#17355,#17356);
#14580=AXIS2_PLACEMENT_3D('',#59683,#17358,#17359);
#14581=AXIS2_PLACEMENT_3D('',#59684,#17360,#17361);
#14582=AXIS2_PLACEMENT_3D('',#59688,#17364,#17365);
#14583=AXIS2_PLACEMENT_3D('',#59690,#17367,#17368);
#14584=AXIS2_PLACEMENT_3D('',#59691,#17369,#17370);
#14585=AXIS2_PLACEMENT_3D('',#59695,#17373,#17374);
#14586=AXIS2_PLACEMENT_3D('',#59697,#17376,#17377);
#14587=AXIS2_PLACEMENT_3D('',#59698,#17378,#17379);
#14588=AXIS2_PLACEMENT_3D('',#59702,#17382,#17383);
#14589=AXIS2_PLACEMENT_3D('',#59704,#17385,#17386);
#14590=AXIS2_PLACEMENT_3D('',#59705,#17387,#17388);
#14591=AXIS2_PLACEMENT_3D('',#59718,#17395,#17396);
#14592=AXIS2_PLACEMENT_3D('',#59722,#17398,#17399);
#14593=AXIS2_PLACEMENT_3D('',#59723,#17400,#17401);
#14594=AXIS2_PLACEMENT_3D('',#59726,#17403,#17404);
#14595=AXIS2_PLACEMENT_3D('',#59727,#17405,#17406);
#14596=AXIS2_PLACEMENT_3D('',#59730,#17408,#17409);
#14597=AXIS2_PLACEMENT_3D('',#59731,#17410,#17411);
#14598=AXIS2_PLACEMENT_3D('',#59734,#17413,#17414);
#14599=AXIS2_PLACEMENT_3D('',#59735,#17415,#17416);
#14600=AXIS2_PLACEMENT_3D('',#59738,#17418,#17419);
#14601=AXIS2_PLACEMENT_3D('',#59739,#17420,#17421);
#14602=AXIS2_PLACEMENT_3D('',#59741,#17423,#17424);
#14603=AXIS2_PLACEMENT_3D('',#59742,#17425,#17426);
#14604=AXIS2_PLACEMENT_3D('',#59745,#17428,#17429);
#14605=AXIS2_PLACEMENT_3D('',#59748,#17432,#17433);
#14606=AXIS2_PLACEMENT_3D('',#59750,#17435,#17436);
#14607=AXIS2_PLACEMENT_3D('',#59752,#17438,#17439);
#14608=AXIS2_PLACEMENT_3D('',#59754,#17441,#17442);
#14609=AXIS2_PLACEMENT_3D('',#59756,#17444,#17445);
#14610=AXIS2_PLACEMENT_3D('',#59757,#17446,#17447);
#14611=AXIS2_PLACEMENT_3D('',#59758,#17448,#17449);
#14612=AXIS2_PLACEMENT_3D('',#59918,#17451,#17452);
#14613=AXIS2_PLACEMENT_3D('',#60031,#17453,#17454);
#14614=AXIS2_PLACEMENT_3D('',#60431,#17456,#17457);
#14615=AXIS2_PLACEMENT_3D('',#60647,#17459,#17460);
#14616=AXIS2_PLACEMENT_3D('',#60869,#17462,#17463);
#14617=AXIS2_PLACEMENT_3D('',#61252,#17465,#17466);
#14618=AXIS2_PLACEMENT_3D('',#61637,#17468,#17469);
#14619=AXIS2_PLACEMENT_3D('',#62094,#17471,#17472);
#14620=AXIS2_PLACEMENT_3D('',#62577,#17474,#17475);
#14621=AXIS2_PLACEMENT_3D('',#63072,#17477,#17478);
#14622=AXIS2_PLACEMENT_3D('',#63303,#17480,#17481);
#14623=AXIS2_PLACEMENT_3D('',#63540,#17483,#17484);
#14624=AXIS2_PLACEMENT_3D('',#63911,#17486,#17487);
#14625=AXIS2_PLACEMENT_3D('',#64379,#17489,#17490);
#14626=AXIS2_PLACEMENT_3D('',#64761,#17492,#17493);
#14627=AXIS2_PLACEMENT_3D('',#64835,#17494,#17495);
#14628=AXIS2_PLACEMENT_3D('',#67071,#17496,#17497);
#14629=AXIS2_PLACEMENT_3D('',#69226,#17498,#17499);
#14630=AXIS2_PLACEMENT_3D('',#69407,#17500,#17501);
#14631=AXIS2_PLACEMENT_3D('',#69554,#17502,#17503);
#14632=AXIS2_PLACEMENT_3D('',#69557,#17504,#17505);
#14633=AXIS2_PLACEMENT_3D('',#69745,#17506,#17507);
#14634=AXIS2_PLACEMENT_3D('',#70226,#17508,#17509);
#14635=AXIS2_PLACEMENT_3D('',#70229,#17510,#17511);
#14636=AXIS2_PLACEMENT_3D('',#70321,#17512,#17513);
#14637=AXIS2_PLACEMENT_3D('',#70714,#17514,#17515);
#14638=AXIS2_PLACEMENT_3D('',#70716,#17516,#17517);
#14639=AXIS2_PLACEMENT_3D('',#70717,#17518,#17519);
#14640=AXIS2_PLACEMENT_3D('',#70718,#17520,#17521);
#14641=AXIS2_PLACEMENT_3D('',#70720,#17522,#17523);
#14642=AXIS2_PLACEMENT_3D('',#70721,#17524,#17525);
#14643=AXIS2_PLACEMENT_3D('',#70724,#17527,#17528);
#14644=AXIS2_PLACEMENT_3D('',#70725,#17529,#17530);
#14645=AXIS2_PLACEMENT_3D('',#70726,#17531,#17532);
#14646=AXIS2_PLACEMENT_3D('',#70737,#17536,#17537);
#14647=AXIS2_PLACEMENT_3D('',#70745,#17540,#17541);
#14648=AXIS2_PLACEMENT_3D('',#70746,#17542,#17543);
#14649=AXIS2_PLACEMENT_3D('',#70747,#17544,#17545);
#14650=AXIS2_PLACEMENT_3D('',#70754,#17546,#17547);
#14651=AXIS2_PLACEMENT_3D('',#70764,#17548,#17549);
#14652=AXIS2_PLACEMENT_3D('',#70774,#17550,#17551);
#14653=AXIS2_PLACEMENT_3D('',#70784,#17552,#17553);
#14654=AXIS2_PLACEMENT_3D('',#70794,#17554,#17555);
#14655=AXIS2_PLACEMENT_3D('',#70804,#17556,#17557);
#14656=AXIS2_PLACEMENT_3D('',#70814,#17558,#17559);
#14657=AXIS2_PLACEMENT_3D('',#70824,#17560,#17561);
#14658=AXIS2_PLACEMENT_3D('',#70834,#17562,#17563);
#14659=AXIS2_PLACEMENT_3D('',#70844,#17564,#17565);
#14660=AXIS2_PLACEMENT_3D('',#70854,#17566,#17567);
#14661=AXIS2_PLACEMENT_3D('',#70864,#17568,#17569);
#14662=AXIS2_PLACEMENT_3D('',#70874,#17570,#17571);
#14663=AXIS2_PLACEMENT_3D('',#70884,#17572,#17573);
#14664=AXIS2_PLACEMENT_3D('',#70894,#17574,#17575);
#14665=AXIS2_PLACEMENT_3D('',#70904,#17576,#17577);
#14666=AXIS2_PLACEMENT_3D('',#70914,#17578,#17579);
#14667=AXIS2_PLACEMENT_3D('',#70924,#17580,#17581);
#14668=AXIS2_PLACEMENT_3D('',#70933,#17582,#17583);
#14669=AXIS2_PLACEMENT_3D('',#70935,#17584,#17585);
#14670=AXIS2_PLACEMENT_3D('',#70945,#17586,#17587);
#14671=AXIS2_PLACEMENT_3D('',#70955,#17588,#17589);
#14672=AXIS2_PLACEMENT_3D('',#70965,#17590,#17591);
#14673=AXIS2_PLACEMENT_3D('',#70975,#17592,#17593);
#14674=AXIS2_PLACEMENT_3D('',#70985,#17594,#17595);
#14675=AXIS2_PLACEMENT_3D('',#70995,#17596,#17597);
#14676=AXIS2_PLACEMENT_3D('',#71005,#17598,#17599);
#14677=AXIS2_PLACEMENT_3D('',#71015,#17600,#17601);
#14678=AXIS2_PLACEMENT_3D('',#71025,#17602,#17603);
#14679=AXIS2_PLACEMENT_3D('',#71035,#17604,#17605);
#14680=AXIS2_PLACEMENT_3D('',#71045,#17606,#17607);
#14681=AXIS2_PLACEMENT_3D('',#71055,#17608,#17609);
#14682=AXIS2_PLACEMENT_3D('',#71065,#17610,#17611);
#14683=AXIS2_PLACEMENT_3D('',#71075,#17612,#17613);
#14684=AXIS2_PLACEMENT_3D('',#71085,#17614,#17615);
#14685=AXIS2_PLACEMENT_3D('',#71095,#17616,#17617);
#14686=AXIS2_PLACEMENT_3D('',#71101,#17619,#17620);
#14687=AXIS2_PLACEMENT_3D('',#71102,#17621,#17622);
#14688=AXIS2_PLACEMENT_3D('',#71108,#17626,#17627);
#14689=AXIS2_PLACEMENT_3D('',#71112,#17630,#17631);
#14690=AXIS2_PLACEMENT_3D('',#71113,#17632,#17633);
#14691=AXIS2_PLACEMENT_3D('',#71114,#17634,#17635);
#14692=AXIS2_PLACEMENT_3D('',#71120,#17639,#17640);
#14693=AXIS2_PLACEMENT_3D('',#71124,#17643,#17644);
#14694=AXIS2_PLACEMENT_3D('',#71125,#17645,#17646);
#14695=AXIS2_PLACEMENT_3D('',#71126,#17647,#17648);
#14696=AXIS2_PLACEMENT_3D('',#71132,#17652,#17653);
#14697=AXIS2_PLACEMENT_3D('',#71136,#17656,#17657);
#14698=AXIS2_PLACEMENT_3D('',#71137,#17658,#17659);
#14699=AXIS2_PLACEMENT_3D('',#71138,#17660,#17661);
#14700=AXIS2_PLACEMENT_3D('',#71144,#17665,#17666);
#14701=AXIS2_PLACEMENT_3D('',#71148,#17669,#17670);
#14702=AXIS2_PLACEMENT_3D('',#71149,#17671,#17672);
#14703=AXIS2_PLACEMENT_3D('',#71150,#17673,#17674);
#14704=AXIS2_PLACEMENT_3D('',#71156,#17678,#17679);
#14705=AXIS2_PLACEMENT_3D('',#71160,#17682,#17683);
#14706=AXIS2_PLACEMENT_3D('',#71161,#17684,#17685);
#14707=AXIS2_PLACEMENT_3D('',#71162,#17686,#17687);
#14708=AXIS2_PLACEMENT_3D('',#71168,#17691,#17692);
#14709=AXIS2_PLACEMENT_3D('',#71172,#17695,#17696);
#14710=AXIS2_PLACEMENT_3D('',#71173,#17697,#17698);
#14711=AXIS2_PLACEMENT_3D('',#71174,#17699,#17700);
#14712=AXIS2_PLACEMENT_3D('',#71180,#17704,#17705);
#14713=AXIS2_PLACEMENT_3D('',#71184,#17708,#17709);
#14714=AXIS2_PLACEMENT_3D('',#71185,#17710,#17711);
#14715=AXIS2_PLACEMENT_3D('',#71186,#17712,#17713);
#14716=AXIS2_PLACEMENT_3D('',#71192,#17717,#17718);
#14717=AXIS2_PLACEMENT_3D('',#71196,#17721,#17722);
#14718=AXIS2_PLACEMENT_3D('',#71197,#17723,#17724);
#14719=AXIS2_PLACEMENT_3D('',#71198,#17725,#17726);
#14720=AXIS2_PLACEMENT_3D('',#71204,#17730,#17731);
#14721=AXIS2_PLACEMENT_3D('',#71208,#17734,#17735);
#14722=AXIS2_PLACEMENT_3D('',#71209,#17736,#17737);
#14723=AXIS2_PLACEMENT_3D('',#71210,#17738,#17739);
#14724=AXIS2_PLACEMENT_3D('',#71216,#17743,#17744);
#14725=AXIS2_PLACEMENT_3D('',#71220,#17747,#17748);
#14726=AXIS2_PLACEMENT_3D('',#71221,#17749,#17750);
#14727=AXIS2_PLACEMENT_3D('',#71222,#17751,#17752);
#14728=AXIS2_PLACEMENT_3D('',#71228,#17756,#17757);
#14729=AXIS2_PLACEMENT_3D('',#71232,#17760,#17761);
#14730=AXIS2_PLACEMENT_3D('',#71233,#17762,#17763);
#14731=AXIS2_PLACEMENT_3D('',#71234,#17764,#17765);
#14732=AXIS2_PLACEMENT_3D('',#71240,#17769,#17770);
#14733=AXIS2_PLACEMENT_3D('',#71244,#17773,#17774);
#14734=AXIS2_PLACEMENT_3D('',#71245,#17775,#17776);
#14735=AXIS2_PLACEMENT_3D('',#71246,#17777,#17778);
#14736=AXIS2_PLACEMENT_3D('',#71252,#17782,#17783);
#14737=AXIS2_PLACEMENT_3D('',#71256,#17786,#17787);
#14738=AXIS2_PLACEMENT_3D('',#71257,#17788,#17789);
#14739=AXIS2_PLACEMENT_3D('',#71258,#17790,#17791);
#14740=AXIS2_PLACEMENT_3D('',#71264,#17795,#17796);
#14741=AXIS2_PLACEMENT_3D('',#71268,#17799,#17800);
#14742=AXIS2_PLACEMENT_3D('',#71269,#17801,#17802);
#14743=AXIS2_PLACEMENT_3D('',#71270,#17803,#17804);
#14744=AXIS2_PLACEMENT_3D('',#71276,#17808,#17809);
#14745=AXIS2_PLACEMENT_3D('',#71280,#17812,#17813);
#14746=AXIS2_PLACEMENT_3D('',#71281,#17814,#17815);
#14747=AXIS2_PLACEMENT_3D('',#71282,#17816,#17817);
#14748=AXIS2_PLACEMENT_3D('',#71288,#17821,#17822);
#14749=AXIS2_PLACEMENT_3D('',#71292,#17825,#17826);
#14750=AXIS2_PLACEMENT_3D('',#71293,#17827,#17828);
#14751=AXIS2_PLACEMENT_3D('',#71294,#17829,#17830);
#14752=AXIS2_PLACEMENT_3D('',#71300,#17834,#17835);
#14753=AXIS2_PLACEMENT_3D('',#71304,#17838,#17839);
#14754=AXIS2_PLACEMENT_3D('',#71306,#17840,#17841);
#14755=AXIS2_PLACEMENT_3D('',#71307,#17842,#17843);
#14756=AXIS2_PLACEMENT_3D('',#71308,#17844,#17845);
#14757=AXIS2_PLACEMENT_3D('',#71314,#17849,#17850);
#14758=AXIS2_PLACEMENT_3D('',#71318,#17853,#17854);
#14759=AXIS2_PLACEMENT_3D('',#71319,#17855,#17856);
#14760=AXIS2_PLACEMENT_3D('',#71320,#17857,#17858);
#14761=AXIS2_PLACEMENT_3D('',#71326,#17862,#17863);
#14762=AXIS2_PLACEMENT_3D('',#71330,#17866,#17867);
#14763=AXIS2_PLACEMENT_3D('',#71331,#17868,#17869);
#14764=AXIS2_PLACEMENT_3D('',#71332,#17870,#17871);
#14765=AXIS2_PLACEMENT_3D('',#71338,#17875,#17876);
#14766=AXIS2_PLACEMENT_3D('',#71342,#17879,#17880);
#14767=AXIS2_PLACEMENT_3D('',#71343,#17881,#17882);
#14768=AXIS2_PLACEMENT_3D('',#71344,#17883,#17884);
#14769=AXIS2_PLACEMENT_3D('',#71350,#17888,#17889);
#14770=AXIS2_PLACEMENT_3D('',#71354,#17892,#17893);
#14771=AXIS2_PLACEMENT_3D('',#71355,#17894,#17895);
#14772=AXIS2_PLACEMENT_3D('',#71356,#17896,#17897);
#14773=AXIS2_PLACEMENT_3D('',#71362,#17901,#17902);
#14774=AXIS2_PLACEMENT_3D('',#71366,#17905,#17906);
#14775=AXIS2_PLACEMENT_3D('',#71367,#17907,#17908);
#14776=AXIS2_PLACEMENT_3D('',#71368,#17909,#17910);
#14777=AXIS2_PLACEMENT_3D('',#71374,#17914,#17915);
#14778=AXIS2_PLACEMENT_3D('',#71378,#17918,#17919);
#14779=AXIS2_PLACEMENT_3D('',#71379,#17920,#17921);
#14780=AXIS2_PLACEMENT_3D('',#71380,#17922,#17923);
#14781=AXIS2_PLACEMENT_3D('',#71386,#17927,#17928);
#14782=AXIS2_PLACEMENT_3D('',#71390,#17931,#17932);
#14783=AXIS2_PLACEMENT_3D('',#71391,#17933,#17934);
#14784=AXIS2_PLACEMENT_3D('',#71392,#17935,#17936);
#14785=AXIS2_PLACEMENT_3D('',#71398,#17940,#17941);
#14786=AXIS2_PLACEMENT_3D('',#71402,#17944,#17945);
#14787=AXIS2_PLACEMENT_3D('',#71403,#17946,#17947);
#14788=AXIS2_PLACEMENT_3D('',#71404,#17948,#17949);
#14789=AXIS2_PLACEMENT_3D('',#71410,#17953,#17954);
#14790=AXIS2_PLACEMENT_3D('',#71414,#17957,#17958);
#14791=AXIS2_PLACEMENT_3D('',#71415,#17959,#17960);
#14792=AXIS2_PLACEMENT_3D('',#71416,#17961,#17962);
#14793=AXIS2_PLACEMENT_3D('',#71422,#17966,#17967);
#14794=AXIS2_PLACEMENT_3D('',#71426,#17970,#17971);
#14795=AXIS2_PLACEMENT_3D('',#71427,#17972,#17973);
#14796=AXIS2_PLACEMENT_3D('',#71428,#17974,#17975);
#14797=AXIS2_PLACEMENT_3D('',#71434,#17979,#17980);
#14798=AXIS2_PLACEMENT_3D('',#71438,#17983,#17984);
#14799=AXIS2_PLACEMENT_3D('',#71439,#17985,#17986);
#14800=AXIS2_PLACEMENT_3D('',#71440,#17987,#17988);
#14801=AXIS2_PLACEMENT_3D('',#71446,#17992,#17993);
#14802=AXIS2_PLACEMENT_3D('',#71450,#17996,#17997);
#14803=AXIS2_PLACEMENT_3D('',#71451,#17998,#17999);
#14804=AXIS2_PLACEMENT_3D('',#71452,#18000,#18001);
#14805=AXIS2_PLACEMENT_3D('',#71458,#18005,#18006);
#14806=AXIS2_PLACEMENT_3D('',#71462,#18009,#18010);
#14807=AXIS2_PLACEMENT_3D('',#71463,#18011,#18012);
#14808=AXIS2_PLACEMENT_3D('',#71464,#18013,#18014);
#14809=AXIS2_PLACEMENT_3D('',#71470,#18018,#18019);
#14810=AXIS2_PLACEMENT_3D('',#71474,#18022,#18023);
#14811=AXIS2_PLACEMENT_3D('',#71475,#18024,#18025);
#14812=AXIS2_PLACEMENT_3D('',#71476,#18026,#18027);
#14813=AXIS2_PLACEMENT_3D('',#71482,#18031,#18032);
#14814=AXIS2_PLACEMENT_3D('',#71486,#18035,#18036);
#14815=AXIS2_PLACEMENT_3D('',#71487,#18037,#18038);
#14816=AXIS2_PLACEMENT_3D('',#71488,#18039,#18040);
#14817=AXIS2_PLACEMENT_3D('',#71494,#18044,#18045);
#14818=AXIS2_PLACEMENT_3D('',#71498,#18048,#18049);
#14819=AXIS2_PLACEMENT_3D('',#71499,#18050,#18051);
#14820=AXIS2_PLACEMENT_3D('',#71500,#18052,#18053);
#14821=AXIS2_PLACEMENT_3D('',#71506,#18057,#18058);
#14822=AXIS2_PLACEMENT_3D('',#71510,#18061,#18062);
#14823=AXIS2_PLACEMENT_3D('',#71511,#18063,#18064);
#14824=AXIS2_PLACEMENT_3D('',#71512,#18065,#18066);
#14825=AXIS2_PLACEMENT_3D('',#71518,#18070,#18071);
#14826=AXIS2_PLACEMENT_3D('',#71522,#18074,#18075);
#14827=AXIS2_PLACEMENT_3D('',#71523,#18076,#18077);
#14828=AXIS2_PLACEMENT_3D('',#71524,#18078,#18079);
#14829=AXIS2_PLACEMENT_3D('',#71526,#18081,#18082);
#14830=AXIS2_PLACEMENT_3D('',#71539,#18089,#18090);
#14831=AXIS2_PLACEMENT_3D('',#71543,#18092,#18093);
#14832=AXIS2_PLACEMENT_3D('',#71544,#18094,#18095);
#14833=AXIS2_PLACEMENT_3D('',#71547,#18097,#18098);
#14834=AXIS2_PLACEMENT_3D('',#71548,#18099,#18100);
#14835=AXIS2_PLACEMENT_3D('',#71551,#18102,#18103);
#14836=AXIS2_PLACEMENT_3D('',#71552,#18104,#18105);
#14837=AXIS2_PLACEMENT_3D('',#71555,#18107,#18108);
#14838=AXIS2_PLACEMENT_3D('',#71556,#18109,#18110);
#14839=AXIS2_PLACEMENT_3D('',#71559,#18112,#18113);
#14840=AXIS2_PLACEMENT_3D('',#71560,#18114,#18115);
#14841=AXIS2_PLACEMENT_3D('',#71562,#18117,#18118);
#14842=AXIS2_PLACEMENT_3D('',#71563,#18119,#18120);
#14843=AXIS2_PLACEMENT_3D('',#71566,#18122,#18123);
#14844=AXIS2_PLACEMENT_3D('',#71569,#18126,#18127);
#14845=AXIS2_PLACEMENT_3D('',#71571,#18129,#18130);
#14846=AXIS2_PLACEMENT_3D('',#71573,#18132,#18133);
#14847=AXIS2_PLACEMENT_3D('',#71575,#18135,#18136);
#14848=AXIS2_PLACEMENT_3D('',#71577,#18138,#18139);
#14849=AXIS2_PLACEMENT_3D('',#71578,#18140,#18141);
#14850=AXIS2_PLACEMENT_3D('',#71579,#18142,#18143);
#14851=AXIS2_PLACEMENT_3D('',#71580,#18144,#18145);
#14852=AXIS2_PLACEMENT_3D('',#71581,#18146,#18147);
#14853=AXIS2_PLACEMENT_3D('',#71582,#18148,#18149);
#14854=AXIS2_PLACEMENT_3D('',#71583,#18150,#18151);
#14855=AXIS2_PLACEMENT_3D('',#71584,#18152,#18153);
#14856=AXIS2_PLACEMENT_3D('',#71585,#18154,#18155);
#14857=AXIS2_PLACEMENT_3D('',#71586,#18156,#18157);
#14858=AXIS2_PLACEMENT_3D('',#71587,#18158,#18159);
#14859=AXIS2_PLACEMENT_3D('',#71588,#18160,#18161);
#14860=AXIS2_PLACEMENT_3D('',#71589,#18162,#18163);
#14861=AXIS2_PLACEMENT_3D('',#71590,#18164,#18165);
#14862=AXIS2_PLACEMENT_3D('',#71591,#18166,#18167);
#14863=AXIS2_PLACEMENT_3D('',#71592,#18168,#18169);
#14864=AXIS2_PLACEMENT_3D('',#71593,#18170,#18171);
#14865=AXIS2_PLACEMENT_3D('',#71594,#18172,#18173);
#14866=AXIS2_PLACEMENT_3D('',#71595,#18174,#18175);
#14867=AXIS2_PLACEMENT_3D('',#71596,#18176,#18177);
#14868=AXIS2_PLACEMENT_3D('',#71597,#18178,#18179);
#14869=AXIS2_PLACEMENT_3D('',#71598,#18180,#18181);
#14870=AXIS2_PLACEMENT_3D('',#71599,#18182,#18183);
#14871=AXIS2_PLACEMENT_3D('',#71600,#18184,#18185);
#14872=AXIS2_PLACEMENT_3D('',#71601,#18186,#18187);
#14873=AXIS2_PLACEMENT_3D('',#71602,#18188,#18189);
#14874=AXIS2_PLACEMENT_3D('',#71603,#18190,#18191);
#14875=AXIS2_PLACEMENT_3D('',#71604,#18192,#18193);
#14876=AXIS2_PLACEMENT_3D('',#71605,#18194,#18195);
#14877=AXIS2_PLACEMENT_3D('',#71606,#18196,#18197);
#14878=AXIS2_PLACEMENT_3D('',#71607,#18198,#18199);
#14879=AXIS2_PLACEMENT_3D('',#71608,#18200,#18201);
#14880=AXIS2_PLACEMENT_3D('',#71609,#18202,#18203);
#14881=AXIS2_PLACEMENT_3D('',#71610,#18204,#18205);
#14882=AXIS2_PLACEMENT_3D('',#71611,#18206,#18207);
#14883=AXIS2_PLACEMENT_3D('',#71612,#18208,#18209);
#14884=AXIS2_PLACEMENT_3D('',#71613,#18210,#18211);
#14885=AXIS2_PLACEMENT_3D('',#71614,#18212,#18213);
#14886=AXIS2_PLACEMENT_3D('',#71615,#18214,#18215);
#14887=AXIS2_PLACEMENT_3D('',#71616,#18216,#18217);
#14888=AXIS2_PLACEMENT_3D('',#71617,#18218,#18219);
#14889=AXIS2_PLACEMENT_3D('',#71618,#18220,#18221);
#14890=AXIS2_PLACEMENT_3D('',#71619,#18222,#18223);
#14891=AXIS2_PLACEMENT_3D('',#71620,#18224,#18225);
#14892=AXIS2_PLACEMENT_3D('',#71621,#18226,#18227);
#14893=AXIS2_PLACEMENT_3D('',#71622,#18228,#18229);
#14894=AXIS2_PLACEMENT_3D('',#71623,#18230,#18231);
#14895=AXIS2_PLACEMENT_3D('',#71624,#18232,#18233);
#14896=AXIS2_PLACEMENT_3D('',#71625,#18234,#18235);
#14897=AXIS2_PLACEMENT_3D('',#71626,#18236,#18237);
#14898=AXIS2_PLACEMENT_3D('',#71627,#18238,#18239);
#14899=AXIS2_PLACEMENT_3D('',#71628,#18240,#18241);
#14900=AXIS2_PLACEMENT_3D('',#71629,#18242,#18243);
#14901=AXIS2_PLACEMENT_3D('',#71630,#18244,#18245);
#14902=AXIS2_PLACEMENT_3D('',#71631,#18246,#18247);
#14903=AXIS2_PLACEMENT_3D('',#71632,#18248,#18249);
#14904=AXIS2_PLACEMENT_3D('',#71633,#18250,#18251);
#14905=AXIS2_PLACEMENT_3D('',#71634,#18252,#18253);
#14906=AXIS2_PLACEMENT_3D('',#71635,#18254,#18255);
#14907=AXIS2_PLACEMENT_3D('',#71636,#18256,#18257);
#14908=AXIS2_PLACEMENT_3D('',#71637,#18258,#18259);
#14909=AXIS2_PLACEMENT_3D('',#71638,#18260,#18261);
#14910=AXIS2_PLACEMENT_3D('',#71639,#18262,#18263);
#14911=AXIS2_PLACEMENT_3D('',#71640,#18264,#18265);
#14912=AXIS2_PLACEMENT_3D('',#71641,#18266,#18267);
#14913=AXIS2_PLACEMENT_3D('',#71642,#18268,#18269);
#14914=AXIS2_PLACEMENT_3D('',#71643,#18270,#18271);
#14915=AXIS2_PLACEMENT_3D('',#71644,#18272,#18273);
#14916=AXIS2_PLACEMENT_3D('',#71645,#18274,#18275);
#14917=AXIS2_PLACEMENT_3D('',#71646,#18276,#18277);
#14918=AXIS2_PLACEMENT_3D('',#71647,#18278,#18279);
#14919=AXIS2_PLACEMENT_3D('',#71648,#18280,#18281);
#14920=AXIS2_PLACEMENT_3D('',#71649,#18282,#18283);
#14921=AXIS2_PLACEMENT_3D('',#71650,#18284,#18285);
#14922=AXIS2_PLACEMENT_3D('',#71651,#18286,#18287);
#14923=AXIS2_PLACEMENT_3D('',#71652,#18288,#18289);
#14924=AXIS2_PLACEMENT_3D('',#71653,#18290,#18291);
#14925=AXIS2_PLACEMENT_3D('',#71654,#18292,#18293);
#14926=AXIS2_PLACEMENT_3D('',#71655,#18294,#18295);
#14927=AXIS2_PLACEMENT_3D('',#71656,#18296,#18297);
#14928=AXIS2_PLACEMENT_3D('',#71657,#18298,#18299);
#14929=AXIS2_PLACEMENT_3D('',#71658,#18300,#18301);
#14930=AXIS2_PLACEMENT_3D('',#71659,#18302,#18303);
#14931=AXIS2_PLACEMENT_3D('',#71660,#18304,#18305);
#14932=AXIS2_PLACEMENT_3D('',#71661,#18306,#18307);
#14933=AXIS2_PLACEMENT_3D('',#71662,#18308,#18309);
#14934=AXIS2_PLACEMENT_3D('',#71663,#18310,#18311);
#14935=AXIS2_PLACEMENT_3D('',#71664,#18312,#18313);
#14936=AXIS2_PLACEMENT_3D('',#71665,#18314,#18315);
#14937=AXIS2_PLACEMENT_3D('',#71666,#18316,#18317);
#14938=AXIS2_PLACEMENT_3D('',#71667,#18318,#18319);
#14939=AXIS2_PLACEMENT_3D('',#71668,#18320,#18321);
#14940=AXIS2_PLACEMENT_3D('',#71669,#18322,#18323);
#14941=AXIS2_PLACEMENT_3D('',#71670,#18324,#18325);
#14942=AXIS2_PLACEMENT_3D('',#71671,#18326,#18327);
#14943=AXIS2_PLACEMENT_3D('',#71672,#18328,#18329);
#14944=AXIS2_PLACEMENT_3D('',#71673,#18330,#18331);
#14945=AXIS2_PLACEMENT_3D('',#71674,#18332,#18333);
#14946=AXIS2_PLACEMENT_3D('',#71675,#18334,#18335);
#14947=AXIS2_PLACEMENT_3D('',#71676,#18336,#18337);
#14948=AXIS2_PLACEMENT_3D('',#71677,#18338,#18339);
#14949=AXIS2_PLACEMENT_3D('',#71678,#18340,#18341);
#14950=AXIS2_PLACEMENT_3D('',#71679,#18342,#18343);
#14951=AXIS2_PLACEMENT_3D('',#71680,#18344,#18345);
#14952=AXIS2_PLACEMENT_3D('',#71681,#18346,#18347);
#14953=AXIS2_PLACEMENT_3D('',#71682,#18348,#18349);
#14954=AXIS2_PLACEMENT_3D('',#71683,#18350,#18351);
#14955=AXIS2_PLACEMENT_3D('',#71684,#18352,#18353);
#14956=AXIS2_PLACEMENT_3D('',#71685,#18354,#18355);
#14957=AXIS2_PLACEMENT_3D('',#71686,#18356,#18357);
#14958=AXIS2_PLACEMENT_3D('',#71687,#18358,#18359);
#14959=AXIS2_PLACEMENT_3D('',#71688,#18360,#18361);
#14960=AXIS2_PLACEMENT_3D('',#71689,#18362,#18363);
#14961=AXIS2_PLACEMENT_3D('',#71690,#18364,#18365);
#14962=AXIS2_PLACEMENT_3D('',#71691,#18366,#18367);
#14963=AXIS2_PLACEMENT_3D('',#71692,#18368,#18369);
#14964=AXIS2_PLACEMENT_3D('',#71693,#18370,#18371);
#14965=AXIS2_PLACEMENT_3D('',#71694,#18372,#18373);
#14966=AXIS2_PLACEMENT_3D('',#71695,#18374,#18375);
#14967=AXIS2_PLACEMENT_3D('',#71696,#18376,#18377);
#14968=AXIS2_PLACEMENT_3D('',#71697,#18378,#18379);
#14969=AXIS2_PLACEMENT_3D('',#71698,#18380,#18381);
#14970=AXIS2_PLACEMENT_3D('',#71699,#18382,#18383);
#14971=AXIS2_PLACEMENT_3D('',#71700,#18384,#18385);
#14972=AXIS2_PLACEMENT_3D('',#71701,#18386,#18387);
#14973=AXIS2_PLACEMENT_3D('',#71702,#18388,#18389);
#14974=AXIS2_PLACEMENT_3D('',#71703,#18390,#18391);
#14975=AXIS2_PLACEMENT_3D('',#71704,#18392,#18393);
#14976=AXIS2_PLACEMENT_3D('',#71705,#18394,#18395);
#14977=AXIS2_PLACEMENT_3D('',#71706,#18396,#18397);
#14978=AXIS2_PLACEMENT_3D('',#71707,#18398,#18399);
#14979=AXIS2_PLACEMENT_3D('',#71708,#18400,#18401);
#14980=AXIS2_PLACEMENT_3D('',#71709,#18402,#18403);
#14981=AXIS2_PLACEMENT_3D('',#71710,#18404,#18405);
#14982=AXIS2_PLACEMENT_3D('',#71711,#18406,#18407);
#14983=AXIS2_PLACEMENT_3D('',#71712,#18408,#18409);
#14984=AXIS2_PLACEMENT_3D('',#71713,#18410,#18411);
#14985=AXIS2_PLACEMENT_3D('',#71714,#18412,#18413);
#14986=AXIS2_PLACEMENT_3D('',#71715,#18414,#18415);
#14987=AXIS2_PLACEMENT_3D('',#71716,#18416,#18417);
#14988=AXIS2_PLACEMENT_3D('',#71717,#18418,#18419);
#14989=AXIS2_PLACEMENT_3D('',#71718,#18420,#18421);
#14990=AXIS2_PLACEMENT_3D('',#71719,#18422,#18423);
#14991=AXIS2_PLACEMENT_3D('',#71720,#18424,#18425);
#14992=AXIS2_PLACEMENT_3D('',#71721,#18426,#18427);
#14993=AXIS2_PLACEMENT_3D('',#71722,#18428,#18429);
#14994=AXIS2_PLACEMENT_3D('',#71723,#18430,#18431);
#14995=AXIS2_PLACEMENT_3D('',#71724,#18432,#18433);
#14996=AXIS2_PLACEMENT_3D('',#71725,#18434,#18435);
#14997=AXIS2_PLACEMENT_3D('',#71726,#18436,#18437);
#14998=AXIS2_PLACEMENT_3D('',#71727,#18438,#18439);
#14999=AXIS2_PLACEMENT_3D('',#71728,#18440,#18441);
#15000=AXIS2_PLACEMENT_3D('',#71729,#18442,#18443);
#15001=AXIS2_PLACEMENT_3D('',#71730,#18444,#18445);
#15002=AXIS2_PLACEMENT_3D('',#71731,#18446,#18447);
#15003=AXIS2_PLACEMENT_3D('',#71732,#18448,#18449);
#15004=AXIS2_PLACEMENT_3D('',#71733,#18450,#18451);
#15005=AXIS2_PLACEMENT_3D('',#71734,#18452,#18453);
#15006=AXIS2_PLACEMENT_3D('',#71735,#18454,#18455);
#15007=AXIS2_PLACEMENT_3D('',#71736,#18456,#18457);
#15008=AXIS2_PLACEMENT_3D('',#71737,#18458,#18459);
#15009=AXIS2_PLACEMENT_3D('',#71738,#18460,#18461);
#15010=AXIS2_PLACEMENT_3D('',#71739,#18462,#18463);
#15011=AXIS2_PLACEMENT_3D('',#71740,#18464,#18465);
#15012=AXIS2_PLACEMENT_3D('',#71741,#18466,#18467);
#15013=AXIS2_PLACEMENT_3D('',#71742,#18468,#18469);
#15014=AXIS2_PLACEMENT_3D('',#71743,#18470,#18471);
#15015=AXIS2_PLACEMENT_3D('',#71744,#18472,#18473);
#15016=AXIS2_PLACEMENT_3D('',#71745,#18474,#18475);
#15017=AXIS2_PLACEMENT_3D('',#71746,#18476,#18477);
#15018=AXIS2_PLACEMENT_3D('',#71747,#18478,#18479);
#15019=AXIS2_PLACEMENT_3D('',#71748,#18480,#18481);
#15020=AXIS2_PLACEMENT_3D('',#71749,#18482,#18483);
#15021=AXIS2_PLACEMENT_3D('',#71750,#18484,#18485);
#15022=AXIS2_PLACEMENT_3D('',#71751,#18486,#18487);
#15023=AXIS2_PLACEMENT_3D('',#71752,#18488,#18489);
#15024=AXIS2_PLACEMENT_3D('',#71753,#18490,#18491);
#15025=AXIS2_PLACEMENT_3D('',#71754,#18492,#18493);
#15026=AXIS2_PLACEMENT_3D('',#71755,#18494,#18495);
#15027=AXIS2_PLACEMENT_3D('',#71756,#18496,#18497);
#15028=AXIS2_PLACEMENT_3D('',#71757,#18498,#18499);
#15029=AXIS2_PLACEMENT_3D('',#71758,#18500,#18501);
#15030=AXIS2_PLACEMENT_3D('',#71759,#18502,#18503);
#15031=AXIS2_PLACEMENT_3D('',#71760,#18504,#18505);
#15032=AXIS2_PLACEMENT_3D('',#71761,#18506,#18507);
#15033=AXIS2_PLACEMENT_3D('',#71762,#18508,#18509);
#15034=AXIS2_PLACEMENT_3D('',#71763,#18510,#18511);
#15035=AXIS2_PLACEMENT_3D('',#71764,#18512,#18513);
#15036=AXIS2_PLACEMENT_3D('',#71765,#18514,#18515);
#15037=AXIS2_PLACEMENT_3D('',#71766,#18516,#18517);
#15038=AXIS2_PLACEMENT_3D('',#71767,#18518,#18519);
#15039=AXIS2_PLACEMENT_3D('',#71768,#18520,#18521);
#15040=AXIS2_PLACEMENT_3D('',#71769,#18522,#18523);
#15041=AXIS2_PLACEMENT_3D('',#71770,#18524,#18525);
#15042=AXIS2_PLACEMENT_3D('',#71771,#18526,#18527);
#15043=DIRECTION('axis',(0.,0.,1.));
#15044=DIRECTION('refdir',(1.,0.,0.));
#15045=DIRECTION('axis',(0.,0.,1.));
#15046=DIRECTION('refdir',(1.,0.,0.));
#15047=DIRECTION('center_axis',(0.,0.707106781186547,-0.707106781186548));
#15048=DIRECTION('ref_axis',(0.,0.707106781186548,0.707106781186547));
#15049=DIRECTION('center_axis',(0.,1.,0.));
#15050=DIRECTION('ref_axis',(0.,0.,1.));
#15051=DIRECTION('',(0.,0.707106781186547,-0.707106781186548));
#15052=DIRECTION('center_axis',(0.,0.707106781186547,-0.707106781186548));
#15053=DIRECTION('ref_axis',(1.,0.,0.));
#15054=DIRECTION('center_axis',(0.,0.707106781186547,-0.707106781186548));
#15055=DIRECTION('ref_axis',(-1.,0.,0.));
#15056=DIRECTION('center_axis',(0.,0.707106781186547,-0.707106781186548));
#15057=DIRECTION('ref_axis',(1.,0.,0.));
#15058=DIRECTION('center_axis',(0.,0.707106781186547,-0.707106781186548));
#15059=DIRECTION('ref_axis',(0.,0.707106781186548,0.707106781186547));
#15060=DIRECTION('',(0.,0.707106781186547,-0.707106781186548));
#15061=DIRECTION('center_axis',(0.,0.707106781186547,-0.707106781186548));
#15062=DIRECTION('ref_axis',(0.,0.707106781186548,0.707106781186547));
#15063=DIRECTION('center_axis',(0.,1.,0.));
#15064=DIRECTION('ref_axis',(0.,0.,1.));
#15065=DIRECTION('',(0.,0.707106781186547,-0.707106781186548));
#15066=DIRECTION('center_axis',(0.,0.707106781186547,-0.707106781186548));
#15067=DIRECTION('ref_axis',(1.,0.,0.));
#15068=DIRECTION('center_axis',(0.,0.707106781186547,-0.707106781186548));
#15069=DIRECTION('ref_axis',(-1.,0.,0.));
#15070=DIRECTION('center_axis',(0.,0.707106781186547,-0.707106781186548));
#15071=DIRECTION('ref_axis',(1.,0.,0.));
#15072=DIRECTION('center_axis',(0.,0.707106781186547,-0.707106781186548));
#15073=DIRECTION('ref_axis',(0.,0.707106781186548,0.707106781186547));
#15074=DIRECTION('',(0.,0.707106781186547,-0.707106781186548));
#15075=DIRECTION('center_axis',(0.,0.707106781186547,-0.707106781186548));
#15076=DIRECTION('ref_axis',(0.,0.707106781186548,0.707106781186547));
#15077=DIRECTION('center_axis',(0.,1.,0.));
#15078=DIRECTION('ref_axis',(0.,0.,1.));
#15079=DIRECTION('',(0.,0.707106781186547,-0.707106781186548));
#15080=DIRECTION('center_axis',(0.,0.707106781186547,-0.707106781186548));
#15081=DIRECTION('ref_axis',(1.,0.,0.));
#15082=DIRECTION('center_axis',(0.,0.707106781186547,-0.707106781186548));
#15083=DIRECTION('ref_axis',(-1.,0.,0.));
#15084=DIRECTION('center_axis',(0.,0.707106781186547,-0.707106781186548));
#15085=DIRECTION('ref_axis',(1.,0.,0.));
#15086=DIRECTION('center_axis',(0.,0.707106781186547,-0.707106781186548));
#15087=DIRECTION('ref_axis',(0.,0.707106781186548,0.707106781186547));
#15088=DIRECTION('',(0.,0.707106781186547,-0.707106781186548));
#15089=DIRECTION('center_axis',(0.,0.707106781186547,0.707106781186548));
#15090=DIRECTION('ref_axis',(0.,-0.707106781186548,0.707106781186547));
#15091=DIRECTION('center_axis',(0.,1.,0.));
#15092=DIRECTION('ref_axis',(0.,0.,1.));
#15093=DIRECTION('',(0.,0.707106781186547,0.707106781186548));
#15094=DIRECTION('center_axis',(0.,0.707106781186547,0.707106781186548));
#15095=DIRECTION('ref_axis',(1.,0.,0.));
#15096=DIRECTION('center_axis',(0.,0.707106781186547,0.707106781186548));
#15097=DIRECTION('ref_axis',(1.,0.,0.));
#15098=DIRECTION('center_axis',(0.,0.707106781186547,0.707106781186548));
#15099=DIRECTION('ref_axis',(1.,0.,0.));
#15100=DIRECTION('center_axis',(0.,0.707106781186547,0.707106781186548));
#15101=DIRECTION('ref_axis',(0.,-0.707106781186548,0.707106781186547));
#15102=DIRECTION('',(0.,0.707106781186547,0.707106781186548));
#15103=DIRECTION('center_axis',(0.,0.707106781186547,0.707106781186548));
#15104=DIRECTION('ref_axis',(0.,-0.707106781186548,0.707106781186547));
#15105=DIRECTION('center_axis',(0.,1.,0.));
#15106=DIRECTION('ref_axis',(0.,0.,1.));
#15107=DIRECTION('',(0.,0.707106781186547,0.707106781186548));
#15108=DIRECTION('center_axis',(0.,0.707106781186547,0.707106781186548));
#15109=DIRECTION('ref_axis',(1.,0.,0.));
#15110=DIRECTION('center_axis',(0.,0.707106781186547,0.707106781186548));
#15111=DIRECTION('ref_axis',(1.,0.,0.));
#15112=DIRECTION('center_axis',(0.,0.707106781186547,0.707106781186548));
#15113=DIRECTION('ref_axis',(1.,0.,0.));
#15114=DIRECTION('center_axis',(0.,0.707106781186547,0.707106781186548));
#15115=DIRECTION('ref_axis',(0.,-0.707106781186548,0.707106781186547));
#15116=DIRECTION('',(0.,0.707106781186547,0.707106781186548));
#15117=DIRECTION('center_axis',(0.,0.707106781186547,0.707106781186548));
#15118=DIRECTION('ref_axis',(0.,-0.707106781186548,0.707106781186547));
#15119=DIRECTION('center_axis',(0.,1.,0.));
#15120=DIRECTION('ref_axis',(0.,0.,1.));
#15121=DIRECTION('',(0.,0.707106781186547,0.707106781186548));
#15122=DIRECTION('center_axis',(0.,0.707106781186547,0.707106781186548));
#15123=DIRECTION('ref_axis',(1.,0.,0.));
#15124=DIRECTION('center_axis',(0.,0.707106781186547,0.707106781186548));
#15125=DIRECTION('ref_axis',(1.,0.,0.));
#15126=DIRECTION('center_axis',(0.,0.707106781186547,0.707106781186548));
#15127=DIRECTION('ref_axis',(1.,0.,0.));
#15128=DIRECTION('center_axis',(0.,0.707106781186547,0.707106781186548));
#15129=DIRECTION('ref_axis',(0.,-0.707106781186548,0.707106781186547));
#15130=DIRECTION('',(0.,0.707106781186547,0.707106781186548));
#15131=DIRECTION('center_axis',(0.,1.,0.));
#15132=DIRECTION('ref_axis',(1.,0.,0.));
#15133=DIRECTION('center_axis',(0.,-1.,0.));
#15134=DIRECTION('ref_axis',(1.,0.,0.));
#15135=DIRECTION('',(-0.707106781186539,0.707106781186556,8.65956056235484E-17));
#15136=DIRECTION('center_axis',(0.,1.,0.));
#15137=DIRECTION('ref_axis',(1.,0.,0.));
#15138=DIRECTION('center_axis',(0.,1.,0.));
#15139=DIRECTION('ref_axis',(0.,0.,1.));
#15140=DIRECTION('',(0.,0.,1.));
#15141=DIRECTION('',(1.,0.,0.));
#15142=DIRECTION('',(0.,0.,1.));
#15143=DIRECTION('',(1.,0.,0.));
#15144=DIRECTION('center_axis',(0.,1.,0.));
#15145=DIRECTION('ref_axis',(1.,0.,0.));
#15146=DIRECTION('center_axis',(0.,1.,0.));
#15147=DIRECTION('ref_axis',(1.,0.,0.));
#15148=DIRECTION('center_axis',(0.,1.,0.));
#15149=DIRECTION('ref_axis',(1.,0.,0.));
#15150=DIRECTION('center_axis',(0.,-1.,0.));
#15151=DIRECTION('ref_axis',(1.,0.,0.));
#15152=DIRECTION('',(0.,-1.,0.));
#15153=DIRECTION('center_axis',(0.,-1.,0.));
#15154=DIRECTION('ref_axis',(1.,0.,0.));
#15155=DIRECTION('center_axis',(0.,1.,0.));
#15156=DIRECTION('ref_axis',(1.,0.,0.));
#15157=DIRECTION('center_axis',(0.,-1.,0.));
#15158=DIRECTION('ref_axis',(1.,0.,0.));
#15159=DIRECTION('',(-0.70710678118655,0.707106781186545,8.65956056235497E-17));
#15160=DIRECTION('center_axis',(0.,-1.,0.));
#15161=DIRECTION('ref_axis',(1.,0.,0.));
#15162=DIRECTION('',(0.,-1.,0.));
#15163=DIRECTION('center_axis',(0.,-1.,0.));
#15164=DIRECTION('ref_axis',(1.,0.,0.));
#15165=DIRECTION('center_axis',(0.,1.,0.));
#15166=DIRECTION('ref_axis',(1.,0.,0.));
#15167=DIRECTION('center_axis',(0.,-1.,0.));
#15168=DIRECTION('ref_axis',(1.,0.,0.));
#15169=DIRECTION('',(-0.70710678118655,0.707106781186545,8.65956056235497E-17));
#15170=DIRECTION('center_axis',(0.,-1.,0.));
#15171=DIRECTION('ref_axis',(1.,0.,0.));
#15172=DIRECTION('',(0.,-1.,0.));
#15173=DIRECTION('center_axis',(0.,-1.,0.));
#15174=DIRECTION('ref_axis',(1.,0.,0.));
#15175=DIRECTION('center_axis',(0.,1.,0.));
#15176=DIRECTION('ref_axis',(1.,0.,0.));
#15177=DIRECTION('center_axis',(0.,-1.,0.));
#15178=DIRECTION('ref_axis',(1.,0.,0.));
#15179=DIRECTION('',(-0.707106781186539,0.707106781186556,8.65956056235484E-17));
#15180=DIRECTION('center_axis',(0.,-1.,0.));
#15181=DIRECTION('ref_axis',(1.,0.,0.));
#15182=DIRECTION('',(0.,-1.,0.));
#15183=DIRECTION('center_axis',(0.,-1.,0.));
#15184=DIRECTION('ref_axis',(1.,0.,0.));
#15185=DIRECTION('center_axis',(0.,1.,0.));
#15186=DIRECTION('ref_axis',(1.,0.,0.));
#15187=DIRECTION('center_axis',(0.,1.,0.));
#15188=DIRECTION('ref_axis',(1.,0.,0.));
#15189=DIRECTION('center_axis',(0.,1.,0.));
#15190=DIRECTION('ref_axis',(1.,0.,0.));
#15191=DIRECTION('center_axis',(0.,1.,0.));
#15192=DIRECTION('ref_axis',(1.,0.,0.));
#15193=DIRECTION('center_axis',(0.,1.,0.));
#15194=DIRECTION('ref_axis',(1.,0.,0.));
#15195=DIRECTION('center_axis',(0.,1.,0.));
#15196=DIRECTION('ref_axis',(1.,0.,0.));
#15197=DIRECTION('center_axis',(0.,1.,0.));
#15198=DIRECTION('ref_axis',(1.,0.,0.));
#15199=DIRECTION('center_axis',(0.,1.,0.));
#15200=DIRECTION('ref_axis',(1.,0.,0.));
#15201=DIRECTION('center_axis',(0.,-1.,0.));
#15202=DIRECTION('ref_axis',(1.,0.,0.));
#15203=DIRECTION('',(0.,-1.,0.));
#15204=DIRECTION('center_axis',(0.,1.,0.));
#15205=DIRECTION('ref_axis',(1.,0.,0.));
#15206=DIRECTION('center_axis',(0.,-1.,0.));
#15207=DIRECTION('ref_axis',(1.,0.,0.));
#15208=DIRECTION('',(0.,-1.,0.));
#15209=DIRECTION('center_axis',(0.,1.,0.));
#15210=DIRECTION('ref_axis',(1.,0.,0.));
#15211=DIRECTION('center_axis',(0.,-1.,0.));
#15212=DIRECTION('ref_axis',(1.,0.,0.));
#15213=DIRECTION('',(0.,-1.,0.));
#15214=DIRECTION('center_axis',(0.,1.,0.));
#15215=DIRECTION('ref_axis',(1.,0.,0.));
#15216=DIRECTION('center_axis',(0.,-1.,0.));
#15217=DIRECTION('ref_axis',(1.,0.,0.));
#15218=DIRECTION('',(0.,-1.,0.));
#15219=DIRECTION('center_axis',(0.,1.,0.));
#15220=DIRECTION('ref_axis',(1.,0.,0.));
#15221=DIRECTION('center_axis',(0.,0.707106781186548,0.707106781186548));
#15222=DIRECTION('ref_axis',(1.,0.,0.));
#15223=DIRECTION('',(0.,0.707106781186547,-0.707106781186547));
#15224=DIRECTION('',(-1.,0.,0.));
#15225=DIRECTION('',(0.,-0.707106781186547,0.707106781186547));
#15226=DIRECTION('',(1.,0.,0.));
#15227=DIRECTION('center_axis',(0.,0.,1.));
#15228=DIRECTION('ref_axis',(0.,-1.,0.));
#15229=DIRECTION('',(0.,-1.,0.));
#15230=DIRECTION('',(0.,-1.,0.));
#15231=DIRECTION('center_axis',(1.,0.,0.));
#15232=DIRECTION('ref_axis',(0.,0.,-1.));
#15233=DIRECTION('',(0.,0.,1.));
#15234=DIRECTION('',(0.,-0.707106781186548,0.707106781186547));
#15235=DIRECTION('center_axis',(1.,0.,0.));
#15236=DIRECTION('ref_axis',(0.,-0.21859823653748,0.975814947099451));
#15237=DIRECTION('',(0.,0.707106781186547,-0.707106781186547));
#15238=DIRECTION('',(0.,1.,0.));
#15239=DIRECTION('',(0.,0.707106781186549,-0.707106781186546));
#15240=DIRECTION('',(0.,0.,1.));
#15241=DIRECTION('',(0.,-0.707106781186549,-0.707106781186546));
#15242=DIRECTION('',(0.,1.,0.));
#15243=DIRECTION('',(0.,0.707106781186547,0.707106781186547));
#15244=DIRECTION('center_axis',(1.,0.,0.));
#15245=DIRECTION('ref_axis',(0.,-0.975814947099451,-0.218598236537478));
#15246=DIRECTION('',(0.,-0.707106781186548,-0.707106781186547));
#15247=DIRECTION('',(0.,0.,-1.));
#15248=DIRECTION('',(0.,0.707106781186547,0.707106781186547));
#15249=DIRECTION('',(0.,-1.,0.));
#15250=DIRECTION('center_axis',(0.,0.707106781186548,-0.707106781186548));
#15251=DIRECTION('ref_axis',(-1.,0.,0.));
#15252=DIRECTION('',(0.,-0.707106781186547,-0.707106781186547));
#15253=DIRECTION('',(-1.,0.,0.));
#15254=DIRECTION('',(1.,0.,0.));
#15255=DIRECTION('center_axis',(0.,1.,0.));
#15256=DIRECTION('ref_axis',(0.,0.,1.));
#15257=DIRECTION('',(1.,0.,0.));
#15258=DIRECTION('',(0.,0.,1.));
#15259=DIRECTION('center_axis',(0.,-0.707106781186546,0.707106781186549));
#15260=DIRECTION('ref_axis',(1.,0.,0.));
#15261=DIRECTION('',(0.,0.707106781186549,0.707106781186546));
#15262=DIRECTION('',(-1.,0.,0.));
#15263=DIRECTION('',(1.,0.,0.));
#15264=DIRECTION('center_axis',(0.,-1.,0.));
#15265=DIRECTION('ref_axis',(0.,0.,-1.));
#15266=DIRECTION('',(-1.,0.,0.));
#15267=DIRECTION('',(0.,0.,-1.));
#15268=DIRECTION('center_axis',(0.,-0.707106781186546,-0.707106781186549));
#15269=DIRECTION('ref_axis',(-1.,0.,0.));
#15270=DIRECTION('',(0.,-0.707106781186549,0.707106781186546));
#15271=DIRECTION('',(1.,0.,0.));
#15272=DIRECTION('center_axis',(1.,0.,0.));
#15273=DIRECTION('ref_axis',(0.,-0.21859823653748,0.975814947099451));
#15274=DIRECTION('',(1.,0.,0.));
#15275=DIRECTION('center_axis',(-1.,0.,0.));
#15276=DIRECTION('ref_axis',(0.,-0.21859823653748,0.975814947099451));
#15277=DIRECTION('',(1.,0.,0.));
#15278=DIRECTION('center_axis',(0.,-0.707106781186548,-0.707106781186548));
#15279=DIRECTION('ref_axis',(0.,0.707106781186548,-0.707106781186548));
#15280=DIRECTION('',(0.,0.707106781186547,-0.707106781186547));
#15281=DIRECTION('',(1.,0.,0.));
#15282=DIRECTION('center_axis',(0.,0.,-1.));
#15283=DIRECTION('ref_axis',(0.,1.,0.));
#15284=DIRECTION('',(0.,1.,0.));
#15285=DIRECTION('center_axis',(0.,0.,1.));
#15286=DIRECTION('ref_axis',(0.,-1.,0.));
#15287=DIRECTION('',(0.,-1.,0.));
#15288=DIRECTION('',(1.,0.,0.));
#15289=DIRECTION('center_axis',(0.,-0.707106781186548,0.707106781186548));
#15290=DIRECTION('ref_axis',(0.,-0.707106781186548,-0.707106781186548));
#15291=DIRECTION('',(0.,-0.707106781186547,-0.707106781186547));
#15292=DIRECTION('',(1.,0.,0.));
#15293=DIRECTION('center_axis',(1.,0.,0.));
#15294=DIRECTION('ref_axis',(0.,-0.975814947099451,-0.218598236537478));
#15295=DIRECTION('center_axis',(-1.,0.,0.));
#15296=DIRECTION('ref_axis',(0.,-0.975814947099451,-0.218598236537478));
#15297=DIRECTION('',(1.,0.,0.));
#15298=DIRECTION('center_axis',(0.,0.707106781186547,-0.707106781186548));
#15299=DIRECTION('ref_axis',(0.,0.707106781186548,0.707106781186547));
#15300=DIRECTION('',(0.,0.707106781186548,0.707106781186547));
#15301=DIRECTION('center_axis',(0.,0.,-1.));
#15302=DIRECTION('ref_axis',(0.,1.,0.));
#15303=DIRECTION('',(0.,1.,0.));
#15304=DIRECTION('center_axis',(0.,1.,0.));
#15305=DIRECTION('ref_axis',(0.,0.,1.));
#15306=DIRECTION('',(0.,0.,1.));
#15307=DIRECTION('',(1.,0.,0.));
#15308=DIRECTION('center_axis',(0.,0.707106781186547,0.707106781186548));
#15309=DIRECTION('ref_axis',(0.,-0.707106781186548,0.707106781186547));
#15310=DIRECTION('',(0.,-0.707106781186548,0.707106781186547));
#15311=DIRECTION('center_axis',(1.,0.,0.));
#15312=DIRECTION('ref_axis',(0.,0.,-1.));
#15313=DIRECTION('axis',(0.,0.,1.));
#15314=DIRECTION('refdir',(1.,0.,0.));
#15315=DIRECTION('center_axis',(0.,1.,0.));
#15316=DIRECTION('ref_axis',(-0.429672959082026,0.,0.902984578070797));
#15317=DIRECTION('center_axis',(0.,1.,0.));
#15318=DIRECTION('ref_axis',(-1.,0.,0.));
#15319=DIRECTION('center_axis',(0.,-1.,0.));
#15320=DIRECTION('ref_axis',(-1.,0.,0.));
#15321=DIRECTION('center_axis',(0.,1.,0.));
#15322=DIRECTION('ref_axis',(0.,0.,1.));
#15323=DIRECTION('',(0.,0.,1.));
#15324=DIRECTION('',(1.,0.,0.));
#15325=DIRECTION('',(0.,0.,-1.));
#15326=DIRECTION('',(-1.,0.,0.));
#15327=DIRECTION('center_axis',(0.,1.,0.));
#15328=DIRECTION('ref_axis',(1.,0.,0.));
#15329=DIRECTION('center_axis',(0.,1.,0.));
#15330=DIRECTION('ref_axis',(1.,0.,0.));
#15331=DIRECTION('center_axis',(0.,1.,0.));
#15332=DIRECTION('ref_axis',(1.,0.,0.));
#15333=DIRECTION('center_axis',(0.,1.,0.));
#15334=DIRECTION('ref_axis',(1.,0.,0.));
#15335=DIRECTION('center_axis',(0.,1.,0.));
#15336=DIRECTION('ref_axis',(-1.,0.,0.));
#15337=DIRECTION('center_axis',(0.,1.,0.));
#15338=DIRECTION('ref_axis',(1.,0.,0.));
#15339=DIRECTION('center_axis',(0.,1.,0.));
#15340=DIRECTION('ref_axis',(1.,0.,0.));
#15341=DIRECTION('center_axis',(0.,1.,0.));
#15342=DIRECTION('ref_axis',(1.,0.,0.));
#15343=DIRECTION('center_axis',(0.,1.,0.));
#15344=DIRECTION('ref_axis',(1.,0.,0.));
#15345=DIRECTION('center_axis',(0.,1.,0.));
#15346=DIRECTION('ref_axis',(1.,0.,0.));
#15347=DIRECTION('center_axis',(0.,1.,0.));
#15348=DIRECTION('ref_axis',(1.,0.,0.));
#15349=DIRECTION('center_axis',(0.,1.,0.));
#15350=DIRECTION('ref_axis',(1.,0.,0.));
#15351=DIRECTION('center_axis',(0.,1.,0.));
#15352=DIRECTION('ref_axis',(1.,0.,0.));
#15353=DIRECTION('center_axis',(0.,1.,0.));
#15354=DIRECTION('ref_axis',(1.,0.,0.));
#15355=DIRECTION('center_axis',(0.,1.,0.));
#15356=DIRECTION('ref_axis',(1.,0.,0.));
#15357=DIRECTION('center_axis',(0.,1.,0.));
#15358=DIRECTION('ref_axis',(1.,0.,0.));
#15359=DIRECTION('center_axis',(0.,-1.,0.));
#15360=DIRECTION('ref_axis',(1.,0.,0.));
#15361=DIRECTION('',(-0.707106781186537,0.707106781186558,8.65956056235481E-17));
#15362=DIRECTION('center_axis',(0.,-1.,0.));
#15363=DIRECTION('ref_axis',(1.,0.,0.));
#15364=DIRECTION('',(0.,-1.,0.));
#15365=DIRECTION('center_axis',(0.,-1.,0.));
#15366=DIRECTION('ref_axis',(1.,0.,0.));
#15367=DIRECTION('center_axis',(0.,1.,0.));
#15368=DIRECTION('ref_axis',(0.429672959082026,0.,-0.902984578070797));
#15369=DIRECTION('center_axis',(0.,-1.,0.));
#15370=DIRECTION('ref_axis',(1.,0.,0.));
#15371=DIRECTION('center_axis',(0.,1.,0.));
#15372=DIRECTION('ref_axis',(1.,0.,0.));
#15373=DIRECTION('center_axis',(0.,-1.,0.));
#15374=DIRECTION('ref_axis',(1.,0.,0.));
#15375=DIRECTION('',(-0.707106781186547,0.707106781186548,8.65956056235493E-17));
#15376=DIRECTION('center_axis',(0.,-1.,0.));
#15377=DIRECTION('ref_axis',(1.,0.,0.));
#15378=DIRECTION('',(0.,-1.,0.));
#15379=DIRECTION('center_axis',(0.,-1.,0.));
#15380=DIRECTION('ref_axis',(1.,0.,0.));
#15381=DIRECTION('center_axis',(0.,1.,0.));
#15382=DIRECTION('ref_axis',(0.429672959082009,0.,0.902984578070805));
#15383=DIRECTION('center_axis',(0.,-1.,0.));
#15384=DIRECTION('ref_axis',(1.,0.,0.));
#15385=DIRECTION('center_axis',(0.,1.,0.));
#15386=DIRECTION('ref_axis',(1.,0.,0.));
#15387=DIRECTION('center_axis',(0.,-1.,0.));
#15388=DIRECTION('ref_axis',(1.,0.,0.));
#15389=DIRECTION('',(-0.707106781186547,0.707106781186548,8.65956056235493E-17));
#15390=DIRECTION('center_axis',(0.,-1.,0.));
#15391=DIRECTION('ref_axis',(1.,0.,0.));
#15392=DIRECTION('',(0.,-1.,0.));
#15393=DIRECTION('center_axis',(0.,-1.,0.));
#15394=DIRECTION('ref_axis',(1.,0.,0.));
#15395=DIRECTION('center_axis',(0.,1.,0.));
#15396=DIRECTION('ref_axis',(1.,0.,0.));
#15397=DIRECTION('center_axis',(0.,-1.,0.));
#15398=DIRECTION('ref_axis',(1.,0.,0.));
#15399=DIRECTION('',(-0.707106781186537,0.707106781186558,8.65956056235481E-17));
#15400=DIRECTION('center_axis',(0.,-1.,0.));
#15401=DIRECTION('ref_axis',(1.,0.,0.));
#15402=DIRECTION('',(0.,-1.,0.));
#15403=DIRECTION('center_axis',(0.,-1.,0.));
#15404=DIRECTION('ref_axis',(1.,0.,0.));
#15405=DIRECTION('center_axis',(0.,1.,0.));
#15406=DIRECTION('ref_axis',(-0.429672959082014,0.,-0.902984578070803));
#15407=DIRECTION('center_axis',(0.,-1.,0.));
#15408=DIRECTION('ref_axis',(-1.,0.,0.));
#15409=DIRECTION('center_axis',(0.,-1.,0.));
#15410=DIRECTION('ref_axis',(-0.429672959082013,0.,-0.902984578070803));
#15411=DIRECTION('',(0.,1.,0.));
#15412=DIRECTION('center_axis',(0.,-1.,0.));
#15413=DIRECTION('ref_axis',(1.,0.,0.));
#15414=DIRECTION('',(0.,-1.,0.));
#15415=DIRECTION('center_axis',(0.,1.,0.));
#15416=DIRECTION('ref_axis',(1.,0.,0.));
#15417=DIRECTION('center_axis',(0.,1.,0.));
#15418=DIRECTION('ref_axis',(1.,0.,0.));
#15419=DIRECTION('center_axis',(0.,1.,0.));
#15420=DIRECTION('ref_axis',(1.,0.,0.));
#15421=DIRECTION('center_axis',(0.,1.,0.));
#15422=DIRECTION('ref_axis',(1.,0.,0.));
#15423=DIRECTION('center_axis',(0.,1.,0.));
#15424=DIRECTION('ref_axis',(1.,0.,0.));
#15425=DIRECTION('center_axis',(0.,1.,0.));
#15426=DIRECTION('ref_axis',(1.,0.,0.));
#15427=DIRECTION('center_axis',(0.,1.,0.));
#15428=DIRECTION('ref_axis',(1.,0.,0.));
#15429=DIRECTION('center_axis',(0.,-1.,0.));
#15430=DIRECTION('ref_axis',(0.429672959082017,0.,0.902984578070801));
#15431=DIRECTION('',(0.,1.,0.));
#15432=DIRECTION('center_axis',(0.,-1.,0.));
#15433=DIRECTION('ref_axis',(1.,0.,0.));
#15434=DIRECTION('',(0.,-1.,0.));
#15435=DIRECTION('center_axis',(0.,1.,0.));
#15436=DIRECTION('ref_axis',(1.,0.,0.));
#15437=DIRECTION('center_axis',(0.,1.,0.));
#15438=DIRECTION('ref_axis',(1.,0.,0.));
#15439=DIRECTION('center_axis',(0.,1.,0.));
#15440=DIRECTION('ref_axis',(1.,0.,0.));
#15441=DIRECTION('center_axis',(0.,1.,0.));
#15442=DIRECTION('ref_axis',(1.,0.,0.));
#15443=DIRECTION('center_axis',(0.,1.,0.));
#15444=DIRECTION('ref_axis',(1.,0.,0.));
#15445=DIRECTION('center_axis',(0.,-1.,0.));
#15446=DIRECTION('ref_axis',(0.429672959082017,0.,-0.902984578070801));
#15447=DIRECTION('',(0.,1.,0.));
#15448=DIRECTION('center_axis',(0.,-1.,0.));
#15449=DIRECTION('ref_axis',(1.,0.,0.));
#15450=DIRECTION('',(0.,-1.,0.));
#15451=DIRECTION('center_axis',(0.,1.,0.));
#15452=DIRECTION('ref_axis',(1.,0.,0.));
#15453=DIRECTION('center_axis',(0.,1.,0.));
#15454=DIRECTION('ref_axis',(1.,0.,0.));
#15455=DIRECTION('center_axis',(0.,1.,0.));
#15456=DIRECTION('ref_axis',(1.,0.,0.));
#15457=DIRECTION('center_axis',(0.,1.,0.));
#15458=DIRECTION('ref_axis',(1.,0.,0.));
#15459=DIRECTION('center_axis',(0.,1.,0.));
#15460=DIRECTION('ref_axis',(1.,0.,0.));
#15461=DIRECTION('center_axis',(0.,-1.,0.));
#15462=DIRECTION('ref_axis',(-0.429672959082013,0.,0.902984578070803));
#15463=DIRECTION('',(0.,1.,0.));
#15464=DIRECTION('center_axis',(0.,-1.,0.));
#15465=DIRECTION('ref_axis',(1.,0.,0.));
#15466=DIRECTION('',(0.,-1.,0.));
#15467=DIRECTION('center_axis',(0.,1.,0.));
#15468=DIRECTION('ref_axis',(1.,0.,0.));
#15469=DIRECTION('center_axis',(0.,1.,0.));
#15470=DIRECTION('ref_axis',(1.,0.,0.));
#15471=DIRECTION('center_axis',(0.,1.,0.));
#15472=DIRECTION('ref_axis',(1.,0.,0.));
#15473=DIRECTION('center_axis',(0.,1.,0.));
#15474=DIRECTION('ref_axis',(0.429672959082025,0.,0.902984578070798));
#15475=DIRECTION('center_axis',(0.,-1.,0.));
#15476=DIRECTION('ref_axis',(1.,0.,0.));
#15477=DIRECTION('center_axis',(0.,-1.,0.));
#15478=DIRECTION('ref_axis',(1.,0.,0.));
#15479=DIRECTION('center_axis',(0.,1.,0.));
#15480=DIRECTION('ref_axis',(-0.429672959082016,0.,-0.902984578070802));
#15481=DIRECTION('center_axis',(0.,-1.,0.));
#15482=DIRECTION('ref_axis',(1.,0.,0.));
#15483=DIRECTION('center_axis',(0.,-1.,0.));
#15484=DIRECTION('ref_axis',(1.,0.,0.));
#15485=DIRECTION('center_axis',(0.,1.,0.));
#15486=DIRECTION('ref_axis',(-0.429672959082016,0.,0.902984578070802));
#15487=DIRECTION('center_axis',(0.,-1.,0.));
#15488=DIRECTION('ref_axis',(1.,0.,0.));
#15489=DIRECTION('center_axis',(0.,-1.,0.));
#15490=DIRECTION('ref_axis',(1.,0.,0.));
#15491=DIRECTION('center_axis',(0.,1.,0.));
#15492=DIRECTION('ref_axis',(0.429672959082026,0.,-0.902984578070797));
#15493=DIRECTION('center_axis',(0.,-1.,0.));
#15494=DIRECTION('ref_axis',(1.,0.,0.));
#15495=DIRECTION('center_axis',(0.,-1.,0.));
#15496=DIRECTION('ref_axis',(1.,0.,0.));
#15497=DIRECTION('center_axis',(0.,-1.,0.));
#15498=DIRECTION('ref_axis',(1.,0.,0.));
#15499=DIRECTION('',(0.,-1.,0.));
#15500=DIRECTION('center_axis',(0.,1.,0.));
#15501=DIRECTION('ref_axis',(1.,0.,0.));
#15502=DIRECTION('center_axis',(0.,-1.,0.));
#15503=DIRECTION('ref_axis',(1.,0.,0.));
#15504=DIRECTION('',(0.,-1.,0.));
#15505=DIRECTION('center_axis',(0.,1.,0.));
#15506=DIRECTION('ref_axis',(1.,0.,0.));
#15507=DIRECTION('center_axis',(0.,-1.,0.));
#15508=DIRECTION('ref_axis',(1.,0.,0.));
#15509=DIRECTION('',(0.,-1.,0.));
#15510=DIRECTION('center_axis',(0.,1.,0.));
#15511=DIRECTION('ref_axis',(1.,0.,0.));
#15512=DIRECTION('center_axis',(0.,-1.,0.));
#15513=DIRECTION('ref_axis',(1.,0.,0.));
#15514=DIRECTION('',(0.,-1.,0.));
#15515=DIRECTION('center_axis',(0.,1.,0.));
#15516=DIRECTION('ref_axis',(1.,0.,0.));
#15517=DIRECTION('center_axis',(0.,-1.,0.));
#15518=DIRECTION('ref_axis',(1.,0.,0.));
#15519=DIRECTION('',(0.,-1.,0.));
#15520=DIRECTION('center_axis',(0.,1.,0.));
#15521=DIRECTION('ref_axis',(1.,0.,0.));
#15522=DIRECTION('center_axis',(0.,-1.,0.));
#15523=DIRECTION('ref_axis',(1.,0.,0.));
#15524=DIRECTION('',(0.,-1.,0.));
#15525=DIRECTION('center_axis',(0.,1.,0.));
#15526=DIRECTION('ref_axis',(1.,0.,0.));
#15527=DIRECTION('center_axis',(0.,-1.,0.));
#15528=DIRECTION('ref_axis',(1.,0.,0.));
#15529=DIRECTION('',(0.,-1.,0.));
#15530=DIRECTION('center_axis',(0.,1.,0.));
#15531=DIRECTION('ref_axis',(1.,0.,0.));
#15532=DIRECTION('center_axis',(0.,-1.,0.));
#15533=DIRECTION('ref_axis',(1.,0.,0.));
#15534=DIRECTION('',(0.,-1.,0.));
#15535=DIRECTION('center_axis',(0.,1.,0.));
#15536=DIRECTION('ref_axis',(1.,0.,0.));
#15537=DIRECTION('center_axis',(0.,1.,0.));
#15538=DIRECTION('ref_axis',(1.,0.,0.));
#15539=DIRECTION('center_axis',(0.,-1.,0.));
#15540=DIRECTION('ref_axis',(1.,0.,0.));
#15541=DIRECTION('',(-0.707106781186539,0.707106781186556,8.65956056235484E-17));
#15542=DIRECTION('center_axis',(0.,-1.,0.));
#15543=DIRECTION('ref_axis',(1.,0.,0.));
#15544=DIRECTION('',(0.,-1.,0.));
#15545=DIRECTION('center_axis',(0.,-1.,0.));
#15546=DIRECTION('ref_axis',(1.,0.,0.));
#15547=DIRECTION('center_axis',(0.,1.,0.));
#15548=DIRECTION('ref_axis',(1.,0.,0.));
#15549=DIRECTION('center_axis',(0.,-1.,0.));
#15550=DIRECTION('ref_axis',(1.,0.,0.));
#15551=DIRECTION('',(-0.707106781186547,0.707106781186548,8.65956056235493E-17));
#15552=DIRECTION('center_axis',(0.,-1.,0.));
#15553=DIRECTION('ref_axis',(1.,0.,0.));
#15554=DIRECTION('',(0.,-1.,0.));
#15555=DIRECTION('center_axis',(0.,-1.,0.));
#15556=DIRECTION('ref_axis',(1.,0.,0.));
#15557=DIRECTION('center_axis',(0.,-1.,0.));
#15558=DIRECTION('ref_axis',(1.,0.,0.));
#15559=DIRECTION('',(0.,-1.,0.));
#15560=DIRECTION('center_axis',(0.,-1.,0.));
#15561=DIRECTION('ref_axis',(1.,0.,0.));
#15562=DIRECTION('center_axis',(0.,-1.,0.));
#15563=DIRECTION('ref_axis',(1.,0.,0.));
#15564=DIRECTION('',(0.,-1.,0.));
#15565=DIRECTION('center_axis',(0.,-1.,0.));
#15566=DIRECTION('ref_axis',(1.,0.,0.));
#15567=DIRECTION('center_axis',(0.,-1.,0.));
#15568=DIRECTION('ref_axis',(1.,0.,0.));
#15569=DIRECTION('',(0.,-1.,0.));
#15570=DIRECTION('center_axis',(0.,-1.,0.));
#15571=DIRECTION('ref_axis',(1.,0.,0.));
#15572=DIRECTION('center_axis',(0.,-1.,0.));
#15573=DIRECTION('ref_axis',(1.,0.,0.));
#15574=DIRECTION('',(0.,-1.,0.));
#15575=DIRECTION('center_axis',(0.,-1.,0.));
#15576=DIRECTION('ref_axis',(1.,0.,0.));
#15577=DIRECTION('center_axis',(0.,1.,0.));
#15578=DIRECTION('ref_axis',(1.,0.,0.));
#15579=DIRECTION('center_axis',(0.,-1.,0.));
#15580=DIRECTION('ref_axis',(1.,0.,0.));
#15581=DIRECTION('',(-0.707106781186547,0.707106781186548,8.65956056235493E-17));
#15582=DIRECTION('center_axis',(0.,-1.,0.));
#15583=DIRECTION('ref_axis',(1.,0.,0.));
#15584=DIRECTION('',(0.,-1.,0.));
#15585=DIRECTION('center_axis',(0.,-1.,0.));
#15586=DIRECTION('ref_axis',(1.,0.,0.));
#15587=DIRECTION('center_axis',(0.,1.,0.));
#15588=DIRECTION('ref_axis',(1.,0.,0.));
#15589=DIRECTION('center_axis',(0.,-1.,0.));
#15590=DIRECTION('ref_axis',(1.,0.,0.));
#15591=DIRECTION('',(-0.707106781186539,0.707106781186556,8.65956056235484E-17));
#15592=DIRECTION('center_axis',(0.,-1.,0.));
#15593=DIRECTION('ref_axis',(1.,0.,0.));
#15594=DIRECTION('',(0.,-1.,0.));
#15595=DIRECTION('center_axis',(0.,-1.,0.));
#15596=DIRECTION('ref_axis',(1.,0.,0.));
#15597=DIRECTION('center_axis',(0.,1.,0.));
#15598=DIRECTION('ref_axis',(1.,0.,0.));
#15599=DIRECTION('',(-0.85716730070211,0.515038074910058,1.04972719113862E-16));
#15600=DIRECTION('center_axis',(0.,1.,0.));
#15601=DIRECTION('ref_axis',(1.,0.,0.));
#15602=DIRECTION('',(-0.85716730070211,0.515038074910058,1.04972719113862E-16));
#15603=DIRECTION('center_axis',(0.,1.,0.));
#15604=DIRECTION('ref_axis',(1.,0.,0.));
#15605=DIRECTION('',(-0.85716730070211,0.515038074910058,1.04972719113862E-16));
#15606=DIRECTION('center_axis',(0.,1.,0.));
#15607=DIRECTION('ref_axis',(1.,0.,0.));
#15608=DIRECTION('',(-0.85716730070211,0.515038074910058,1.04972719113862E-16));
#15609=DIRECTION('center_axis',(0.,1.,0.));
#15610=DIRECTION('ref_axis',(1.,0.,0.));
#15611=DIRECTION('',(-0.85716730070211,0.515038074910058,1.04972719113862E-16));
#15612=DIRECTION('center_axis',(0.,1.,0.));
#15613=DIRECTION('ref_axis',(1.,0.,0.));
#15614=DIRECTION('',(-0.85716730070211,0.515038074910058,1.04972719113862E-16));
#15615=DIRECTION('center_axis',(0.,1.,0.));
#15616=DIRECTION('ref_axis',(1.,0.,0.));
#15617=DIRECTION('',(-0.85716730070211,0.515038074910058,1.04972719113862E-16));
#15618=DIRECTION('center_axis',(0.,1.,0.));
#15619=DIRECTION('ref_axis',(1.,0.,0.));
#15620=DIRECTION('',(-0.85716730070211,0.515038074910058,1.04972719113862E-16));
#15621=DIRECTION('center_axis',(0.707106781186548,0.707106781186548,0.));
#15622=DIRECTION('ref_axis',(0.,0.,-1.));
#15623=DIRECTION('',(0.577350269189626,-0.577350269189626,0.577350269189626));
#15624=DIRECTION('',(0.,0.,-1.));
#15625=DIRECTION('',(0.577350269189626,-0.577350269189626,-0.577350269189626));
#15626=DIRECTION('center_axis',(0.,0.707106781186548,0.707106781186548));
#15627=DIRECTION('ref_axis',(1.,0.,0.));
#15628=DIRECTION('',(-0.577350269189626,-0.577350269189626,0.577350269189626));
#15629=DIRECTION('',(1.,0.,0.));
#15630=DIRECTION('center_axis',(-0.707106781186548,0.707106781186548,0.));
#15631=DIRECTION('ref_axis',(0.,0.,1.));
#15632=DIRECTION('',(-0.577350269189626,-0.577350269189626,-0.577350269189626));
#15633=DIRECTION('',(0.,0.,1.));
#15634=DIRECTION('center_axis',(0.,0.707106781186548,-0.707106781186548));
#15635=DIRECTION('ref_axis',(-1.,0.,0.));
#15636=DIRECTION('',(-1.,0.,0.));
#15637=DIRECTION('center_axis',(0.,0.,-1.));
#15638=DIRECTION('ref_axis',(-1.,0.,0.));
#15639=DIRECTION('',(0.,1.,0.));
#15640=DIRECTION('',(1.,0.,0.));
#15641=DIRECTION('',(0.,1.,0.));
#15642=DIRECTION('center_axis',(1.,0.,0.));
#15643=DIRECTION('ref_axis',(0.,0.,-1.));
#15644=DIRECTION('',(0.,1.,0.));
#15645=DIRECTION('',(0.,0.,1.));
#15646=DIRECTION('center_axis',(-1.,0.,0.));
#15647=DIRECTION('ref_axis',(0.,0.,1.));
#15648=DIRECTION('',(0.,0.,-1.));
#15649=DIRECTION('',(0.,1.,0.));
#15650=DIRECTION('center_axis',(0.,0.,1.));
#15651=DIRECTION('ref_axis',(1.,0.,0.));
#15652=DIRECTION('',(-1.,0.,0.));
#15653=DIRECTION('center_axis',(0.,1.,0.));
#15654=DIRECTION('ref_axis',(1.,0.,0.));
#15655=DIRECTION('axis',(0.,0.,1.));
#15656=DIRECTION('refdir',(1.,0.,0.));
#15657=DIRECTION('center_axis',(0.,0.707106781186548,0.707106781186548));
#15658=DIRECTION('ref_axis',(0.,-0.707106781186548,0.707106781186548));
#15659=DIRECTION('',(0.,0.707106781186548,0.707106781186548));
#15660=DIRECTION('center_axis',(0.,0.707106781186548,0.707106781186548));
#15661=DIRECTION('ref_axis',(1.,0.,0.));
#15662=DIRECTION('center_axis',(0.,-0.707106781186548,-0.707106781186548));
#15663=DIRECTION('ref_axis',(0.,-0.707106781186548,0.707106781186548));
#15664=DIRECTION('',(1.04605873377251E-16,0.236301539303659,-0.971679773651135));
#15665=DIRECTION('center_axis',(0.,0.707106781186548,0.707106781186548));
#15666=DIRECTION('ref_axis',(0.,-0.707106781186548,0.707106781186548));
#15667=DIRECTION('',(0.,0.707106781186548,0.707106781186548));
#15668=DIRECTION('center_axis',(0.,0.707106781186548,0.707106781186548));
#15669=DIRECTION('ref_axis',(1.,0.,0.));
#15670=DIRECTION('center_axis',(0.,-0.707106781186548,-0.707106781186548));
#15671=DIRECTION('ref_axis',(0.,-0.707106781186548,0.707106781186548));
#15672=DIRECTION('',(1.04605873377251E-16,0.236301539303659,-0.971679773651135));
#15673=DIRECTION('center_axis',(0.,0.707106781186548,0.707106781186548));
#15674=DIRECTION('ref_axis',(0.,-0.707106781186548,0.707106781186548));
#15675=DIRECTION('',(0.,0.707106781186548,0.707106781186548));
#15676=DIRECTION('center_axis',(0.,0.707106781186548,0.707106781186548));
#15677=DIRECTION('ref_axis',(1.,0.,0.));
#15678=DIRECTION('center_axis',(0.,-0.707106781186548,-0.707106781186548));
#15679=DIRECTION('ref_axis',(0.,-0.707106781186548,0.707106781186548));
#15680=DIRECTION('',(1.04605873377251E-16,0.236301539303659,-0.971679773651135));
#15681=DIRECTION('center_axis',(-1.,0.,0.));
#15682=DIRECTION('ref_axis',(0.,0.,1.));
#15683=DIRECTION('center_axis',(1.,0.,0.));
#15684=DIRECTION('ref_axis',(0.,0.,-1.));
#15685=DIRECTION('center_axis',(1.,0.,0.));
#15686=DIRECTION('ref_axis',(0.,1.,0.));
#15687=DIRECTION('center_axis',(1.,0.,0.));
#15688=DIRECTION('ref_axis',(0.,0.,-1.));
#15689=DIRECTION('',(-0.707106781186548,0.707106781186547,8.65956056235492E-17));
#15690=DIRECTION('center_axis',(1.,0.,0.));
#15691=DIRECTION('ref_axis',(0.,1.,0.));
#15692=DIRECTION('center_axis',(1.,0.,0.));
#15693=DIRECTION('ref_axis',(0.,0.,-1.));
#15694=DIRECTION('',(-1.,0.,0.));
#15695=DIRECTION('center_axis',(-1.,0.,0.));
#15696=DIRECTION('ref_axis',(0.,1.,0.));
#15697=DIRECTION('',(0.707106781186554,0.707106781186541,-8.65956056235485E-17));
#15698=DIRECTION('center_axis',(1.,0.,0.));
#15699=DIRECTION('ref_axis',(0.,0.,-1.));
#15700=DIRECTION('center_axis',(1.,0.,0.));
#15701=DIRECTION('ref_axis',(0.,0.,-1.));
#15702=DIRECTION('axis',(0.,0.,1.));
#15703=DIRECTION('refdir',(1.,0.,0.));
#15704=DIRECTION('center_axis',(0.,1.,0.));
#15705=DIRECTION('ref_axis',(1.,0.,0.));
#15706=DIRECTION('center_axis',(0.,-1.,0.));
#15707=DIRECTION('ref_axis',(1.,0.,0.));
#15708=DIRECTION('',(-0.707106781186553,0.707106781186542,8.659560562355E-17));
#15709=DIRECTION('center_axis',(0.,1.,0.));
#15710=DIRECTION('ref_axis',(1.,0.,0.));
#15711=DIRECTION('center_axis',(0.,1.,0.));
#15712=DIRECTION('ref_axis',(0.,0.,1.));
#15713=DIRECTION('',(1.,0.,0.));
#15714=DIRECTION('',(0.,0.,-1.));
#15715=DIRECTION('',(-1.,0.,0.));
#15716=DIRECTION('',(0.,0.,1.));
#15717=DIRECTION('center_axis',(0.,1.,0.));
#15718=DIRECTION('ref_axis',(1.,0.,0.));
#15719=DIRECTION('center_axis',(0.,-1.,0.));
#15720=DIRECTION('ref_axis',(1.,0.,0.));
#15721=DIRECTION('',(0.,-1.,0.));
#15722=DIRECTION('center_axis',(0.,-1.,0.));
#15723=DIRECTION('ref_axis',(1.,0.,0.));
#15724=DIRECTION('center_axis',(0.,-1.,0.));
#15725=DIRECTION('ref_axis',(1.,0.,0.));
#15726=DIRECTION('center_axis',(0.,1.,0.));
#15727=DIRECTION('ref_axis',(1.,0.,0.));
#15728=DIRECTION('center_axis',(0.,-1.,0.));
#15729=DIRECTION('ref_axis',(1.,0.,0.));
#15730=DIRECTION('',(-0.707106781186553,0.707106781186542,8.659560562355E-17));
#15731=DIRECTION('center_axis',(0.,-1.,0.));
#15732=DIRECTION('ref_axis',(1.,0.,0.));
#15733=DIRECTION('',(0.,-1.,0.));
#15734=DIRECTION('center_axis',(0.,-1.,0.));
#15735=DIRECTION('ref_axis',(1.,0.,0.));
#15736=DIRECTION('center_axis',(0.,-1.,0.));
#15737=DIRECTION('ref_axis',(1.,0.,0.));
#15738=DIRECTION('center_axis',(0.,1.,0.));
#15739=DIRECTION('ref_axis',(1.,0.,0.));
#15740=DIRECTION('',(-0.857167300702115,0.515038074910049,1.04972719113862E-16));
#15741=DIRECTION('center_axis',(1.,0.,0.));
#15742=DIRECTION('ref_axis',(0.,0.707106781186547,0.707106781186547));
#15743=DIRECTION('center_axis',(-1.,0.,0.));
#15744=DIRECTION('ref_axis',(0.,0.,1.));
#15745=DIRECTION('',(1.,0.,0.));
#15746=DIRECTION('center_axis',(1.,0.,0.));
#15747=DIRECTION('ref_axis',(0.,0.,1.));
#15748=DIRECTION('',(-1.,0.,0.));
#15749=DIRECTION('center_axis',(0.,1.,0.));
#15750=DIRECTION('ref_axis',(1.,0.,0.));
#15751=DIRECTION('',(-0.85716730070211,0.515038074910058,1.04972719113862E-16));
#15752=DIRECTION('center_axis',(1.,0.,0.));
#15753=DIRECTION('ref_axis',(0.,0.707106781186547,0.707106781186548));
#15754=DIRECTION('',(0.707106781186546,-0.110615871041237,-0.698401123333712));
#15755=DIRECTION('center_axis',(1.,0.,0.));
#15756=DIRECTION('ref_axis',(0.,0.,1.));
#15757=DIRECTION('',(-0.707106781186546,0.698401123333712,0.110615871041237));
#15758=DIRECTION('center_axis',(1.,0.,0.));
#15759=DIRECTION('ref_axis',(0.,0.,-1.));
#15760=DIRECTION('',(0.,-0.156434465040231,-0.987688340595138));
#15761=DIRECTION('',(0.,1.,0.));
#15762=DIRECTION('',(0.,-0.707106781186547,-0.707106781186547));
#15763=DIRECTION('',(0.,0.707106781186547,-0.707106781186547));
#15764=DIRECTION('',(0.,-1.,0.));
#15765=DIRECTION('',(0.,0.707106781186543,0.707106781186552));
#15766=DIRECTION('',(0.,0.,-1.));
#15767=DIRECTION('',(0.,0.987688340595138,0.156434465040231));
#15768=DIRECTION('center_axis',(0.,-0.987688340595138,0.156434465040231));
#15769=DIRECTION('ref_axis',(0.,-0.156434465040231,-0.987688340595138));
#15770=DIRECTION('',(0.707106781186546,0.110615871041237,0.698401123333712));
#15771=DIRECTION('',(0.,0.156434465040231,0.987688340595138));
#15772=DIRECTION('',(1.,0.,0.));
#15773=DIRECTION('center_axis',(-1.,0.,0.));
#15774=DIRECTION('ref_axis',(0.,0.707106781186547,0.707106781186548));
#15775=DIRECTION('',(-0.707106781186546,-0.698401123333712,-0.110615871041237));
#15776=DIRECTION('center_axis',(-1.,0.,0.));
#15777=DIRECTION('ref_axis',(0.,0.,1.));
#15778=DIRECTION('center_axis',(1.,0.,0.));
#15779=DIRECTION('ref_axis',(0.,0.,-1.));
#15780=DIRECTION('',(0.,-0.987688340595138,-0.156434465040231));
#15781=DIRECTION('',(0.,0.,1.));
#15782=DIRECTION('',(0.,-0.707106781186543,-0.707106781186552));
#15783=DIRECTION('',(0.,1.,0.));
#15784=DIRECTION('',(0.,-0.707106781186547,0.707106781186547));
#15785=DIRECTION('',(0.,0.707106781186547,0.707106781186547));
#15786=DIRECTION('',(0.,-1.,0.));
#15787=DIRECTION('center_axis',(0.,0.156434465040231,-0.987688340595138));
#15788=DIRECTION('ref_axis',(0.,0.987688340595138,0.156434465040231));
#15789=DIRECTION('',(1.,0.,0.));
#15790=DIRECTION('center_axis',(0.,0.707106781186548,-0.707106781186548));
#15791=DIRECTION('ref_axis',(-1.,0.,0.));
#15792=DIRECTION('',(-1.,0.,0.));
#15793=DIRECTION('center_axis',(0.,0.707106781186548,0.707106781186548));
#15794=DIRECTION('ref_axis',(1.,0.,0.));
#15795=DIRECTION('',(1.,0.,0.));
#15796=DIRECTION('center_axis',(0.,0.,1.));
#15797=DIRECTION('ref_axis',(0.,-1.,0.));
#15798=DIRECTION('',(-1.,0.,0.));
#15799=DIRECTION('center_axis',(0.,-0.707106781186552,0.707106781186543));
#15800=DIRECTION('ref_axis',(1.,0.,0.));
#15801=DIRECTION('',(1.,0.,0.));
#15802=DIRECTION('center_axis',(0.,-1.,0.));
#15803=DIRECTION('ref_axis',(0.,0.,-1.));
#15804=DIRECTION('center_axis',(0.,0.,-1.));
#15805=DIRECTION('ref_axis',(0.,1.,0.));
#15806=DIRECTION('axis',(0.,0.,1.));
#15807=DIRECTION('refdir',(1.,0.,0.));
#15808=DIRECTION('center_axis',(0.,0.987688340595138,-0.156434465040231));
#15809=DIRECTION('ref_axis',(0.,0.156434465040231,0.987688340595138));
#15810=DIRECTION('',(-0.707106781186555,-0.110615871041236,-0.698401123333703));
#15811=DIRECTION('',(0.,-0.156434465040231,-0.987688340595138));
#15812=DIRECTION('',(1.,0.,0.));
#15813=DIRECTION('',(0.,0.156434465040231,0.987688340595138));
#15814=DIRECTION('',(-0.707106781186547,0.110615871041237,0.698401123333711));
#15815=DIRECTION('',(-1.,0.,0.));
#15816=DIRECTION('center_axis',(0.,-0.156434465040231,0.987688340595138));
#15817=DIRECTION('ref_axis',(0.,-0.987688340595138,-0.156434465040231));
#15818=DIRECTION('',(0.707106781186555,0.698401123333703,0.110615871041236));
#15819=DIRECTION('',(1.,0.,0.));
#15820=DIRECTION('',(0.707106781186547,-0.69840112333371,-0.110615871041237));
#15821=DIRECTION('',(0.,-0.987688340595138,-0.156434465040231));
#15822=DIRECTION('',(-1.,0.,0.));
#15823=DIRECTION('',(0.,0.987688340595138,0.156434465040231));
#15824=DIRECTION('center_axis',(-1.,0.,0.));
#15825=DIRECTION('ref_axis',(0.,0.707106781186547,0.707106781186548));
#15826=DIRECTION('center_axis',(1.,0.,0.));
#15827=DIRECTION('ref_axis',(0.,0.,-1.));
#15828=DIRECTION('center_axis',(1.,0.,0.));
#15829=DIRECTION('ref_axis',(0.,0.,-1.));
#15830=DIRECTION('center_axis',(1.,0.,0.));
#15831=DIRECTION('ref_axis',(0.,0.,-1.));
#15832=DIRECTION('center_axis',(1.,0.,0.));
#15833=DIRECTION('ref_axis',(0.,0.,-1.));
#15834=DIRECTION('center_axis',(1.,0.,0.));
#15835=DIRECTION('ref_axis',(0.,0.707106781186547,0.707106781186548));
#15836=DIRECTION('center_axis',(1.,0.,0.));
#15837=DIRECTION('ref_axis',(0.,0.,-1.));
#15838=DIRECTION('center_axis',(-1.,0.,0.));
#15839=DIRECTION('ref_axis',(0.,0.,1.));
#15840=DIRECTION('center_axis',(1.,0.,0.));
#15841=DIRECTION('ref_axis',(0.,0.,-1.));
#15842=DIRECTION('center_axis',(1.,0.,0.));
#15843=DIRECTION('ref_axis',(0.,0.707106781186547,0.707106781186548));
#15844=DIRECTION('center_axis',(1.,0.,0.));
#15845=DIRECTION('ref_axis',(0.,0.,-1.));
#15846=DIRECTION('center_axis',(1.,0.,0.));
#15847=DIRECTION('ref_axis',(0.,0.707106781186547,0.707106781186548));
#15848=DIRECTION('axis',(0.,0.,1.));
#15849=DIRECTION('refdir',(1.,0.,0.));
#15850=DIRECTION('center_axis',(0.,0.258819045102523,0.965925826289068));
#15851=DIRECTION('ref_axis',(0.,-0.965925826289068,0.258819045102523));
#15852=DIRECTION('',(-1.,0.,0.));
#15853=DIRECTION('',(0.,-0.965925826289068,0.258819045102523));
#15854=DIRECTION('',(1.,0.,0.));
#15855=DIRECTION('',(0.,0.965925826289068,-0.258819045102523));
#15856=DIRECTION('center_axis',(1.,0.,0.));
#15857=DIRECTION('ref_axis',(0.,0.,-1.));
#15858=DIRECTION('center_axis',(-1.,0.,0.));
#15859=DIRECTION('ref_axis',(0.,1.,0.));
#15860=DIRECTION('center_axis',(1.,0.,0.));
#15861=DIRECTION('ref_axis',(0.,1.,0.));
#15862=DIRECTION('',(0.,-0.965925826289068,0.258819045102523));
#15863=DIRECTION('center_axis',(0.,-0.258819045102523,-0.965925826289068));
#15864=DIRECTION('ref_axis',(0.,0.965925826289068,-0.258819045102523));
#15865=DIRECTION('',(1.,0.,0.));
#15866=DIRECTION('',(-1.,0.,0.));
#15867=DIRECTION('',(0.,0.965925826289068,-0.258819045102523));
#15868=DIRECTION('center_axis',(1.,0.,0.));
#15869=DIRECTION('ref_axis',(0.,0.,-1.));
#15870=DIRECTION('center_axis',(1.,0.,0.));
#15871=DIRECTION('ref_axis',(0.,1.,0.));
#15872=DIRECTION('center_axis',(-1.,0.,0.));
#15873=DIRECTION('ref_axis',(0.,1.,0.));
#15874=DIRECTION('center_axis',(0.,-0.707106781186549,0.707106781186546));
#15875=DIRECTION('ref_axis',(0.,-0.707106781186546,-0.707106781186549));
#15876=DIRECTION('',(-1.,0.,0.));
#15877=DIRECTION('',(0.,-0.707106781186546,-0.707106781186549));
#15878=DIRECTION('',(1.,0.,0.));
#15879=DIRECTION('',(0.,0.707106781186546,0.707106781186549));
#15880=DIRECTION('center_axis',(1.,0.,0.));
#15881=DIRECTION('ref_axis',(0.,0.,-1.));
#15882=DIRECTION('center_axis',(-1.,0.,0.));
#15883=DIRECTION('ref_axis',(0.,1.,0.));
#15884=DIRECTION('center_axis',(1.,0.,0.));
#15885=DIRECTION('ref_axis',(0.,1.,0.));
#15886=DIRECTION('',(0.,-0.707106781186547,-0.707106781186547));
#15887=DIRECTION('center_axis',(0.,0.707106781186548,-0.707106781186548));
#15888=DIRECTION('ref_axis',(0.,0.707106781186548,0.707106781186548));
#15889=DIRECTION('',(1.,0.,0.));
#15890=DIRECTION('',(-1.,0.,0.));
#15891=DIRECTION('',(0.,0.707106781186547,0.707106781186547));
#15892=DIRECTION('center_axis',(1.,0.,0.));
#15893=DIRECTION('ref_axis',(0.,0.,-1.));
#15894=DIRECTION('center_axis',(1.,0.,0.));
#15895=DIRECTION('ref_axis',(0.,1.,0.));
#15896=DIRECTION('center_axis',(-1.,0.,0.));
#15897=DIRECTION('ref_axis',(0.,1.,0.));
#15898=DIRECTION('center_axis',(0.,-0.965925826289068,-0.258819045102522));
#15899=DIRECTION('ref_axis',(0.,0.258819045102522,-0.965925826289068));
#15900=DIRECTION('',(-1.,0.,0.));
#15901=DIRECTION('',(0.,0.258819045102522,-0.965925826289068));
#15902=DIRECTION('',(1.,0.,0.));
#15903=DIRECTION('',(0.,-0.258819045102522,0.965925826289068));
#15904=DIRECTION('center_axis',(1.,0.,0.));
#15905=DIRECTION('ref_axis',(0.,0.,-1.));
#15906=DIRECTION('center_axis',(-1.,0.,0.));
#15907=DIRECTION('ref_axis',(0.,1.,0.));
#15908=DIRECTION('center_axis',(1.,0.,0.));
#15909=DIRECTION('ref_axis',(0.,1.,0.));
#15910=DIRECTION('',(0.,0.25881904510252,-0.965925826289068));
#15911=DIRECTION('center_axis',(0.,0.965925826289069,0.25881904510252));
#15912=DIRECTION('ref_axis',(0.,-0.25881904510252,0.965925826289069));
#15913=DIRECTION('',(1.,0.,0.));
#15914=DIRECTION('',(-1.,0.,0.));
#15915=DIRECTION('',(0.,-0.25881904510252,0.965925826289068));
#15916=DIRECTION('center_axis',(1.,0.,0.));
#15917=DIRECTION('ref_axis',(0.,0.,-1.));
#15918=DIRECTION('center_axis',(1.,0.,0.));
#15919=DIRECTION('ref_axis',(0.,1.,0.));
#15920=DIRECTION('center_axis',(-1.,0.,0.));
#15921=DIRECTION('ref_axis',(0.,1.,0.));
#15922=DIRECTION('center_axis',(0.,-0.25881904510252,-0.965925826289069));
#15923=DIRECTION('ref_axis',(0.,0.965925826289069,-0.25881904510252));
#15924=DIRECTION('',(-1.,0.,0.));
#15925=DIRECTION('',(0.,0.965925826289068,-0.25881904510252));
#15926=DIRECTION('',(1.,0.,0.));
#15927=DIRECTION('',(0.,-0.965925826289068,0.25881904510252));
#15928=DIRECTION('center_axis',(1.,0.,0.));
#15929=DIRECTION('ref_axis',(0.,0.,-1.));
#15930=DIRECTION('center_axis',(-1.,0.,0.));
#15931=DIRECTION('ref_axis',(0.,1.,0.));
#15932=DIRECTION('center_axis',(1.,0.,0.));
#15933=DIRECTION('ref_axis',(0.,1.,0.));
#15934=DIRECTION('',(0.,0.965925826289069,-0.25881904510252));
#15935=DIRECTION('center_axis',(0.,0.25881904510252,0.965925826289069));
#15936=DIRECTION('ref_axis',(0.,-0.965925826289069,0.25881904510252));
#15937=DIRECTION('',(1.,0.,0.));
#15938=DIRECTION('',(-1.,0.,0.));
#15939=DIRECTION('',(0.,-0.965925826289069,0.25881904510252));
#15940=DIRECTION('center_axis',(1.,0.,0.));
#15941=DIRECTION('ref_axis',(0.,0.,-1.));
#15942=DIRECTION('center_axis',(1.,0.,0.));
#15943=DIRECTION('ref_axis',(0.,1.,0.));
#15944=DIRECTION('center_axis',(-1.,0.,0.));
#15945=DIRECTION('ref_axis',(0.,1.,0.));
#15946=DIRECTION('center_axis',(0.,0.965925826289069,0.25881904510252));
#15947=DIRECTION('ref_axis',(0.,-0.25881904510252,0.965925826289069));
#15948=DIRECTION('',(-1.,0.,0.));
#15949=DIRECTION('',(0.,-0.25881904510252,0.965925826289068));
#15950=DIRECTION('',(1.,0.,0.));
#15951=DIRECTION('',(0.,0.25881904510252,-0.965925826289068));
#15952=DIRECTION('center_axis',(1.,0.,0.));
#15953=DIRECTION('ref_axis',(0.,0.,-1.));
#15954=DIRECTION('center_axis',(-1.,0.,0.));
#15955=DIRECTION('ref_axis',(0.,1.,0.));
#15956=DIRECTION('center_axis',(1.,0.,0.));
#15957=DIRECTION('ref_axis',(0.,1.,0.));
#15958=DIRECTION('',(0.,-0.25881904510252,0.965925826289069));
#15959=DIRECTION('center_axis',(0.,-0.965925826289069,-0.25881904510252));
#15960=DIRECTION('ref_axis',(0.,0.25881904510252,-0.965925826289069));
#15961=DIRECTION('',(1.,0.,0.));
#15962=DIRECTION('',(-1.,0.,0.));
#15963=DIRECTION('',(0.,0.25881904510252,-0.965925826289069));
#15964=DIRECTION('center_axis',(1.,0.,0.));
#15965=DIRECTION('ref_axis',(0.,0.,-1.));
#15966=DIRECTION('center_axis',(1.,0.,0.));
#15967=DIRECTION('ref_axis',(0.,1.,0.));
#15968=DIRECTION('center_axis',(-1.,0.,0.));
#15969=DIRECTION('ref_axis',(0.,1.,0.));
#15970=DIRECTION('center_axis',(0.,-0.156434465040231,0.987688340595138));
#15971=DIRECTION('ref_axis',(0.,-0.987688340595138,-0.156434465040231));
#15972=DIRECTION('',(-1.,0.,0.));
#15973=DIRECTION('',(0.,0.987688340595138,0.156434465040231));
#15974=DIRECTION('',(1.,0.,0.));
#15975=DIRECTION('',(0.,-0.987688340595138,-0.156434465040231));
#15976=DIRECTION('center_axis',(0.,0.987688340595138,-0.156434465040231));
#15977=DIRECTION('ref_axis',(0.,0.156434465040231,0.987688340595138));
#15978=DIRECTION('',(1.,0.,0.));
#15979=DIRECTION('',(0.,0.156434465040231,0.987688340595138));
#15980=DIRECTION('',(-1.,0.,0.));
#15981=DIRECTION('',(0.,-0.156434465040231,-0.987688340595138));
#15982=DIRECTION('center_axis',(1.,0.,0.));
#15983=DIRECTION('ref_axis',(0.,0.,-1.));
#15984=DIRECTION('center_axis',(1.,0.,0.));
#15985=DIRECTION('ref_axis',(0.,0.,-1.));
#15986=DIRECTION('center_axis',(1.,0.,0.));
#15987=DIRECTION('ref_axis',(0.,0.,-1.));
#15988=DIRECTION('center_axis',(1.,0.,0.));
#15989=DIRECTION('ref_axis',(0.,0.707106781186547,0.707106781186548));
#15990=DIRECTION('center_axis',(1.,0.,0.));
#15991=DIRECTION('ref_axis',(0.,0.,-1.));
#15992=DIRECTION('center_axis',(1.,0.,0.));
#15993=DIRECTION('ref_axis',(0.,0.707106781186547,0.707106781186548));
#15994=DIRECTION('center_axis',(1.,0.,0.));
#15995=DIRECTION('ref_axis',(0.,0.,-1.));
#15996=DIRECTION('center_axis',(-1.,0.,0.));
#15997=DIRECTION('ref_axis',(0.,0.,1.));
#15998=DIRECTION('axis',(0.,0.,1.));
#15999=DIRECTION('refdir',(1.,0.,0.));
#16000=DIRECTION('center_axis',(0.,0.,1.));
#16001=DIRECTION('ref_axis',(1.,0.,0.));
#16002=DIRECTION('center_axis',(0.,-1.,0.));
#16003=DIRECTION('ref_axis',(-1.,0.,0.));
#16004=DIRECTION('axis',(0.,0.,1.));
#16005=DIRECTION('refdir',(1.,0.,0.));
#16006=DIRECTION('center_axis',(0.,-1.,0.));
#16007=DIRECTION('ref_axis',(0.314059274495562,0.,-0.94940337691801));
#16008=DIRECTION('',(0.,1.,0.));
#16009=DIRECTION('center_axis',(0.,1.,0.));
#16010=DIRECTION('ref_axis',(1.,0.,1.05892830722154E-13));
#16011=DIRECTION('center_axis',(0.,-1.,0.));
#16012=DIRECTION('ref_axis',(0.314059274495562,0.,-0.94940337691801));
#16013=DIRECTION('',(0.,1.,0.));
#16014=DIRECTION('center_axis',(0.,-1.,0.));
#16015=DIRECTION('ref_axis',(0.314059274495562,0.,-0.94940337691801));
#16016=DIRECTION('',(0.,1.,0.));
#16017=DIRECTION('center_axis',(0.,-1.,0.));
#16018=DIRECTION('ref_axis',(0.314059274495562,0.,-0.94940337691801));
#16019=DIRECTION('',(0.,1.,0.));
#16020=DIRECTION('center_axis',(0.,-1.,0.));
#16021=DIRECTION('ref_axis',(0.314059274495562,0.,-0.94940337691801));
#16022=DIRECTION('',(0.,1.,0.));
#16023=DIRECTION('center_axis',(0.,-1.,0.));
#16024=DIRECTION('ref_axis',(0.314059274495562,0.,-0.94940337691801));
#16025=DIRECTION('',(0.,1.,0.));
#16026=DIRECTION('center_axis',(0.,-1.,0.));
#16027=DIRECTION('ref_axis',(0.314059274495562,0.,-0.94940337691801));
#16028=DIRECTION('',(0.,1.,0.));
#16029=DIRECTION('center_axis',(0.,-1.,0.));
#16030=DIRECTION('ref_axis',(0.314059274495562,0.,-0.94940337691801));
#16031=DIRECTION('',(0.,1.,0.));
#16032=DIRECTION('center_axis',(0.,-1.,0.));
#16033=DIRECTION('ref_axis',(0.314059274495562,0.,-0.94940337691801));
#16034=DIRECTION('',(0.,1.,0.));
#16035=DIRECTION('center_axis',(0.,-1.,0.));
#16036=DIRECTION('ref_axis',(0.314059274495562,0.,-0.94940337691801));
#16037=DIRECTION('',(0.,1.,0.));
#16038=DIRECTION('center_axis',(0.,-1.,0.));
#16039=DIRECTION('ref_axis',(0.314059274495562,0.,-0.94940337691801));
#16040=DIRECTION('',(0.,1.,0.));
#16041=DIRECTION('center_axis',(0.,-1.,0.));
#16042=DIRECTION('ref_axis',(0.314059274495562,0.,-0.94940337691801));
#16043=DIRECTION('',(0.,1.,0.));
#16044=DIRECTION('center_axis',(0.,-1.,0.));
#16045=DIRECTION('ref_axis',(0.314059274495562,0.,-0.94940337691801));
#16046=DIRECTION('',(0.,1.,0.));
#16047=DIRECTION('center_axis',(0.,-1.,0.));
#16048=DIRECTION('ref_axis',(0.314059274495562,0.,-0.94940337691801));
#16049=DIRECTION('',(0.,1.,0.));
#16050=DIRECTION('center_axis',(0.,-1.,0.));
#16051=DIRECTION('ref_axis',(0.314059274495562,0.,-0.94940337691801));
#16052=DIRECTION('',(0.,1.,0.));
#16053=DIRECTION('center_axis',(0.,-1.,0.));
#16054=DIRECTION('ref_axis',(0.314059274495562,0.,-0.94940337691801));
#16055=DIRECTION('',(0.,1.,0.));
#16056=DIRECTION('center_axis',(0.,-1.,0.));
#16057=DIRECTION('ref_axis',(0.314059274495562,0.,-0.94940337691801));
#16058=DIRECTION('',(0.,1.,0.));
#16059=DIRECTION('center_axis',(0.,-1.,0.));
#16060=DIRECTION('ref_axis',(0.314059274495562,0.,-0.94940337691801));
#16061=DIRECTION('',(0.,1.,0.));
#16062=DIRECTION('center_axis',(0.,-1.,0.));
#16063=DIRECTION('ref_axis',(0.314059274495562,0.,-0.94940337691801));
#16064=DIRECTION('',(0.,1.,0.));
#16065=DIRECTION('center_axis',(0.,-1.,0.));
#16066=DIRECTION('ref_axis',(1.,0.,0.));
#16067=DIRECTION('center_axis',(0.,1.,0.));
#16068=DIRECTION('ref_axis',(1.,0.,0.));
#16069=DIRECTION('center_axis',(0.,-1.,0.));
#16070=DIRECTION('ref_axis',(1.,0.,0.));
#16071=DIRECTION('center_axis',(0.,-1.,0.));
#16072=DIRECTION('ref_axis',(1.,0.,0.));
#16073=DIRECTION('center_axis',(0.,-1.,0.));
#16074=DIRECTION('ref_axis',(-0.3010495107773,0.,-0.953608510899912));
#16075=DIRECTION('center_axis',(0.,-1.,0.));
#16076=DIRECTION('ref_axis',(1.,0.,1.05892830722154E-13));
#16077=DIRECTION('center_axis',(0.,1.,0.));
#16078=DIRECTION('ref_axis',(0.,0.,1.));
#16079=DIRECTION('center_axis',(0.,-1.,0.));
#16080=DIRECTION('ref_axis',(1.,0.,0.));
#16081=DIRECTION('center_axis',(0.,1.,0.));
#16082=DIRECTION('ref_axis',(0.,0.,1.));
#16083=DIRECTION('center_axis',(0.,1.,0.));
#16084=DIRECTION('ref_axis',(1.,0.,0.));
#16085=DIRECTION('center_axis',(0.,1.,0.));
#16086=DIRECTION('ref_axis',(1.,0.,0.));
#16087=DIRECTION('center_axis',(0.,1.,0.));
#16088=DIRECTION('ref_axis',(0.,0.,1.));
#16089=DIRECTION('center_axis',(0.,-1.,0.));
#16090=DIRECTION('ref_axis',(1.,0.,0.));
#16091=DIRECTION('center_axis',(1.,0.,0.));
#16092=DIRECTION('ref_axis',(0.,0.,-1.));
#16093=DIRECTION('center_axis',(0.,1.,0.));
#16094=DIRECTION('ref_axis',(1.,0.,0.));
#16095=DIRECTION('center_axis',(0.,1.,0.));
#16096=DIRECTION('ref_axis',(1.,0.,0.));
#16097=DIRECTION('center_axis',(0.,1.,0.));
#16098=DIRECTION('ref_axis',(1.,0.,0.));
#16099=DIRECTION('',(0.707106781186547,-0.707106781186548,-8.65956056235493E-17));
#16100=DIRECTION('center_axis',(0.,1.,0.));
#16101=DIRECTION('ref_axis',(1.,0.,0.));
#16102=DIRECTION('center_axis',(0.,1.,0.));
#16103=DIRECTION('ref_axis',(1.,0.,0.));
#16104=DIRECTION('center_axis',(-0.241286600017026,0.,0.970453902383943));
#16105=DIRECTION('ref_axis',(-0.970453902383943,0.,-0.241286600017026));
#16106=DIRECTION('',(0.,1.,0.));
#16107=DIRECTION('',(-0.970453902383943,0.,-0.241286600017026));
#16108=DIRECTION('',(0.,-1.,0.));
#16109=DIRECTION('center_axis',(-0.558650020314832,0.,-0.829403493362693));
#16110=DIRECTION('ref_axis',(0.829403493362693,0.,-0.558650020314832));
#16111=DIRECTION('',(0.,-1.,0.));
#16112=DIRECTION('',(0.829403493362693,0.,-0.558650020314832));
#16113=DIRECTION('center_axis',(0.,-1.,0.));
#16114=DIRECTION('ref_axis',(-0.17364817766693,0.,-0.984807753012208));
#16115=DIRECTION('center_axis',(0.,-1.,0.));
#16116=DIRECTION('ref_axis',(1.,0.,0.));
#16117=DIRECTION('center_axis',(0.,-1.,0.));
#16118=DIRECTION('ref_axis',(1.,0.,0.));
#16119=DIRECTION('center_axis',(0.,1.,0.));
#16120=DIRECTION('ref_axis',(1.,0.,0.));
#16121=DIRECTION('center_axis',(0.,1.,0.));
#16122=DIRECTION('ref_axis',(1.,0.,0.));
#16123=DIRECTION('center_axis',(0.,1.,0.));
#16124=DIRECTION('ref_axis',(1.,0.,0.));
#16125=DIRECTION('center_axis',(0.,1.,0.));
#16126=DIRECTION('ref_axis',(1.,0.,0.));
#16127=DIRECTION('center_axis',(0.,1.,0.));
#16128=DIRECTION('ref_axis',(1.,0.,0.));
#16129=DIRECTION('center_axis',(0.,1.,0.));
#16130=DIRECTION('ref_axis',(1.,0.,0.));
#16131=DIRECTION('center_axis',(0.,1.,0.));
#16132=DIRECTION('ref_axis',(1.,0.,0.));
#16133=DIRECTION('center_axis',(0.,1.,0.));
#16134=DIRECTION('ref_axis',(1.,0.,0.));
#16135=DIRECTION('center_axis',(0.,1.,0.));
#16136=DIRECTION('ref_axis',(1.,0.,0.));
#16137=DIRECTION('center_axis',(0.,1.,0.));
#16138=DIRECTION('ref_axis',(1.,0.,0.));
#16139=DIRECTION('center_axis',(0.,1.,0.));
#16140=DIRECTION('ref_axis',(1.,0.,0.));
#16141=DIRECTION('center_axis',(0.,1.,0.));
#16142=DIRECTION('ref_axis',(1.,0.,0.));
#16143=DIRECTION('center_axis',(0.,1.,0.));
#16144=DIRECTION('ref_axis',(1.,0.,0.));
#16145=DIRECTION('center_axis',(0.,1.,0.));
#16146=DIRECTION('ref_axis',(1.,0.,0.));
#16147=DIRECTION('center_axis',(0.,1.,0.));
#16148=DIRECTION('ref_axis',(1.,0.,0.));
#16149=DIRECTION('center_axis',(0.,1.,0.));
#16150=DIRECTION('ref_axis',(1.,0.,0.));
#16151=DIRECTION('center_axis',(0.,1.,0.));
#16152=DIRECTION('ref_axis',(1.,0.,0.));
#16153=DIRECTION('center_axis',(0.,1.,0.));
#16154=DIRECTION('ref_axis',(1.,0.,0.));
#16155=DIRECTION('center_axis',(0.,1.,0.));
#16156=DIRECTION('ref_axis',(1.,0.,0.));
#16157=DIRECTION('center_axis',(0.,1.,0.));
#16158=DIRECTION('ref_axis',(1.,0.,0.));
#16159=DIRECTION('center_axis',(0.,1.,0.));
#16160=DIRECTION('ref_axis',(1.,0.,0.));
#16161=DIRECTION('center_axis',(0.,1.,0.));
#16162=DIRECTION('ref_axis',(1.,0.,0.));
#16163=DIRECTION('center_axis',(0.,1.,0.));
#16164=DIRECTION('ref_axis',(1.,0.,0.));
#16165=DIRECTION('center_axis',(0.,1.,0.));
#16166=DIRECTION('ref_axis',(1.,0.,0.));
#16167=DIRECTION('center_axis',(0.,1.,0.));
#16168=DIRECTION('ref_axis',(1.,0.,0.));
#16169=DIRECTION('center_axis',(0.,1.,0.));
#16170=DIRECTION('ref_axis',(1.,0.,0.));
#16171=DIRECTION('center_axis',(0.,1.,0.));
#16172=DIRECTION('ref_axis',(1.,0.,0.));
#16173=DIRECTION('center_axis',(0.,1.,0.));
#16174=DIRECTION('ref_axis',(1.,0.,0.));
#16175=DIRECTION('center_axis',(0.,1.,0.));
#16176=DIRECTION('ref_axis',(1.,0.,0.));
#16177=DIRECTION('center_axis',(0.,1.,0.));
#16178=DIRECTION('ref_axis',(1.,0.,0.));
#16179=DIRECTION('center_axis',(0.,1.,0.));
#16180=DIRECTION('ref_axis',(1.,0.,0.));
#16181=DIRECTION('center_axis',(0.,1.,0.));
#16182=DIRECTION('ref_axis',(1.,0.,0.));
#16183=DIRECTION('center_axis',(0.,1.,0.));
#16184=DIRECTION('ref_axis',(1.,0.,0.));
#16185=DIRECTION('center_axis',(0.,1.,0.));
#16186=DIRECTION('ref_axis',(1.,0.,0.));
#16187=DIRECTION('center_axis',(0.,1.,0.));
#16188=DIRECTION('ref_axis',(1.,0.,0.));
#16189=DIRECTION('center_axis',(0.,1.,0.));
#16190=DIRECTION('ref_axis',(1.,0.,0.));
#16191=DIRECTION('',(0.707106781186547,0.707106781186548,8.65956056235493E-17));
#16192=DIRECTION('center_axis',(0.,-1.,0.));
#16193=DIRECTION('ref_axis',(1.,0.,0.));
#16194=DIRECTION('center_axis',(-0.0691033627359896,0.,0.997609505397066));
#16195=DIRECTION('ref_axis',(-0.997609505397066,0.,-0.0691033627359896));
#16196=DIRECTION('',(0.,1.,0.));
#16197=DIRECTION('',(-0.997609505397066,0.,-0.0691033627359896));
#16198=DIRECTION('',(0.,-1.,0.));
#16199=DIRECTION('center_axis',(-0.694187276399492,0.,-0.719794432657725));
#16200=DIRECTION('ref_axis',(0.719794432657725,0.,-0.694187276399492));
#16201=DIRECTION('',(0.,-1.,0.));
#16202=DIRECTION('',(0.719794432657725,0.,-0.694187276399492));
#16203=DIRECTION('center_axis',(0.,-1.,0.));
#16204=DIRECTION('ref_axis',(-0.342020143325669,0.,-0.939692620785908));
#16205=DIRECTION('center_axis',(0.,-1.,0.));
#16206=DIRECTION('ref_axis',(1.,0.,0.));
#16207=DIRECTION('center_axis',(0.10517954525379,0.,0.994453248403466));
#16208=DIRECTION('ref_axis',(-0.994453248403466,0.,0.10517954525379));
#16209=DIRECTION('',(0.,1.,0.));
#16210=DIRECTION('',(-0.994453248403466,0.,0.10517954525379));
#16211=DIRECTION('',(0.,-1.,0.));
#16212=DIRECTION('center_axis',(-0.808632003366464,0.,-0.58831478235001));
#16213=DIRECTION('ref_axis',(0.58831478235001,0.,-0.808632003366464));
#16214=DIRECTION('',(0.,-1.,0.));
#16215=DIRECTION('',(0.58831478235001,0.,-0.808632003366464));
#16216=DIRECTION('center_axis',(0.,-1.,0.));
#16217=DIRECTION('ref_axis',(-0.5,0.,-0.866025403784438));
#16218=DIRECTION('center_axis',(0.,-1.,0.));
#16219=DIRECTION('ref_axis',(1.,0.,0.));
#16220=DIRECTION('center_axis',(0.276266625984452,0.,0.961081032674752));
#16221=DIRECTION('ref_axis',(-0.961081032674752,0.,0.276266625984452));
#16222=DIRECTION('',(0.,1.,0.));
#16223=DIRECTION('',(-0.961081032674752,0.,0.276266625984452));
#16224=DIRECTION('',(0.,-1.,0.));
#16225=DIRECTION('center_axis',(-0.898506856098683,0.,-0.438959485082234));
#16226=DIRECTION('ref_axis',(0.438959485082234,0.,-0.898506856098683));
#16227=DIRECTION('',(0.,-1.,0.));
#16228=DIRECTION('',(0.438959485082234,0.,-0.898506856098683));
#16229=DIRECTION('center_axis',(0.,-1.,0.));
#16230=DIRECTION('ref_axis',(-0.64278760968654,0.,-0.766044443118978));
#16231=DIRECTION('center_axis',(0.,-1.,0.));
#16232=DIRECTION('ref_axis',(1.,0.,0.));
#16233=DIRECTION('center_axis',(0.438959485082234,0.,0.898506856098683));
#16234=DIRECTION('ref_axis',(-0.898506856098683,0.,0.438959485082234));
#16235=DIRECTION('',(0.,1.,0.));
#16236=DIRECTION('',(-0.898506856098683,0.,0.438959485082234));
#16237=DIRECTION('',(0.,-1.,0.));
#16238=DIRECTION('center_axis',(-0.961081032674752,0.,-0.276266625984452));
#16239=DIRECTION('ref_axis',(0.276266625984452,0.,-0.961081032674752));
#16240=DIRECTION('',(0.,-1.,0.));
#16241=DIRECTION('',(0.276266625984452,0.,-0.961081032674752));
#16242=DIRECTION('center_axis',(0.,-1.,0.));
#16243=DIRECTION('ref_axis',(-0.766044443118978,0.,-0.642787609686539));
#16244=DIRECTION('center_axis',(0.,-1.,0.));
#16245=DIRECTION('ref_axis',(1.,0.,0.));
#16246=DIRECTION('center_axis',(0.58831478235001,0.,0.808632003366464));
#16247=DIRECTION('ref_axis',(-0.808632003366464,0.,0.58831478235001));
#16248=DIRECTION('',(0.,1.,0.));
#16249=DIRECTION('',(-0.808632003366464,0.,0.58831478235001));
#16250=DIRECTION('',(0.,-1.,0.));
#16251=DIRECTION('center_axis',(-0.994453248403466,0.,-0.10517954525379));
#16252=DIRECTION('ref_axis',(0.10517954525379,0.,-0.994453248403466));
#16253=DIRECTION('',(0.,-1.,0.));
#16254=DIRECTION('',(0.10517954525379,0.,-0.994453248403466));
#16255=DIRECTION('center_axis',(0.,-1.,0.));
#16256=DIRECTION('ref_axis',(-0.866025403784439,0.,-0.5));
#16257=DIRECTION('center_axis',(0.,-1.,0.));
#16258=DIRECTION('ref_axis',(1.,0.,0.));
#16259=DIRECTION('center_axis',(0.719794432657726,0.,0.694187276399491));
#16260=DIRECTION('ref_axis',(-0.694187276399491,0.,0.719794432657726));
#16261=DIRECTION('',(0.,1.,0.));
#16262=DIRECTION('',(-0.694187276399491,0.,0.719794432657726));
#16263=DIRECTION('',(0.,-1.,0.));
#16264=DIRECTION('center_axis',(-0.997609505397066,0.,0.0691033627359909));
#16265=DIRECTION('ref_axis',(-0.0691033627359909,0.,-0.997609505397066));
#16266=DIRECTION('',(0.,-1.,0.));
#16267=DIRECTION('',(-0.0691033627359909,0.,-0.997609505397066));
#16268=DIRECTION('center_axis',(0.,-1.,0.));
#16269=DIRECTION('ref_axis',(-0.939692620785909,0.,-0.342020143325668));
#16270=DIRECTION('center_axis',(0.,-1.,0.));
#16271=DIRECTION('ref_axis',(1.,0.,0.));
#16272=DIRECTION('center_axis',(0.829403493362693,0.,0.558650020314831));
#16273=DIRECTION('ref_axis',(-0.558650020314831,0.,0.829403493362693));
#16274=DIRECTION('',(0.,1.,0.));
#16275=DIRECTION('',(-0.558650020314831,0.,0.829403493362693));
#16276=DIRECTION('',(0.,-1.,0.));
#16277=DIRECTION('center_axis',(-0.970453902383943,0.,0.241286600017027));
#16278=DIRECTION('ref_axis',(-0.241286600017027,0.,-0.970453902383943));
#16279=DIRECTION('',(0.,-1.,0.));
#16280=DIRECTION('',(-0.241286600017027,0.,-0.970453902383943));
#16281=DIRECTION('center_axis',(0.,-1.,0.));
#16282=DIRECTION('ref_axis',(-0.984807753012208,0.,-0.17364817766693));
#16283=DIRECTION('center_axis',(0.,-1.,0.));
#16284=DIRECTION('ref_axis',(1.,0.,0.));
#16285=DIRECTION('center_axis',(0.913811548620253,0.,0.406138466053456));
#16286=DIRECTION('ref_axis',(-0.406138466053456,0.,0.913811548620253));
#16287=DIRECTION('',(0.,1.,0.));
#16288=DIRECTION('',(-0.406138466053456,0.,0.913811548620253));
#16289=DIRECTION('',(0.,-1.,0.));
#16290=DIRECTION('center_axis',(-0.913811548620253,0.,0.406138466053456));
#16291=DIRECTION('ref_axis',(-0.406138466053456,0.,-0.913811548620253));
#16292=DIRECTION('',(0.,-1.,0.));
#16293=DIRECTION('',(-0.406138466053456,0.,-0.913811548620253));
#16294=DIRECTION('center_axis',(0.,-1.,0.));
#16295=DIRECTION('ref_axis',(-1.,0.,1.83697019872103E-16));
#16296=DIRECTION('center_axis',(0.,-1.,0.));
#16297=DIRECTION('ref_axis',(1.,0.,0.));
#16298=DIRECTION('center_axis',(0.970453902383943,0.,0.241286600017026));
#16299=DIRECTION('ref_axis',(-0.241286600017026,0.,0.970453902383943));
#16300=DIRECTION('',(0.,1.,0.));
#16301=DIRECTION('',(-0.241286600017026,0.,0.970453902383943));
#16302=DIRECTION('',(0.,-1.,0.));
#16303=DIRECTION('center_axis',(-0.829403493362693,0.,0.558650020314831));
#16304=DIRECTION('ref_axis',(-0.558650020314831,0.,-0.829403493362693));
#16305=DIRECTION('',(0.,-1.,0.));
#16306=DIRECTION('',(-0.558650020314831,0.,-0.829403493362693));
#16307=DIRECTION('center_axis',(0.,-1.,0.));
#16308=DIRECTION('ref_axis',(-0.984807753012208,0.,0.17364817766693));
#16309=DIRECTION('center_axis',(0.,-1.,0.));
#16310=DIRECTION('ref_axis',(1.,0.,0.));
#16311=DIRECTION('center_axis',(0.997609505397066,0.,0.0691033627359897));
#16312=DIRECTION('ref_axis',(-0.0691033627359897,0.,0.997609505397066));
#16313=DIRECTION('',(0.,1.,0.));
#16314=DIRECTION('',(-0.0691033627359897,0.,0.997609505397066));
#16315=DIRECTION('',(0.,-1.,0.));
#16316=DIRECTION('center_axis',(-0.719794432657725,0.,0.694187276399492));
#16317=DIRECTION('ref_axis',(-0.694187276399492,0.,-0.719794432657725));
#16318=DIRECTION('',(0.,-1.,0.));
#16319=DIRECTION('',(-0.694187276399492,0.,-0.719794432657725));
#16320=DIRECTION('center_axis',(0.,-1.,0.));
#16321=DIRECTION('ref_axis',(-0.939692620785908,0.,0.342020143325669));
#16322=DIRECTION('center_axis',(0.,-1.,0.));
#16323=DIRECTION('ref_axis',(1.,0.,0.));
#16324=DIRECTION('center_axis',(0.994453248403466,0.,-0.10517954525379));
#16325=DIRECTION('ref_axis',(0.10517954525379,0.,0.994453248403466));
#16326=DIRECTION('',(0.,1.,0.));
#16327=DIRECTION('',(0.10517954525379,0.,0.994453248403466));
#16328=DIRECTION('',(0.,-1.,0.));
#16329=DIRECTION('center_axis',(-0.58831478235001,0.,0.808632003366464));
#16330=DIRECTION('ref_axis',(-0.808632003366464,0.,-0.58831478235001));
#16331=DIRECTION('',(0.,-1.,0.));
#16332=DIRECTION('',(-0.808632003366464,0.,-0.58831478235001));
#16333=DIRECTION('center_axis',(0.,-1.,0.));
#16334=DIRECTION('ref_axis',(-0.866025403784438,0.,0.5));
#16335=DIRECTION('center_axis',(0.,-1.,0.));
#16336=DIRECTION('ref_axis',(1.,0.,0.));
#16337=DIRECTION('center_axis',(0.961081032674752,0.,-0.276266625984452));
#16338=DIRECTION('ref_axis',(0.276266625984452,0.,0.961081032674752));
#16339=DIRECTION('',(0.,1.,0.));
#16340=DIRECTION('',(0.276266625984452,0.,0.961081032674752));
#16341=DIRECTION('',(0.,-1.,0.));
#16342=DIRECTION('center_axis',(-0.438959485082234,0.,0.898506856098683));
#16343=DIRECTION('ref_axis',(-0.898506856098683,0.,-0.438959485082234));
#16344=DIRECTION('',(0.,-1.,0.));
#16345=DIRECTION('',(-0.898506856098683,0.,-0.438959485082234));
#16346=DIRECTION('center_axis',(0.,-1.,0.));
#16347=DIRECTION('ref_axis',(-0.766044443118978,0.,0.642787609686539));
#16348=DIRECTION('center_axis',(0.,-1.,0.));
#16349=DIRECTION('ref_axis',(1.,0.,0.));
#16350=DIRECTION('center_axis',(0.898506856098683,0.,-0.438959485082234));
#16351=DIRECTION('ref_axis',(0.438959485082234,0.,0.898506856098683));
#16352=DIRECTION('',(0.,1.,0.));
#16353=DIRECTION('',(0.438959485082234,0.,0.898506856098683));
#16354=DIRECTION('',(0.,-1.,0.));
#16355=DIRECTION('center_axis',(-0.276266625984452,0.,0.961081032674752));
#16356=DIRECTION('ref_axis',(-0.961081032674752,0.,-0.276266625984452));
#16357=DIRECTION('',(0.,-1.,0.));
#16358=DIRECTION('',(-0.961081032674752,0.,-0.276266625984452));
#16359=DIRECTION('center_axis',(0.,-1.,0.));
#16360=DIRECTION('ref_axis',(-0.642787609686539,0.,0.766044443118978));
#16361=DIRECTION('center_axis',(0.,-1.,0.));
#16362=DIRECTION('ref_axis',(1.,0.,0.));
#16363=DIRECTION('center_axis',(0.808632003366463,0.,-0.58831478235001));
#16364=DIRECTION('ref_axis',(0.58831478235001,0.,0.808632003366463));
#16365=DIRECTION('',(0.,1.,0.));
#16366=DIRECTION('',(0.58831478235001,0.,0.808632003366463));
#16367=DIRECTION('',(0.,-1.,0.));
#16368=DIRECTION('center_axis',(-0.10517954525379,0.,0.994453248403466));
#16369=DIRECTION('ref_axis',(-0.994453248403466,0.,-0.10517954525379));
#16370=DIRECTION('',(0.,-1.,0.));
#16371=DIRECTION('',(-0.994453248403466,0.,-0.10517954525379));
#16372=DIRECTION('center_axis',(0.,-1.,0.));
#16373=DIRECTION('ref_axis',(-0.5,0.,0.866025403784439));
#16374=DIRECTION('center_axis',(0.,-1.,0.));
#16375=DIRECTION('ref_axis',(1.,0.,0.));
#16376=DIRECTION('center_axis',(0.694187276399491,0.,-0.719794432657725));
#16377=DIRECTION('ref_axis',(0.719794432657725,0.,0.694187276399491));
#16378=DIRECTION('',(0.,1.,0.));
#16379=DIRECTION('',(0.719794432657725,0.,0.694187276399491));
#16380=DIRECTION('',(0.,-1.,0.));
#16381=DIRECTION('center_axis',(0.0691033627359905,0.,0.997609505397066));
#16382=DIRECTION('ref_axis',(-0.997609505397066,0.,0.0691033627359905));
#16383=DIRECTION('',(0.,-1.,0.));
#16384=DIRECTION('',(-0.997609505397066,0.,0.0691033627359905));
#16385=DIRECTION('center_axis',(0.,-1.,0.));
#16386=DIRECTION('ref_axis',(-0.342020143325669,0.,0.939692620785908));
#16387=DIRECTION('center_axis',(0.,-1.,0.));
#16388=DIRECTION('ref_axis',(1.,0.,0.));
#16389=DIRECTION('center_axis',(0.558650020314831,0.,-0.829403493362693));
#16390=DIRECTION('ref_axis',(0.829403493362693,0.,0.558650020314831));
#16391=DIRECTION('',(0.,1.,0.));
#16392=DIRECTION('',(0.829403493362693,0.,0.558650020314831));
#16393=DIRECTION('',(0.,-1.,0.));
#16394=DIRECTION('center_axis',(0.241286600017027,0.,0.970453902383943));
#16395=DIRECTION('ref_axis',(-0.970453902383943,0.,0.241286600017027));
#16396=DIRECTION('',(0.,-1.,0.));
#16397=DIRECTION('',(-0.970453902383943,0.,0.241286600017027));
#16398=DIRECTION('center_axis',(0.,-1.,0.));
#16399=DIRECTION('ref_axis',(-0.17364817766693,0.,0.984807753012208));
#16400=DIRECTION('center_axis',(0.,-1.,0.));
#16401=DIRECTION('ref_axis',(1.,0.,0.));
#16402=DIRECTION('center_axis',(0.406138466053456,0.,-0.913811548620253));
#16403=DIRECTION('ref_axis',(0.913811548620253,0.,0.406138466053456));
#16404=DIRECTION('',(0.,1.,0.));
#16405=DIRECTION('',(0.913811548620253,0.,0.406138466053456));
#16406=DIRECTION('',(0.,-1.,0.));
#16407=DIRECTION('center_axis',(0.406138466053456,0.,0.913811548620253));
#16408=DIRECTION('ref_axis',(-0.913811548620253,0.,0.406138466053456));
#16409=DIRECTION('',(0.,-1.,0.));
#16410=DIRECTION('',(-0.913811548620253,0.,0.406138466053456));
#16411=DIRECTION('center_axis',(0.,-1.,0.));
#16412=DIRECTION('ref_axis',(1.22464679914735E-16,0.,1.));
#16413=DIRECTION('center_axis',(0.,-1.,0.));
#16414=DIRECTION('ref_axis',(1.,0.,0.));
#16415=DIRECTION('center_axis',(0.,-1.,0.));
#16416=DIRECTION('ref_axis',(1.,0.,0.));
#16417=DIRECTION('center_axis',(0.241286600017026,0.,-0.970453902383943));
#16418=DIRECTION('ref_axis',(0.970453902383943,0.,0.241286600017026));
#16419=DIRECTION('',(0.,1.,0.));
#16420=DIRECTION('',(0.970453902383943,0.,0.241286600017026));
#16421=DIRECTION('',(0.,-1.,0.));
#16422=DIRECTION('center_axis',(0.558650020314832,0.,0.829403493362693));
#16423=DIRECTION('ref_axis',(-0.829403493362693,0.,0.558650020314832));
#16424=DIRECTION('',(0.,-1.,0.));
#16425=DIRECTION('',(-0.829403493362692,0.,0.558650020314832));
#16426=DIRECTION('center_axis',(0.,-1.,0.));
#16427=DIRECTION('ref_axis',(0.173648177666931,0.,0.984807753012208));
#16428=DIRECTION('center_axis',(0.,-1.,0.));
#16429=DIRECTION('ref_axis',(1.,0.,0.));
#16430=DIRECTION('center_axis',(0.0691033627359902,0.,-0.997609505397066));
#16431=DIRECTION('ref_axis',(0.997609505397066,0.,0.0691033627359902));
#16432=DIRECTION('',(0.,1.,0.));
#16433=DIRECTION('',(0.997609505397066,0.,0.0691033627359902));
#16434=DIRECTION('',(0.,-1.,0.));
#16435=DIRECTION('center_axis',(0.694187276399491,0.,0.719794432657725));
#16436=DIRECTION('ref_axis',(-0.719794432657725,0.,0.694187276399491));
#16437=DIRECTION('',(0.,-1.,0.));
#16438=DIRECTION('',(-0.719794432657725,0.,0.694187276399491));
#16439=DIRECTION('center_axis',(0.,-1.,0.));
#16440=DIRECTION('ref_axis',(0.342020143325669,0.,0.939692620785908));
#16441=DIRECTION('center_axis',(0.,-1.,0.));
#16442=DIRECTION('ref_axis',(1.,0.,0.));
#16443=DIRECTION('center_axis',(-0.10517954525379,0.,-0.994453248403466));
#16444=DIRECTION('ref_axis',(0.994453248403466,0.,-0.10517954525379));
#16445=DIRECTION('',(0.,1.,0.));
#16446=DIRECTION('',(0.994453248403466,0.,-0.10517954525379));
#16447=DIRECTION('',(0.,-1.,0.));
#16448=DIRECTION('center_axis',(0.808632003366463,0.,0.58831478235001));
#16449=DIRECTION('ref_axis',(-0.58831478235001,0.,0.808632003366463));
#16450=DIRECTION('',(0.,-1.,0.));
#16451=DIRECTION('',(-0.58831478235001,0.,0.808632003366463));
#16452=DIRECTION('center_axis',(0.,-1.,0.));
#16453=DIRECTION('ref_axis',(0.5,0.,0.866025403784439));
#16454=DIRECTION('center_axis',(0.,-1.,0.));
#16455=DIRECTION('ref_axis',(1.,0.,0.));
#16456=DIRECTION('center_axis',(-0.276266625984452,0.,-0.961081032674752));
#16457=DIRECTION('ref_axis',(0.961081032674752,0.,-0.276266625984452));
#16458=DIRECTION('',(0.,1.,0.));
#16459=DIRECTION('',(0.961081032674752,0.,-0.276266625984452));
#16460=DIRECTION('',(0.,-1.,0.));
#16461=DIRECTION('center_axis',(0.898506856098683,0.,0.438959485082234));
#16462=DIRECTION('ref_axis',(-0.438959485082234,0.,0.898506856098683));
#16463=DIRECTION('',(0.,-1.,0.));
#16464=DIRECTION('',(-0.438959485082234,0.,0.898506856098683));
#16465=DIRECTION('center_axis',(0.,-1.,0.));
#16466=DIRECTION('ref_axis',(0.642787609686539,0.,0.766044443118978));
#16467=DIRECTION('center_axis',(0.,-1.,0.));
#16468=DIRECTION('ref_axis',(1.,0.,0.));
#16469=DIRECTION('center_axis',(-0.438959485082234,0.,-0.898506856098683));
#16470=DIRECTION('ref_axis',(0.898506856098683,0.,-0.438959485082234));
#16471=DIRECTION('',(0.,1.,0.));
#16472=DIRECTION('',(0.898506856098683,0.,-0.438959485082234));
#16473=DIRECTION('',(0.,-1.,0.));
#16474=DIRECTION('center_axis',(0.961081032674752,0.,0.276266625984452));
#16475=DIRECTION('ref_axis',(-0.276266625984452,0.,0.961081032674752));
#16476=DIRECTION('',(0.,-1.,0.));
#16477=DIRECTION('',(-0.276266625984452,0.,0.961081032674752));
#16478=DIRECTION('center_axis',(0.,-1.,0.));
#16479=DIRECTION('ref_axis',(0.766044443118978,0.,0.642787609686539));
#16480=DIRECTION('center_axis',(0.,-1.,0.));
#16481=DIRECTION('ref_axis',(1.,0.,0.));
#16482=DIRECTION('center_axis',(-0.58831478235001,0.,-0.808632003366463));
#16483=DIRECTION('ref_axis',(0.808632003366463,0.,-0.58831478235001));
#16484=DIRECTION('',(0.,1.,0.));
#16485=DIRECTION('',(0.808632003366463,0.,-0.58831478235001));
#16486=DIRECTION('',(0.,-1.,0.));
#16487=DIRECTION('center_axis',(0.994453248403466,0.,0.10517954525379));
#16488=DIRECTION('ref_axis',(-0.10517954525379,0.,0.994453248403466));
#16489=DIRECTION('',(0.,-1.,0.));
#16490=DIRECTION('',(-0.10517954525379,0.,0.994453248403466));
#16491=DIRECTION('center_axis',(0.,-1.,0.));
#16492=DIRECTION('ref_axis',(0.866025403784439,0.,0.5));
#16493=DIRECTION('center_axis',(0.,-1.,0.));
#16494=DIRECTION('ref_axis',(1.,0.,0.));
#16495=DIRECTION('center_axis',(-0.719794432657725,0.,-0.694187276399491));
#16496=DIRECTION('ref_axis',(0.694187276399491,0.,-0.719794432657725));
#16497=DIRECTION('',(0.,1.,0.));
#16498=DIRECTION('',(0.694187276399491,0.,-0.719794432657725));
#16499=DIRECTION('',(0.,-1.,0.));
#16500=DIRECTION('center_axis',(0.997609505397066,0.,-0.0691033627359904));
#16501=DIRECTION('ref_axis',(0.0691033627359904,0.,0.997609505397066));
#16502=DIRECTION('',(0.,-1.,0.));
#16503=DIRECTION('',(0.0691033627359904,0.,0.997609505397066));
#16504=DIRECTION('center_axis',(0.,-1.,0.));
#16505=DIRECTION('ref_axis',(0.939692620785908,0.,0.342020143325669));
#16506=DIRECTION('center_axis',(0.,-1.,0.));
#16507=DIRECTION('ref_axis',(1.,0.,0.));
#16508=DIRECTION('center_axis',(-0.829403493362693,0.,-0.558650020314831));
#16509=DIRECTION('ref_axis',(0.558650020314831,0.,-0.829403493362693));
#16510=DIRECTION('',(0.,1.,0.));
#16511=DIRECTION('',(0.558650020314831,0.,-0.829403493362693));
#16512=DIRECTION('',(0.,-1.,0.));
#16513=DIRECTION('center_axis',(0.970453902383943,0.,-0.241286600017027));
#16514=DIRECTION('ref_axis',(0.241286600017027,0.,0.970453902383943));
#16515=DIRECTION('',(0.,-1.,0.));
#16516=DIRECTION('',(0.241286600017026,0.,0.970453902383943));
#16517=DIRECTION('center_axis',(0.,-1.,0.));
#16518=DIRECTION('ref_axis',(0.984807753012208,0.,0.17364817766693));
#16519=DIRECTION('center_axis',(0.,-1.,0.));
#16520=DIRECTION('ref_axis',(1.,0.,0.));
#16521=DIRECTION('center_axis',(-0.913811548620253,0.,-0.406138466053456));
#16522=DIRECTION('ref_axis',(0.406138466053456,0.,-0.913811548620253));
#16523=DIRECTION('',(0.,1.,0.));
#16524=DIRECTION('',(0.406138466053456,0.,-0.913811548620253));
#16525=DIRECTION('',(0.,-1.,0.));
#16526=DIRECTION('center_axis',(0.913811548620253,0.,-0.406138466053456));
#16527=DIRECTION('ref_axis',(0.406138466053456,0.,0.913811548620253));
#16528=DIRECTION('',(0.,-1.,0.));
#16529=DIRECTION('',(0.406138466053456,0.,0.913811548620253));
#16530=DIRECTION('center_axis',(0.,-1.,0.));
#16531=DIRECTION('ref_axis',(1.,0.,-6.12323399573677E-17));
#16532=DIRECTION('center_axis',(0.,-1.,0.));
#16533=DIRECTION('ref_axis',(1.,0.,0.));
#16534=DIRECTION('center_axis',(-0.970453902383943,0.,-0.241286600017026));
#16535=DIRECTION('ref_axis',(0.241286600017026,0.,-0.970453902383943));
#16536=DIRECTION('',(0.,1.,0.));
#16537=DIRECTION('',(0.241286600017026,0.,-0.970453902383943));
#16538=DIRECTION('',(0.,-1.,0.));
#16539=DIRECTION('center_axis',(0.829403493362693,0.,-0.558650020314832));
#16540=DIRECTION('ref_axis',(0.558650020314832,0.,0.829403493362693));
#16541=DIRECTION('',(0.,-1.,0.));
#16542=DIRECTION('',(0.558650020314832,0.,0.829403493362693));
#16543=DIRECTION('center_axis',(0.,-1.,0.));
#16544=DIRECTION('ref_axis',(0.984807753012208,0.,-0.17364817766693));
#16545=DIRECTION('center_axis',(0.,-1.,0.));
#16546=DIRECTION('ref_axis',(1.,0.,0.));
#16547=DIRECTION('center_axis',(-0.997609505397066,0.,-0.0691033627359903));
#16548=DIRECTION('ref_axis',(0.0691033627359903,0.,-0.997609505397066));
#16549=DIRECTION('',(0.,1.,0.));
#16550=DIRECTION('',(0.0691033627359903,0.,-0.997609505397066));
#16551=DIRECTION('',(0.,-1.,0.));
#16552=DIRECTION('center_axis',(0.719794432657725,0.,-0.694187276399491));
#16553=DIRECTION('ref_axis',(0.694187276399491,0.,0.719794432657725));
#16554=DIRECTION('',(0.,-1.,0.));
#16555=DIRECTION('',(0.694187276399491,0.,0.719794432657725));
#16556=DIRECTION('center_axis',(0.,-1.,0.));
#16557=DIRECTION('ref_axis',(0.939692620785908,0.,-0.342020143325669));
#16558=DIRECTION('center_axis',(0.,-1.,0.));
#16559=DIRECTION('ref_axis',(1.,0.,0.));
#16560=DIRECTION('center_axis',(-0.994453248403466,0.,0.10517954525379));
#16561=DIRECTION('ref_axis',(-0.10517954525379,0.,-0.994453248403466));
#16562=DIRECTION('',(0.,1.,0.));
#16563=DIRECTION('',(-0.10517954525379,0.,-0.994453248403466));
#16564=DIRECTION('',(0.,-1.,0.));
#16565=DIRECTION('center_axis',(0.58831478235001,0.,-0.808632003366464));
#16566=DIRECTION('ref_axis',(0.808632003366464,0.,0.58831478235001));
#16567=DIRECTION('',(0.,-1.,0.));
#16568=DIRECTION('',(0.808632003366464,0.,0.58831478235001));
#16569=DIRECTION('center_axis',(0.,-1.,0.));
#16570=DIRECTION('ref_axis',(0.866025403784439,0.,-0.5));
#16571=DIRECTION('center_axis',(0.,-1.,0.));
#16572=DIRECTION('ref_axis',(1.,0.,0.));
#16573=DIRECTION('center_axis',(-0.961081032674752,0.,0.276266625984452));
#16574=DIRECTION('ref_axis',(-0.276266625984452,0.,-0.961081032674752));
#16575=DIRECTION('',(0.,1.,0.));
#16576=DIRECTION('',(-0.276266625984452,0.,-0.961081032674752));
#16577=DIRECTION('',(0.,-1.,0.));
#16578=DIRECTION('center_axis',(0.438959485082234,0.,-0.898506856098683));
#16579=DIRECTION('ref_axis',(0.898506856098683,0.,0.438959485082234));
#16580=DIRECTION('',(0.,-1.,0.));
#16581=DIRECTION('',(0.898506856098683,0.,0.438959485082234));
#16582=DIRECTION('center_axis',(0.,-1.,0.));
#16583=DIRECTION('ref_axis',(0.766044443118978,0.,-0.642787609686539));
#16584=DIRECTION('center_axis',(0.,-1.,0.));
#16585=DIRECTION('ref_axis',(1.,0.,0.));
#16586=DIRECTION('center_axis',(-0.898506856098683,0.,0.438959485082234));
#16587=DIRECTION('ref_axis',(-0.438959485082234,0.,-0.898506856098683));
#16588=DIRECTION('',(0.,1.,0.));
#16589=DIRECTION('',(-0.438959485082234,0.,-0.898506856098683));
#16590=DIRECTION('',(0.,-1.,0.));
#16591=DIRECTION('center_axis',(0.276266625984452,0.,-0.961081032674752));
#16592=DIRECTION('ref_axis',(0.961081032674752,0.,0.276266625984452));
#16593=DIRECTION('',(0.,-1.,0.));
#16594=DIRECTION('',(0.961081032674752,0.,0.276266625984452));
#16595=DIRECTION('center_axis',(0.,-1.,0.));
#16596=DIRECTION('ref_axis',(0.642787609686539,0.,-0.766044443118978));
#16597=DIRECTION('center_axis',(0.,-1.,0.));
#16598=DIRECTION('ref_axis',(1.,0.,0.));
#16599=DIRECTION('center_axis',(-0.808632003366463,0.,0.58831478235001));
#16600=DIRECTION('ref_axis',(-0.58831478235001,0.,-0.808632003366463));
#16601=DIRECTION('',(0.,1.,0.));
#16602=DIRECTION('',(-0.58831478235001,0.,-0.808632003366463));
#16603=DIRECTION('',(0.,-1.,0.));
#16604=DIRECTION('center_axis',(0.10517954525379,0.,-0.994453248403466));
#16605=DIRECTION('ref_axis',(0.994453248403466,0.,0.10517954525379));
#16606=DIRECTION('',(0.,-1.,0.));
#16607=DIRECTION('',(0.994453248403466,0.,0.10517954525379));
#16608=DIRECTION('center_axis',(0.,-1.,0.));
#16609=DIRECTION('ref_axis',(0.5,0.,-0.866025403784439));
#16610=DIRECTION('center_axis',(0.,-1.,0.));
#16611=DIRECTION('ref_axis',(1.,0.,0.));
#16612=DIRECTION('center_axis',(-0.694187276399491,0.,0.719794432657725));
#16613=DIRECTION('ref_axis',(-0.719794432657725,0.,-0.694187276399491));
#16614=DIRECTION('',(0.,1.,0.));
#16615=DIRECTION('',(-0.719794432657725,0.,-0.694187276399491));
#16616=DIRECTION('',(0.,-1.,0.));
#16617=DIRECTION('center_axis',(-0.0691033627359904,0.,-0.997609505397066));
#16618=DIRECTION('ref_axis',(0.997609505397066,0.,-0.0691033627359904));
#16619=DIRECTION('',(0.,-1.,0.));
#16620=DIRECTION('',(0.997609505397066,0.,-0.0691033627359904));
#16621=DIRECTION('center_axis',(0.,-1.,0.));
#16622=DIRECTION('ref_axis',(0.342020143325669,0.,-0.939692620785908));
#16623=DIRECTION('center_axis',(0.,-1.,0.));
#16624=DIRECTION('ref_axis',(1.,0.,0.));
#16625=DIRECTION('center_axis',(-0.558650020314831,0.,0.829403493362693));
#16626=DIRECTION('ref_axis',(-0.829403493362693,0.,-0.558650020314831));
#16627=DIRECTION('',(0.,1.,0.));
#16628=DIRECTION('',(-0.829403493362693,0.,-0.558650020314831));
#16629=DIRECTION('',(0.,-1.,0.));
#16630=DIRECTION('center_axis',(-0.241286600017026,0.,-0.970453902383943));
#16631=DIRECTION('ref_axis',(0.970453902383943,0.,-0.241286600017026));
#16632=DIRECTION('',(0.,-1.,0.));
#16633=DIRECTION('',(0.970453902383943,0.,-0.241286600017026));
#16634=DIRECTION('center_axis',(0.,-1.,0.));
#16635=DIRECTION('ref_axis',(0.17364817766693,0.,-0.984807753012208));
#16636=DIRECTION('center_axis',(0.,-1.,0.));
#16637=DIRECTION('ref_axis',(1.,0.,0.));
#16638=DIRECTION('center_axis',(-0.406138466053456,0.,0.913811548620253));
#16639=DIRECTION('ref_axis',(-0.913811548620253,0.,-0.406138466053456));
#16640=DIRECTION('',(0.,1.,0.));
#16641=DIRECTION('',(-0.913811548620253,0.,-0.406138466053456));
#16642=DIRECTION('',(0.,-1.,0.));
#16643=DIRECTION('center_axis',(-0.406138466053456,0.,-0.913811548620253));
#16644=DIRECTION('ref_axis',(0.913811548620253,0.,-0.406138466053456));
#16645=DIRECTION('',(0.,-1.,0.));
#16646=DIRECTION('',(0.913811548620253,0.,-0.406138466053456));
#16647=DIRECTION('center_axis',(0.,-1.,0.));
#16648=DIRECTION('ref_axis',(0.,0.,-1.));
#16649=DIRECTION('center_axis',(0.,-1.,0.));
#16650=DIRECTION('ref_axis',(1.,0.,0.));
#16651=DIRECTION('center_axis',(0.,1.,0.));
#16652=DIRECTION('ref_axis',(1.,0.,0.));
#16653=DIRECTION('',(0.,-1.,0.));
#16654=DIRECTION('center_axis',(0.,1.,0.));
#16655=DIRECTION('ref_axis',(1.,0.,0.));
#16656=DIRECTION('',(0.499999999999998,0.,-0.86602540378444));
#16657=DIRECTION('',(1.,0.,0.));
#16658=DIRECTION('',(0.499999999999998,0.,0.86602540378444));
#16659=DIRECTION('',(-0.499999999999998,0.,0.86602540378444));
#16660=DIRECTION('',(-1.,0.,0.));
#16661=DIRECTION('',(-0.499999999999998,0.,-0.86602540378444));
#16662=DIRECTION('center_axis',(0.,1.,0.));
#16663=DIRECTION('ref_axis',(0.,0.,1.));
#16664=DIRECTION('',(0.499999999999998,0.,-0.86602540378444));
#16665=DIRECTION('center_axis',(0.,-1.,0.));
#16666=DIRECTION('ref_axis',(1.,0.,0.));
#16667=DIRECTION('center_axis',(0.,1.,0.));
#16668=DIRECTION('ref_axis',(0.,0.,1.));
#16669=DIRECTION('',(1.,0.,0.));
#16670=DIRECTION('center_axis',(0.,-1.,0.));
#16671=DIRECTION('ref_axis',(1.,0.,0.));
#16672=DIRECTION('center_axis',(0.,1.,0.));
#16673=DIRECTION('ref_axis',(0.,0.,1.));
#16674=DIRECTION('',(0.499999999999998,0.,0.86602540378444));
#16675=DIRECTION('center_axis',(0.,-1.,0.));
#16676=DIRECTION('ref_axis',(1.,0.,0.));
#16677=DIRECTION('center_axis',(0.,1.,0.));
#16678=DIRECTION('ref_axis',(0.,0.,1.));
#16679=DIRECTION('',(-0.499999999999998,0.,0.86602540378444));
#16680=DIRECTION('center_axis',(0.,-1.,0.));
#16681=DIRECTION('ref_axis',(1.,0.,0.));
#16682=DIRECTION('center_axis',(0.,1.,0.));
#16683=DIRECTION('ref_axis',(0.,0.,1.));
#16684=DIRECTION('',(-1.,0.,0.));
#16685=DIRECTION('center_axis',(0.,-1.,0.));
#16686=DIRECTION('ref_axis',(1.,0.,0.));
#16687=DIRECTION('center_axis',(0.,1.,0.));
#16688=DIRECTION('ref_axis',(0.,0.,1.));
#16689=DIRECTION('',(-0.499999999999998,0.,-0.86602540378444));
#16690=DIRECTION('center_axis',(0.,-1.,0.));
#16691=DIRECTION('ref_axis',(1.,0.,0.));
#16692=DIRECTION('center_axis',(0.,1.,0.));
#16693=DIRECTION('ref_axis',(1.,0.,0.));
#16694=DIRECTION('',(-0.85716730070211,0.515038074910058,1.04972719113862E-16));
#16695=DIRECTION('center_axis',(-0.86602540378444,0.,-0.499999999999998));
#16696=DIRECTION('ref_axis',(0.499999999999998,0.,-0.86602540378444));
#16697=DIRECTION('',(0.,-1.,0.));
#16698=DIRECTION('',(0.,-1.,0.));
#16699=DIRECTION('center_axis',(-0.86602540378444,0.,0.499999999999998));
#16700=DIRECTION('ref_axis',(-0.499999999999998,0.,-0.86602540378444));
#16701=DIRECTION('',(0.,-1.,0.));
#16702=DIRECTION('center_axis',(0.,0.,1.));
#16703=DIRECTION('ref_axis',(-1.,0.,0.));
#16704=DIRECTION('',(0.,-1.,0.));
#16705=DIRECTION('center_axis',(0.86602540378444,0.,0.499999999999998));
#16706=DIRECTION('ref_axis',(-0.499999999999998,0.,0.86602540378444));
#16707=DIRECTION('',(0.,-1.,0.));
#16708=DIRECTION('center_axis',(0.86602540378444,0.,-0.499999999999998));
#16709=DIRECTION('ref_axis',(0.499999999999998,0.,0.86602540378444));
#16710=DIRECTION('',(0.,-1.,0.));
#16711=DIRECTION('center_axis',(0.,0.,-1.));
#16712=DIRECTION('ref_axis',(1.,0.,0.));
#16713=DIRECTION('axis',(0.,0.,1.));
#16714=DIRECTION('refdir',(1.,0.,0.));
#16715=DIRECTION('center_axis',(0.,1.,0.));
#16716=DIRECTION('ref_axis',(0.314077325660087,0.,0.949397405466335));
#16717=DIRECTION('',(0.,-1.,0.));
#16718=DIRECTION('center_axis',(0.,-1.,0.));
#16719=DIRECTION('ref_axis',(1.,0.,9.89867765446222E-14));
#16720=DIRECTION('center_axis',(0.,1.,0.));
#16721=DIRECTION('ref_axis',(0.314077325660087,0.,0.949397405466335));
#16722=DIRECTION('',(0.,-1.,0.));
#16723=DIRECTION('center_axis',(0.,1.,0.));
#16724=DIRECTION('ref_axis',(0.314077325660087,0.,0.949397405466335));
#16725=DIRECTION('',(0.,-1.,0.));
#16726=DIRECTION('center_axis',(0.,1.,0.));
#16727=DIRECTION('ref_axis',(0.314077325660087,0.,0.949397405466335));
#16728=DIRECTION('',(0.,-1.,0.));
#16729=DIRECTION('center_axis',(0.,1.,0.));
#16730=DIRECTION('ref_axis',(0.314077325660087,0.,0.949397405466335));
#16731=DIRECTION('',(0.,-1.,0.));
#16732=DIRECTION('center_axis',(0.,1.,0.));
#16733=DIRECTION('ref_axis',(0.314077325660087,0.,0.949397405466335));
#16734=DIRECTION('',(0.,-1.,0.));
#16735=DIRECTION('center_axis',(0.,1.,0.));
#16736=DIRECTION('ref_axis',(0.314077325660087,0.,0.949397405466335));
#16737=DIRECTION('',(0.,-1.,0.));
#16738=DIRECTION('center_axis',(0.,1.,0.));
#16739=DIRECTION('ref_axis',(0.314077325660087,0.,0.949397405466335));
#16740=DIRECTION('',(0.,-1.,0.));
#16741=DIRECTION('center_axis',(0.,1.,0.));
#16742=DIRECTION('ref_axis',(0.314077325660087,0.,0.949397405466335));
#16743=DIRECTION('',(0.,-1.,0.));
#16744=DIRECTION('center_axis',(0.,1.,0.));
#16745=DIRECTION('ref_axis',(0.314077325660087,0.,0.949397405466335));
#16746=DIRECTION('',(0.,-1.,0.));
#16747=DIRECTION('center_axis',(0.,1.,0.));
#16748=DIRECTION('ref_axis',(0.314077325660087,0.,0.949397405466335));
#16749=DIRECTION('',(0.,-1.,0.));
#16750=DIRECTION('center_axis',(0.,1.,0.));
#16751=DIRECTION('ref_axis',(0.314077325660087,0.,0.949397405466335));
#16752=DIRECTION('',(0.,-1.,0.));
#16753=DIRECTION('center_axis',(0.,1.,0.));
#16754=DIRECTION('ref_axis',(0.314077325660087,0.,0.949397405466335));
#16755=DIRECTION('',(0.,-1.,0.));
#16756=DIRECTION('center_axis',(0.,1.,0.));
#16757=DIRECTION('ref_axis',(0.314077325660087,0.,0.949397405466335));
#16758=DIRECTION('',(0.,-1.,0.));
#16759=DIRECTION('center_axis',(0.,1.,0.));
#16760=DIRECTION('ref_axis',(0.314077325660087,0.,0.949397405466335));
#16761=DIRECTION('',(0.,-1.,0.));
#16762=DIRECTION('center_axis',(0.,1.,0.));
#16763=DIRECTION('ref_axis',(0.314077325660087,0.,0.949397405466335));
#16764=DIRECTION('',(0.,-1.,0.));
#16765=DIRECTION('center_axis',(0.,1.,0.));
#16766=DIRECTION('ref_axis',(0.314077325660087,0.,0.949397405466335));
#16767=DIRECTION('',(0.,-1.,0.));
#16768=DIRECTION('center_axis',(0.,1.,0.));
#16769=DIRECTION('ref_axis',(0.314077325660087,0.,0.949397405466335));
#16770=DIRECTION('',(0.,-1.,0.));
#16771=DIRECTION('center_axis',(0.,1.,0.));
#16772=DIRECTION('ref_axis',(0.314077325660087,0.,0.949397405466335));
#16773=DIRECTION('',(0.,-1.,0.));
#16774=DIRECTION('center_axis',(0.,1.,0.));
#16775=DIRECTION('ref_axis',(0.314077325660087,0.,0.949397405466335));
#16776=DIRECTION('',(0.,-1.,0.));
#16777=DIRECTION('center_axis',(0.,1.,0.));
#16778=DIRECTION('ref_axis',(0.314077325660087,0.,0.949397405466335));
#16779=DIRECTION('',(0.,-1.,0.));
#16780=DIRECTION('center_axis',(0.,1.,0.));
#16781=DIRECTION('ref_axis',(0.314077325660087,0.,0.949397405466335));
#16782=DIRECTION('',(0.,-1.,0.));
#16783=DIRECTION('center_axis',(0.,1.,0.));
#16784=DIRECTION('ref_axis',(0.314077325660087,0.,0.949397405466335));
#16785=DIRECTION('',(0.,-1.,0.));
#16786=DIRECTION('center_axis',(0.,1.,0.));
#16787=DIRECTION('ref_axis',(0.314077325660087,0.,0.949397405466335));
#16788=DIRECTION('',(0.,-1.,0.));
#16789=DIRECTION('center_axis',(0.,1.,0.));
#16790=DIRECTION('ref_axis',(0.314077325660087,0.,0.949397405466335));
#16791=DIRECTION('',(0.,-1.,0.));
#16792=DIRECTION('center_axis',(0.,1.,0.));
#16793=DIRECTION('ref_axis',(0.314077325660087,0.,0.949397405466335));
#16794=DIRECTION('',(0.,-1.,0.));
#16795=DIRECTION('center_axis',(0.,1.,0.));
#16796=DIRECTION('ref_axis',(0.314077325660087,0.,0.949397405466335));
#16797=DIRECTION('',(0.,-1.,0.));
#16798=DIRECTION('center_axis',(0.,1.,0.));
#16799=DIRECTION('ref_axis',(1.,0.,0.));
#16800=DIRECTION('center_axis',(0.,-1.,0.));
#16801=DIRECTION('ref_axis',(1.,0.,0.));
#16802=DIRECTION('center_axis',(0.,1.,0.));
#16803=DIRECTION('ref_axis',(1.,0.,0.));
#16804=DIRECTION('center_axis',(0.,1.,0.));
#16805=DIRECTION('ref_axis',(1.,0.,0.));
#16806=DIRECTION('center_axis',(0.,1.,0.));
#16807=DIRECTION('ref_axis',(0.314077325660087,0.,0.949397405466335));
#16808=DIRECTION('center_axis',(0.,1.,0.));
#16809=DIRECTION('ref_axis',(1.,0.,9.89867765446222E-14));
#16810=DIRECTION('center_axis',(0.,1.,0.));
#16811=DIRECTION('ref_axis',(0.,0.,1.));
#16812=DIRECTION('center_axis',(0.,1.,0.));
#16813=DIRECTION('ref_axis',(1.,0.,0.));
#16814=DIRECTION('center_axis',(0.,1.,0.));
#16815=DIRECTION('ref_axis',(0.,0.,1.));
#16816=DIRECTION('center_axis',(0.,-1.,0.));
#16817=DIRECTION('ref_axis',(1.,0.,0.));
#16818=DIRECTION('center_axis',(0.,-1.,0.));
#16819=DIRECTION('ref_axis',(1.,0.,0.));
#16820=DIRECTION('center_axis',(0.,-1.,0.));
#16821=DIRECTION('ref_axis',(0.,0.,-1.));
#16822=DIRECTION('center_axis',(0.,1.,0.));
#16823=DIRECTION('ref_axis',(1.,0.,0.));
#16824=DIRECTION('center_axis',(1.,0.,0.));
#16825=DIRECTION('ref_axis',(0.,0.,1.));
#16826=DIRECTION('center_axis',(0.,1.,0.));
#16827=DIRECTION('ref_axis',(1.,0.,0.));
#16828=DIRECTION('center_axis',(0.,1.,0.));
#16829=DIRECTION('ref_axis',(1.,0.,0.));
#16830=DIRECTION('center_axis',(0.,-1.,0.));
#16831=DIRECTION('ref_axis',(1.,0.,0.));
#16832=DIRECTION('',(0.707106781186547,0.707106781186548,8.65956056235493E-17));
#16833=DIRECTION('center_axis',(0.,-1.,0.));
#16834=DIRECTION('ref_axis',(1.,0.,0.));
#16835=DIRECTION('center_axis',(0.,1.,0.));
#16836=DIRECTION('ref_axis',(1.,0.,0.));
#16837=DIRECTION('center_axis',(-0.241286600017026,0.,-0.970453902383943));
#16838=DIRECTION('ref_axis',(-0.970453902383943,0.,0.241286600017026));
#16839=DIRECTION('',(0.,-1.,0.));
#16840=DIRECTION('',(-0.970453902383943,0.,0.241286600017026));
#16841=DIRECTION('',(0.,1.,0.));
#16842=DIRECTION('center_axis',(-0.558650020314825,0.,0.829403493362697));
#16843=DIRECTION('ref_axis',(0.829403493362697,0.,0.558650020314825));
#16844=DIRECTION('',(0.829403493362697,0.,0.558650020314825));
#16845=DIRECTION('',(0.,1.,0.));
#16846=DIRECTION('center_axis',(0.,1.,0.));
#16847=DIRECTION('ref_axis',(-0.17364817766693,0.,0.984807753012208));
#16848=DIRECTION('center_axis',(0.,1.,0.));
#16849=DIRECTION('ref_axis',(1.,0.,0.));
#16850=DIRECTION('center_axis',(0.,1.,0.));
#16851=DIRECTION('ref_axis',(1.,0.,0.));
#16852=DIRECTION('center_axis',(0.,-1.,0.));
#16853=DIRECTION('ref_axis',(1.,0.,0.));
#16854=DIRECTION('center_axis',(0.,-1.,0.));
#16855=DIRECTION('ref_axis',(1.,0.,0.));
#16856=DIRECTION('center_axis',(0.,-1.,0.));
#16857=DIRECTION('ref_axis',(1.,0.,0.));
#16858=DIRECTION('center_axis',(0.,-1.,0.));
#16859=DIRECTION('ref_axis',(1.,0.,0.));
#16860=DIRECTION('center_axis',(0.,-1.,0.));
#16861=DIRECTION('ref_axis',(1.,0.,0.));
#16862=DIRECTION('center_axis',(0.,-1.,0.));
#16863=DIRECTION('ref_axis',(1.,0.,0.));
#16864=DIRECTION('center_axis',(0.,-1.,0.));
#16865=DIRECTION('ref_axis',(1.,0.,0.));
#16866=DIRECTION('center_axis',(0.,-1.,0.));
#16867=DIRECTION('ref_axis',(1.,0.,0.));
#16868=DIRECTION('center_axis',(0.,-1.,0.));
#16869=DIRECTION('ref_axis',(1.,0.,0.));
#16870=DIRECTION('center_axis',(0.,-1.,0.));
#16871=DIRECTION('ref_axis',(1.,0.,0.));
#16872=DIRECTION('center_axis',(0.,-1.,0.));
#16873=DIRECTION('ref_axis',(1.,0.,0.));
#16874=DIRECTION('center_axis',(0.,-1.,0.));
#16875=DIRECTION('ref_axis',(1.,0.,0.));
#16876=DIRECTION('center_axis',(0.,-1.,0.));
#16877=DIRECTION('ref_axis',(1.,0.,0.));
#16878=DIRECTION('center_axis',(0.,-1.,0.));
#16879=DIRECTION('ref_axis',(1.,0.,0.));
#16880=DIRECTION('center_axis',(0.,-1.,0.));
#16881=DIRECTION('ref_axis',(1.,0.,0.));
#16882=DIRECTION('center_axis',(0.,-1.,0.));
#16883=DIRECTION('ref_axis',(1.,0.,0.));
#16884=DIRECTION('center_axis',(0.,-1.,0.));
#16885=DIRECTION('ref_axis',(1.,0.,0.));
#16886=DIRECTION('center_axis',(0.,-1.,0.));
#16887=DIRECTION('ref_axis',(1.,0.,0.));
#16888=DIRECTION('center_axis',(0.,-1.,0.));
#16889=DIRECTION('ref_axis',(1.,0.,0.));
#16890=DIRECTION('center_axis',(0.,-1.,0.));
#16891=DIRECTION('ref_axis',(1.,0.,0.));
#16892=DIRECTION('center_axis',(0.,-1.,0.));
#16893=DIRECTION('ref_axis',(1.,0.,0.));
#16894=DIRECTION('center_axis',(0.,-1.,0.));
#16895=DIRECTION('ref_axis',(1.,0.,0.));
#16896=DIRECTION('center_axis',(0.,-1.,0.));
#16897=DIRECTION('ref_axis',(1.,0.,0.));
#16898=DIRECTION('center_axis',(0.,-1.,0.));
#16899=DIRECTION('ref_axis',(1.,0.,0.));
#16900=DIRECTION('center_axis',(0.,-1.,0.));
#16901=DIRECTION('ref_axis',(1.,0.,0.));
#16902=DIRECTION('center_axis',(0.,-1.,0.));
#16903=DIRECTION('ref_axis',(1.,0.,0.));
#16904=DIRECTION('center_axis',(0.,-1.,0.));
#16905=DIRECTION('ref_axis',(1.,0.,0.));
#16906=DIRECTION('center_axis',(0.,-1.,0.));
#16907=DIRECTION('ref_axis',(1.,0.,0.));
#16908=DIRECTION('center_axis',(0.,-1.,0.));
#16909=DIRECTION('ref_axis',(1.,0.,0.));
#16910=DIRECTION('center_axis',(0.,-1.,0.));
#16911=DIRECTION('ref_axis',(1.,0.,0.));
#16912=DIRECTION('center_axis',(0.,-1.,0.));
#16913=DIRECTION('ref_axis',(1.,0.,0.));
#16914=DIRECTION('center_axis',(0.,-1.,0.));
#16915=DIRECTION('ref_axis',(1.,0.,0.));
#16916=DIRECTION('center_axis',(0.,-1.,0.));
#16917=DIRECTION('ref_axis',(1.,0.,0.));
#16918=DIRECTION('center_axis',(0.,-1.,0.));
#16919=DIRECTION('ref_axis',(1.,0.,0.));
#16920=DIRECTION('center_axis',(0.,-1.,0.));
#16921=DIRECTION('ref_axis',(1.,0.,0.));
#16922=DIRECTION('center_axis',(0.,-1.,0.));
#16923=DIRECTION('ref_axis',(1.,0.,0.));
#16924=DIRECTION('',(0.707106781186547,-0.707106781186548,-8.65956056235493E-17));
#16925=DIRECTION('center_axis',(0.,1.,0.));
#16926=DIRECTION('ref_axis',(1.,0.,0.));
#16927=DIRECTION('center_axis',(0.,1.,0.));
#16928=DIRECTION('ref_axis',(-0.342020143325669,0.,0.939692620785908));
#16929=DIRECTION('center_axis',(0.,1.,0.));
#16930=DIRECTION('ref_axis',(1.,0.,0.));
#16931=DIRECTION('',(0.71979443265773,0.,0.694187276399486));
#16932=DIRECTION('',(-0.997609505397066,0.,0.0691033627359896));
#16933=DIRECTION('center_axis',(-0.0691033627359896,0.,-0.997609505397066));
#16934=DIRECTION('ref_axis',(-0.997609505397066,0.,0.0691033627359896));
#16935=DIRECTION('',(0.,-1.,0.));
#16936=DIRECTION('',(0.,1.,0.));
#16937=DIRECTION('center_axis',(-0.694187276399486,0.,0.71979443265773));
#16938=DIRECTION('ref_axis',(0.71979443265773,0.,0.694187276399486));
#16939=DIRECTION('',(0.,1.,0.));
#16940=DIRECTION('center_axis',(0.,-1.,0.));
#16941=DIRECTION('ref_axis',(1.,0.,0.));
#16942=DIRECTION('center_axis',(0.,1.,0.));
#16943=DIRECTION('ref_axis',(1.,0.,0.));
#16944=DIRECTION('',(0.,1.,0.));
#16945=DIRECTION('center_axis',(0.,1.,0.));
#16946=DIRECTION('ref_axis',(1.,0.,0.));
#16947=DIRECTION('',(0.,-1.,0.));
#16948=DIRECTION('',(0.,1.,0.));
#16949=DIRECTION('center_axis',(0.,1.,0.));
#16950=DIRECTION('ref_axis',(1.,0.,0.));
#16951=DIRECTION('',(0.,-1.,0.));
#16952=DIRECTION('',(0.,1.,0.));
#16953=DIRECTION('center_axis',(0.,1.,0.));
#16954=DIRECTION('ref_axis',(1.,0.,0.));
#16955=DIRECTION('',(0.,-1.,0.));
#16956=DIRECTION('',(0.,1.,0.));
#16957=DIRECTION('center_axis',(0.,1.,0.));
#16958=DIRECTION('ref_axis',(1.,0.,0.));
#16959=DIRECTION('',(0.,-1.,0.));
#16960=DIRECTION('',(0.,1.,0.));
#16961=DIRECTION('center_axis',(0.,1.,0.));
#16962=DIRECTION('ref_axis',(1.,0.,0.));
#16963=DIRECTION('',(0.,-1.,0.));
#16964=DIRECTION('',(0.,1.,0.));
#16965=DIRECTION('center_axis',(0.,1.,0.));
#16966=DIRECTION('ref_axis',(1.,0.,0.));
#16967=DIRECTION('',(0.,-1.,0.));
#16968=DIRECTION('',(0.,1.,0.));
#16969=DIRECTION('center_axis',(0.,1.,0.));
#16970=DIRECTION('ref_axis',(1.,0.,0.));
#16971=DIRECTION('',(0.,-1.,0.));
#16972=DIRECTION('',(0.,1.,0.));
#16973=DIRECTION('center_axis',(0.,1.,0.));
#16974=DIRECTION('ref_axis',(1.,0.,0.));
#16975=DIRECTION('',(0.,-1.,0.));
#16976=DIRECTION('',(0.,1.,0.));
#16977=DIRECTION('center_axis',(0.,1.,0.));
#16978=DIRECTION('ref_axis',(1.,0.,0.));
#16979=DIRECTION('',(0.,-1.,0.));
#16980=DIRECTION('',(0.,1.,0.));
#16981=DIRECTION('center_axis',(0.,1.,0.));
#16982=DIRECTION('ref_axis',(1.,0.,0.));
#16983=DIRECTION('',(0.,-1.,0.));
#16984=DIRECTION('',(0.,1.,0.));
#16985=DIRECTION('center_axis',(0.,1.,0.));
#16986=DIRECTION('ref_axis',(1.,0.,0.));
#16987=DIRECTION('',(0.,-1.,0.));
#16988=DIRECTION('',(0.,1.,0.));
#16989=DIRECTION('center_axis',(0.,1.,0.));
#16990=DIRECTION('ref_axis',(1.,0.,0.));
#16991=DIRECTION('',(0.,-1.,0.));
#16992=DIRECTION('',(0.,1.,0.));
#16993=DIRECTION('center_axis',(0.,1.,0.));
#16994=DIRECTION('ref_axis',(1.,0.,0.));
#16995=DIRECTION('',(0.,-1.,0.));
#16996=DIRECTION('',(0.,1.,0.));
#16997=DIRECTION('center_axis',(0.,1.,0.));
#16998=DIRECTION('ref_axis',(1.,0.,0.));
#16999=DIRECTION('',(0.,-1.,0.));
#17000=DIRECTION('',(0.,1.,0.));
#17001=DIRECTION('center_axis',(0.,1.,0.));
#17002=DIRECTION('ref_axis',(1.,0.,0.));
#17003=DIRECTION('',(0.,-1.,0.));
#17004=DIRECTION('',(0.,1.,0.));
#17005=DIRECTION('center_axis',(0.,1.,0.));
#17006=DIRECTION('ref_axis',(1.,0.,0.));
#17007=DIRECTION('',(0.,-1.,0.));
#17008=DIRECTION('',(0.,1.,0.));
#17009=DIRECTION('center_axis',(0.,1.,0.));
#17010=DIRECTION('ref_axis',(1.,0.,0.));
#17011=DIRECTION('',(0.,-1.,0.));
#17012=DIRECTION('',(0.,1.,0.));
#17013=DIRECTION('center_axis',(0.,1.,0.));
#17014=DIRECTION('ref_axis',(1.,0.,0.));
#17015=DIRECTION('',(0.,-1.,0.));
#17016=DIRECTION('',(0.,1.,0.));
#17017=DIRECTION('center_axis',(0.,1.,0.));
#17018=DIRECTION('ref_axis',(1.,0.,0.));
#17019=DIRECTION('',(0.,-1.,0.));
#17020=DIRECTION('',(0.,1.,0.));
#17021=DIRECTION('center_axis',(0.,1.,0.));
#17022=DIRECTION('ref_axis',(1.,0.,0.));
#17023=DIRECTION('',(0.,-1.,0.));
#17024=DIRECTION('',(0.,1.,0.));
#17025=DIRECTION('center_axis',(0.,1.,0.));
#17026=DIRECTION('ref_axis',(1.,0.,0.));
#17027=DIRECTION('',(0.,-1.,0.));
#17028=DIRECTION('',(0.,1.,0.));
#17029=DIRECTION('center_axis',(0.,1.,0.));
#17030=DIRECTION('ref_axis',(1.,0.,0.));
#17031=DIRECTION('',(0.,-1.,0.));
#17032=DIRECTION('',(0.,1.,0.));
#17033=DIRECTION('center_axis',(0.,1.,0.));
#17034=DIRECTION('ref_axis',(1.,0.,0.));
#17035=DIRECTION('',(0.,-1.,0.));
#17036=DIRECTION('',(0.,1.,0.));
#17037=DIRECTION('center_axis',(0.,1.,0.));
#17038=DIRECTION('ref_axis',(1.,0.,0.));
#17039=DIRECTION('',(0.,-1.,0.));
#17040=DIRECTION('',(0.,1.,0.));
#17041=DIRECTION('center_axis',(0.,1.,0.));
#17042=DIRECTION('ref_axis',(1.,0.,0.));
#17043=DIRECTION('',(0.,-1.,0.));
#17044=DIRECTION('',(0.,1.,0.));
#17045=DIRECTION('center_axis',(0.,1.,0.));
#17046=DIRECTION('ref_axis',(1.,0.,0.));
#17047=DIRECTION('',(0.,-1.,0.));
#17048=DIRECTION('',(0.,1.,0.));
#17049=DIRECTION('center_axis',(0.,1.,0.));
#17050=DIRECTION('ref_axis',(1.,0.,0.));
#17051=DIRECTION('',(0.,-1.,0.));
#17052=DIRECTION('',(0.,1.,0.));
#17053=DIRECTION('center_axis',(0.,1.,0.));
#17054=DIRECTION('ref_axis',(1.,0.,0.));
#17055=DIRECTION('',(0.,-1.,0.));
#17056=DIRECTION('',(0.,1.,0.));
#17057=DIRECTION('center_axis',(0.,1.,0.));
#17058=DIRECTION('ref_axis',(1.,0.,0.));
#17059=DIRECTION('',(0.,-1.,0.));
#17060=DIRECTION('',(0.,1.,0.));
#17061=DIRECTION('center_axis',(0.,1.,0.));
#17062=DIRECTION('ref_axis',(1.,0.,0.));
#17063=DIRECTION('',(0.,-1.,0.));
#17064=DIRECTION('',(0.,1.,0.));
#17065=DIRECTION('center_axis',(0.,1.,0.));
#17066=DIRECTION('ref_axis',(1.,0.,0.));
#17067=DIRECTION('',(0.,-1.,0.));
#17068=DIRECTION('',(0.,1.,0.));
#17069=DIRECTION('center_axis',(0.,1.,0.));
#17070=DIRECTION('ref_axis',(1.,0.,0.));
#17071=DIRECTION('',(0.,-1.,0.));
#17072=DIRECTION('',(0.,1.,0.));
#17073=DIRECTION('center_axis',(0.,1.,0.));
#17074=DIRECTION('ref_axis',(1.,0.,0.));
#17075=DIRECTION('',(0.,-1.,0.));
#17076=DIRECTION('',(0.,1.,0.));
#17077=DIRECTION('center_axis',(0.,1.,0.));
#17078=DIRECTION('ref_axis',(1.,0.,0.));
#17079=DIRECTION('',(0.,-1.,0.));
#17080=DIRECTION('',(0.,1.,0.));
#17081=DIRECTION('center_axis',(0.10517954525379,0.,-0.994453248403466));
#17082=DIRECTION('ref_axis',(-0.994453248403466,0.,-0.10517954525379));
#17083=DIRECTION('',(-0.994453248403466,0.,-0.10517954525379));
#17084=DIRECTION('',(0.,1.,0.));
#17085=DIRECTION('center_axis',(-0.808632003366459,0.,0.588314782350016));
#17086=DIRECTION('ref_axis',(0.588314782350016,0.,0.808632003366459));
#17087=DIRECTION('',(0.588314782350016,0.,0.808632003366459));
#17088=DIRECTION('center_axis',(0.,1.,0.));
#17089=DIRECTION('ref_axis',(-0.5,0.,0.866025403784438));
#17090=DIRECTION('center_axis',(0.,1.,0.));
#17091=DIRECTION('ref_axis',(-0.64278760968654,0.,0.766044443118978));
#17092=DIRECTION('',(0.438959485082241,0.,0.89850685609868));
#17093=DIRECTION('',(-0.961081032674752,0.,-0.276266625984452));
#17094=DIRECTION('center_axis',(0.276266625984452,0.,-0.961081032674752));
#17095=DIRECTION('ref_axis',(-0.961081032674752,0.,-0.276266625984452));
#17096=DIRECTION('',(0.,1.,0.));
#17097=DIRECTION('center_axis',(-0.89850685609868,0.,0.438959485082241));
#17098=DIRECTION('ref_axis',(0.438959485082241,0.,0.89850685609868));
#17099=DIRECTION('center_axis',(0.438959485082234,0.,-0.898506856098683));
#17100=DIRECTION('ref_axis',(-0.898506856098683,0.,-0.438959485082234));
#17101=DIRECTION('',(-0.898506856098683,0.,-0.438959485082234));
#17102=DIRECTION('',(0.,1.,0.));
#17103=DIRECTION('center_axis',(-0.961081032674749,0.,0.27626662598446));
#17104=DIRECTION('ref_axis',(0.27626662598446,0.,0.961081032674749));
#17105=DIRECTION('',(0.27626662598446,0.,0.961081032674749));
#17106=DIRECTION('center_axis',(0.,1.,0.));
#17107=DIRECTION('ref_axis',(-0.766044443118978,0.,0.642787609686539));
#17108=DIRECTION('center_axis',(0.,1.,0.));
#17109=DIRECTION('ref_axis',(-0.866025403784439,0.,0.5));
#17110=DIRECTION('',(0.105179545253798,0.,0.994453248403465));
#17111=DIRECTION('',(-0.808632003366464,0.,-0.58831478235001));
#17112=DIRECTION('center_axis',(0.58831478235001,0.,-0.808632003366464));
#17113=DIRECTION('ref_axis',(-0.808632003366464,0.,-0.58831478235001));
#17114=DIRECTION('',(0.,1.,0.));
#17115=DIRECTION('center_axis',(-0.994453248403465,0.,0.105179545253798));
#17116=DIRECTION('ref_axis',(0.105179545253798,0.,0.994453248403465));
#17117=DIRECTION('center_axis',(0.719794432657726,0.,-0.694187276399491));
#17118=DIRECTION('ref_axis',(-0.694187276399491,0.,-0.719794432657726));
#17119=DIRECTION('',(-0.694187276399491,0.,-0.719794432657726));
#17120=DIRECTION('',(0.,1.,0.));
#17121=DIRECTION('center_axis',(-0.997609505397066,0.,-0.0691033627359827));
#17122=DIRECTION('ref_axis',(-0.0691033627359827,0.,0.997609505397066));
#17123=DIRECTION('',(-0.0691033627359827,0.,0.997609505397066));
#17124=DIRECTION('center_axis',(0.,1.,0.));
#17125=DIRECTION('ref_axis',(-0.939692620785909,0.,0.342020143325668));
#17126=DIRECTION('center_axis',(0.,1.,0.));
#17127=DIRECTION('ref_axis',(-0.984807753012208,0.,0.17364817766693));
#17128=DIRECTION('',(-0.241286600017019,0.,0.970453902383945));
#17129=DIRECTION('',(-0.558650020314831,0.,-0.829403493362693));
#17130=DIRECTION('center_axis',(0.829403493362693,0.,-0.558650020314831));
#17131=DIRECTION('ref_axis',(-0.558650020314831,0.,-0.829403493362693));
#17132=DIRECTION('',(0.,1.,0.));
#17133=DIRECTION('center_axis',(-0.970453902383945,0.,-0.241286600017019));
#17134=DIRECTION('ref_axis',(-0.241286600017019,0.,0.970453902383945));
#17135=DIRECTION('center_axis',(0.913811548620253,0.,-0.406138466053456));
#17136=DIRECTION('ref_axis',(-0.406138466053456,0.,-0.913811548620253));
#17137=DIRECTION('',(-0.406138466053456,0.,-0.913811548620253));
#17138=DIRECTION('',(0.,1.,0.));
#17139=DIRECTION('center_axis',(-0.913811548620257,0.,-0.406138466053449));
#17140=DIRECTION('ref_axis',(-0.406138466053449,0.,0.913811548620257));
#17141=DIRECTION('',(-0.406138466053449,0.,0.913811548620257));
#17142=DIRECTION('center_axis',(0.,1.,0.));
#17143=DIRECTION('ref_axis',(-1.,0.,-1.83697019872103E-16));
#17144=DIRECTION('center_axis',(0.,1.,0.));
#17145=DIRECTION('ref_axis',(-0.984807753012208,0.,-0.17364817766693));
#17146=DIRECTION('',(-0.558650020314825,0.,0.829403493362697));
#17147=DIRECTION('',(-0.241286600017026,0.,-0.970453902383943));
#17148=DIRECTION('center_axis',(0.970453902383943,0.,-0.241286600017026));
#17149=DIRECTION('ref_axis',(-0.241286600017026,0.,-0.970453902383943));
#17150=DIRECTION('',(0.,1.,0.));
#17151=DIRECTION('center_axis',(-0.829403493362697,0.,-0.558650020314825));
#17152=DIRECTION('ref_axis',(-0.558650020314825,0.,0.829403493362697));
#17153=DIRECTION('center_axis',(0.997609505397066,0.,-0.0691033627359897));
#17154=DIRECTION('ref_axis',(-0.0691033627359897,0.,-0.997609505397066));
#17155=DIRECTION('',(-0.0691033627359897,0.,-0.997609505397066));
#17156=DIRECTION('',(0.,1.,0.));
#17157=DIRECTION('center_axis',(-0.719794432657731,0.,-0.694187276399486));
#17158=DIRECTION('ref_axis',(-0.694187276399486,0.,0.719794432657731));
#17159=DIRECTION('',(-0.694187276399485,0.,0.719794432657731));
#17160=DIRECTION('center_axis',(0.,1.,0.));
#17161=DIRECTION('ref_axis',(-0.939692620785908,0.,-0.342020143325669));
#17162=DIRECTION('center_axis',(0.,1.,0.));
#17163=DIRECTION('ref_axis',(-0.866025403784438,0.,-0.5));
#17164=DIRECTION('',(-0.808632003366459,0.,0.588314782350016));
#17165=DIRECTION('',(0.10517954525379,0.,-0.994453248403466));
#17166=DIRECTION('center_axis',(0.994453248403466,0.,0.10517954525379));
#17167=DIRECTION('ref_axis',(0.10517954525379,0.,-0.994453248403466));
#17168=DIRECTION('',(0.,1.,0.));
#17169=DIRECTION('center_axis',(-0.588314782350016,0.,-0.808632003366459));
#17170=DIRECTION('ref_axis',(-0.808632003366459,0.,0.588314782350016));
#17171=DIRECTION('center_axis',(0.961081032674752,0.,0.276266625984452));
#17172=DIRECTION('ref_axis',(0.276266625984452,0.,-0.961081032674752));
#17173=DIRECTION('',(0.276266625984452,0.,-0.961081032674752));
#17174=DIRECTION('',(0.,1.,0.));
#17175=DIRECTION('center_axis',(-0.438959485082242,0.,-0.89850685609868));
#17176=DIRECTION('ref_axis',(-0.89850685609868,0.,0.438959485082242));
#17177=DIRECTION('',(-0.89850685609868,0.,0.438959485082241));
#17178=DIRECTION('center_axis',(0.,1.,0.));
#17179=DIRECTION('ref_axis',(-0.766044443118978,0.,-0.642787609686539));
#17180=DIRECTION('center_axis',(0.,1.,0.));
#17181=DIRECTION('ref_axis',(-0.642787609686539,0.,-0.766044443118978));
#17182=DIRECTION('',(-0.961081032674749,0.,0.27626662598446));
#17183=DIRECTION('',(0.438959485082234,0.,-0.898506856098683));
#17184=DIRECTION('center_axis',(0.898506856098683,0.,0.438959485082234));
#17185=DIRECTION('ref_axis',(0.438959485082234,0.,-0.898506856098683));
#17186=DIRECTION('',(0.,1.,0.));
#17187=DIRECTION('center_axis',(-0.27626662598446,0.,-0.961081032674749));
#17188=DIRECTION('ref_axis',(-0.961081032674749,0.,0.27626662598446));
#17189=DIRECTION('center_axis',(0.808632003366463,0.,0.58831478235001));
#17190=DIRECTION('ref_axis',(0.58831478235001,0.,-0.808632003366463));
#17191=DIRECTION('',(0.58831478235001,0.,-0.808632003366463));
#17192=DIRECTION('',(0.,1.,0.));
#17193=DIRECTION('center_axis',(-0.105179545253798,0.,-0.994453248403465));
#17194=DIRECTION('ref_axis',(-0.994453248403465,0.,0.105179545253798));
#17195=DIRECTION('',(-0.994453248403465,0.,0.105179545253798));
#17196=DIRECTION('center_axis',(0.,1.,0.));
#17197=DIRECTION('ref_axis',(-0.5,0.,-0.866025403784439));
#17198=DIRECTION('center_axis',(0.,1.,0.));
#17199=DIRECTION('ref_axis',(-0.342020143325669,0.,-0.939692620785908));
#17200=DIRECTION('',(-0.997609505397066,0.,-0.0691033627359822));
#17201=DIRECTION('',(0.719794432657725,0.,-0.694187276399491));
#17202=DIRECTION('center_axis',(0.694187276399491,0.,0.719794432657725));
#17203=DIRECTION('ref_axis',(0.719794432657725,0.,-0.694187276399491));
#17204=DIRECTION('',(0.,1.,0.));
#17205=DIRECTION('center_axis',(0.0691033627359822,0.,-0.997609505397066));
#17206=DIRECTION('ref_axis',(-0.997609505397066,0.,-0.0691033627359822));
#17207=DIRECTION('center_axis',(0.558650020314831,0.,0.829403493362693));
#17208=DIRECTION('ref_axis',(0.829403493362693,0.,-0.558650020314831));
#17209=DIRECTION('',(0.829403493362693,0.,-0.558650020314831));
#17210=DIRECTION('',(0.,1.,0.));
#17211=DIRECTION('center_axis',(0.241286600017019,0.,-0.970453902383945));
#17212=DIRECTION('ref_axis',(-0.970453902383945,0.,-0.241286600017019));
#17213=DIRECTION('',(-0.970453902383945,0.,-0.241286600017019));
#17214=DIRECTION('center_axis',(0.,1.,0.));
#17215=DIRECTION('ref_axis',(-0.17364817766693,0.,-0.984807753012208));
#17216=DIRECTION('center_axis',(0.,1.,0.));
#17217=DIRECTION('ref_axis',(1.22464679914735E-16,0.,-1.));
#17218=DIRECTION('',(-0.913811548620257,0.,-0.406138466053448));
#17219=DIRECTION('',(0.913811548620253,0.,-0.406138466053456));
#17220=DIRECTION('center_axis',(0.406138466053456,0.,0.913811548620253));
#17221=DIRECTION('ref_axis',(0.913811548620253,0.,-0.406138466053456));
#17222=DIRECTION('',(0.,1.,0.));
#17223=DIRECTION('center_axis',(0.406138466053449,0.,-0.913811548620257));
#17224=DIRECTION('ref_axis',(-0.913811548620257,0.,-0.406138466053449));
#17225=DIRECTION('center_axis',(0.241286600017026,0.,0.970453902383943));
#17226=DIRECTION('ref_axis',(0.970453902383943,0.,-0.241286600017026));
#17227=DIRECTION('',(0.970453902383943,0.,-0.241286600017026));
#17228=DIRECTION('',(0.,1.,0.));
#17229=DIRECTION('center_axis',(0.558650020314825,0.,-0.829403493362697));
#17230=DIRECTION('ref_axis',(-0.829403493362697,0.,-0.558650020314825));
#17231=DIRECTION('',(-0.829403493362697,0.,-0.558650020314825));
#17232=DIRECTION('center_axis',(0.,1.,0.));
#17233=DIRECTION('ref_axis',(0.173648177666931,0.,-0.984807753012208));
#17234=DIRECTION('center_axis',(0.,1.,0.));
#17235=DIRECTION('ref_axis',(0.342020143325669,0.,-0.939692620785908));
#17236=DIRECTION('',(-0.719794432657731,0.,-0.694187276399485));
#17237=DIRECTION('',(0.997609505397066,0.,-0.0691033627359902));
#17238=DIRECTION('center_axis',(0.0691033627359902,0.,0.997609505397066));
#17239=DIRECTION('ref_axis',(0.997609505397066,0.,-0.0691033627359902));
#17240=DIRECTION('',(0.,1.,0.));
#17241=DIRECTION('center_axis',(0.694187276399485,0.,-0.719794432657731));
#17242=DIRECTION('ref_axis',(-0.719794432657731,0.,-0.694187276399485));
#17243=DIRECTION('center_axis',(-0.10517954525379,0.,0.994453248403466));
#17244=DIRECTION('ref_axis',(0.994453248403466,0.,0.10517954525379));
#17245=DIRECTION('',(0.994453248403466,0.,0.10517954525379));
#17246=DIRECTION('',(0.,1.,0.));
#17247=DIRECTION('center_axis',(0.808632003366459,0.,-0.588314782350017));
#17248=DIRECTION('ref_axis',(-0.588314782350017,0.,-0.808632003366459));
#17249=DIRECTION('',(-0.588314782350017,0.,-0.808632003366458));
#17250=DIRECTION('center_axis',(0.,1.,0.));
#17251=DIRECTION('ref_axis',(0.5,0.,-0.866025403784439));
#17252=DIRECTION('center_axis',(0.,1.,0.));
#17253=DIRECTION('ref_axis',(0.642787609686539,0.,-0.766044443118978));
#17254=DIRECTION('',(-0.438959485082241,0.,-0.89850685609868));
#17255=DIRECTION('',(0.961081032674752,0.,0.276266625984452));
#17256=DIRECTION('center_axis',(-0.276266625984452,0.,0.961081032674752));
#17257=DIRECTION('ref_axis',(0.961081032674752,0.,0.276266625984452));
#17258=DIRECTION('',(0.,1.,0.));
#17259=DIRECTION('center_axis',(0.89850685609868,0.,-0.438959485082242));
#17260=DIRECTION('ref_axis',(-0.438959485082242,0.,-0.89850685609868));
#17261=DIRECTION('center_axis',(-0.438959485082234,0.,0.898506856098683));
#17262=DIRECTION('ref_axis',(0.898506856098683,0.,0.438959485082234));
#17263=DIRECTION('',(0.898506856098683,0.,0.438959485082234));
#17264=DIRECTION('',(0.,1.,0.));
#17265=DIRECTION('center_axis',(0.961081032674749,0.,-0.27626662598446));
#17266=DIRECTION('ref_axis',(-0.27626662598446,0.,-0.961081032674749));
#17267=DIRECTION('',(-0.27626662598446,0.,-0.961081032674749));
#17268=DIRECTION('center_axis',(0.,1.,0.));
#17269=DIRECTION('ref_axis',(0.766044443118978,0.,-0.642787609686539));
#17270=DIRECTION('center_axis',(0.,1.,0.));
#17271=DIRECTION('ref_axis',(0.866025403784439,0.,-0.5));
#17272=DIRECTION('',(-0.105179545253798,0.,-0.994453248403465));
#17273=DIRECTION('',(0.808632003366463,0.,0.58831478235001));
#17274=DIRECTION('center_axis',(-0.58831478235001,0.,0.808632003366463));
#17275=DIRECTION('ref_axis',(0.808632003366463,0.,0.58831478235001));
#17276=DIRECTION('',(0.,1.,0.));
#17277=DIRECTION('center_axis',(0.994453248403465,0.,-0.105179545253798));
#17278=DIRECTION('ref_axis',(-0.105179545253798,0.,-0.994453248403465));
#17279=DIRECTION('center_axis',(-0.719794432657725,0.,0.694187276399491));
#17280=DIRECTION('ref_axis',(0.694187276399491,0.,0.719794432657725));
#17281=DIRECTION('',(0.694187276399491,0.,0.719794432657725));
#17282=DIRECTION('',(0.,1.,0.));
#17283=DIRECTION('center_axis',(0.997609505397066,0.,0.0691033627359822));
#17284=DIRECTION('ref_axis',(0.0691033627359822,0.,-0.997609505397066));
#17285=DIRECTION('',(0.0691033627359822,0.,-0.997609505397066));
#17286=DIRECTION('center_axis',(0.,1.,0.));
#17287=DIRECTION('ref_axis',(0.939692620785908,0.,-0.342020143325669));
#17288=DIRECTION('center_axis',(0.,1.,0.));
#17289=DIRECTION('ref_axis',(0.984807753012208,0.,-0.17364817766693));
#17290=DIRECTION('',(0.241286600017018,0.,-0.970453902383945));
#17291=DIRECTION('',(0.558650020314831,0.,0.829403493362693));
#17292=DIRECTION('center_axis',(-0.829403493362693,0.,0.558650020314831));
#17293=DIRECTION('ref_axis',(0.558650020314831,0.,0.829403493362693));
#17294=DIRECTION('',(0.,1.,0.));
#17295=DIRECTION('center_axis',(0.970453902383945,0.,0.241286600017018));
#17296=DIRECTION('ref_axis',(0.241286600017018,0.,-0.970453902383945));
#17297=DIRECTION('center_axis',(-0.913811548620253,0.,0.406138466053456));
#17298=DIRECTION('ref_axis',(0.406138466053456,0.,0.913811548620253));
#17299=DIRECTION('',(0.406138466053456,0.,0.913811548620253));
#17300=DIRECTION('',(0.,1.,0.));
#17301=DIRECTION('center_axis',(0.913811548620257,0.,0.406138466053448));
#17302=DIRECTION('ref_axis',(0.406138466053448,0.,-0.913811548620257));
#17303=DIRECTION('',(0.406138466053448,0.,-0.913811548620257));
#17304=DIRECTION('center_axis',(0.,1.,0.));
#17305=DIRECTION('ref_axis',(1.,0.,6.12323399573677E-17));
#17306=DIRECTION('center_axis',(0.,1.,0.));
#17307=DIRECTION('ref_axis',(0.984807753012208,0.,0.17364817766693));
#17308=DIRECTION('',(0.558650020314825,0.,-0.829403493362697));
#17309=DIRECTION('',(0.241286600017026,0.,0.970453902383943));
#17310=DIRECTION('center_axis',(-0.970453902383943,0.,0.241286600017026));
#17311=DIRECTION('ref_axis',(0.241286600017026,0.,0.970453902383943));
#17312=DIRECTION('',(0.,1.,0.));
#17313=DIRECTION('center_axis',(0.829403493362697,0.,0.558650020314825));
#17314=DIRECTION('ref_axis',(0.558650020314825,0.,-0.829403493362697));
#17315=DIRECTION('center_axis',(-0.997609505397066,0.,0.0691033627359903));
#17316=DIRECTION('ref_axis',(0.0691033627359903,0.,0.997609505397066));
#17317=DIRECTION('',(0.0691033627359903,0.,0.997609505397066));
#17318=DIRECTION('',(0.,1.,0.));
#17319=DIRECTION('center_axis',(0.719794432657731,0.,0.694187276399485));
#17320=DIRECTION('ref_axis',(0.694187276399485,0.,-0.719794432657731));
#17321=DIRECTION('',(0.694187276399485,0.,-0.719794432657731));
#17322=DIRECTION('center_axis',(0.,1.,0.));
#17323=DIRECTION('ref_axis',(0.939692620785908,0.,0.342020143325669));
#17324=DIRECTION('center_axis',(0.,1.,0.));
#17325=DIRECTION('ref_axis',(0.866025403784439,0.,0.5));
#17326=DIRECTION('',(0.808632003366459,0.,-0.588314782350017));
#17327=DIRECTION('',(-0.10517954525379,0.,0.994453248403466));
#17328=DIRECTION('center_axis',(-0.994453248403466,0.,-0.10517954525379));
#17329=DIRECTION('ref_axis',(-0.10517954525379,0.,0.994453248403466));
#17330=DIRECTION('',(0.,1.,0.));
#17331=DIRECTION('center_axis',(0.588314782350017,0.,0.808632003366459));
#17332=DIRECTION('ref_axis',(0.808632003366459,0.,-0.588314782350017));
#17333=DIRECTION('center_axis',(-0.961081032674752,0.,-0.276266625984452));
#17334=DIRECTION('ref_axis',(-0.276266625984452,0.,0.961081032674752));
#17335=DIRECTION('',(-0.276266625984452,0.,0.961081032674752));
#17336=DIRECTION('',(0.,1.,0.));
#17337=DIRECTION('center_axis',(0.438959485082242,0.,0.89850685609868));
#17338=DIRECTION('ref_axis',(0.89850685609868,0.,-0.438959485082242));
#17339=DIRECTION('',(0.89850685609868,0.,-0.438959485082242));
#17340=DIRECTION('center_axis',(0.,1.,0.));
#17341=DIRECTION('ref_axis',(0.766044443118978,0.,0.642787609686539));
#17342=DIRECTION('center_axis',(0.,1.,0.));
#17343=DIRECTION('ref_axis',(0.642787609686539,0.,0.766044443118978));
#17344=DIRECTION('',(0.961081032674749,0.,-0.27626662598446));
#17345=DIRECTION('',(-0.438959485082234,0.,0.898506856098683));
#17346=DIRECTION('center_axis',(-0.898506856098683,0.,-0.438959485082234));
#17347=DIRECTION('ref_axis',(-0.438959485082234,0.,0.898506856098683));
#17348=DIRECTION('',(0.,1.,0.));
#17349=DIRECTION('center_axis',(0.27626662598446,0.,0.961081032674749));
#17350=DIRECTION('ref_axis',(0.961081032674749,0.,-0.27626662598446));
#17351=DIRECTION('center_axis',(-0.808632003366463,0.,-0.58831478235001));
#17352=DIRECTION('ref_axis',(-0.58831478235001,0.,0.808632003366463));
#17353=DIRECTION('',(-0.58831478235001,0.,0.808632003366463));
#17354=DIRECTION('',(0.,1.,0.));
#17355=DIRECTION('center_axis',(0.105179545253798,0.,0.994453248403465));
#17356=DIRECTION('ref_axis',(0.994453248403465,0.,-0.105179545253798));
#17357=DIRECTION('',(0.994453248403465,0.,-0.105179545253798));
#17358=DIRECTION('center_axis',(0.,1.,0.));
#17359=DIRECTION('ref_axis',(0.5,0.,0.866025403784439));
#17360=DIRECTION('center_axis',(0.,1.,0.));
#17361=DIRECTION('ref_axis',(0.342020143325669,0.,0.939692620785908));
#17362=DIRECTION('',(0.997609505397066,0.,0.0691033627359822));
#17363=DIRECTION('',(-0.719794432657725,0.,0.694187276399491));
#17364=DIRECTION('center_axis',(-0.694187276399491,0.,-0.719794432657725));
#17365=DIRECTION('ref_axis',(-0.719794432657725,0.,0.694187276399491));
#17366=DIRECTION('',(0.,1.,0.));
#17367=DIRECTION('center_axis',(-0.0691033627359822,0.,0.997609505397066));
#17368=DIRECTION('ref_axis',(0.997609505397066,0.,0.0691033627359822));
#17369=DIRECTION('center_axis',(-0.558650020314831,0.,-0.829403493362693));
#17370=DIRECTION('ref_axis',(-0.829403493362693,0.,0.558650020314831));
#17371=DIRECTION('',(-0.829403493362693,0.,0.558650020314831));
#17372=DIRECTION('',(0.,1.,0.));
#17373=DIRECTION('center_axis',(-0.241286600017018,0.,0.970453902383945));
#17374=DIRECTION('ref_axis',(0.970453902383945,0.,0.241286600017018));
#17375=DIRECTION('',(0.970453902383945,0.,0.241286600017018));
#17376=DIRECTION('center_axis',(0.,1.,0.));
#17377=DIRECTION('ref_axis',(0.17364817766693,0.,0.984807753012208));
#17378=DIRECTION('center_axis',(0.,1.,0.));
#17379=DIRECTION('ref_axis',(0.,0.,1.));
#17380=DIRECTION('',(0.913811548620257,0.,0.406138466053448));
#17381=DIRECTION('',(-0.913811548620253,0.,0.406138466053456));
#17382=DIRECTION('center_axis',(-0.406138466053456,0.,-0.913811548620253));
#17383=DIRECTION('ref_axis',(-0.913811548620253,0.,0.406138466053456));
#17384=DIRECTION('',(0.,1.,0.));
#17385=DIRECTION('center_axis',(-0.406138466053448,0.,0.913811548620257));
#17386=DIRECTION('ref_axis',(0.913811548620257,0.,0.406138466053448));
#17387=DIRECTION('center_axis',(0.,1.,0.));
#17388=DIRECTION('ref_axis',(1.,0.,0.));
#17389=DIRECTION('',(-0.5,0.,-0.866025403784439));
#17390=DIRECTION('',(-1.,0.,0.));
#17391=DIRECTION('',(-0.499999999999999,0.,0.866025403784439));
#17392=DIRECTION('',(0.500000000000001,0.,0.866025403784438));
#17393=DIRECTION('',(1.,0.,0.));
#17394=DIRECTION('',(0.5,0.,-0.866025403784438));
#17395=DIRECTION('center_axis',(0.,-1.,0.));
#17396=DIRECTION('ref_axis',(0.,0.,-1.));
#17397=DIRECTION('',(-0.5,0.,-0.866025403784439));
#17398=DIRECTION('center_axis',(0.,-1.,0.));
#17399=DIRECTION('ref_axis',(1.,0.,0.));
#17400=DIRECTION('center_axis',(0.,-1.,0.));
#17401=DIRECTION('ref_axis',(0.,0.,-1.));
#17402=DIRECTION('',(-1.,0.,0.));
#17403=DIRECTION('center_axis',(0.,-1.,0.));
#17404=DIRECTION('ref_axis',(1.,0.,0.));
#17405=DIRECTION('center_axis',(0.,-1.,0.));
#17406=DIRECTION('ref_axis',(0.,0.,-1.));
#17407=DIRECTION('',(-0.499999999999999,0.,0.866025403784439));
#17408=DIRECTION('center_axis',(0.,-1.,0.));
#17409=DIRECTION('ref_axis',(1.,0.,0.));
#17410=DIRECTION('center_axis',(0.,-1.,0.));
#17411=DIRECTION('ref_axis',(0.,0.,-1.));
#17412=DIRECTION('',(0.500000000000001,0.,0.866025403784438));
#17413=DIRECTION('center_axis',(0.,-1.,0.));
#17414=DIRECTION('ref_axis',(1.,0.,0.));
#17415=DIRECTION('center_axis',(0.,-1.,0.));
#17416=DIRECTION('ref_axis',(0.,0.,-1.));
#17417=DIRECTION('',(1.,0.,0.));
#17418=DIRECTION('center_axis',(0.,-1.,0.));
#17419=DIRECTION('ref_axis',(1.,0.,0.));
#17420=DIRECTION('center_axis',(0.,-1.,0.));
#17421=DIRECTION('ref_axis',(0.,0.,-1.));
#17422=DIRECTION('',(0.5,0.,-0.866025403784438));
#17423=DIRECTION('center_axis',(0.,-1.,0.));
#17424=DIRECTION('ref_axis',(1.,0.,0.));
#17425=DIRECTION('center_axis',(0.,-1.,0.));
#17426=DIRECTION('ref_axis',(1.,0.,0.));
#17427=DIRECTION('',(-0.85716730070211,-0.515038074910058,-1.04972719113862E-16));
#17428=DIRECTION('center_axis',(0.866025403784439,0.,-0.5));
#17429=DIRECTION('ref_axis',(-0.5,0.,-0.866025403784439));
#17430=DIRECTION('',(0.,1.,0.));
#17431=DIRECTION('',(0.,1.,0.));
#17432=DIRECTION('center_axis',(0.866025403784438,0.,0.5));
#17433=DIRECTION('ref_axis',(0.5,0.,-0.866025403784438));
#17434=DIRECTION('',(0.,1.,0.));
#17435=DIRECTION('center_axis',(0.,0.,1.));
#17436=DIRECTION('ref_axis',(1.,0.,0.));
#17437=DIRECTION('',(0.,1.,0.));
#17438=DIRECTION('center_axis',(-0.866025403784438,0.,0.500000000000001));
#17439=DIRECTION('ref_axis',(0.500000000000001,0.,0.866025403784438));
#17440=DIRECTION('',(0.,1.,0.));
#17441=DIRECTION('center_axis',(-0.866025403784439,0.,-0.499999999999999));
#17442=DIRECTION('ref_axis',(-0.499999999999999,0.,0.866025403784439));
#17443=DIRECTION('',(0.,1.,0.));
#17444=DIRECTION('center_axis',(0.,0.,-1.));
#17445=DIRECTION('ref_axis',(-1.,0.,0.));
#17446=DIRECTION('axis',(0.,0.,1.));
#17447=DIRECTION('refdir',(1.,0.,0.));
#17448=DIRECTION('center_axis',(0.,-1.,0.));
#17449=DIRECTION('ref_axis',(0.932069076459839,0.,-0.362280604928421));
#17450=DIRECTION('',(0.,1.,0.));
#17451=DIRECTION('center_axis',(0.,1.,0.));
#17452=DIRECTION('ref_axis',(1.,0.,9.69272361004426E-14));
#17453=DIRECTION('center_axis',(0.,-1.,0.));
#17454=DIRECTION('ref_axis',(0.932069076459839,0.,-0.362280604928421));
#17455=DIRECTION('',(0.,1.,0.));
#17456=DIRECTION('center_axis',(0.,-1.,0.));
#17457=DIRECTION('ref_axis',(0.932069076459839,0.,-0.362280604928421));
#17458=DIRECTION('',(0.,1.,0.));
#17459=DIRECTION('center_axis',(0.,-1.,0.));
#17460=DIRECTION('ref_axis',(0.932069076459839,0.,-0.362280604928421));
#17461=DIRECTION('',(0.,1.,0.));
#17462=DIRECTION('center_axis',(0.,-1.,0.));
#17463=DIRECTION('ref_axis',(0.932069076459839,0.,-0.362280604928421));
#17464=DIRECTION('',(0.,1.,0.));
#17465=DIRECTION('center_axis',(0.,-1.,0.));
#17466=DIRECTION('ref_axis',(0.932069076459839,0.,-0.362280604928421));
#17467=DIRECTION('',(0.,1.,0.));
#17468=DIRECTION('center_axis',(0.,-1.,0.));
#17469=DIRECTION('ref_axis',(0.932069076459839,0.,-0.362280604928421));
#17470=DIRECTION('',(0.,1.,0.));
#17471=DIRECTION('center_axis',(0.,-1.,0.));
#17472=DIRECTION('ref_axis',(0.932069076459839,0.,-0.362280604928421));
#17473=DIRECTION('',(0.,1.,0.));
#17474=DIRECTION('center_axis',(0.,-1.,0.));
#17475=DIRECTION('ref_axis',(0.932069076459839,0.,-0.362280604928421));
#17476=DIRECTION('',(0.,1.,0.));
#17477=DIRECTION('center_axis',(0.,-1.,0.));
#17478=DIRECTION('ref_axis',(0.932069076459839,0.,-0.362280604928421));
#17479=DIRECTION('',(0.,1.,0.));
#17480=DIRECTION('center_axis',(0.,-1.,0.));
#17481=DIRECTION('ref_axis',(0.932069076459839,0.,-0.362280604928421));
#17482=DIRECTION('',(0.,1.,0.));
#17483=DIRECTION('center_axis',(0.,-1.,0.));
#17484=DIRECTION('ref_axis',(0.932069076459839,0.,-0.362280604928421));
#17485=DIRECTION('',(0.,1.,0.));
#17486=DIRECTION('center_axis',(0.,-1.,0.));
#17487=DIRECTION('ref_axis',(0.932069076459839,0.,-0.362280604928421));
#17488=DIRECTION('',(0.,1.,0.));
#17489=DIRECTION('center_axis',(0.,-1.,0.));
#17490=DIRECTION('ref_axis',(0.932069076459839,0.,-0.362280604928421));
#17491=DIRECTION('',(0.,1.,0.));
#17492=DIRECTION('center_axis',(0.,-1.,0.));
#17493=DIRECTION('ref_axis',(1.,0.,0.));
#17494=DIRECTION('center_axis',(0.,1.,0.));
#17495=DIRECTION('ref_axis',(1.,0.,0.));
#17496=DIRECTION('center_axis',(0.,-1.,0.));
#17497=DIRECTION('ref_axis',(1.,0.,0.));
#17498=DIRECTION('center_axis',(0.,-1.,0.));
#17499=DIRECTION('ref_axis',(0.846353653806749,0.,-0.532621340811618));
#17500=DIRECTION('center_axis',(0.,-1.,0.));
#17501=DIRECTION('ref_axis',(1.,0.,9.69272361004426E-14));
#17502=DIRECTION('center_axis',(0.,1.,0.));
#17503=DIRECTION('ref_axis',(0.,0.,1.));
#17504=DIRECTION('center_axis',(0.,-1.,0.));
#17505=DIRECTION('ref_axis',(1.,0.,0.));
#17506=DIRECTION('center_axis',(0.,-1.,0.));
#17507=DIRECTION('ref_axis',(1.,0.,0.));
#17508=DIRECTION('center_axis',(0.,1.,0.));
#17509=DIRECTION('ref_axis',(0.,0.,1.));
#17510=DIRECTION('center_axis',(0.,1.,0.));
#17511=DIRECTION('ref_axis',(1.,0.,0.));
#17512=DIRECTION('center_axis',(0.,1.,0.));
#17513=DIRECTION('ref_axis',(1.,0.,0.));
#17514=DIRECTION('center_axis',(0.,1.,0.));
#17515=DIRECTION('ref_axis',(0.,0.,1.));
#17516=DIRECTION('center_axis',(0.,-1.,0.));
#17517=DIRECTION('ref_axis',(1.,0.,0.));
#17518=DIRECTION('center_axis',(1.,0.,0.));
#17519=DIRECTION('ref_axis',(0.,0.,-1.));
#17520=DIRECTION('center_axis',(0.,1.,0.));
#17521=DIRECTION('ref_axis',(1.,0.,0.));
#17522=DIRECTION('center_axis',(0.,1.,0.));
#17523=DIRECTION('ref_axis',(1.,0.,0.));
#17524=DIRECTION('center_axis',(0.,1.,0.));
#17525=DIRECTION('ref_axis',(1.,0.,0.));
#17526=DIRECTION('',(0.707106781186547,-0.707106781186548,-8.65956056235493E-17));
#17527=DIRECTION('center_axis',(0.,1.,0.));
#17528=DIRECTION('ref_axis',(1.,0.,0.));
#17529=DIRECTION('center_axis',(0.,1.,0.));
#17530=DIRECTION('ref_axis',(1.,0.,0.));
#17531=DIRECTION('center_axis',(-0.241286600017018,0.,0.970453902383945));
#17532=DIRECTION('ref_axis',(-0.970453902383945,0.,-0.241286600017018));
#17533=DIRECTION('',(0.,1.,0.));
#17534=DIRECTION('',(-0.970453902383945,0.,-0.241286600017018));
#17535=DIRECTION('',(0.,-1.,0.));
#17536=DIRECTION('center_axis',(-0.558650020314823,0.,-0.829403493362699));
#17537=DIRECTION('ref_axis',(0.829403493362699,0.,-0.558650020314823));
#17538=DIRECTION('',(0.,-1.,0.));
#17539=DIRECTION('',(0.829403493362699,0.,-0.558650020314823));
#17540=DIRECTION('center_axis',(0.,-1.,0.));
#17541=DIRECTION('ref_axis',(-0.17364817766693,0.,-0.984807753012208));
#17542=DIRECTION('center_axis',(0.,-1.,0.));
#17543=DIRECTION('ref_axis',(1.,0.,0.));
#17544=DIRECTION('center_axis',(0.,-1.,0.));
#17545=DIRECTION('ref_axis',(1.,0.,0.));
#17546=DIRECTION('center_axis',(0.,1.,0.));
#17547=DIRECTION('ref_axis',(1.,0.,0.));
#17548=DIRECTION('center_axis',(0.,1.,0.));
#17549=DIRECTION('ref_axis',(1.,0.,0.));
#17550=DIRECTION('center_axis',(0.,1.,0.));
#17551=DIRECTION('ref_axis',(1.,0.,0.));
#17552=DIRECTION('center_axis',(0.,1.,0.));
#17553=DIRECTION('ref_axis',(1.,0.,0.));
#17554=DIRECTION('center_axis',(0.,1.,0.));
#17555=DIRECTION('ref_axis',(1.,0.,0.));
#17556=DIRECTION('center_axis',(0.,1.,0.));
#17557=DIRECTION('ref_axis',(1.,0.,0.));
#17558=DIRECTION('center_axis',(0.,1.,0.));
#17559=DIRECTION('ref_axis',(1.,0.,0.));
#17560=DIRECTION('center_axis',(0.,1.,0.));
#17561=DIRECTION('ref_axis',(1.,0.,0.));
#17562=DIRECTION('center_axis',(0.,1.,0.));
#17563=DIRECTION('ref_axis',(1.,0.,0.));
#17564=DIRECTION('center_axis',(0.,1.,0.));
#17565=DIRECTION('ref_axis',(1.,0.,0.));
#17566=DIRECTION('center_axis',(0.,1.,0.));
#17567=DIRECTION('ref_axis',(1.,0.,0.));
#17568=DIRECTION('center_axis',(0.,1.,0.));
#17569=DIRECTION('ref_axis',(1.,0.,0.));
#17570=DIRECTION('center_axis',(0.,1.,0.));
#17571=DIRECTION('ref_axis',(1.,0.,0.));
#17572=DIRECTION('center_axis',(0.,1.,0.));
#17573=DIRECTION('ref_axis',(1.,0.,0.));
#17574=DIRECTION('center_axis',(0.,1.,0.));
#17575=DIRECTION('ref_axis',(1.,0.,0.));
#17576=DIRECTION('center_axis',(0.,1.,0.));
#17577=DIRECTION('ref_axis',(1.,0.,0.));
#17578=DIRECTION('center_axis',(0.,1.,0.));
#17579=DIRECTION('ref_axis',(1.,0.,0.));
#17580=DIRECTION('center_axis',(0.,1.,0.));
#17581=DIRECTION('ref_axis',(1.,0.,0.));
#17582=DIRECTION('center_axis',(0.,1.,0.));
#17583=DIRECTION('ref_axis',(1.,0.,0.));
#17584=DIRECTION('center_axis',(0.,1.,0.));
#17585=DIRECTION('ref_axis',(1.,0.,0.));
#17586=DIRECTION('center_axis',(0.,1.,0.));
#17587=DIRECTION('ref_axis',(1.,0.,0.));
#17588=DIRECTION('center_axis',(0.,1.,0.));
#17589=DIRECTION('ref_axis',(1.,0.,0.));
#17590=DIRECTION('center_axis',(0.,1.,0.));
#17591=DIRECTION('ref_axis',(1.,0.,0.));
#17592=DIRECTION('center_axis',(0.,1.,0.));
#17593=DIRECTION('ref_axis',(1.,0.,0.));
#17594=DIRECTION('center_axis',(0.,1.,0.));
#17595=DIRECTION('ref_axis',(1.,0.,0.));
#17596=DIRECTION('center_axis',(0.,1.,0.));
#17597=DIRECTION('ref_axis',(1.,0.,0.));
#17598=DIRECTION('center_axis',(0.,1.,0.));
#17599=DIRECTION('ref_axis',(1.,0.,0.));
#17600=DIRECTION('center_axis',(0.,1.,0.));
#17601=DIRECTION('ref_axis',(1.,0.,0.));
#17602=DIRECTION('center_axis',(0.,1.,0.));
#17603=DIRECTION('ref_axis',(1.,0.,0.));
#17604=DIRECTION('center_axis',(0.,1.,0.));
#17605=DIRECTION('ref_axis',(1.,0.,0.));
#17606=DIRECTION('center_axis',(0.,1.,0.));
#17607=DIRECTION('ref_axis',(1.,0.,0.));
#17608=DIRECTION('center_axis',(0.,1.,0.));
#17609=DIRECTION('ref_axis',(1.,0.,0.));
#17610=DIRECTION('center_axis',(0.,1.,0.));
#17611=DIRECTION('ref_axis',(1.,0.,0.));
#17612=DIRECTION('center_axis',(0.,1.,0.));
#17613=DIRECTION('ref_axis',(1.,0.,0.));
#17614=DIRECTION('center_axis',(0.,1.,0.));
#17615=DIRECTION('ref_axis',(1.,0.,0.));
#17616=DIRECTION('center_axis',(0.,1.,0.));
#17617=DIRECTION('ref_axis',(1.,0.,0.));
#17618=DIRECTION('',(0.707106781186547,0.707106781186548,8.65956056235493E-17));
#17619=DIRECTION('center_axis',(0.,-1.,0.));
#17620=DIRECTION('ref_axis',(1.,0.,0.));
#17621=DIRECTION('center_axis',(-0.0691033627359813,0.,0.997609505397066));
#17622=DIRECTION('ref_axis',(-0.997609505397066,0.,-0.0691033627359813));
#17623=DIRECTION('',(0.,1.,0.));
#17624=DIRECTION('',(-0.997609505397066,0.,-0.0691033627359813));
#17625=DIRECTION('',(0.,-1.,0.));
#17626=DIRECTION('center_axis',(-0.694187276399484,0.,-0.719794432657732));
#17627=DIRECTION('ref_axis',(0.719794432657732,0.,-0.694187276399484));
#17628=DIRECTION('',(0.,-1.,0.));
#17629=DIRECTION('',(0.719794432657732,0.,-0.694187276399484));
#17630=DIRECTION('center_axis',(0.,-1.,0.));
#17631=DIRECTION('ref_axis',(-0.342020143325669,0.,-0.939692620785908));
#17632=DIRECTION('center_axis',(0.,-1.,0.));
#17633=DIRECTION('ref_axis',(1.,0.,0.));
#17634=DIRECTION('center_axis',(0.105179545253799,0.,0.994453248403465));
#17635=DIRECTION('ref_axis',(-0.994453248403465,0.,0.105179545253799));
#17636=DIRECTION('',(0.,1.,0.));
#17637=DIRECTION('',(-0.994453248403465,0.,0.105179545253799));
#17638=DIRECTION('',(0.,-1.,0.));
#17639=DIRECTION('center_axis',(-0.808632003366458,0.,-0.588314782350018));
#17640=DIRECTION('ref_axis',(0.588314782350018,0.,-0.808632003366458));
#17641=DIRECTION('',(0.,-1.,0.));
#17642=DIRECTION('',(0.588314782350018,0.,-0.808632003366458));
#17643=DIRECTION('center_axis',(0.,-1.,0.));
#17644=DIRECTION('ref_axis',(-0.5,0.,-0.866025403784438));
#17645=DIRECTION('center_axis',(0.,-1.,0.));
#17646=DIRECTION('ref_axis',(1.,0.,0.));
#17647=DIRECTION('center_axis',(0.27626662598446,0.,0.961081032674749));
#17648=DIRECTION('ref_axis',(-0.961081032674749,0.,0.27626662598446));
#17649=DIRECTION('',(0.,1.,0.));
#17650=DIRECTION('',(-0.961081032674749,0.,0.27626662598446));
#17651=DIRECTION('',(0.,-1.,0.));
#17652=DIRECTION('center_axis',(-0.898506856098679,0.,-0.438959485082243));
#17653=DIRECTION('ref_axis',(0.438959485082243,0.,-0.898506856098679));
#17654=DIRECTION('',(0.,-1.,0.));
#17655=DIRECTION('',(0.438959485082243,0.,-0.898506856098679));
#17656=DIRECTION('center_axis',(0.,-1.,0.));
#17657=DIRECTION('ref_axis',(-0.64278760968654,0.,-0.766044443118978));
#17658=DIRECTION('center_axis',(0.,-1.,0.));
#17659=DIRECTION('ref_axis',(1.,0.,0.));
#17660=DIRECTION('center_axis',(0.438959485082242,0.,0.89850685609868));
#17661=DIRECTION('ref_axis',(-0.89850685609868,0.,0.438959485082242));
#17662=DIRECTION('',(0.,1.,0.));
#17663=DIRECTION('',(-0.89850685609868,0.,0.438959485082242));
#17664=DIRECTION('',(0.,-1.,0.));
#17665=DIRECTION('center_axis',(-0.961081032674749,0.,-0.276266625984462));
#17666=DIRECTION('ref_axis',(0.276266625984462,0.,-0.961081032674749));
#17667=DIRECTION('',(0.,-1.,0.));
#17668=DIRECTION('',(0.276266625984462,0.,-0.961081032674749));
#17669=DIRECTION('center_axis',(0.,-1.,0.));
#17670=DIRECTION('ref_axis',(-0.766044443118978,0.,-0.642787609686539));
#17671=DIRECTION('center_axis',(0.,-1.,0.));
#17672=DIRECTION('ref_axis',(1.,0.,0.));
#17673=DIRECTION('center_axis',(0.588314782350017,0.,0.808632003366459));
#17674=DIRECTION('ref_axis',(-0.808632003366459,0.,0.588314782350017));
#17675=DIRECTION('',(0.,1.,0.));
#17676=DIRECTION('',(-0.808632003366459,0.,0.588314782350017));
#17677=DIRECTION('',(0.,-1.,0.));
#17678=DIRECTION('center_axis',(-0.994453248403465,0.,-0.1051795452538));
#17679=DIRECTION('ref_axis',(0.1051795452538,0.,-0.994453248403465));
#17680=DIRECTION('',(0.,-1.,0.));
#17681=DIRECTION('',(0.1051795452538,0.,-0.994453248403465));
#17682=DIRECTION('center_axis',(0.,-1.,0.));
#17683=DIRECTION('ref_axis',(-0.866025403784439,0.,-0.5));
#17684=DIRECTION('center_axis',(0.,-1.,0.));
#17685=DIRECTION('ref_axis',(1.,0.,0.));
#17686=DIRECTION('center_axis',(0.719794432657731,0.,0.694187276399485));
#17687=DIRECTION('ref_axis',(-0.694187276399485,0.,0.719794432657731));
#17688=DIRECTION('',(0.,1.,0.));
#17689=DIRECTION('',(-0.694187276399485,0.,0.719794432657731));
#17690=DIRECTION('',(0.,-1.,0.));
#17691=DIRECTION('center_axis',(-0.997609505397066,0.,0.0691033627359807));
#17692=DIRECTION('ref_axis',(-0.0691033627359807,0.,-0.997609505397066));
#17693=DIRECTION('',(0.,-1.,0.));
#17694=DIRECTION('',(-0.0691033627359807,0.,-0.997609505397066));
#17695=DIRECTION('center_axis',(0.,-1.,0.));
#17696=DIRECTION('ref_axis',(-0.939692620785909,0.,-0.342020143325668));
#17697=DIRECTION('center_axis',(0.,-1.,0.));
#17698=DIRECTION('ref_axis',(1.,0.,0.));
#17699=DIRECTION('center_axis',(0.829403493362698,0.,0.558650020314824));
#17700=DIRECTION('ref_axis',(-0.558650020314824,0.,0.829403493362698));
#17701=DIRECTION('',(0.,1.,0.));
#17702=DIRECTION('',(-0.558650020314824,0.,0.829403493362698));
#17703=DIRECTION('',(0.,-1.,0.));
#17704=DIRECTION('center_axis',(-0.970453902383945,0.,0.241286600017017));
#17705=DIRECTION('ref_axis',(-0.241286600017017,0.,-0.970453902383945));
#17706=DIRECTION('',(0.,-1.,0.));
#17707=DIRECTION('',(-0.241286600017017,0.,-0.970453902383945));
#17708=DIRECTION('center_axis',(0.,-1.,0.));
#17709=DIRECTION('ref_axis',(-0.984807753012208,0.,-0.17364817766693));
#17710=DIRECTION('center_axis',(0.,-1.,0.));
#17711=DIRECTION('ref_axis',(1.,0.,0.));
#17712=DIRECTION('center_axis',(0.913811548620257,0.,0.406138466053448));
#17713=DIRECTION('ref_axis',(-0.406138466053448,0.,0.913811548620257));
#17714=DIRECTION('',(0.,1.,0.));
#17715=DIRECTION('',(-0.406138466053448,0.,0.913811548620257));
#17716=DIRECTION('',(0.,-1.,0.));
#17717=DIRECTION('center_axis',(-0.913811548620258,0.,0.406138466053447));
#17718=DIRECTION('ref_axis',(-0.406138466053447,0.,-0.913811548620258));
#17719=DIRECTION('',(0.,-1.,0.));
#17720=DIRECTION('',(-0.406138466053447,0.,-0.913811548620257));
#17721=DIRECTION('center_axis',(0.,-1.,0.));
#17722=DIRECTION('ref_axis',(-1.,0.,1.83697019872103E-16));
#17723=DIRECTION('center_axis',(0.,-1.,0.));
#17724=DIRECTION('ref_axis',(1.,0.,0.));
#17725=DIRECTION('center_axis',(0.970453902383945,0.,0.241286600017018));
#17726=DIRECTION('ref_axis',(-0.241286600017018,0.,0.970453902383945));
#17727=DIRECTION('',(0.,1.,0.));
#17728=DIRECTION('',(-0.241286600017018,0.,0.970453902383945));
#17729=DIRECTION('',(0.,-1.,0.));
#17730=DIRECTION('center_axis',(-0.829403493362699,0.,0.558650020314823));
#17731=DIRECTION('ref_axis',(-0.558650020314823,0.,-0.829403493362699));
#17732=DIRECTION('',(0.,-1.,0.));
#17733=DIRECTION('',(-0.558650020314823,0.,-0.829403493362699));
#17734=DIRECTION('center_axis',(0.,-1.,0.));
#17735=DIRECTION('ref_axis',(-0.984807753012208,0.,0.17364817766693));
#17736=DIRECTION('center_axis',(0.,-1.,0.));
#17737=DIRECTION('ref_axis',(1.,0.,0.));
#17738=DIRECTION('center_axis',(0.997609505397066,0.,0.0691033627359814));
#17739=DIRECTION('ref_axis',(-0.0691033627359814,0.,0.997609505397066));
#17740=DIRECTION('',(0.,1.,0.));
#17741=DIRECTION('',(-0.0691033627359814,0.,0.997609505397066));
#17742=DIRECTION('',(0.,-1.,0.));
#17743=DIRECTION('center_axis',(-0.719794432657732,0.,0.694187276399484));
#17744=DIRECTION('ref_axis',(-0.694187276399484,0.,-0.719794432657732));
#17745=DIRECTION('',(0.,-1.,0.));
#17746=DIRECTION('',(-0.694187276399484,0.,-0.719794432657732));
#17747=DIRECTION('center_axis',(0.,-1.,0.));
#17748=DIRECTION('ref_axis',(-0.939692620785908,0.,0.342020143325669));
#17749=DIRECTION('center_axis',(0.,-1.,0.));
#17750=DIRECTION('ref_axis',(1.,0.,0.));
#17751=DIRECTION('center_axis',(0.994453248403465,0.,-0.105179545253799));
#17752=DIRECTION('ref_axis',(0.105179545253799,0.,0.994453248403465));
#17753=DIRECTION('',(0.,1.,0.));
#17754=DIRECTION('',(0.105179545253799,0.,0.994453248403465));
#17755=DIRECTION('',(0.,-1.,0.));
#17756=DIRECTION('center_axis',(-0.588314782350018,0.,0.808632003366458));
#17757=DIRECTION('ref_axis',(-0.808632003366458,0.,-0.588314782350018));
#17758=DIRECTION('',(0.,-1.,0.));
#17759=DIRECTION('',(-0.808632003366458,0.,-0.588314782350018));
#17760=DIRECTION('center_axis',(0.,-1.,0.));
#17761=DIRECTION('ref_axis',(-0.866025403784438,0.,0.5));
#17762=DIRECTION('center_axis',(0.,-1.,0.));
#17763=DIRECTION('ref_axis',(1.,0.,0.));
#17764=DIRECTION('center_axis',(0.961081032674749,0.,-0.27626662598446));
#17765=DIRECTION('ref_axis',(0.27626662598446,0.,0.961081032674749));
#17766=DIRECTION('',(0.,1.,0.));
#17767=DIRECTION('',(0.27626662598446,0.,0.961081032674749));
#17768=DIRECTION('',(0.,-1.,0.));
#17769=DIRECTION('center_axis',(-0.438959485082243,0.,0.898506856098679));
#17770=DIRECTION('ref_axis',(-0.898506856098679,0.,-0.438959485082243));
#17771=DIRECTION('',(0.,-1.,0.));
#17772=DIRECTION('',(-0.898506856098679,0.,-0.438959485082243));
#17773=DIRECTION('center_axis',(0.,-1.,0.));
#17774=DIRECTION('ref_axis',(-0.766044443118978,0.,0.642787609686539));
#17775=DIRECTION('center_axis',(0.,-1.,0.));
#17776=DIRECTION('ref_axis',(1.,0.,0.));
#17777=DIRECTION('center_axis',(0.89850685609868,0.,-0.438959485082242));
#17778=DIRECTION('ref_axis',(0.438959485082242,0.,0.89850685609868));
#17779=DIRECTION('',(0.,1.,0.));
#17780=DIRECTION('',(0.438959485082242,0.,0.89850685609868));
#17781=DIRECTION('',(0.,-1.,0.));
#17782=DIRECTION('center_axis',(-0.276266625984462,0.,0.961081032674749));
#17783=DIRECTION('ref_axis',(-0.961081032674749,0.,-0.276266625984462));
#17784=DIRECTION('',(0.,-1.,0.));
#17785=DIRECTION('',(-0.961081032674749,0.,-0.276266625984462));
#17786=DIRECTION('center_axis',(0.,-1.,0.));
#17787=DIRECTION('ref_axis',(-0.642787609686539,0.,0.766044443118978));
#17788=DIRECTION('center_axis',(0.,-1.,0.));
#17789=DIRECTION('ref_axis',(1.,0.,0.));
#17790=DIRECTION('center_axis',(0.808632003366458,0.,-0.588314782350017));
#17791=DIRECTION('ref_axis',(0.588314782350017,0.,0.808632003366458));
#17792=DIRECTION('',(0.,1.,0.));
#17793=DIRECTION('',(0.588314782350017,0.,0.808632003366458));
#17794=DIRECTION('',(0.,-1.,0.));
#17795=DIRECTION('center_axis',(-0.1051795452538,0.,0.994453248403465));
#17796=DIRECTION('ref_axis',(-0.994453248403465,0.,-0.1051795452538));
#17797=DIRECTION('',(0.,-1.,0.));
#17798=DIRECTION('',(-0.994453248403465,0.,-0.1051795452538));
#17799=DIRECTION('center_axis',(0.,-1.,0.));
#17800=DIRECTION('ref_axis',(-0.5,0.,0.866025403784439));
#17801=DIRECTION('center_axis',(0.,-1.,0.));
#17802=DIRECTION('ref_axis',(1.,0.,0.));
#17803=DIRECTION('center_axis',(0.694187276399485,0.,-0.719794432657731));
#17804=DIRECTION('ref_axis',(0.719794432657731,0.,0.694187276399485));
#17805=DIRECTION('',(0.,1.,0.));
#17806=DIRECTION('',(0.719794432657731,0.,0.694187276399485));
#17807=DIRECTION('',(0.,-1.,0.));
#17808=DIRECTION('center_axis',(0.0691033627359802,0.,0.997609505397066));
#17809=DIRECTION('ref_axis',(-0.997609505397067,0.,0.0691033627359802));
#17810=DIRECTION('',(0.,-1.,0.));
#17811=DIRECTION('',(-0.997609505397066,0.,0.0691033627359802));
#17812=DIRECTION('center_axis',(0.,-1.,0.));
#17813=DIRECTION('ref_axis',(-0.342020143325669,0.,0.939692620785908));
#17814=DIRECTION('center_axis',(0.,-1.,0.));
#17815=DIRECTION('ref_axis',(1.,0.,0.));
#17816=DIRECTION('center_axis',(0.558650020314824,0.,-0.829403493362698));
#17817=DIRECTION('ref_axis',(0.829403493362698,0.,0.558650020314824));
#17818=DIRECTION('',(0.,1.,0.));
#17819=DIRECTION('',(0.829403493362698,0.,0.558650020314824));
#17820=DIRECTION('',(0.,-1.,0.));
#17821=DIRECTION('center_axis',(0.241286600017017,0.,0.970453902383945));
#17822=DIRECTION('ref_axis',(-0.970453902383945,0.,0.241286600017017));
#17823=DIRECTION('',(0.,-1.,0.));
#17824=DIRECTION('',(-0.970453902383945,0.,0.241286600017017));
#17825=DIRECTION('center_axis',(0.,-1.,0.));
#17826=DIRECTION('ref_axis',(-0.17364817766693,0.,0.984807753012208));
#17827=DIRECTION('center_axis',(0.,-1.,0.));
#17828=DIRECTION('ref_axis',(1.,0.,0.));
#17829=DIRECTION('center_axis',(0.406138466053448,0.,-0.913811548620257));
#17830=DIRECTION('ref_axis',(0.913811548620257,0.,0.406138466053448));
#17831=DIRECTION('',(0.,1.,0.));
#17832=DIRECTION('',(0.913811548620257,0.,0.406138466053448));
#17833=DIRECTION('',(0.,-1.,0.));
#17834=DIRECTION('center_axis',(0.406138466053447,0.,0.913811548620258));
#17835=DIRECTION('ref_axis',(-0.913811548620258,0.,0.406138466053447));
#17836=DIRECTION('',(0.,-1.,0.));
#17837=DIRECTION('',(-0.913811548620257,0.,0.406138466053447));
#17838=DIRECTION('center_axis',(0.,-1.,0.));
#17839=DIRECTION('ref_axis',(1.22464679914735E-16,0.,1.));
#17840=DIRECTION('center_axis',(0.,-1.,0.));
#17841=DIRECTION('ref_axis',(1.,0.,0.));
#17842=DIRECTION('center_axis',(0.,-1.,0.));
#17843=DIRECTION('ref_axis',(1.,0.,0.));
#17844=DIRECTION('center_axis',(0.241286600017018,0.,-0.970453902383945));
#17845=DIRECTION('ref_axis',(0.970453902383945,0.,0.241286600017018));
#17846=DIRECTION('',(0.,1.,0.));
#17847=DIRECTION('',(0.970453902383945,0.,0.241286600017018));
#17848=DIRECTION('',(0.,-1.,0.));
#17849=DIRECTION('center_axis',(0.558650020314823,0.,0.829403493362698));
#17850=DIRECTION('ref_axis',(-0.829403493362698,0.,0.558650020314823));
#17851=DIRECTION('',(0.,-1.,0.));
#17852=DIRECTION('',(-0.829403493362698,0.,0.558650020314823));
#17853=DIRECTION('center_axis',(0.,-1.,0.));
#17854=DIRECTION('ref_axis',(0.173648177666931,0.,0.984807753012208));
#17855=DIRECTION('center_axis',(0.,-1.,0.));
#17856=DIRECTION('ref_axis',(1.,0.,0.));
#17857=DIRECTION('center_axis',(0.0691033627359819,0.,-0.997609505397066));
#17858=DIRECTION('ref_axis',(0.997609505397066,0.,0.0691033627359819));
#17859=DIRECTION('',(0.,1.,0.));
#17860=DIRECTION('',(0.997609505397066,0.,0.0691033627359819));
#17861=DIRECTION('',(0.,-1.,0.));
#17862=DIRECTION('center_axis',(0.694187276399484,0.,0.719794432657732));
#17863=DIRECTION('ref_axis',(-0.719794432657732,0.,0.694187276399484));
#17864=DIRECTION('',(0.,-1.,0.));
#17865=DIRECTION('',(-0.719794432657732,0.,0.694187276399484));
#17866=DIRECTION('center_axis',(0.,-1.,0.));
#17867=DIRECTION('ref_axis',(0.342020143325669,0.,0.939692620785908));
#17868=DIRECTION('center_axis',(0.,-1.,0.));
#17869=DIRECTION('ref_axis',(1.,0.,0.));
#17870=DIRECTION('center_axis',(-0.105179545253798,0.,-0.994453248403465));
#17871=DIRECTION('ref_axis',(0.994453248403465,0.,-0.105179545253798));
#17872=DIRECTION('',(0.,1.,0.));
#17873=DIRECTION('',(0.994453248403465,0.,-0.105179545253798));
#17874=DIRECTION('',(0.,-1.,0.));
#17875=DIRECTION('center_axis',(0.808632003366457,0.,0.588314782350019));
#17876=DIRECTION('ref_axis',(-0.588314782350019,0.,0.808632003366457));
#17877=DIRECTION('',(0.,-1.,0.));
#17878=DIRECTION('',(-0.588314782350019,0.,0.808632003366457));
#17879=DIRECTION('center_axis',(0.,-1.,0.));
#17880=DIRECTION('ref_axis',(0.5,0.,0.866025403784439));
#17881=DIRECTION('center_axis',(0.,-1.,0.));
#17882=DIRECTION('ref_axis',(1.,0.,0.));
#17883=DIRECTION('center_axis',(-0.27626662598446,0.,-0.961081032674749));
#17884=DIRECTION('ref_axis',(0.961081032674749,0.,-0.27626662598446));
#17885=DIRECTION('',(0.,1.,0.));
#17886=DIRECTION('',(0.961081032674749,0.,-0.27626662598446));
#17887=DIRECTION('',(0.,-1.,0.));
#17888=DIRECTION('center_axis',(0.898506856098679,0.,0.438959485082243));
#17889=DIRECTION('ref_axis',(-0.438959485082243,0.,0.898506856098679));
#17890=DIRECTION('',(0.,-1.,0.));
#17891=DIRECTION('',(-0.438959485082243,0.,0.898506856098679));
#17892=DIRECTION('center_axis',(0.,-1.,0.));
#17893=DIRECTION('ref_axis',(0.642787609686539,0.,0.766044443118978));
#17894=DIRECTION('center_axis',(0.,-1.,0.));
#17895=DIRECTION('ref_axis',(1.,0.,0.));
#17896=DIRECTION('center_axis',(-0.438959485082242,0.,-0.89850685609868));
#17897=DIRECTION('ref_axis',(0.89850685609868,0.,-0.438959485082242));
#17898=DIRECTION('',(0.,1.,0.));
#17899=DIRECTION('',(0.89850685609868,0.,-0.438959485082242));
#17900=DIRECTION('',(0.,-1.,0.));
#17901=DIRECTION('center_axis',(0.961081032674749,0.,0.276266625984462));
#17902=DIRECTION('ref_axis',(-0.276266625984462,0.,0.961081032674749));
#17903=DIRECTION('',(0.,-1.,0.));
#17904=DIRECTION('',(-0.276266625984462,0.,0.961081032674749));
#17905=DIRECTION('center_axis',(0.,-1.,0.));
#17906=DIRECTION('ref_axis',(0.766044443118978,0.,0.642787609686539));
#17907=DIRECTION('center_axis',(0.,-1.,0.));
#17908=DIRECTION('ref_axis',(1.,0.,0.));
#17909=DIRECTION('center_axis',(-0.588314782350017,0.,-0.808632003366458));
#17910=DIRECTION('ref_axis',(0.808632003366458,0.,-0.588314782350017));
#17911=DIRECTION('',(0.,1.,0.));
#17912=DIRECTION('',(0.808632003366458,0.,-0.588314782350017));
#17913=DIRECTION('',(0.,-1.,0.));
#17914=DIRECTION('center_axis',(0.994453248403465,0.,0.1051795452538));
#17915=DIRECTION('ref_axis',(-0.1051795452538,0.,0.994453248403465));
#17916=DIRECTION('',(0.,-1.,0.));
#17917=DIRECTION('',(-0.1051795452538,0.,0.994453248403465));
#17918=DIRECTION('center_axis',(0.,-1.,0.));
#17919=DIRECTION('ref_axis',(0.866025403784439,0.,0.5));
#17920=DIRECTION('center_axis',(0.,-1.,0.));
#17921=DIRECTION('ref_axis',(1.,0.,0.));
#17922=DIRECTION('center_axis',(-0.719794432657731,0.,-0.694187276399485));
#17923=DIRECTION('ref_axis',(0.694187276399485,0.,-0.719794432657731));
#17924=DIRECTION('',(0.,1.,0.));
#17925=DIRECTION('',(0.694187276399485,0.,-0.719794432657731));
#17926=DIRECTION('',(0.,-1.,0.));
#17927=DIRECTION('center_axis',(0.997609505397066,0.,-0.0691033627359801));
#17928=DIRECTION('ref_axis',(0.0691033627359801,0.,0.997609505397067));
#17929=DIRECTION('',(0.,-1.,0.));
#17930=DIRECTION('',(0.0691033627359801,0.,0.997609505397066));
#17931=DIRECTION('center_axis',(0.,-1.,0.));
#17932=DIRECTION('ref_axis',(0.939692620785908,0.,0.342020143325669));
#17933=DIRECTION('center_axis',(0.,-1.,0.));
#17934=DIRECTION('ref_axis',(1.,0.,0.));
#17935=DIRECTION('center_axis',(-0.829403493362697,0.,-0.558650020314825));
#17936=DIRECTION('ref_axis',(0.558650020314825,0.,-0.829403493362697));
#17937=DIRECTION('',(0.,1.,0.));
#17938=DIRECTION('',(0.558650020314825,0.,-0.829403493362697));
#17939=DIRECTION('',(0.,-1.,0.));
#17940=DIRECTION('center_axis',(0.970453902383946,0.,-0.241286600017016));
#17941=DIRECTION('ref_axis',(0.241286600017016,0.,0.970453902383946));
#17942=DIRECTION('',(0.,-1.,0.));
#17943=DIRECTION('',(0.241286600017016,0.,0.970453902383946));
#17944=DIRECTION('center_axis',(0.,-1.,0.));
#17945=DIRECTION('ref_axis',(0.984807753012208,0.,0.17364817766693));
#17946=DIRECTION('center_axis',(0.,-1.,0.));
#17947=DIRECTION('ref_axis',(1.,0.,0.));
#17948=DIRECTION('center_axis',(-0.913811548620257,0.,-0.406138466053448));
#17949=DIRECTION('ref_axis',(0.406138466053448,0.,-0.913811548620257));
#17950=DIRECTION('',(0.,1.,0.));
#17951=DIRECTION('',(0.406138466053448,0.,-0.913811548620257));
#17952=DIRECTION('',(0.,-1.,0.));
#17953=DIRECTION('center_axis',(0.913811548620258,0.,-0.406138466053447));
#17954=DIRECTION('ref_axis',(0.406138466053447,0.,0.913811548620258));
#17955=DIRECTION('',(0.,-1.,0.));
#17956=DIRECTION('',(0.406138466053447,0.,0.913811548620257));
#17957=DIRECTION('center_axis',(0.,-1.,0.));
#17958=DIRECTION('ref_axis',(1.,0.,-6.12323399573677E-17));
#17959=DIRECTION('center_axis',(0.,-1.,0.));
#17960=DIRECTION('ref_axis',(1.,0.,0.));
#17961=DIRECTION('center_axis',(-0.970453902383945,0.,-0.241286600017018));
#17962=DIRECTION('ref_axis',(0.241286600017018,0.,-0.970453902383945));
#17963=DIRECTION('',(0.,1.,0.));
#17964=DIRECTION('',(0.241286600017018,0.,-0.970453902383945));
#17965=DIRECTION('',(0.,-1.,0.));
#17966=DIRECTION('center_axis',(0.829403493362699,0.,-0.558650020314823));
#17967=DIRECTION('ref_axis',(0.558650020314823,0.,0.829403493362699));
#17968=DIRECTION('',(0.,-1.,0.));
#17969=DIRECTION('',(0.558650020314823,0.,0.829403493362699));
#17970=DIRECTION('center_axis',(0.,-1.,0.));
#17971=DIRECTION('ref_axis',(0.984807753012208,0.,-0.17364817766693));
#17972=DIRECTION('center_axis',(0.,-1.,0.));
#17973=DIRECTION('ref_axis',(1.,0.,0.));
#17974=DIRECTION('center_axis',(-0.997609505397066,0.,-0.069103362735982));
#17975=DIRECTION('ref_axis',(0.069103362735982,0.,-0.997609505397066));
#17976=DIRECTION('',(0.,1.,0.));
#17977=DIRECTION('',(0.069103362735982,0.,-0.997609505397066));
#17978=DIRECTION('',(0.,-1.,0.));
#17979=DIRECTION('center_axis',(0.719794432657732,0.,-0.694187276399484));
#17980=DIRECTION('ref_axis',(0.694187276399484,0.,0.719794432657732));
#17981=DIRECTION('',(0.,-1.,0.));
#17982=DIRECTION('',(0.694187276399484,0.,0.719794432657732));
#17983=DIRECTION('center_axis',(0.,-1.,0.));
#17984=DIRECTION('ref_axis',(0.939692620785908,0.,-0.342020143325669));
#17985=DIRECTION('center_axis',(0.,-1.,0.));
#17986=DIRECTION('ref_axis',(1.,0.,0.));
#17987=DIRECTION('center_axis',(-0.994453248403465,0.,0.105179545253798));
#17988=DIRECTION('ref_axis',(-0.105179545253798,0.,-0.994453248403465));
#17989=DIRECTION('',(0.,1.,0.));
#17990=DIRECTION('',(-0.105179545253798,0.,-0.994453248403465));
#17991=DIRECTION('',(0.,-1.,0.));
#17992=DIRECTION('center_axis',(0.588314782350018,0.,-0.808632003366458));
#17993=DIRECTION('ref_axis',(0.808632003366458,0.,0.588314782350018));
#17994=DIRECTION('',(0.,-1.,0.));
#17995=DIRECTION('',(0.808632003366457,0.,0.588314782350018));
#17996=DIRECTION('center_axis',(0.,-1.,0.));
#17997=DIRECTION('ref_axis',(0.866025403784439,0.,-0.5));
#17998=DIRECTION('center_axis',(0.,-1.,0.));
#17999=DIRECTION('ref_axis',(1.,0.,0.));
#18000=DIRECTION('center_axis',(-0.961081032674749,0.,0.27626662598446));
#18001=DIRECTION('ref_axis',(-0.27626662598446,0.,-0.961081032674749));
#18002=DIRECTION('',(0.,1.,0.));
#18003=DIRECTION('',(-0.27626662598446,0.,-0.961081032674749));
#18004=DIRECTION('',(0.,-1.,0.));
#18005=DIRECTION('center_axis',(0.438959485082244,0.,-0.898506856098679));
#18006=DIRECTION('ref_axis',(0.898506856098679,0.,0.438959485082244));
#18007=DIRECTION('',(0.,-1.,0.));
#18008=DIRECTION('',(0.898506856098678,0.,0.438959485082244));
#18009=DIRECTION('center_axis',(0.,-1.,0.));
#18010=DIRECTION('ref_axis',(0.766044443118978,0.,-0.642787609686539));
#18011=DIRECTION('center_axis',(0.,-1.,0.));
#18012=DIRECTION('ref_axis',(1.,0.,0.));
#18013=DIRECTION('center_axis',(-0.89850685609868,0.,0.438959485082242));
#18014=DIRECTION('ref_axis',(-0.438959485082242,0.,-0.89850685609868));
#18015=DIRECTION('',(0.,1.,0.));
#18016=DIRECTION('',(-0.438959485082242,0.,-0.89850685609868));
#18017=DIRECTION('',(0.,-1.,0.));
#18018=DIRECTION('center_axis',(0.276266625984462,0.,-0.961081032674749));
#18019=DIRECTION('ref_axis',(0.961081032674749,0.,0.276266625984462));
#18020=DIRECTION('',(0.,-1.,0.));
#18021=DIRECTION('',(0.961081032674749,0.,0.276266625984462));
#18022=DIRECTION('center_axis',(0.,-1.,0.));
#18023=DIRECTION('ref_axis',(0.642787609686539,0.,-0.766044443118978));
#18024=DIRECTION('center_axis',(0.,-1.,0.));
#18025=DIRECTION('ref_axis',(1.,0.,0.));
#18026=DIRECTION('center_axis',(-0.808632003366459,0.,0.588314782350017));
#18027=DIRECTION('ref_axis',(-0.588314782350017,0.,-0.808632003366459));
#18028=DIRECTION('',(0.,1.,0.));
#18029=DIRECTION('',(-0.588314782350017,0.,-0.808632003366458));
#18030=DIRECTION('',(0.,-1.,0.));
#18031=DIRECTION('center_axis',(0.1051795452538,0.,-0.994453248403465));
#18032=DIRECTION('ref_axis',(0.994453248403465,0.,0.1051795452538));
#18033=DIRECTION('',(0.,-1.,0.));
#18034=DIRECTION('',(0.994453248403465,0.,0.1051795452538));
#18035=DIRECTION('center_axis',(0.,-1.,0.));
#18036=DIRECTION('ref_axis',(0.5,0.,-0.866025403784439));
#18037=DIRECTION('center_axis',(0.,-1.,0.));
#18038=DIRECTION('ref_axis',(1.,0.,0.));
#18039=DIRECTION('center_axis',(-0.694187276399485,0.,0.719794432657731));
#18040=DIRECTION('ref_axis',(-0.719794432657731,0.,-0.694187276399485));
#18041=DIRECTION('',(0.,1.,0.));
#18042=DIRECTION('',(-0.719794432657731,0.,-0.694187276399485));
#18043=DIRECTION('',(0.,-1.,0.));
#18044=DIRECTION('center_axis',(-0.0691033627359801,0.,-0.997609505397066));
#18045=DIRECTION('ref_axis',(0.997609505397067,0.,-0.0691033627359801));
#18046=DIRECTION('',(0.,-1.,0.));
#18047=DIRECTION('',(0.997609505397066,0.,-0.0691033627359801));
#18048=DIRECTION('center_axis',(0.,-1.,0.));
#18049=DIRECTION('ref_axis',(0.342020143325669,0.,-0.939692620785908));
#18050=DIRECTION('center_axis',(0.,-1.,0.));
#18051=DIRECTION('ref_axis',(1.,0.,0.));
#18052=DIRECTION('center_axis',(-0.558650020314825,0.,0.829403493362697));
#18053=DIRECTION('ref_axis',(-0.829403493362697,0.,-0.558650020314825));
#18054=DIRECTION('',(0.,1.,0.));
#18055=DIRECTION('',(-0.829403493362697,0.,-0.558650020314825));
#18056=DIRECTION('',(0.,-1.,0.));
#18057=DIRECTION('center_axis',(-0.241286600017016,0.,-0.970453902383946));
#18058=DIRECTION('ref_axis',(0.970453902383946,0.,-0.241286600017016));
#18059=DIRECTION('',(0.,-1.,0.));
#18060=DIRECTION('',(0.970453902383946,0.,-0.241286600017016));
#18061=DIRECTION('center_axis',(0.,-1.,0.));
#18062=DIRECTION('ref_axis',(0.17364817766693,0.,-0.984807753012208));
#18063=DIRECTION('center_axis',(0.,-1.,0.));
#18064=DIRECTION('ref_axis',(1.,0.,0.));
#18065=DIRECTION('center_axis',(-0.406138466053448,0.,0.913811548620257));
#18066=DIRECTION('ref_axis',(-0.913811548620257,0.,-0.406138466053448));
#18067=DIRECTION('',(0.,1.,0.));
#18068=DIRECTION('',(-0.913811548620257,0.,-0.406138466053448));
#18069=DIRECTION('',(0.,-1.,0.));
#18070=DIRECTION('center_axis',(-0.406138466053447,0.,-0.913811548620258));
#18071=DIRECTION('ref_axis',(0.913811548620258,0.,-0.406138466053447));
#18072=DIRECTION('',(0.,-1.,0.));
#18073=DIRECTION('',(0.913811548620257,0.,-0.406138466053447));
#18074=DIRECTION('center_axis',(0.,-1.,0.));
#18075=DIRECTION('ref_axis',(0.,0.,-1.));
#18076=DIRECTION('center_axis',(0.,-1.,0.));
#18077=DIRECTION('ref_axis',(1.,0.,0.));
#18078=DIRECTION('center_axis',(0.,1.,0.));
#18079=DIRECTION('ref_axis',(1.,0.,0.));
#18080=DIRECTION('',(0.,-1.,0.));
#18081=DIRECTION('center_axis',(0.,1.,0.));
#18082=DIRECTION('ref_axis',(1.,0.,0.));
#18083=DIRECTION('',(0.499999999999999,0.,-0.866025403784439));
#18084=DIRECTION('',(1.,0.,0.));
#18085=DIRECTION('',(0.5,0.,0.866025403784438));
#18086=DIRECTION('',(-0.5,0.,0.866025403784439));
#18087=DIRECTION('',(-1.,0.,0.));
#18088=DIRECTION('',(-0.500000000000001,0.,-0.866025403784438));
#18089=DIRECTION('center_axis',(0.,1.,0.));
#18090=DIRECTION('ref_axis',(0.,0.,1.));
#18091=DIRECTION('',(0.499999999999999,0.,-0.866025403784439));
#18092=DIRECTION('center_axis',(0.,-1.,0.));
#18093=DIRECTION('ref_axis',(1.,0.,0.));
#18094=DIRECTION('center_axis',(0.,1.,0.));
#18095=DIRECTION('ref_axis',(0.,0.,1.));
#18096=DIRECTION('',(1.,0.,0.));
#18097=DIRECTION('center_axis',(0.,-1.,0.));
#18098=DIRECTION('ref_axis',(1.,0.,0.));
#18099=DIRECTION('center_axis',(0.,1.,0.));
#18100=DIRECTION('ref_axis',(0.,0.,1.));
#18101=DIRECTION('',(0.5,0.,0.866025403784438));
#18102=DIRECTION('center_axis',(0.,-1.,0.));
#18103=DIRECTION('ref_axis',(1.,0.,0.));
#18104=DIRECTION('center_axis',(0.,1.,0.));
#18105=DIRECTION('ref_axis',(0.,0.,1.));
#18106=DIRECTION('',(-0.5,0.,0.866025403784439));
#18107=DIRECTION('center_axis',(0.,-1.,0.));
#18108=DIRECTION('ref_axis',(1.,0.,0.));
#18109=DIRECTION('center_axis',(0.,1.,0.));
#18110=DIRECTION('ref_axis',(0.,0.,1.));
#18111=DIRECTION('',(-1.,0.,0.));
#18112=DIRECTION('center_axis',(0.,-1.,0.));
#18113=DIRECTION('ref_axis',(1.,0.,0.));
#18114=DIRECTION('center_axis',(0.,1.,0.));
#18115=DIRECTION('ref_axis',(0.,0.,1.));
#18116=DIRECTION('',(-0.500000000000001,0.,-0.866025403784438));
#18117=DIRECTION('center_axis',(0.,-1.,0.));
#18118=DIRECTION('ref_axis',(1.,0.,0.));
#18119=DIRECTION('center_axis',(0.,1.,0.));
#18120=DIRECTION('ref_axis',(1.,0.,0.));
#18121=DIRECTION('',(-0.85716730070211,0.515038074910058,1.04972719113862E-16));
#18122=DIRECTION('center_axis',(-0.866025403784439,0.,-0.499999999999999));
#18123=DIRECTION('ref_axis',(0.499999999999999,0.,-0.866025403784439));
#18124=DIRECTION('',(0.,-1.,0.));
#18125=DIRECTION('',(0.,-1.,0.));
#18126=DIRECTION('center_axis',(-0.866025403784438,0.,0.500000000000001));
#18127=DIRECTION('ref_axis',(-0.500000000000001,0.,-0.866025403784438));
#18128=DIRECTION('',(0.,-1.,0.));
#18129=DIRECTION('center_axis',(0.,0.,1.));
#18130=DIRECTION('ref_axis',(-1.,0.,0.));
#18131=DIRECTION('',(0.,-1.,0.));
#18132=DIRECTION('center_axis',(0.866025403784439,0.,0.5));
#18133=DIRECTION('ref_axis',(-0.5,0.,0.866025403784439));
#18134=DIRECTION('',(0.,-1.,0.));
#18135=DIRECTION('center_axis',(0.866025403784439,0.,-0.5));
#18136=DIRECTION('ref_axis',(0.5,0.,0.866025403784439));
#18137=DIRECTION('',(0.,-1.,0.));
#18138=DIRECTION('center_axis',(0.,0.,-1.));
#18139=DIRECTION('ref_axis',(1.,0.,0.));
#18140=DIRECTION('',(0.,0.,1.));
#18141=DIRECTION('',(1.,0.,0.));
#18142=DIRECTION('',(0.,0.,1.));
#18143=DIRECTION('',(1.,0.,0.));
#18144=DIRECTION('',(0.,0.,1.));
#18145=DIRECTION('',(1.,0.,0.));
#18146=DIRECTION('',(0.,0.,1.));
#18147=DIRECTION('',(1.,0.,0.));
#18148=DIRECTION('',(0.,0.,1.));
#18149=DIRECTION('',(1.,0.,0.));
#18150=DIRECTION('',(0.,0.,1.));
#18151=DIRECTION('',(1.,0.,0.));
#18152=DIRECTION('',(0.,0.,1.));
#18153=DIRECTION('',(1.,0.,0.));
#18154=DIRECTION('',(0.,0.,1.));
#18155=DIRECTION('',(1.,0.,0.));
#18156=DIRECTION('',(0.,0.,1.));
#18157=DIRECTION('',(1.,0.,0.));
#18158=DIRECTION('',(0.,-0.707106781186548,0.707106781186547));
#18159=DIRECTION('',(1.,0.,0.));
#18160=DIRECTION('',(1.22464679914735E-16,0.,-1.));
#18161=DIRECTION('',(-1.,0.,-1.22464679914735E-16));
#18162=DIRECTION('',(0.,0.,1.));
#18163=DIRECTION('',(1.,0.,0.));
#18164=DIRECTION('',(1.22464679914735E-16,0.,-1.));
#18165=DIRECTION('',(-1.,0.,-1.22464679914735E-16));
#18166=DIRECTION('',(1.22464679914735E-16,0.,-1.));
#18167=DIRECTION('',(-1.,0.,-1.22464679914735E-16));
#18168=DIRECTION('',(0.,0.,1.));
#18169=DIRECTION('',(1.,0.,0.));
#18170=DIRECTION('',(1.22464679914735E-16,0.,-1.));
#18171=DIRECTION('',(-1.,0.,-1.22464679914735E-16));
#18172=DIRECTION('',(1.22464679914735E-16,0.,-1.));
#18173=DIRECTION('',(-1.,0.,-1.22464679914735E-16));
#18174=DIRECTION('',(0.,0.,1.));
#18175=DIRECTION('',(1.,0.,0.));
#18176=DIRECTION('',(1.22464679914735E-16,0.,-1.));
#18177=DIRECTION('',(-1.,0.,-1.22464679914735E-16));
#18178=DIRECTION('',(1.22464679914735E-16,0.,-1.));
#18179=DIRECTION('',(-1.,0.,-1.22464679914735E-16));
#18180=DIRECTION('',(0.,0.,1.));
#18181=DIRECTION('',(1.,0.,0.));
#18182=DIRECTION('',(0.,0.,1.));
#18183=DIRECTION('',(1.,0.,0.));
#18184=DIRECTION('',(0.,0.,1.));
#18185=DIRECTION('',(1.,0.,0.));
#18186=DIRECTION('',(0.,0.,1.));
#18187=DIRECTION('',(1.,0.,0.));
#18188=DIRECTION('',(0.,0.,1.));
#18189=DIRECTION('',(1.,0.,0.));
#18190=DIRECTION('',(0.,0.,1.));
#18191=DIRECTION('',(1.,0.,0.));
#18192=DIRECTION('',(0.,0.,1.));
#18193=DIRECTION('',(1.,0.,0.));
#18194=DIRECTION('',(0.,0.866025403784439,0.5));
#18195=DIRECTION('',(1.,0.,0.));
#18196=DIRECTION('',(0.,0.866025403784439,0.5));
#18197=DIRECTION('',(1.,0.,0.));
#18198=DIRECTION('',(0.,0.866025403784439,0.5));
#18199=DIRECTION('',(1.,0.,0.));
#18200=DIRECTION('',(0.,0.866025403784439,0.5));
#18201=DIRECTION('',(1.,0.,0.));
#18202=DIRECTION('',(0.,0.866025403784439,0.5));
#18203=DIRECTION('',(1.,0.,0.));
#18204=DIRECTION('',(0.,0.866025403784439,0.5));
#18205=DIRECTION('',(1.,0.,0.));
#18206=DIRECTION('',(0.,0.866025403784439,0.5));
#18207=DIRECTION('',(1.,0.,0.));
#18208=DIRECTION('',(0.,0.866025403784439,0.5));
#18209=DIRECTION('',(1.,0.,0.));
#18210=DIRECTION('',(0.,0.866025403784438,-0.5));
#18211=DIRECTION('',(1.,0.,0.));
#18212=DIRECTION('',(0.,0.866025403784438,-0.5));
#18213=DIRECTION('',(1.,0.,0.));
#18214=DIRECTION('',(0.,0.866025403784438,-0.5));
#18215=DIRECTION('',(1.,0.,0.));
#18216=DIRECTION('',(0.,0.866025403784438,-0.5));
#18217=DIRECTION('',(1.,0.,0.));
#18218=DIRECTION('',(0.,0.866025403784438,-0.5));
#18219=DIRECTION('',(1.,0.,0.));
#18220=DIRECTION('',(0.,0.866025403784438,-0.5));
#18221=DIRECTION('',(1.,0.,0.));
#18222=DIRECTION('',(0.,0.866025403784438,-0.5));
#18223=DIRECTION('',(1.,0.,0.));
#18224=DIRECTION('',(0.,0.866025403784438,-0.5));
#18225=DIRECTION('',(1.,0.,0.));
#18226=DIRECTION('',(0.,-1.22464679914735E-16,-1.));
#18227=DIRECTION('',(1.,0.,0.));
#18228=DIRECTION('',(0.,-1.22464679914735E-16,-1.));
#18229=DIRECTION('',(1.,0.,0.));
#18230=DIRECTION('',(0.,-1.22464679914735E-16,-1.));
#18231=DIRECTION('',(1.,0.,0.));
#18232=DIRECTION('',(0.,-1.22464679914735E-16,-1.));
#18233=DIRECTION('',(1.,0.,0.));
#18234=DIRECTION('',(0.,-1.22464679914735E-16,-1.));
#18235=DIRECTION('',(1.,0.,0.));
#18236=DIRECTION('',(0.,-1.22464679914735E-16,-1.));
#18237=DIRECTION('',(1.,0.,0.));
#18238=DIRECTION('',(0.,-1.22464679914735E-16,-1.));
#18239=DIRECTION('',(1.,0.,0.));
#18240=DIRECTION('',(0.,-1.22464679914735E-16,-1.));
#18241=DIRECTION('',(1.,0.,0.));
#18242=DIRECTION('',(0.,-0.866025403784439,-0.5));
#18243=DIRECTION('',(1.,0.,0.));
#18244=DIRECTION('',(0.,-0.866025403784439,-0.5));
#18245=DIRECTION('',(1.,0.,0.));
#18246=DIRECTION('',(0.,-0.866025403784439,-0.5));
#18247=DIRECTION('',(1.,0.,0.));
#18248=DIRECTION('',(0.,-0.866025403784439,-0.5));
#18249=DIRECTION('',(1.,0.,0.));
#18250=DIRECTION('',(0.,-0.866025403784439,-0.5));
#18251=DIRECTION('',(1.,0.,0.));
#18252=DIRECTION('',(0.,-0.866025403784439,-0.5));
#18253=DIRECTION('',(1.,0.,0.));
#18254=DIRECTION('',(0.,-0.866025403784439,-0.5));
#18255=DIRECTION('',(1.,0.,0.));
#18256=DIRECTION('',(0.,-0.866025403784439,-0.5));
#18257=DIRECTION('',(1.,0.,0.));
#18258=DIRECTION('',(0.,0.,1.));
#18259=DIRECTION('',(1.,0.,0.));
#18260=DIRECTION('',(0.,0.,1.));
#18261=DIRECTION('',(1.,0.,0.));
#18262=DIRECTION('',(0.,0.,1.));
#18263=DIRECTION('',(1.,0.,0.));
#18264=DIRECTION('',(0.,0.,1.));
#18265=DIRECTION('',(1.,0.,0.));
#18266=DIRECTION('',(0.,0.,1.));
#18267=DIRECTION('',(1.,0.,0.));
#18268=DIRECTION('',(0.,0.,1.));
#18269=DIRECTION('',(1.,0.,0.));
#18270=DIRECTION('',(0.,0.,1.));
#18271=DIRECTION('',(1.,0.,0.));
#18272=DIRECTION('',(0.,0.,1.));
#18273=DIRECTION('',(1.,0.,0.));
#18274=DIRECTION('',(0.,0.866025403784439,0.5));
#18275=DIRECTION('',(1.,0.,0.));
#18276=DIRECTION('',(0.,0.866025403784439,0.5));
#18277=DIRECTION('',(1.,0.,0.));
#18278=DIRECTION('',(0.,0.866025403784439,0.5));
#18279=DIRECTION('',(1.,0.,0.));
#18280=DIRECTION('',(0.,0.866025403784439,0.5));
#18281=DIRECTION('',(1.,0.,0.));
#18282=DIRECTION('',(0.,0.866025403784439,0.5));
#18283=DIRECTION('',(1.,0.,0.));
#18284=DIRECTION('',(0.,0.866025403784439,0.5));
#18285=DIRECTION('',(1.,0.,0.));
#18286=DIRECTION('',(0.,0.866025403784439,0.5));
#18287=DIRECTION('',(1.,0.,0.));
#18288=DIRECTION('',(0.,0.866025403784439,0.5));
#18289=DIRECTION('',(1.,0.,0.));
#18290=DIRECTION('',(0.,0.866025403784438,-0.5));
#18291=DIRECTION('',(1.,0.,0.));
#18292=DIRECTION('',(0.,0.866025403784438,-0.5));
#18293=DIRECTION('',(1.,0.,0.));
#18294=DIRECTION('',(0.,0.866025403784438,-0.5));
#18295=DIRECTION('',(1.,0.,0.));
#18296=DIRECTION('',(0.,0.866025403784438,-0.5));
#18297=DIRECTION('',(1.,0.,0.));
#18298=DIRECTION('',(0.,0.866025403784438,-0.5));
#18299=DIRECTION('',(1.,0.,0.));
#18300=DIRECTION('',(0.,0.866025403784438,-0.5));
#18301=DIRECTION('',(1.,0.,0.));
#18302=DIRECTION('',(0.,0.866025403784438,-0.5));
#18303=DIRECTION('',(1.,0.,0.));
#18304=DIRECTION('',(0.,0.866025403784438,-0.5));
#18305=DIRECTION('',(1.,0.,0.));
#18306=DIRECTION('',(0.,-1.22464679914735E-16,-1.));
#18307=DIRECTION('',(1.,0.,0.));
#18308=DIRECTION('',(0.,-1.22464679914735E-16,-1.));
#18309=DIRECTION('',(1.,0.,0.));
#18310=DIRECTION('',(0.,-1.22464679914735E-16,-1.));
#18311=DIRECTION('',(1.,0.,0.));
#18312=DIRECTION('',(0.,-1.22464679914735E-16,-1.));
#18313=DIRECTION('',(1.,0.,0.));
#18314=DIRECTION('',(0.,-1.22464679914735E-16,-1.));
#18315=DIRECTION('',(1.,0.,0.));
#18316=DIRECTION('',(0.,-1.22464679914735E-16,-1.));
#18317=DIRECTION('',(1.,0.,0.));
#18318=DIRECTION('',(0.,-1.22464679914735E-16,-1.));
#18319=DIRECTION('',(1.,0.,0.));
#18320=DIRECTION('',(0.,-1.22464679914735E-16,-1.));
#18321=DIRECTION('',(1.,0.,0.));
#18322=DIRECTION('',(0.,-0.866025403784439,-0.5));
#18323=DIRECTION('',(1.,0.,0.));
#18324=DIRECTION('',(0.,-0.866025403784439,-0.5));
#18325=DIRECTION('',(1.,0.,0.));
#18326=DIRECTION('',(0.,-0.866025403784439,-0.5));
#18327=DIRECTION('',(1.,0.,0.));
#18328=DIRECTION('',(0.,-0.866025403784439,-0.5));
#18329=DIRECTION('',(1.,0.,0.));
#18330=DIRECTION('',(0.,-0.866025403784439,-0.5));
#18331=DIRECTION('',(1.,0.,0.));
#18332=DIRECTION('',(0.,-0.866025403784439,-0.5));
#18333=DIRECTION('',(1.,0.,0.));
#18334=DIRECTION('',(0.,-0.866025403784439,-0.5));
#18335=DIRECTION('',(1.,0.,0.));
#18336=DIRECTION('',(0.,-0.866025403784439,-0.5));
#18337=DIRECTION('',(1.,0.,0.));
#18338=DIRECTION('',(1.22464679914735E-16,0.,-1.));
#18339=DIRECTION('',(-1.,0.,-1.22464679914735E-16));
#18340=DIRECTION('',(1.22464679914735E-16,0.,-1.));
#18341=DIRECTION('',(-1.,0.,-1.22464679914735E-16));
#18342=DIRECTION('',(1.22464679914735E-16,0.,-1.));
#18343=DIRECTION('',(-1.,0.,-1.22464679914735E-16));
#18344=DIRECTION('',(1.22464679914735E-16,0.,-1.));
#18345=DIRECTION('',(-1.,0.,-1.22464679914735E-16));
#18346=DIRECTION('',(1.22464679914735E-16,0.,-1.));
#18347=DIRECTION('',(-1.,0.,-1.22464679914735E-16));
#18348=DIRECTION('',(1.22464679914735E-16,0.,-1.));
#18349=DIRECTION('',(-1.,0.,-1.22464679914735E-16));
#18350=DIRECTION('',(1.22464679914735E-16,0.,-1.));
#18351=DIRECTION('',(-1.,0.,-1.22464679914735E-16));
#18352=DIRECTION('',(1.22464679914735E-16,0.,-1.));
#18353=DIRECTION('',(-1.,0.,-1.22464679914735E-16));
#18354=DIRECTION('',(6.12323399573677E-17,0.866025403784439,-0.5));
#18355=DIRECTION('',(-1.,1.72655894117776E-31,-1.22464679914735E-16));
#18356=DIRECTION('',(6.12323399573677E-17,0.866025403784439,-0.5));
#18357=DIRECTION('',(-1.,1.72655894117776E-31,-1.22464679914735E-16));
#18358=DIRECTION('',(6.12323399573677E-17,0.866025403784439,-0.5));
#18359=DIRECTION('',(-1.,1.72655894117776E-31,-1.22464679914735E-16));
#18360=DIRECTION('',(6.12323399573677E-17,0.866025403784439,-0.5));
#18361=DIRECTION('',(-1.,1.72655894117776E-31,-1.22464679914735E-16));
#18362=DIRECTION('',(6.12323399573677E-17,0.866025403784439,-0.5));
#18363=DIRECTION('',(-1.,1.72655894117776E-31,-1.22464679914735E-16));
#18364=DIRECTION('',(6.12323399573677E-17,0.866025403784439,-0.5));
#18365=DIRECTION('',(-1.,1.72655894117776E-31,-1.22464679914735E-16));
#18366=DIRECTION('',(6.12323399573677E-17,0.866025403784439,-0.5));
#18367=DIRECTION('',(-1.,1.72655894117776E-31,-1.22464679914735E-16));
#18368=DIRECTION('',(6.12323399573677E-17,0.866025403784439,-0.5));
#18369=DIRECTION('',(-1.,1.72655894117776E-31,-1.22464679914735E-16));
#18370=DIRECTION('',(-6.12323399573677E-17,0.866025403784438,0.5));
#18371=DIRECTION('',(-1.,-1.64144897904239E-31,-1.22464679914735E-16));
#18372=DIRECTION('',(-6.12323399573677E-17,0.866025403784438,0.5));
#18373=DIRECTION('',(-1.,-1.64144897904239E-31,-1.22464679914735E-16));
#18374=DIRECTION('',(-6.12323399573677E-17,0.866025403784438,0.5));
#18375=DIRECTION('',(-1.,-1.64144897904239E-31,-1.22464679914735E-16));
#18376=DIRECTION('',(-6.12323399573677E-17,0.866025403784438,0.5));
#18377=DIRECTION('',(-1.,-1.64144897904239E-31,-1.22464679914735E-16));
#18378=DIRECTION('',(-6.12323399573677E-17,0.866025403784438,0.5));
#18379=DIRECTION('',(-1.,-1.64144897904239E-31,-1.22464679914735E-16));
#18380=DIRECTION('',(-6.12323399573677E-17,0.866025403784438,0.5));
#18381=DIRECTION('',(-1.,-1.64144897904239E-31,-1.22464679914735E-16));
#18382=DIRECTION('',(-6.12323399573677E-17,0.866025403784438,0.5));
#18383=DIRECTION('',(-1.,-1.64144897904239E-31,-1.22464679914735E-16));
#18384=DIRECTION('',(-6.12323399573677E-17,0.866025403784438,0.5));
#18385=DIRECTION('',(-1.,-1.64144897904239E-31,-1.22464679914735E-16));
#18386=DIRECTION('',(-1.22464679914735E-16,-1.22464679914735E-16,1.));
#18387=DIRECTION('',(-1.,-1.258548236767E-48,-1.22464679914735E-16));
#18388=DIRECTION('',(-1.22464679914735E-16,-1.22464679914735E-16,1.));
#18389=DIRECTION('',(-1.,-1.258548236767E-48,-1.22464679914735E-16));
#18390=DIRECTION('',(-1.22464679914735E-16,-1.22464679914735E-16,1.));
#18391=DIRECTION('',(-1.,-1.258548236767E-48,-1.22464679914735E-16));
#18392=DIRECTION('',(-1.22464679914735E-16,-1.22464679914735E-16,1.));
#18393=DIRECTION('',(-1.,-1.258548236767E-48,-1.22464679914735E-16));
#18394=DIRECTION('',(-1.22464679914735E-16,-1.22464679914735E-16,1.));
#18395=DIRECTION('',(-1.,-1.258548236767E-48,-1.22464679914735E-16));
#18396=DIRECTION('',(-1.22464679914735E-16,-1.22464679914735E-16,1.));
#18397=DIRECTION('',(-1.,-1.258548236767E-48,-1.22464679914735E-16));
#18398=DIRECTION('',(-1.22464679914735E-16,-1.22464679914735E-16,1.));
#18399=DIRECTION('',(-1.,-1.258548236767E-48,-1.22464679914735E-16));
#18400=DIRECTION('',(-1.22464679914735E-16,-1.22464679914735E-16,1.));
#18401=DIRECTION('',(-1.,-1.258548236767E-48,-1.22464679914735E-16));
#18402=DIRECTION('',(-6.12323399573676E-17,-0.866025403784439,0.5));
#18403=DIRECTION('',(-1.,8.72591961210534E-32,-1.22464679914735E-16));
#18404=DIRECTION('',(-6.12323399573676E-17,-0.866025403784439,0.5));
#18405=DIRECTION('',(-1.,8.72591961210534E-32,-1.22464679914735E-16));
#18406=DIRECTION('',(-6.12323399573676E-17,-0.866025403784439,0.5));
#18407=DIRECTION('',(-1.,8.72591961210534E-32,-1.22464679914735E-16));
#18408=DIRECTION('',(-6.12323399573676E-17,-0.866025403784439,0.5));
#18409=DIRECTION('',(-1.,8.72591961210534E-32,-1.22464679914735E-16));
#18410=DIRECTION('',(-6.12323399573676E-17,-0.866025403784439,0.5));
#18411=DIRECTION('',(-1.,8.72591961210534E-32,-1.22464679914735E-16));
#18412=DIRECTION('',(-6.12323399573676E-17,-0.866025403784439,0.5));
#18413=DIRECTION('',(-1.,8.72591961210534E-32,-1.22464679914735E-16));
#18414=DIRECTION('',(-6.12323399573676E-17,-0.866025403784439,0.5));
#18415=DIRECTION('',(-1.,8.72591961210534E-32,-1.22464679914735E-16));
#18416=DIRECTION('',(-6.12323399573676E-17,-0.866025403784439,0.5));
#18417=DIRECTION('',(-1.,8.72591961210534E-32,-1.22464679914735E-16));
#18418=DIRECTION('',(1.22464679914735E-16,0.,-1.));
#18419=DIRECTION('',(-1.,0.,-1.22464679914735E-16));
#18420=DIRECTION('',(1.22464679914735E-16,0.,-1.));
#18421=DIRECTION('',(-1.,0.,-1.22464679914735E-16));
#18422=DIRECTION('',(1.22464679914735E-16,0.,-1.));
#18423=DIRECTION('',(-1.,0.,-1.22464679914735E-16));
#18424=DIRECTION('',(1.22464679914735E-16,0.,-1.));
#18425=DIRECTION('',(-1.,0.,-1.22464679914735E-16));
#18426=DIRECTION('',(1.22464679914735E-16,0.,-1.));
#18427=DIRECTION('',(-1.,0.,-1.22464679914735E-16));
#18428=DIRECTION('',(1.22464679914735E-16,0.,-1.));
#18429=DIRECTION('',(-1.,0.,-1.22464679914735E-16));
#18430=DIRECTION('',(1.22464679914735E-16,0.,-1.));
#18431=DIRECTION('',(-1.,0.,-1.22464679914735E-16));
#18432=DIRECTION('',(1.22464679914735E-16,0.,-1.));
#18433=DIRECTION('',(-1.,0.,-1.22464679914735E-16));
#18434=DIRECTION('',(6.12323399573677E-17,0.866025403784439,-0.5));
#18435=DIRECTION('',(-1.,1.72655894117776E-31,-1.22464679914735E-16));
#18436=DIRECTION('',(6.12323399573677E-17,0.866025403784439,-0.5));
#18437=DIRECTION('',(-1.,1.72655894117776E-31,-1.22464679914735E-16));
#18438=DIRECTION('',(6.12323399573677E-17,0.866025403784439,-0.5));
#18439=DIRECTION('',(-1.,1.72655894117776E-31,-1.22464679914735E-16));
#18440=DIRECTION('',(6.12323399573677E-17,0.866025403784439,-0.5));
#18441=DIRECTION('',(-1.,1.72655894117776E-31,-1.22464679914735E-16));
#18442=DIRECTION('',(6.12323399573677E-17,0.866025403784439,-0.5));
#18443=DIRECTION('',(-1.,1.72655894117776E-31,-1.22464679914735E-16));
#18444=DIRECTION('',(6.12323399573677E-17,0.866025403784439,-0.5));
#18445=DIRECTION('',(-1.,1.72655894117776E-31,-1.22464679914735E-16));
#18446=DIRECTION('',(6.12323399573677E-17,0.866025403784439,-0.5));
#18447=DIRECTION('',(-1.,1.72655894117776E-31,-1.22464679914735E-16));
#18448=DIRECTION('',(6.12323399573677E-17,0.866025403784439,-0.5));
#18449=DIRECTION('',(-1.,1.72655894117776E-31,-1.22464679914735E-16));
#18450=DIRECTION('',(-6.12323399573677E-17,0.866025403784438,0.5));
#18451=DIRECTION('',(-1.,-1.64144897904239E-31,-1.22464679914735E-16));
#18452=DIRECTION('',(-6.12323399573677E-17,0.866025403784438,0.5));
#18453=DIRECTION('',(-1.,-1.64144897904239E-31,-1.22464679914735E-16));
#18454=DIRECTION('',(-6.12323399573677E-17,0.866025403784438,0.5));
#18455=DIRECTION('',(-1.,-1.64144897904239E-31,-1.22464679914735E-16));
#18456=DIRECTION('',(-6.12323399573677E-17,0.866025403784438,0.5));
#18457=DIRECTION('',(-1.,-1.64144897904239E-31,-1.22464679914735E-16));
#18458=DIRECTION('',(-6.12323399573677E-17,0.866025403784438,0.5));
#18459=DIRECTION('',(-1.,-1.64144897904239E-31,-1.22464679914735E-16));
#18460=DIRECTION('',(-6.12323399573677E-17,0.866025403784438,0.5));
#18461=DIRECTION('',(-1.,-1.64144897904239E-31,-1.22464679914735E-16));
#18462=DIRECTION('',(-6.12323399573677E-17,0.866025403784438,0.5));
#18463=DIRECTION('',(-1.,-1.64144897904239E-31,-1.22464679914735E-16));
#18464=DIRECTION('',(-6.12323399573677E-17,0.866025403784438,0.5));
#18465=DIRECTION('',(-1.,-1.64144897904239E-31,-1.22464679914735E-16));
#18466=DIRECTION('',(-1.22464679914735E-16,-1.22464679914735E-16,1.));
#18467=DIRECTION('',(-1.,-1.258548236767E-48,-1.22464679914735E-16));
#18468=DIRECTION('',(-1.22464679914735E-16,-1.22464679914735E-16,1.));
#18469=DIRECTION('',(-1.,-1.258548236767E-48,-1.22464679914735E-16));
#18470=DIRECTION('',(-1.22464679914735E-16,-1.22464679914735E-16,1.));
#18471=DIRECTION('',(-1.,-1.258548236767E-48,-1.22464679914735E-16));
#18472=DIRECTION('',(-1.22464679914735E-16,-1.22464679914735E-16,1.));
#18473=DIRECTION('',(-1.,-1.258548236767E-48,-1.22464679914735E-16));
#18474=DIRECTION('',(-1.22464679914735E-16,-1.22464679914735E-16,1.));
#18475=DIRECTION('',(-1.,-1.258548236767E-48,-1.22464679914735E-16));
#18476=DIRECTION('',(-1.22464679914735E-16,-1.22464679914735E-16,1.));
#18477=DIRECTION('',(-1.,-1.258548236767E-48,-1.22464679914735E-16));
#18478=DIRECTION('',(-1.22464679914735E-16,-1.22464679914735E-16,1.));
#18479=DIRECTION('',(-1.,-1.258548236767E-48,-1.22464679914735E-16));
#18480=DIRECTION('',(-1.22464679914735E-16,-1.22464679914735E-16,1.));
#18481=DIRECTION('',(-1.,-1.258548236767E-48,-1.22464679914735E-16));
#18482=DIRECTION('',(-6.12323399573676E-17,-0.866025403784439,0.5));
#18483=DIRECTION('',(-1.,8.72591961210534E-32,-1.22464679914735E-16));
#18484=DIRECTION('',(-6.12323399573676E-17,-0.866025403784439,0.5));
#18485=DIRECTION('',(-1.,8.72591961210534E-32,-1.22464679914735E-16));
#18486=DIRECTION('',(-6.12323399573676E-17,-0.866025403784439,0.5));
#18487=DIRECTION('',(-1.,8.72591961210534E-32,-1.22464679914735E-16));
#18488=DIRECTION('',(-6.12323399573676E-17,-0.866025403784439,0.5));
#18489=DIRECTION('',(-1.,8.72591961210534E-32,-1.22464679914735E-16));
#18490=DIRECTION('',(-6.12323399573676E-17,-0.866025403784439,0.5));
#18491=DIRECTION('',(-1.,8.72591961210534E-32,-1.22464679914735E-16));
#18492=DIRECTION('',(-6.12323399573676E-17,-0.866025403784439,0.5));
#18493=DIRECTION('',(-1.,8.72591961210534E-32,-1.22464679914735E-16));
#18494=DIRECTION('',(-6.12323399573676E-17,-0.866025403784439,0.5));
#18495=DIRECTION('',(-1.,8.72591961210534E-32,-1.22464679914735E-16));
#18496=DIRECTION('',(-6.12323399573676E-17,-0.866025403784439,0.5));
#18497=DIRECTION('',(-1.,8.72591961210534E-32,-1.22464679914735E-16));
#18498=DIRECTION('',(0.,0.,1.));
#18499=DIRECTION('',(1.,0.,0.));
#18500=DIRECTION('',(0.,0.,1.));
#18501=DIRECTION('',(1.,0.,0.));
#18502=DIRECTION('',(0.,0.,1.));
#18503=DIRECTION('',(1.,0.,0.));
#18504=DIRECTION('',(1.22464679914735E-16,0.,-1.));
#18505=DIRECTION('',(-1.,0.,-1.22464679914735E-16));
#18506=DIRECTION('',(1.22464679914735E-16,0.,-1.));
#18507=DIRECTION('',(-1.,0.,-1.22464679914735E-16));
#18508=DIRECTION('',(1.22464679914735E-16,0.,-1.));
#18509=DIRECTION('',(-1.,0.,-1.22464679914735E-16));
#18510=DIRECTION('',(1.22464679914735E-16,0.,-1.));
#18511=DIRECTION('',(-1.,0.,-1.22464679914735E-16));
#18512=DIRECTION('',(8.65956056235493E-17,-0.707106781186548,-0.707106781186547));
#18513=DIRECTION('',(-1.,-1.84470294816695E-31,-1.22464679914735E-16));
#18514=DIRECTION('',(0.,-0.707106781186548,0.707106781186547));
#18515=DIRECTION('',(1.,0.,0.));
#18516=DIRECTION('',(8.65956056235493E-17,-0.707106781186548,-0.707106781186547));
#18517=DIRECTION('',(-1.,-1.84470294816695E-31,-1.22464679914735E-16));
#18518=DIRECTION('',(0.,-0.707106781186548,0.707106781186547));
#18519=DIRECTION('',(1.,0.,0.));
#18520=DIRECTION('',(8.65956056235493E-17,-0.707106781186548,-0.707106781186547));
#18521=DIRECTION('',(-1.,-1.84470294816695E-31,-1.22464679914735E-16));
#18522=DIRECTION('',(0.,0.,1.));
#18523=DIRECTION('',(1.,0.,0.));
#18524=DIRECTION('',(0.,0.,1.));
#18525=DIRECTION('',(1.,0.,0.));
#18526=DIRECTION('',(0.,0.,1.));
#18527=DIRECTION('',(1.,0.,0.));
#18528=CARTESIAN_POINT('',(0.,0.,0.));
#18529=CARTESIAN_POINT('',(0.,0.,0.));
#18530=CARTESIAN_POINT('Origin',(160.,0.198623766039044,-16.073623766039));
#18531=CARTESIAN_POINT('',(160.,0.,-21.8854076400856));
#18532=CARTESIAN_POINT('Origin',(160.,0.,-15.875));
#18533=CARTESIAN_POINT('',(160.,3.45131495949716,-25.3367225995828));
#18534=CARTESIAN_POINT('',(160.,-2.80658005400379,-19.0788275860818));
#18535=CARTESIAN_POINT('Origin',(160.,6.45651877953999,-22.33151877954));
#18536=CARTESIAN_POINT('Origin',(160.,6.45651877953999,-22.33151877954));
#18537=CARTESIAN_POINT('',(160.,4.61804114845495,-24.169996410625));
#18538=CARTESIAN_POINT('Origin',(160.,6.45651877953999,-22.33151877954));
#18539=CARTESIAN_POINT('Origin',(160.,12.7497691321003,-28.6247691321003));
#18540=CARTESIAN_POINT('',(160.,16.2900299668715,-35.8419852290415));
#18541=CARTESIAN_POINT('',(160.,10.9112915010153,-30.4632467631853));
#18542=CARTESIAN_POINT('',(160.,19.9669852290415,-32.1650299668715));
#18543=CARTESIAN_POINT('Ctrl Pts',(160.,19.9669852290415,-32.1650299668715));
#18544=CARTESIAN_POINT('Ctrl Pts',(159.669086687003,19.9669852290415,-32.1650299668715));
#18545=CARTESIAN_POINT('Ctrl Pts',(159.319226654958,19.8974854281187,-32.1901877843544));
#18546=CARTESIAN_POINT('Ctrl Pts',(158.680055812673,19.6321847802655,-32.3016802236596));
#18547=CARTESIAN_POINT('Ctrl Pts',(158.390338151249,19.4379182273394,-32.3893238446769));
#18548=CARTESIAN_POINT('Ctrl Pts',(157.932962788451,19.0166793035856,-32.6149113620875));
#18549=CARTESIAN_POINT('Ctrl Pts',(157.733428383838,18.7604617888226,-32.7685524550269));
#18550=CARTESIAN_POINT('Ctrl Pts',(157.466846434434,18.2360908160848,-33.1486404414343));
#18551=CARTESIAN_POINT('Ctrl Pts',(157.4,17.9686009905262,-33.3761428884047));
#18552=CARTESIAN_POINT('Ctrl Pts',(157.4,17.5011428884047,-33.8436009905262));
#18553=CARTESIAN_POINT('Ctrl Pts',(157.466846434434,17.2736404414343,-34.1110908160848));
#18554=CARTESIAN_POINT('Ctrl Pts',(157.733428383838,16.8935524550269,-34.6354617888226));
#18555=CARTESIAN_POINT('Ctrl Pts',(157.932962788451,16.7399113620875,-34.8916793035856));
#18556=CARTESIAN_POINT('Ctrl Pts',(158.390338151249,16.5143238446769,-35.3129182273394));
#18557=CARTESIAN_POINT('Ctrl Pts',(158.680055812673,16.4266802236596,-35.5071847802655));
#18558=CARTESIAN_POINT('Ctrl Pts',(159.319226654958,16.3151877843544,-35.7724854281188));
#18559=CARTESIAN_POINT('Ctrl Pts',(159.669086687003,16.2900299668715,-35.8419852290415));
#18560=CARTESIAN_POINT('Ctrl Pts',(160.,16.2900299668715,-35.8419852290415));
#18561=CARTESIAN_POINT('Ctrl Pts',(160.,16.2900299668715,-35.8419852290415));
#18562=CARTESIAN_POINT('Ctrl Pts',(160.330913312997,16.2900299668715,-35.8419852290416));
#18563=CARTESIAN_POINT('Ctrl Pts',(160.680773345042,16.3151877843544,-35.7724854281188));
#18564=CARTESIAN_POINT('Ctrl Pts',(161.319944187327,16.4266802236596,-35.5071847802655));
#18565=CARTESIAN_POINT('Ctrl Pts',(161.609661848751,16.5143238446769,-35.3129182273394));
#18566=CARTESIAN_POINT('Ctrl Pts',(162.067037211549,16.7399113620875,-34.8916793035856));
#18567=CARTESIAN_POINT('Ctrl Pts',(162.266571616162,16.8935524550269,-34.6354617888227));
#18568=CARTESIAN_POINT('Ctrl Pts',(162.533153565566,17.2736404414343,-34.1110908160848));
#18569=CARTESIAN_POINT('Ctrl Pts',(162.6,17.5011428884047,-33.8436009905262));
#18570=CARTESIAN_POINT('Ctrl Pts',(162.6,17.9686009905262,-33.3761428884047));
#18571=CARTESIAN_POINT('Ctrl Pts',(162.533153565566,18.2360908160848,-33.1486404414343));
#18572=CARTESIAN_POINT('Ctrl Pts',(162.266571616161,18.7604617888227,-32.7685524550269));
#18573=CARTESIAN_POINT('Ctrl Pts',(162.067037211549,19.0166793035856,-32.6149113620875));
#18574=CARTESIAN_POINT('Ctrl Pts',(161.609661848751,19.4379182273394,-32.3893238446769));
#18575=CARTESIAN_POINT('Ctrl Pts',(161.319944187327,19.6321847802654,-32.3016802236596));
#18576=CARTESIAN_POINT('Ctrl Pts',(160.680773345042,19.8974854281187,-32.1901877843544));
#18577=CARTESIAN_POINT('Ctrl Pts',(160.330913312997,19.9669852290415,-32.1650299668715));
#18578=CARTESIAN_POINT('Ctrl Pts',(160.,19.9669852290415,-32.1650299668715));
#18579=CARTESIAN_POINT('Origin',(90.,0.198623766039044,-16.073623766039));
#18580=CARTESIAN_POINT('',(90.,0.,-21.8854076400856));
#18581=CARTESIAN_POINT('Origin',(90.,0.,-15.875));
#18582=CARTESIAN_POINT('',(90.,3.45131495949716,-25.3367225995828));
#18583=CARTESIAN_POINT('',(90.,-2.80658005400379,-19.0788275860818));
#18584=CARTESIAN_POINT('Origin',(90.,6.45651877953999,-22.33151877954));
#18585=CARTESIAN_POINT('Origin',(90.,6.45651877953999,-22.33151877954));
#18586=CARTESIAN_POINT('',(90.,4.61804114845495,-24.169996410625));
#18587=CARTESIAN_POINT('Origin',(90.,6.45651877953999,-22.33151877954));
#18588=CARTESIAN_POINT('Origin',(90.,12.7497691321003,-28.6247691321003));
#18589=CARTESIAN_POINT('',(90.,16.2900299668715,-35.8419852290415));
#18590=CARTESIAN_POINT('',(90.,10.9112915010153,-30.4632467631853));
#18591=CARTESIAN_POINT('',(90.,19.9669852290415,-32.1650299668715));
#18592=CARTESIAN_POINT('Ctrl Pts',(90.,19.9669852290415,-32.1650299668715));
#18593=CARTESIAN_POINT('Ctrl Pts',(89.6690866870034,19.9669852290415,-32.1650299668715));
#18594=CARTESIAN_POINT('Ctrl Pts',(89.3192266549576,19.8974854281187,-32.1901877843544));
#18595=CARTESIAN_POINT('Ctrl Pts',(88.6800558126726,19.6321847802655,-32.3016802236596));
#18596=CARTESIAN_POINT('Ctrl Pts',(88.3903381512495,19.4379182273394,-32.3893238446769));
#18597=CARTESIAN_POINT('Ctrl Pts',(87.9329627884514,19.0166793035856,-32.6149113620875));
#18598=CARTESIAN_POINT('Ctrl Pts',(87.7334283838385,18.7604617888226,-32.7685524550269));
#18599=CARTESIAN_POINT('Ctrl Pts',(87.4668464344339,18.2360908160848,-33.1486404414343));
#18600=CARTESIAN_POINT('Ctrl Pts',(87.4,17.9686009905262,-33.3761428884047));
#18601=CARTESIAN_POINT('Ctrl Pts',(87.4,17.5011428884047,-33.8436009905262));
#18602=CARTESIAN_POINT('Ctrl Pts',(87.4668464344339,17.2736404414343,-34.1110908160848));
#18603=CARTESIAN_POINT('Ctrl Pts',(87.7334283838385,16.8935524550269,-34.6354617888227));
#18604=CARTESIAN_POINT('Ctrl Pts',(87.9329627884514,16.7399113620875,-34.8916793035856));
#18605=CARTESIAN_POINT('Ctrl Pts',(88.3903381512495,16.5143238446769,-35.3129182273394));
#18606=CARTESIAN_POINT('Ctrl Pts',(88.6800558126726,16.4266802236596,-35.5071847802655));
#18607=CARTESIAN_POINT('Ctrl Pts',(89.3192266549576,16.3151877843544,-35.7724854281188));
#18608=CARTESIAN_POINT('Ctrl Pts',(89.6690866870034,16.2900299668715,-35.8419852290415));
#18609=CARTESIAN_POINT('Ctrl Pts',(90.,16.2900299668715,-35.8419852290415));
#18610=CARTESIAN_POINT('Ctrl Pts',(90.,16.2900299668715,-35.8419852290415));
#18611=CARTESIAN_POINT('Ctrl Pts',(90.3309133129966,16.2900299668715,-35.8419852290415));
#18612=CARTESIAN_POINT('Ctrl Pts',(90.6807733450424,16.3151877843544,-35.7724854281188));
#18613=CARTESIAN_POINT('Ctrl Pts',(91.3199441873274,16.4266802236596,-35.5071847802655));
#18614=CARTESIAN_POINT('Ctrl Pts',(91.6096618487505,16.5143238446769,-35.3129182273394));
#18615=CARTESIAN_POINT('Ctrl Pts',(92.0670372115486,16.7399113620875,-34.8916793035856));
#18616=CARTESIAN_POINT('Ctrl Pts',(92.2665716161615,16.8935524550269,-34.6354617888227));
#18617=CARTESIAN_POINT('Ctrl Pts',(92.5331535655661,17.2736404414343,-34.1110908160848));
#18618=CARTESIAN_POINT('Ctrl Pts',(92.6,17.5011428884047,-33.8436009905262));
#18619=CARTESIAN_POINT('Ctrl Pts',(92.6,17.9686009905262,-33.3761428884047));
#18620=CARTESIAN_POINT('Ctrl Pts',(92.5331535655662,18.2360908160848,-33.1486404414343));
#18621=CARTESIAN_POINT('Ctrl Pts',(92.2665716161615,18.7604617888226,-32.7685524550269));
#18622=CARTESIAN_POINT('Ctrl Pts',(92.0670372115486,19.0166793035856,-32.6149113620875));
#18623=CARTESIAN_POINT('Ctrl Pts',(91.6096618487505,19.4379182273394,-32.3893238446769));
#18624=CARTESIAN_POINT('Ctrl Pts',(91.3199441873274,19.6321847802655,-32.3016802236596));
#18625=CARTESIAN_POINT('Ctrl Pts',(90.6807733450424,19.8974854281187,-32.1901877843544));
#18626=CARTESIAN_POINT('Ctrl Pts',(90.3309133129966,19.9669852290415,-32.1650299668715));
#18627=CARTESIAN_POINT('Ctrl Pts',(90.,19.9669852290415,-32.1650299668715));
#18628=CARTESIAN_POINT('Origin',(20.,0.198623766039044,-16.073623766039));
#18629=CARTESIAN_POINT('',(20.,0.,-21.8854076400856));
#18630=CARTESIAN_POINT('Origin',(20.,0.,-15.875));
#18631=CARTESIAN_POINT('',(20.,3.45131495949716,-25.3367225995828));
#18632=CARTESIAN_POINT('',(20.,-2.80658005400379,-19.0788275860818));
#18633=CARTESIAN_POINT('Origin',(20.,6.45651877953999,-22.33151877954));
#18634=CARTESIAN_POINT('Origin',(20.,6.45651877953999,-22.33151877954));
#18635=CARTESIAN_POINT('',(20.,4.61804114845495,-24.169996410625));
#18636=CARTESIAN_POINT('Origin',(20.,6.45651877953999,-22.33151877954));
#18637=CARTESIAN_POINT('Origin',(20.,12.7497691321003,-28.6247691321003));
#18638=CARTESIAN_POINT('',(20.,16.2900299668715,-35.8419852290415));
#18639=CARTESIAN_POINT('',(20.,10.9112915010153,-30.4632467631853));
#18640=CARTESIAN_POINT('',(20.,19.9669852290415,-32.1650299668715));
#18641=CARTESIAN_POINT('Ctrl Pts',(20.,19.9669852290415,-32.1650299668715));
#18642=CARTESIAN_POINT('Ctrl Pts',(19.6690866870034,19.9669852290415,-32.1650299668715));
#18643=CARTESIAN_POINT('Ctrl Pts',(19.3192266549576,19.8974854281187,-32.1901877843544));
#18644=CARTESIAN_POINT('Ctrl Pts',(18.6800558126726,19.6321847802655,-32.3016802236596));
#18645=CARTESIAN_POINT('Ctrl Pts',(18.3903381512495,19.4379182273394,-32.3893238446769));
#18646=CARTESIAN_POINT('Ctrl Pts',(17.9329627884514,19.0166793035856,-32.6149113620875));
#18647=CARTESIAN_POINT('Ctrl Pts',(17.7334283838385,18.7604617888226,-32.7685524550269));
#18648=CARTESIAN_POINT('Ctrl Pts',(17.4668464344338,18.2360908160848,-33.1486404414343));
#18649=CARTESIAN_POINT('Ctrl Pts',(17.4,17.9686009905262,-33.3761428884047));
#18650=CARTESIAN_POINT('Ctrl Pts',(17.4,17.5011428884047,-33.8436009905262));
#18651=CARTESIAN_POINT('Ctrl Pts',(17.4668464344338,17.2736404414343,-34.1110908160848));
#18652=CARTESIAN_POINT('Ctrl Pts',(17.7334283838385,16.8935524550269,-34.6354617888227));
#18653=CARTESIAN_POINT('Ctrl Pts',(17.9329627884514,16.7399113620875,-34.8916793035856));
#18654=CARTESIAN_POINT('Ctrl Pts',(18.3903381512495,16.5143238446769,-35.3129182273394));
#18655=CARTESIAN_POINT('Ctrl Pts',(18.6800558126726,16.4266802236596,-35.5071847802655));
#18656=CARTESIAN_POINT('Ctrl Pts',(19.3192266549576,16.3151877843544,-35.7724854281188));
#18657=CARTESIAN_POINT('Ctrl Pts',(19.6690866870034,16.2900299668715,-35.8419852290415));
#18658=CARTESIAN_POINT('Ctrl Pts',(20.,16.2900299668715,-35.8419852290415));
#18659=CARTESIAN_POINT('Ctrl Pts',(20.,16.2900299668715,-35.8419852290415));
#18660=CARTESIAN_POINT('Ctrl Pts',(20.3309133129966,16.2900299668715,-35.8419852290415));
#18661=CARTESIAN_POINT('Ctrl Pts',(20.6807733450423,16.3151877843544,-35.7724854281188));
#18662=CARTESIAN_POINT('Ctrl Pts',(21.3199441873274,16.4266802236596,-35.5071847802655));
#18663=CARTESIAN_POINT('Ctrl Pts',(21.6096618487505,16.5143238446769,-35.3129182273394));
#18664=CARTESIAN_POINT('Ctrl Pts',(22.0670372115486,16.7399113620875,-34.8916793035856));
#18665=CARTESIAN_POINT('Ctrl Pts',(22.2665716161615,16.8935524550269,-34.6354617888227));
#18666=CARTESIAN_POINT('Ctrl Pts',(22.5331535655662,17.2736404414343,-34.1110908160848));
#18667=CARTESIAN_POINT('Ctrl Pts',(22.6,17.5011428884047,-33.8436009905262));
#18668=CARTESIAN_POINT('Ctrl Pts',(22.6,17.9686009905262,-33.3761428884047));
#18669=CARTESIAN_POINT('Ctrl Pts',(22.5331535655662,18.2360908160848,-33.1486404414343));
#18670=CARTESIAN_POINT('Ctrl Pts',(22.2665716161615,18.7604617888226,-32.7685524550269));
#18671=CARTESIAN_POINT('Ctrl Pts',(22.0670372115486,19.0166793035856,-32.6149113620875));
#18672=CARTESIAN_POINT('Ctrl Pts',(21.6096618487505,19.4379182273394,-32.3893238446769));
#18673=CARTESIAN_POINT('Ctrl Pts',(21.3199441873274,19.6321847802655,-32.3016802236596));
#18674=CARTESIAN_POINT('Ctrl Pts',(20.6807733450424,19.8974854281187,-32.1901877843544));
#18675=CARTESIAN_POINT('Ctrl Pts',(20.3309133129966,19.9669852290415,-32.1650299668715));
#18676=CARTESIAN_POINT('Ctrl Pts',(20.,19.9669852290415,-32.1650299668715));
#18677=CARTESIAN_POINT('Origin',(160.,0.198623766039043,16.073623766039));
#18678=CARTESIAN_POINT('',(160.,0.,9.86459235991433));
#18679=CARTESIAN_POINT('Origin',(160.,0.,15.875));
#18680=CARTESIAN_POINT('',(160.,9.46172259958282,19.3263149594972));
#18681=CARTESIAN_POINT('',(160.,3.20382758608187,13.0684199459962));
#18682=CARTESIAN_POINT('Origin',(160.,6.45651877953999,22.33151877954));
#18683=CARTESIAN_POINT('Origin',(160.,6.45651877953999,22.33151877954));
#18684=CARTESIAN_POINT('',(160.,8.29499641062501,20.4930411484549));
#18685=CARTESIAN_POINT('Origin',(160.,6.45651877953999,22.33151877954));
#18686=CARTESIAN_POINT('Origin',(160.,12.7497691321003,28.6247691321003));
#18687=CARTESIAN_POINT('',(160.,19.9669852290415,32.1650299668715));
#18688=CARTESIAN_POINT('',(160.,14.5882467631853,26.7862915010153));
#18689=CARTESIAN_POINT('',(160.,16.2900299668715,35.8419852290415));
#18690=CARTESIAN_POINT('Ctrl Pts',(160.,16.2900299668715,35.8419852290415));
#18691=CARTESIAN_POINT('Ctrl Pts',(159.669086687003,16.2900299668715,35.8419852290415));
#18692=CARTESIAN_POINT('Ctrl Pts',(159.319226654958,16.3151877843544,35.7724854281188));
#18693=CARTESIAN_POINT('Ctrl Pts',(158.680055812673,16.4266802236596,35.5071847802655));
#18694=CARTESIAN_POINT('Ctrl Pts',(158.390338151249,16.5143238446769,35.3129182273394));
#18695=CARTESIAN_POINT('Ctrl Pts',(157.932962788451,16.7399113620875,34.8916793035856));
#18696=CARTESIAN_POINT('Ctrl Pts',(157.733428383838,16.8935524550269,34.6354617888226));
#18697=CARTESIAN_POINT('Ctrl Pts',(157.466846434434,17.2736404414343,34.1110908160848));
#18698=CARTESIAN_POINT('Ctrl Pts',(157.4,17.5011428884047,33.8436009905262));
#18699=CARTESIAN_POINT('Ctrl Pts',(157.4,17.9686009905262,33.3761428884047));
#18700=CARTESIAN_POINT('Ctrl Pts',(157.466846434434,18.2360908160848,33.1486404414343));
#18701=CARTESIAN_POINT('Ctrl Pts',(157.733428383838,18.7604617888226,32.7685524550269));
#18702=CARTESIAN_POINT('Ctrl Pts',(157.932962788451,19.0166793035856,32.6149113620875));
#18703=CARTESIAN_POINT('Ctrl Pts',(158.390338151249,19.4379182273394,32.3893238446769));
#18704=CARTESIAN_POINT('Ctrl Pts',(158.680055812673,19.6321847802654,32.3016802236596));
#18705=CARTESIAN_POINT('Ctrl Pts',(159.319226654958,19.8974854281187,32.1901877843544));
#18706=CARTESIAN_POINT('Ctrl Pts',(159.669086687003,19.9669852290415,32.1650299668715));
#18707=CARTESIAN_POINT('Ctrl Pts',(160.,19.9669852290415,32.1650299668715));
#18708=CARTESIAN_POINT('Ctrl Pts',(160.,19.9669852290415,32.1650299668715));
#18709=CARTESIAN_POINT('Ctrl Pts',(160.330913312997,19.9669852290415,32.1650299668715));
#18710=CARTESIAN_POINT('Ctrl Pts',(160.680773345042,19.8974854281187,32.1901877843544));
#18711=CARTESIAN_POINT('Ctrl Pts',(161.319944187327,19.6321847802655,32.3016802236596));
#18712=CARTESIAN_POINT('Ctrl Pts',(161.609661848751,19.4379182273394,32.3893238446769));
#18713=CARTESIAN_POINT('Ctrl Pts',(162.067037211549,19.0166793035856,32.6149113620875));
#18714=CARTESIAN_POINT('Ctrl Pts',(162.266571616162,18.7604617888227,32.7685524550269));
#18715=CARTESIAN_POINT('Ctrl Pts',(162.533153565566,18.2360908160848,33.1486404414343));
#18716=CARTESIAN_POINT('Ctrl Pts',(162.6,17.9686009905262,33.3761428884047));
#18717=CARTESIAN_POINT('Ctrl Pts',(162.6,17.5011428884047,33.8436009905262));
#18718=CARTESIAN_POINT('Ctrl Pts',(162.533153565566,17.2736404414343,34.1110908160848));
#18719=CARTESIAN_POINT('Ctrl Pts',(162.266571616161,16.8935524550269,34.6354617888227));
#18720=CARTESIAN_POINT('Ctrl Pts',(162.067037211549,16.7399113620875,34.8916793035856));
#18721=CARTESIAN_POINT('Ctrl Pts',(161.609661848751,16.5143238446769,35.3129182273394));
#18722=CARTESIAN_POINT('Ctrl Pts',(161.319944187327,16.4266802236596,35.5071847802655));
#18723=CARTESIAN_POINT('Ctrl Pts',(160.680773345042,16.3151877843544,35.7724854281188));
#18724=CARTESIAN_POINT('Ctrl Pts',(160.330913312997,16.2900299668715,35.8419852290415));
#18725=CARTESIAN_POINT('Ctrl Pts',(160.,16.2900299668715,35.8419852290415));
#18726=CARTESIAN_POINT('Origin',(90.,0.198623766039043,16.073623766039));
#18727=CARTESIAN_POINT('',(90.,0.,9.86459235991433));
#18728=CARTESIAN_POINT('Origin',(90.,0.,15.875));
#18729=CARTESIAN_POINT('',(90.,9.46172259958282,19.3263149594972));
#18730=CARTESIAN_POINT('',(90.,3.20382758608187,13.0684199459962));
#18731=CARTESIAN_POINT('Origin',(90.,6.45651877953999,22.33151877954));
#18732=CARTESIAN_POINT('Origin',(90.,6.45651877953999,22.33151877954));
#18733=CARTESIAN_POINT('',(90.,8.29499641062501,20.4930411484549));
#18734=CARTESIAN_POINT('Origin',(90.,6.45651877953999,22.33151877954));
#18735=CARTESIAN_POINT('Origin',(90.,12.7497691321003,28.6247691321003));
#18736=CARTESIAN_POINT('',(90.,19.9669852290415,32.1650299668715));
#18737=CARTESIAN_POINT('',(90.,14.5882467631853,26.7862915010153));
#18738=CARTESIAN_POINT('',(90.,16.2900299668715,35.8419852290415));
#18739=CARTESIAN_POINT('Ctrl Pts',(90.,16.2900299668715,35.8419852290415));
#18740=CARTESIAN_POINT('Ctrl Pts',(89.6690866870034,16.2900299668715,35.8419852290415));
#18741=CARTESIAN_POINT('Ctrl Pts',(89.3192266549576,16.3151877843544,35.7724854281188));
#18742=CARTESIAN_POINT('Ctrl Pts',(88.6800558126726,16.4266802236596,35.5071847802655));
#18743=CARTESIAN_POINT('Ctrl Pts',(88.3903381512495,16.5143238446769,35.3129182273394));
#18744=CARTESIAN_POINT('Ctrl Pts',(87.9329627884514,16.7399113620875,34.8916793035856));
#18745=CARTESIAN_POINT('Ctrl Pts',(87.7334283838385,16.8935524550269,34.6354617888227));
#18746=CARTESIAN_POINT('Ctrl Pts',(87.4668464344339,17.2736404414343,34.1110908160848));
#18747=CARTESIAN_POINT('Ctrl Pts',(87.4,17.5011428884047,33.8436009905262));
#18748=CARTESIAN_POINT('Ctrl Pts',(87.4,17.9686009905262,33.3761428884047));
#18749=CARTESIAN_POINT('Ctrl Pts',(87.4668464344339,18.2360908160848,33.1486404414343));
#18750=CARTESIAN_POINT('Ctrl Pts',(87.7334283838385,18.7604617888226,32.7685524550269));
#18751=CARTESIAN_POINT('Ctrl Pts',(87.9329627884514,19.0166793035856,32.6149113620875));
#18752=CARTESIAN_POINT('Ctrl Pts',(88.3903381512495,19.4379182273394,32.3893238446769));
#18753=CARTESIAN_POINT('Ctrl Pts',(88.6800558126726,19.6321847802655,32.3016802236596));
#18754=CARTESIAN_POINT('Ctrl Pts',(89.3192266549576,19.8974854281187,32.1901877843544));
#18755=CARTESIAN_POINT('Ctrl Pts',(89.6690866870034,19.9669852290415,32.1650299668715));
#18756=CARTESIAN_POINT('Ctrl Pts',(90.,19.9669852290415,32.1650299668715));
#18757=CARTESIAN_POINT('Ctrl Pts',(90.,19.9669852290415,32.1650299668715));
#18758=CARTESIAN_POINT('Ctrl Pts',(90.3309133129966,19.9669852290415,32.1650299668715));
#18759=CARTESIAN_POINT('Ctrl Pts',(90.6807733450424,19.8974854281188,32.1901877843544));
#18760=CARTESIAN_POINT('Ctrl Pts',(91.3199441873274,19.6321847802655,32.3016802236596));
#18761=CARTESIAN_POINT('Ctrl Pts',(91.6096618487505,19.4379182273394,32.3893238446769));
#18762=CARTESIAN_POINT('Ctrl Pts',(92.0670372115486,19.0166793035856,32.6149113620875));
#18763=CARTESIAN_POINT('Ctrl Pts',(92.2665716161615,18.7604617888226,32.7685524550269));
#18764=CARTESIAN_POINT('Ctrl Pts',(92.5331535655662,18.2360908160848,33.1486404414343));
#18765=CARTESIAN_POINT('Ctrl Pts',(92.6,17.9686009905262,33.3761428884047));
#18766=CARTESIAN_POINT('Ctrl Pts',(92.6,17.5011428884047,33.8436009905262));
#18767=CARTESIAN_POINT('Ctrl Pts',(92.5331535655661,17.2736404414343,34.1110908160848));
#18768=CARTESIAN_POINT('Ctrl Pts',(92.2665716161615,16.8935524550269,34.6354617888227));
#18769=CARTESIAN_POINT('Ctrl Pts',(92.0670372115486,16.7399113620875,34.8916793035856));
#18770=CARTESIAN_POINT('Ctrl Pts',(91.6096618487505,16.5143238446769,35.3129182273394));
#18771=CARTESIAN_POINT('Ctrl Pts',(91.3199441873274,16.4266802236596,35.5071847802655));
#18772=CARTESIAN_POINT('Ctrl Pts',(90.6807733450424,16.3151877843544,35.7724854281188));
#18773=CARTESIAN_POINT('Ctrl Pts',(90.3309133129966,16.2900299668715,35.8419852290415));
#18774=CARTESIAN_POINT('Ctrl Pts',(90.,16.2900299668715,35.8419852290415));
#18775=CARTESIAN_POINT('Origin',(20.,0.198623766039043,16.073623766039));
#18776=CARTESIAN_POINT('',(20.,0.,9.86459235991433));
#18777=CARTESIAN_POINT('Origin',(20.,0.,15.875));
#18778=CARTESIAN_POINT('',(20.,9.46172259958282,19.3263149594972));
#18779=CARTESIAN_POINT('',(20.,3.20382758608187,13.0684199459962));
#18780=CARTESIAN_POINT('Origin',(20.,6.45651877953999,22.33151877954));
#18781=CARTESIAN_POINT('Origin',(20.,6.45651877953999,22.33151877954));
#18782=CARTESIAN_POINT('',(20.,8.29499641062501,20.4930411484549));
#18783=CARTESIAN_POINT('Origin',(20.,6.45651877953999,22.33151877954));
#18784=CARTESIAN_POINT('Origin',(20.,12.7497691321003,28.6247691321003));
#18785=CARTESIAN_POINT('',(20.,19.9669852290415,32.1650299668715));
#18786=CARTESIAN_POINT('',(20.,14.5882467631853,26.7862915010153));
#18787=CARTESIAN_POINT('',(20.,16.2900299668715,35.8419852290415));
#18788=CARTESIAN_POINT('Ctrl Pts',(20.,16.2900299668715,35.8419852290415));
#18789=CARTESIAN_POINT('Ctrl Pts',(19.6690866870034,16.2900299668715,35.8419852290415));
#18790=CARTESIAN_POINT('Ctrl Pts',(19.3192266549576,16.3151877843544,35.7724854281188));
#18791=CARTESIAN_POINT('Ctrl Pts',(18.6800558126726,16.4266802236596,35.5071847802655));
#18792=CARTESIAN_POINT('Ctrl Pts',(18.3903381512495,16.5143238446769,35.3129182273394));
#18793=CARTESIAN_POINT('Ctrl Pts',(17.9329627884514,16.7399113620875,34.8916793035856));
#18794=CARTESIAN_POINT('Ctrl Pts',(17.7334283838385,16.8935524550269,34.6354617888227));
#18795=CARTESIAN_POINT('Ctrl Pts',(17.4668464344338,17.2736404414343,34.1110908160848));
#18796=CARTESIAN_POINT('Ctrl Pts',(17.4,17.5011428884047,33.8436009905262));
#18797=CARTESIAN_POINT('Ctrl Pts',(17.4,17.9686009905262,33.3761428884047));
#18798=CARTESIAN_POINT('Ctrl Pts',(17.4668464344338,18.2360908160848,33.1486404414343));
#18799=CARTESIAN_POINT('Ctrl Pts',(17.7334283838385,18.7604617888226,32.7685524550269));
#18800=CARTESIAN_POINT('Ctrl Pts',(17.9329627884514,19.0166793035856,32.6149113620875));
#18801=CARTESIAN_POINT('Ctrl Pts',(18.3903381512495,19.4379182273394,32.3893238446769));
#18802=CARTESIAN_POINT('Ctrl Pts',(18.6800558126726,19.6321847802655,32.3016802236596));
#18803=CARTESIAN_POINT('Ctrl Pts',(19.3192266549576,19.8974854281187,32.1901877843544));
#18804=CARTESIAN_POINT('Ctrl Pts',(19.6690866870034,19.9669852290415,32.1650299668715));
#18805=CARTESIAN_POINT('Ctrl Pts',(20.,19.9669852290415,32.1650299668715));
#18806=CARTESIAN_POINT('Ctrl Pts',(20.,19.9669852290415,32.1650299668715));
#18807=CARTESIAN_POINT('Ctrl Pts',(20.3309133129966,19.9669852290415,32.1650299668715));
#18808=CARTESIAN_POINT('Ctrl Pts',(20.6807733450423,19.8974854281188,32.1901877843544));
#18809=CARTESIAN_POINT('Ctrl Pts',(21.3199441873274,19.6321847802655,32.3016802236596));
#18810=CARTESIAN_POINT('Ctrl Pts',(21.6096618487505,19.4379182273394,32.3893238446769));
#18811=CARTESIAN_POINT('Ctrl Pts',(22.0670372115486,19.0166793035856,32.6149113620875));
#18812=CARTESIAN_POINT('Ctrl Pts',(22.2665716161615,18.7604617888226,32.7685524550269));
#18813=CARTESIAN_POINT('Ctrl Pts',(22.5331535655662,18.2360908160848,33.1486404414343));
#18814=CARTESIAN_POINT('Ctrl Pts',(22.6,17.9686009905262,33.3761428884047));
#18815=CARTESIAN_POINT('Ctrl Pts',(22.6,17.5011428884047,33.8436009905262));
#18816=CARTESIAN_POINT('Ctrl Pts',(22.5331535655662,17.2736404414343,34.1110908160848));
#18817=CARTESIAN_POINT('Ctrl Pts',(22.2665716161615,16.8935524550269,34.6354617888227));
#18818=CARTESIAN_POINT('Ctrl Pts',(22.0670372115486,16.7399113620875,34.8916793035856));
#18819=CARTESIAN_POINT('Ctrl Pts',(21.6096618487505,16.5143238446769,35.3129182273394));
#18820=CARTESIAN_POINT('Ctrl Pts',(21.3199441873274,16.4266802236596,35.5071847802655));
#18821=CARTESIAN_POINT('Ctrl Pts',(20.6807733450423,16.3151877843544,35.7724854281188));
#18822=CARTESIAN_POINT('Ctrl Pts',(20.3309133129966,16.2900299668715,35.8419852290415));
#18823=CARTESIAN_POINT('Ctrl Pts',(20.,16.2900299668715,35.8419852290415));
#18824=CARTESIAN_POINT('Origin',(140.8,12.35,9.525));
#18825=CARTESIAN_POINT('',(135.45,12.2,9.525));
#18826=CARTESIAN_POINT('Origin',(140.8,12.2,9.525));
#18827=CARTESIAN_POINT('',(135.15,12.5,9.525));
#18828=CARTESIAN_POINT('',(135.3,12.35,9.525));
#18829=CARTESIAN_POINT('Origin',(140.8,12.5,9.525));
#18830=CARTESIAN_POINT('Origin',(0.,12.5,-15.875));
#18831=CARTESIAN_POINT('',(0.,12.5,-15.875));
#18832=CARTESIAN_POINT('',(0.,12.5,15.875));
#18833=CARTESIAN_POINT('',(0.,12.5,-15.875));
#18834=CARTESIAN_POINT('',(180.,12.5,15.875));
#18835=CARTESIAN_POINT('',(0.,12.5,15.875));
#18836=CARTESIAN_POINT('',(180.,12.5,-15.875));
#18837=CARTESIAN_POINT('',(180.,12.5,-15.875));
#18838=CARTESIAN_POINT('',(0.,12.5,-15.875));
#18839=CARTESIAN_POINT('',(33.55,12.5,-9.525));
#18840=CARTESIAN_POINT('Origin',(39.2,12.5,-9.525));
#18841=CARTESIAN_POINT('',(135.15,12.5,-9.525));
#18842=CARTESIAN_POINT('Origin',(140.8,12.5,-9.525));
#18843=CARTESIAN_POINT('',(33.55,12.5,9.525));
#18844=CARTESIAN_POINT('Origin',(39.2,12.5,9.525));
#18845=CARTESIAN_POINT('Origin',(140.8,12.5,9.525));
#18846=CARTESIAN_POINT('',(135.45,5.9,9.525));
#18847=CARTESIAN_POINT('',(135.45,12.5,9.525));
#18848=CARTESIAN_POINT('Origin',(140.8,5.9,9.525));
#18849=CARTESIAN_POINT('Origin',(39.2,12.35,-9.525));
#18850=CARTESIAN_POINT('',(33.85,12.2,-9.525));
#18851=CARTESIAN_POINT('Origin',(39.2,12.2,-9.525));
#18852=CARTESIAN_POINT('',(33.7,12.35,-9.525));
#18853=CARTESIAN_POINT('Origin',(39.2,12.5,-9.525));
#18854=CARTESIAN_POINT('',(33.85,5.9,-9.525));
#18855=CARTESIAN_POINT('',(33.85,12.5,-9.525));
#18856=CARTESIAN_POINT('Origin',(39.2,5.9,-9.525));
#18857=CARTESIAN_POINT('Origin',(39.2,12.35,9.525));
#18858=CARTESIAN_POINT('',(33.85,12.2,9.525));
#18859=CARTESIAN_POINT('Origin',(39.2,12.2,9.525));
#18860=CARTESIAN_POINT('',(33.7,12.35,9.525));
#18861=CARTESIAN_POINT('Origin',(39.2,12.5,9.525));
#18862=CARTESIAN_POINT('',(33.85,5.9,9.525));
#18863=CARTESIAN_POINT('',(33.85,12.5,9.525));
#18864=CARTESIAN_POINT('Origin',(39.2,5.9,9.525));
#18865=CARTESIAN_POINT('Origin',(140.8,12.35,-9.525));
#18866=CARTESIAN_POINT('',(135.45,12.2,-9.525));
#18867=CARTESIAN_POINT('Origin',(140.8,12.2,-9.525));
#18868=CARTESIAN_POINT('',(135.3,12.35,-9.525));
#18869=CARTESIAN_POINT('Origin',(140.8,12.5,-9.525));
#18870=CARTESIAN_POINT('',(135.45,5.9,-9.525));
#18871=CARTESIAN_POINT('',(135.45,12.5,-9.525));
#18872=CARTESIAN_POINT('Origin',(140.8,5.9,-9.525));
#18873=CARTESIAN_POINT('Origin',(140.8,5.9,-9.525));
#18874=CARTESIAN_POINT('',(137.244,5.9,-9.525));
#18875=CARTESIAN_POINT('Origin',(140.8,5.9,-9.525));
#18876=CARTESIAN_POINT('Origin',(39.2,5.9,9.525));
#18877=CARTESIAN_POINT('',(35.644,5.9,9.525));
#18878=CARTESIAN_POINT('Origin',(39.2,5.9,9.525));
#18879=CARTESIAN_POINT('Origin',(39.2,5.9,-9.525));
#18880=CARTESIAN_POINT('',(35.644,5.9,-9.525));
#18881=CARTESIAN_POINT('Origin',(39.2,5.9,-9.525));
#18882=CARTESIAN_POINT('Origin',(140.8,5.9,9.525));
#18883=CARTESIAN_POINT('',(137.244,5.9,9.525));
#18884=CARTESIAN_POINT('Origin',(140.8,5.9,9.525));
#18885=CARTESIAN_POINT('Origin',(140.8,12.5,-9.525));
#18886=CARTESIAN_POINT('',(137.244,0.,-9.525));
#18887=CARTESIAN_POINT('',(137.244,12.5,-9.525));
#18888=CARTESIAN_POINT('Origin',(140.8,0.,-9.525));
#18889=CARTESIAN_POINT('Origin',(39.2,12.5,9.525));
#18890=CARTESIAN_POINT('',(35.644,0.,9.525));
#18891=CARTESIAN_POINT('',(35.644,12.5,9.525));
#18892=CARTESIAN_POINT('Origin',(39.2,0.,9.525));
#18893=CARTESIAN_POINT('Origin',(39.2,12.5,-9.525));
#18894=CARTESIAN_POINT('',(35.644,0.,-9.525));
#18895=CARTESIAN_POINT('',(35.644,12.5,-9.525));
#18896=CARTESIAN_POINT('Origin',(39.2,0.,-9.525));
#18897=CARTESIAN_POINT('Origin',(140.8,12.5,9.525));
#18898=CARTESIAN_POINT('',(137.244,0.,9.525));
#18899=CARTESIAN_POINT('',(137.244,12.5,9.525));
#18900=CARTESIAN_POINT('Origin',(140.8,0.,9.525));
#18901=CARTESIAN_POINT('Origin',(0.,17.3,-16.075));
#18902=CARTESIAN_POINT('',(180.,17.1,-15.875));
#18903=CARTESIAN_POINT('',(180.,17.5,-16.275));
#18904=CARTESIAN_POINT('',(180.,11.5608626497484,-10.3358626497484));
#18905=CARTESIAN_POINT('',(0.,17.5,-16.275));
#18906=CARTESIAN_POINT('',(0.,17.5,-16.275));
#18907=CARTESIAN_POINT('',(0.,17.1,-15.875));
#18908=CARTESIAN_POINT('',(0.,11.5608626497484,-10.3358626497484));
#18909=CARTESIAN_POINT('',(0.,17.1,-15.875));
#18910=CARTESIAN_POINT('Origin',(0.,17.5,-15.875));
#18911=CARTESIAN_POINT('',(0.,17.5,-15.875));
#18912=CARTESIAN_POINT('',(180.,17.5,-15.875));
#18913=CARTESIAN_POINT('Origin',(0.,10.4184505989935,0.));
#18914=CARTESIAN_POINT('',(0.,17.5,-28.5666738879315));
#18915=CARTESIAN_POINT('',(0.,17.5,-28.5666738879315));
#18916=CARTESIAN_POINT('',(0.,20.836901197987,-31.9035750859185));
#18917=CARTESIAN_POINT('',(0.,20.836901197987,-31.9035750859185));
#18918=CARTESIAN_POINT('',(0.,16.0285750859185,-36.711901197987));
#18919=CARTESIAN_POINT('Origin',(0.,22.225,-38.1));
#18920=CARTESIAN_POINT('',(0.,4.71667388793148,-25.4));
#18921=CARTESIAN_POINT('',(0.,4.71667388793148,-25.4));
#18922=CARTESIAN_POINT('',(0.,0.5,-25.4));
#18923=CARTESIAN_POINT('',(0.,0.,-25.4));
#18924=CARTESIAN_POINT('',(0.,0.,-24.9));
#18925=CARTESIAN_POINT('',(0.,-3.49538735025162,-21.4046126497484));
#18926=CARTESIAN_POINT('',(0.,0.,24.9));
#18927=CARTESIAN_POINT('',(0.,0.,0.));
#18928=CARTESIAN_POINT('',(0.,0.5,25.4));
#18929=CARTESIAN_POINT('',(0.,-3.49538735025162,21.4046126497484));
#18930=CARTESIAN_POINT('',(0.,4.71667388793148,25.4));
#18931=CARTESIAN_POINT('',(0.,0.,25.4));
#18932=CARTESIAN_POINT('',(0.,16.0285750859185,36.711901197987));
#18933=CARTESIAN_POINT('',(0.,4.71667388793148,25.4));
#18934=CARTESIAN_POINT('',(0.,20.836901197987,31.9035750859185));
#18935=CARTESIAN_POINT('Origin',(0.,22.225,38.1));
#18936=CARTESIAN_POINT('',(0.,17.5,28.5666738879315));
#18937=CARTESIAN_POINT('',(0.,20.836901197987,31.9035750859185));
#18938=CARTESIAN_POINT('',(0.,17.5,16.275));
#18939=CARTESIAN_POINT('',(0.,17.5,28.5666738879315));
#18940=CARTESIAN_POINT('',(0.,17.1,15.875));
#18941=CARTESIAN_POINT('',(0.,11.5608626497484,10.3358626497484));
#18942=CARTESIAN_POINT('',(0.,17.5,15.875));
#18943=CARTESIAN_POINT('Origin',(0.,17.3,16.075));
#18944=CARTESIAN_POINT('',(180.,17.5,16.275));
#18945=CARTESIAN_POINT('',(180.,17.1,15.875));
#18946=CARTESIAN_POINT('',(180.,11.5608626497484,10.3358626497484));
#18947=CARTESIAN_POINT('',(0.,17.1,15.875));
#18948=CARTESIAN_POINT('',(0.,17.5,16.275));
#18949=CARTESIAN_POINT('Origin',(0.,17.5,15.875));
#18950=CARTESIAN_POINT('',(180.,17.5,28.5666738879315));
#18951=CARTESIAN_POINT('',(0.,17.5,28.5666738879315));
#18952=CARTESIAN_POINT('',(180.,17.5,28.5666738879315));
#18953=CARTESIAN_POINT('Origin',(0.,0.25,25.15));
#18954=CARTESIAN_POINT('',(180.,0.,24.9));
#18955=CARTESIAN_POINT('',(180.,0.5,25.4));
#18956=CARTESIAN_POINT('',(180.,-3.49538735025162,21.4046126497484));
#18957=CARTESIAN_POINT('',(0.,0.5,25.4));
#18958=CARTESIAN_POINT('',(0.,0.,24.9));
#18959=CARTESIAN_POINT('Origin',(0.,0.,25.4));
#18960=CARTESIAN_POINT('',(180.,0.,-24.9));
#18961=CARTESIAN_POINT('',(0.,0.,-24.9));
#18962=CARTESIAN_POINT('',(180.,0.,0.));
#18963=CARTESIAN_POINT('Origin',(0.,0.25,-25.15));
#18964=CARTESIAN_POINT('',(180.,0.5,-25.4));
#18965=CARTESIAN_POINT('',(180.,-3.49538735025162,-21.4046126497484));
#18966=CARTESIAN_POINT('',(0.,0.5,-25.4));
#18967=CARTESIAN_POINT('Origin',(0.,22.225,-38.1));
#18968=CARTESIAN_POINT('',(180.,20.836901197987,-31.9035750859185));
#18969=CARTESIAN_POINT('',(0.,20.836901197987,-31.9035750859185));
#18970=CARTESIAN_POINT('',(180.,16.0285750859185,-36.711901197987));
#18971=CARTESIAN_POINT('Origin',(180.,22.225,-38.1));
#18972=CARTESIAN_POINT('',(0.,16.0285750859185,-36.711901197987));
#18973=CARTESIAN_POINT('Origin',(0.,4.71667388793148,-25.4));
#18974=CARTESIAN_POINT('',(180.,4.71667388793148,-25.4));
#18975=CARTESIAN_POINT('',(180.,4.71667388793148,-25.4));
#18976=CARTESIAN_POINT('',(0.,4.71667388793148,-25.4));
#18977=CARTESIAN_POINT('Origin',(0.,0.,-25.4));
#18978=CARTESIAN_POINT('',(180.,0.,-25.4));
#18979=CARTESIAN_POINT('Origin',(0.,4.71667388793148,25.4));
#18980=CARTESIAN_POINT('',(180.,4.71667388793148,25.4));
#18981=CARTESIAN_POINT('',(180.,0.,25.4));
#18982=CARTESIAN_POINT('',(0.,4.71667388793148,25.4));
#18983=CARTESIAN_POINT('Origin',(0.,16.0285750859185,36.711901197987));
#18984=CARTESIAN_POINT('',(180.,16.0285750859185,36.711901197987));
#18985=CARTESIAN_POINT('',(180.,4.71667388793148,25.4));
#18986=CARTESIAN_POINT('',(0.,16.0285750859185,36.711901197987));
#18987=CARTESIAN_POINT('Origin',(0.,22.225,38.1));
#18988=CARTESIAN_POINT('',(180.,20.836901197987,31.9035750859185));
#18989=CARTESIAN_POINT('Origin',(180.,22.225,38.1));
#18990=CARTESIAN_POINT('',(0.,20.836901197987,31.9035750859185));
#18991=CARTESIAN_POINT('Origin',(0.,17.5,28.5666738879315));
#18992=CARTESIAN_POINT('',(180.,20.836901197987,31.9035750859185));
#18993=CARTESIAN_POINT('Origin',(0.,12.5,15.875));
#18994=CARTESIAN_POINT('',(180.,17.5,15.875));
#18995=CARTESIAN_POINT('Origin',(0.,17.5,-28.5666738879315));
#18996=CARTESIAN_POINT('',(180.,17.5,-28.5666738879315));
#18997=CARTESIAN_POINT('',(180.,17.5,-28.5666738879315));
#18998=CARTESIAN_POINT('',(0.,17.5,-28.5666738879315));
#18999=CARTESIAN_POINT('Origin',(0.,20.836901197987,-31.9035750859185));
#19000=CARTESIAN_POINT('',(180.,20.836901197987,-31.9035750859185));
#19001=CARTESIAN_POINT('Origin',(180.,10.4184505989935,0.));
#19002=CARTESIAN_POINT('',(0.,0.,0.));
#19003=CARTESIAN_POINT('Origin',(137.6,52.2248,48.));
#19004=CARTESIAN_POINT('',(138.782171994385,52.0748000118745,43.917724971177));
#19005=CARTESIAN_POINT('',(137.907849128401,52.3748,43.4604263510609));
#19006=CARTESIAN_POINT('Ctrl Pts',(138.782171998071,52.0748000121059,43.9177249639598));
#19007=CARTESIAN_POINT('Ctrl Pts',(138.651976643645,52.1016376463417,43.8520818493382));
#19008=CARTESIAN_POINT('Ctrl Pts',(138.526269777382,52.1358607961625,43.7875586696316));
#19009=CARTESIAN_POINT('Ctrl Pts',(138.232505475659,52.2319385954063,43.6345597499497));
#19010=CARTESIAN_POINT('Ctrl Pts',(138.06786919821,52.2992964813024,43.5469549723518));
#19011=CARTESIAN_POINT('Ctrl Pts',(137.907849128401,52.3748000000001,43.4604263510608));
#19012=CARTESIAN_POINT('',(140.928421084005,52.3748,44.8977245306789));
#19013=CARTESIAN_POINT('Origin',(137.6,52.3748,48.));
#19014=CARTESIAN_POINT('',(140.022078380249,52.0748000118746,44.5077176008821));
#19015=CARTESIAN_POINT('Ctrl Pts',(140.928421084005,52.3748,44.897724530679));
#19016=CARTESIAN_POINT('Ctrl Pts',(140.760391286209,52.2993184802566,44.828152047826));
#19017=CARTESIAN_POINT('Ctrl Pts',(140.588616367553,52.2319776911148,44.755677770846));
#19018=CARTESIAN_POINT('Ctrl Pts',(140.284602785751,52.1358885558017,44.6242337550021));
#19019=CARTESIAN_POINT('Ctrl Pts',(140.155192346908,52.1016485689512,44.5673651425763));
#19020=CARTESIAN_POINT('Ctrl Pts',(140.022078383524,52.074800012106,44.5077175934691));
#19021=CARTESIAN_POINT('Origin',(137.6,52.0748,48.));
#19022=CARTESIAN_POINT('Origin',(90.,52.3748,0.));
#19023=CARTESIAN_POINT('',(146.35,52.3748,-56.35));
#19024=CARTESIAN_POINT('',(146.35,52.3748,56.35));
#19025=CARTESIAN_POINT('',(146.35,52.3748,28.575));
#19026=CARTESIAN_POINT('',(33.65,52.3748,-56.35));
#19027=CARTESIAN_POINT('',(118.575,52.3748,-56.35));
#19028=CARTESIAN_POINT('',(33.65,52.3748,56.35));
#19029=CARTESIAN_POINT('',(33.65,52.3748,-28.575));
#19030=CARTESIAN_POINT('',(61.425,52.3748,56.35));
#19031=CARTESIAN_POINT('',(114.05,52.3748,48.));
#19032=CARTESIAN_POINT('Origin',(118.6,52.3748,48.));
#19033=CARTESIAN_POINT('',(56.85,52.3748,-48.));
#19034=CARTESIAN_POINT('Origin',(61.4,52.3748,-48.));
#19035=CARTESIAN_POINT('',(56.85,52.3748,48.));
#19036=CARTESIAN_POINT('Origin',(61.4,52.3748,48.));
#19037=CARTESIAN_POINT('',(60.975,52.3748,19.05));
#19038=CARTESIAN_POINT('Origin',(64.6,52.3748,19.05));
#19039=CARTESIAN_POINT('',(140.928421084005,52.3748,-44.8977245306789));
#19040=CARTESIAN_POINT('',(137.907849128401,52.3748,-43.4604263510609));
#19041=CARTESIAN_POINT('Origin',(137.6,52.3748,-48.));
#19042=CARTESIAN_POINT('Origin',(140.8,52.3748,-41.275));
#19043=CARTESIAN_POINT('Origin',(140.8,52.3748,41.275));
#19044=CARTESIAN_POINT('',(111.775,52.3748,-19.05));
#19045=CARTESIAN_POINT('Origin',(115.4,52.3748,-19.05));
#19046=CARTESIAN_POINT('',(60.975,52.3748,-19.05));
#19047=CARTESIAN_POINT('Origin',(64.6,52.3748,-19.05));
#19048=CARTESIAN_POINT('',(39.071578915995,52.3748,44.8977245306789));
#19049=CARTESIAN_POINT('',(42.0921508715986,52.3748,43.4604263510609));
#19050=CARTESIAN_POINT('Origin',(42.4,52.3748,48.));
#19051=CARTESIAN_POINT('Origin',(39.2,52.3748,41.275));
#19052=CARTESIAN_POINT('',(42.0921508715986,52.3748,-43.4604263510609));
#19053=CARTESIAN_POINT('',(39.071578915995,52.3748,-44.8977245306789));
#19054=CARTESIAN_POINT('Origin',(42.4,52.3748,-48.));
#19055=CARTESIAN_POINT('Origin',(39.2,52.3748,-41.275));
#19056=CARTESIAN_POINT('',(111.775,52.3748,19.05));
#19057=CARTESIAN_POINT('Origin',(115.4,52.3748,19.05));
#19058=CARTESIAN_POINT('',(114.05,52.3748,-48.));
#19059=CARTESIAN_POINT('Origin',(118.6,52.3748,-48.));
#19060=CARTESIAN_POINT('Origin',(118.6,52.2248,48.));
#19061=CARTESIAN_POINT('',(114.35,52.0748,48.));
#19062=CARTESIAN_POINT('Origin',(118.6,52.0748,48.));
#19063=CARTESIAN_POINT('',(114.2,52.2248,48.));
#19064=CARTESIAN_POINT('Origin',(118.6,52.3748,48.));
#19065=CARTESIAN_POINT('',(114.35,47.1748,48.));
#19066=CARTESIAN_POINT('',(114.35,52.3748,48.));
#19067=CARTESIAN_POINT('Origin',(118.6,47.1748,48.));
#19068=CARTESIAN_POINT('Origin',(42.4,52.2248,-48.));
#19069=CARTESIAN_POINT('',(41.2178280056156,52.0748000118745,-43.917724971177));
#19070=CARTESIAN_POINT('Ctrl Pts',(41.217828001929,52.074800012106,-43.9177249639597));
#19071=CARTESIAN_POINT('Ctrl Pts',(41.3480233563548,52.1016376463417,-43.8520818493381));
#19072=CARTESIAN_POINT('Ctrl Pts',(41.4737302226176,52.1358607961625,-43.7875586696315));
#19073=CARTESIAN_POINT('Ctrl Pts',(41.7674945243411,52.2319385954063,-43.6345597499497));
#19074=CARTESIAN_POINT('Ctrl Pts',(41.9321308017903,52.2992964813023,-43.5469549723519));
#19075=CARTESIAN_POINT('Ctrl Pts',(42.0921508715986,52.3748,-43.4604263510609));
#19076=CARTESIAN_POINT('',(39.9779216197509,52.0748000118745,-44.5077176008821));
#19077=CARTESIAN_POINT('Ctrl Pts',(39.071578915995,52.3748,-44.897724530679));
#19078=CARTESIAN_POINT('Ctrl Pts',(39.2396087137915,52.2993184802566,-44.828152047826));
#19079=CARTESIAN_POINT('Ctrl Pts',(39.4113836324468,52.2319776911147,-44.755677770846));
#19080=CARTESIAN_POINT('Ctrl Pts',(39.7153972142493,52.1358885558017,-44.6242337550021));
#19081=CARTESIAN_POINT('Ctrl Pts',(39.8448076530922,52.1016485689511,-44.5673651425763));
#19082=CARTESIAN_POINT('Ctrl Pts',(39.9779216164758,52.074800012106,-44.5077175934691));
#19083=CARTESIAN_POINT('Origin',(42.4,52.0748,-48.));
#19084=CARTESIAN_POINT('Origin',(61.4,52.2248,-48.));
#19085=CARTESIAN_POINT('',(57.15,52.0748,-48.));
#19086=CARTESIAN_POINT('Origin',(61.4,52.0748,-48.));
#19087=CARTESIAN_POINT('',(57.,52.2248,-48.));
#19088=CARTESIAN_POINT('Origin',(61.4,52.3748,-48.));
#19089=CARTESIAN_POINT('',(57.15,47.1748,-48.));
#19090=CARTESIAN_POINT('',(57.15,52.3748,-48.));
#19091=CARTESIAN_POINT('Origin',(61.4,47.1748,-48.));
#19092=CARTESIAN_POINT('Origin',(42.4,52.2248,48.));
#19093=CARTESIAN_POINT('',(39.9779216197508,52.0748000118745,44.5077176008821));
#19094=CARTESIAN_POINT('Ctrl Pts',(39.9779216164758,52.074800012106,44.5077175934691));
#19095=CARTESIAN_POINT('Ctrl Pts',(39.8448618069091,52.1016376463417,44.5673408765836));
#19096=CARTESIAN_POINT('Ctrl Pts',(39.7155022091841,52.1358607961625,44.6241876128267));
#19097=CARTESIAN_POINT('Ctrl Pts',(39.4114832568764,52.2319385954063,44.7556357433902));
#19098=CARTESIAN_POINT('Ctrl Pts',(39.2396576857764,52.2992964813023,44.82813177105));
#19099=CARTESIAN_POINT('Ctrl Pts',(39.071578915995,52.3748,44.897724530679));
#19100=CARTESIAN_POINT('',(41.2178280056156,52.0748000118745,43.917724971177));
#19101=CARTESIAN_POINT('Ctrl Pts',(42.0921508715986,52.3748,43.4604263510609));
#19102=CARTESIAN_POINT('Ctrl Pts',(41.9321774257658,52.2993184802566,43.5469297610873));
#19103=CARTESIAN_POINT('Ctrl Pts',(41.7675899759767,52.2319776911147,43.6345089531068));
#19104=CARTESIAN_POINT('Ctrl Pts',(41.4738322546896,52.1358885558017,43.7875063008149));
#19105=CARTESIAN_POINT('Ctrl Pts',(41.3480763443713,52.1016485689512,43.8520551333431));
#19106=CARTESIAN_POINT('Ctrl Pts',(41.217828001929,52.074800012106,43.9177249639597));
#19107=CARTESIAN_POINT('Origin',(42.4,52.0748,48.));
#19108=CARTESIAN_POINT('Origin',(61.4,52.2248,48.));
#19109=CARTESIAN_POINT('',(57.15,52.0748,48.));
#19110=CARTESIAN_POINT('Origin',(61.4,52.0748,48.));
#19111=CARTESIAN_POINT('',(57.,52.2248,48.));
#19112=CARTESIAN_POINT('Origin',(61.4,52.3748,48.));
#19113=CARTESIAN_POINT('',(57.15,47.1748,48.));
#19114=CARTESIAN_POINT('',(57.15,52.3748,48.));
#19115=CARTESIAN_POINT('Origin',(61.4,47.1748,48.));
#19116=CARTESIAN_POINT('Origin',(118.6,52.2248,-48.));
#19117=CARTESIAN_POINT('',(114.35,52.0748,-48.));
#19118=CARTESIAN_POINT('Origin',(118.6,52.0748,-48.));
#19119=CARTESIAN_POINT('',(114.2,52.2248,-48.));
#19120=CARTESIAN_POINT('Origin',(118.6,52.3748,-48.));
#19121=CARTESIAN_POINT('',(114.35,47.1748,-48.));
#19122=CARTESIAN_POINT('',(114.35,52.3748,-48.));
#19123=CARTESIAN_POINT('Origin',(118.6,47.1748,-48.));
#19124=CARTESIAN_POINT('Origin',(137.6,52.2248,-48.));
#19125=CARTESIAN_POINT('',(140.022078380249,52.0748000118745,-44.5077176008821));
#19126=CARTESIAN_POINT('Ctrl Pts',(140.022078383524,52.074800012106,-44.5077175934691));
#19127=CARTESIAN_POINT('Ctrl Pts',(140.155138193091,52.1016376463417,-44.5673408765836));
#19128=CARTESIAN_POINT('Ctrl Pts',(140.284497790816,52.1358607961625,-44.6241876128266));
#19129=CARTESIAN_POINT('Ctrl Pts',(140.588516743124,52.2319385954063,-44.7556357433902));
#19130=CARTESIAN_POINT('Ctrl Pts',(140.760342314224,52.2992964813023,-44.8281317710499));
#19131=CARTESIAN_POINT('Ctrl Pts',(140.928421084005,52.3748,-44.8977245306789));
#19132=CARTESIAN_POINT('',(138.782171994385,52.0748000118745,-43.917724971177));
#19133=CARTESIAN_POINT('Ctrl Pts',(137.907849128401,52.3748000000001,-43.4604263510607));
#19134=CARTESIAN_POINT('Ctrl Pts',(138.067822574234,52.2993184802567,-43.5469297610872));
#19135=CARTESIAN_POINT('Ctrl Pts',(138.232410024023,52.2319776911148,-43.6345089531068));
#19136=CARTESIAN_POINT('Ctrl Pts',(138.526167745311,52.1358885558016,-43.7875063008149));
#19137=CARTESIAN_POINT('Ctrl Pts',(138.651923655629,52.1016485689511,-43.8520551333431));
#19138=CARTESIAN_POINT('Ctrl Pts',(138.782171998071,52.0748000121059,-43.9177249639598));
#19139=CARTESIAN_POINT('Origin',(137.6,52.0748,-48.));
#19140=CARTESIAN_POINT('Origin',(137.6,52.3748,-48.));
#19141=CARTESIAN_POINT('',(139.13467476064,51.9748,-44.0367597374051));
#19142=CARTESIAN_POINT('Ctrl Pts',(139.13467476064,51.9748000000001,-44.036759737405));
#19143=CARTESIAN_POINT('Ctrl Pts',(139.018142335558,51.9963321756324,-43.9916352030039));
#19144=CARTESIAN_POINT('Ctrl Pts',(138.899881099053,52.0304589029105,-43.9518119506536));
#19145=CARTESIAN_POINT('Ctrl Pts',(138.782171996941,52.0748000225489,-43.9177249762358));
#19146=CARTESIAN_POINT('',(139.13467476064,47.1748,-44.0367597374051));
#19147=CARTESIAN_POINT('',(139.13467476064,52.3748,-44.0367597374051));
#19148=CARTESIAN_POINT('',(139.707364790884,47.1748,-44.3092665175952));
#19149=CARTESIAN_POINT('Origin',(137.6,47.1748,-48.));
#19150=CARTESIAN_POINT('',(139.707364790884,51.9748,-44.3092665175952));
#19151=CARTESIAN_POINT('',(139.707364790884,52.3748,-44.3092665175952));
#19152=CARTESIAN_POINT('Ctrl Pts',(140.022078374711,52.074800022549,-44.5077176020895));
#19153=CARTESIAN_POINT('Ctrl Pts',(139.921436670535,52.0304833142233,-44.4379173776217));
#19154=CARTESIAN_POINT('Ctrl Pts',(139.81593061941,51.9963413043493,-44.3712563105783));
#19155=CARTESIAN_POINT('Ctrl Pts',(139.707364790884,51.9748000000001,-44.3092665175953));
#19156=CARTESIAN_POINT('Origin',(137.6,47.1748,-48.));
#19157=CARTESIAN_POINT('Origin',(140.8,47.1748,-41.275));
#19158=CARTESIAN_POINT('',(135.,47.1748,-48.));
#19159=CARTESIAN_POINT('Origin',(137.6,47.1748,-48.));
#19160=CARTESIAN_POINT('Origin',(118.6,47.1748,-48.));
#19161=CARTESIAN_POINT('',(116.,47.1748,-48.));
#19162=CARTESIAN_POINT('Origin',(118.6,47.1748,-48.));
#19163=CARTESIAN_POINT('Origin',(61.4,47.1748,48.));
#19164=CARTESIAN_POINT('',(58.8,47.1748,48.));
#19165=CARTESIAN_POINT('Origin',(61.4,47.1748,48.));
#19166=CARTESIAN_POINT('Origin',(42.4,52.3748,48.));
#19167=CARTESIAN_POINT('',(40.8653252393596,51.9748,44.0367597374051));
#19168=CARTESIAN_POINT('Ctrl Pts',(40.8653252393596,51.9748,44.0367597374051));
#19169=CARTESIAN_POINT('Ctrl Pts',(40.9818576644415,51.9963321756324,43.991635203004));
#19170=CARTESIAN_POINT('Ctrl Pts',(41.1001189009476,52.0304589029105,43.9518119506536));
#19171=CARTESIAN_POINT('Ctrl Pts',(41.2178280030595,52.074800022549,43.9177249762357));
#19172=CARTESIAN_POINT('',(40.8653252393596,47.1748,44.0367597374051));
#19173=CARTESIAN_POINT('',(40.8653252393596,52.3748,44.0367597374051));
#19174=CARTESIAN_POINT('',(40.2926352091164,47.1748,44.3092665175952));
#19175=CARTESIAN_POINT('Origin',(42.4,47.1748,48.));
#19176=CARTESIAN_POINT('',(40.2926352091163,51.9748,44.3092665175952));
#19177=CARTESIAN_POINT('',(40.2926352091164,52.3748,44.3092665175952));
#19178=CARTESIAN_POINT('Ctrl Pts',(39.9779216252887,52.074800022549,44.5077176020895));
#19179=CARTESIAN_POINT('Ctrl Pts',(40.0785633294647,52.0304833142233,44.4379173776217));
#19180=CARTESIAN_POINT('Ctrl Pts',(40.1840693805898,51.9963413043492,44.3712563105783));
#19181=CARTESIAN_POINT('Ctrl Pts',(40.2926352091163,51.9748,44.3092665175952));
#19182=CARTESIAN_POINT('Origin',(42.4,47.1748,48.));
#19183=CARTESIAN_POINT('Origin',(39.2,47.1748,41.275));
#19184=CARTESIAN_POINT('',(39.8,47.1748,48.));
#19185=CARTESIAN_POINT('Origin',(42.4,47.1748,48.));
#19186=CARTESIAN_POINT('Origin',(61.4,47.1748,-48.));
#19187=CARTESIAN_POINT('',(58.8,47.1748,-48.));
#19188=CARTESIAN_POINT('Origin',(61.4,47.1748,-48.));
#19189=CARTESIAN_POINT('Origin',(42.4,52.3748,-48.));
#19190=CARTESIAN_POINT('',(40.2926352091163,51.9748,-44.3092665175952));
#19191=CARTESIAN_POINT('Ctrl Pts',(40.2926352091163,51.9748,-44.3092665175952));
#19192=CARTESIAN_POINT('Ctrl Pts',(40.1841153883286,51.9963321756324,-44.3712300407083));
#19193=CARTESIAN_POINT('Ctrl Pts',(40.0786187667076,52.0304589029105,-44.437878929028));
#19194=CARTESIAN_POINT('Ctrl Pts',(39.9779216252887,52.074800022549,-44.5077176020895));
#19195=CARTESIAN_POINT('',(40.2926352091164,47.1748,-44.3092665175952));
#19196=CARTESIAN_POINT('',(40.2926352091164,52.3748,-44.3092665175952));
#19197=CARTESIAN_POINT('',(40.8653252393596,47.1748,-44.0367597374051));
#19198=CARTESIAN_POINT('Origin',(42.4,47.1748,-48.));
#19199=CARTESIAN_POINT('',(40.8653252393596,51.9748,-44.0367597374051));
#19200=CARTESIAN_POINT('',(40.8653252393596,52.3748,-44.0367597374051));
#19201=CARTESIAN_POINT('Ctrl Pts',(41.2178280030594,52.074800022549,-43.9177249762357));
#19202=CARTESIAN_POINT('Ctrl Pts',(41.1001837038604,52.0304833142233,-43.9517931846007));
#19203=CARTESIAN_POINT('Ctrl Pts',(40.98190706918,51.9963413043492,-43.9916160721413));
#19204=CARTESIAN_POINT('Ctrl Pts',(40.8653252393596,51.9748,-44.0367597374051));
#19205=CARTESIAN_POINT('Origin',(42.4,47.1748,-48.));
#19206=CARTESIAN_POINT('Origin',(39.2,47.1748,-41.275));
#19207=CARTESIAN_POINT('',(39.8,47.1748,-48.));
#19208=CARTESIAN_POINT('Origin',(42.4,47.1748,-48.));
#19209=CARTESIAN_POINT('Origin',(118.6,47.1748,48.));
#19210=CARTESIAN_POINT('',(116.,47.1748,48.));
#19211=CARTESIAN_POINT('Origin',(118.6,47.1748,48.));
#19212=CARTESIAN_POINT('Origin',(137.6,52.3748,48.));
#19213=CARTESIAN_POINT('',(139.707364790884,51.9748,44.3092665175952));
#19214=CARTESIAN_POINT('Ctrl Pts',(139.707364790884,51.9748000000001,44.3092665175953));
#19215=CARTESIAN_POINT('Ctrl Pts',(139.815884611672,51.9963321756325,44.3712300407084));
#19216=CARTESIAN_POINT('Ctrl Pts',(139.921381233292,52.0304589029105,44.4378789290281));
#19217=CARTESIAN_POINT('Ctrl Pts',(140.022078374711,52.074800022549,44.5077176020895));
#19218=CARTESIAN_POINT('',(139.707364790884,47.1748,44.3092665175952));
#19219=CARTESIAN_POINT('',(139.707364790884,52.3748,44.3092665175952));
#19220=CARTESIAN_POINT('',(139.13467476064,47.1748,44.0367597374051));
#19221=CARTESIAN_POINT('Origin',(137.6,47.1748,48.));
#19222=CARTESIAN_POINT('',(139.13467476064,51.9748,44.0367597374051));
#19223=CARTESIAN_POINT('',(139.13467476064,52.3748,44.0367597374051));
#19224=CARTESIAN_POINT('Ctrl Pts',(138.782171996941,52.074800022549,43.9177249762358));
#19225=CARTESIAN_POINT('Ctrl Pts',(138.89981629614,52.0304833142233,43.9517931846007));
#19226=CARTESIAN_POINT('Ctrl Pts',(139.01809293082,51.9963413043493,43.9916160721412));
#19227=CARTESIAN_POINT('Ctrl Pts',(139.13467476064,51.9748000000001,44.036759737405));
#19228=CARTESIAN_POINT('Origin',(137.6,47.1748,48.));
#19229=CARTESIAN_POINT('Origin',(140.8,47.1748,41.275));
#19230=CARTESIAN_POINT('',(135.,47.1748,48.));
#19231=CARTESIAN_POINT('Origin',(137.6,47.1748,48.));
#19232=CARTESIAN_POINT('Origin',(140.8,52.1748,-41.275));
#19233=CARTESIAN_POINT('',(137.575,51.9748,-41.275));
#19234=CARTESIAN_POINT('Origin',(140.8,51.9748,-41.275));
#19235=CARTESIAN_POINT('Origin',(140.8,51.9748,-41.275));
#19236=CARTESIAN_POINT('Origin',(39.2,52.1748,41.275));
#19237=CARTESIAN_POINT('',(35.975,51.9748,41.275));
#19238=CARTESIAN_POINT('Origin',(39.2,51.9748,41.275));
#19239=CARTESIAN_POINT('Origin',(39.2,51.9748,41.275));
#19240=CARTESIAN_POINT('Origin',(39.2,52.1748,-41.275));
#19241=CARTESIAN_POINT('',(35.975,51.9748,-41.275));
#19242=CARTESIAN_POINT('Origin',(39.2,51.9748,-41.275));
#19243=CARTESIAN_POINT('Origin',(39.2,51.9748,-41.275));
#19244=CARTESIAN_POINT('Origin',(140.8,52.1748,41.275));
#19245=CARTESIAN_POINT('',(137.575,51.9748,41.275));
#19246=CARTESIAN_POINT('Origin',(140.8,51.9748,41.275));
#19247=CARTESIAN_POINT('Origin',(140.8,51.9748,41.275));
#19248=CARTESIAN_POINT('Origin',(137.6,52.3748,-48.));
#19249=CARTESIAN_POINT('',(135.,39.6748,-48.));
#19250=CARTESIAN_POINT('',(135.,52.3748,-48.));
#19251=CARTESIAN_POINT('Origin',(137.6,39.6748,-48.));
#19252=CARTESIAN_POINT('Origin',(118.6,52.3748,-48.));
#19253=CARTESIAN_POINT('',(116.,39.6748,-48.));
#19254=CARTESIAN_POINT('',(116.,52.3748,-48.));
#19255=CARTESIAN_POINT('Origin',(118.6,39.6748,-48.));
#19256=CARTESIAN_POINT('Origin',(61.4,52.3748,48.));
#19257=CARTESIAN_POINT('',(58.8,39.6748,48.));
#19258=CARTESIAN_POINT('',(58.8,52.3748,48.));
#19259=CARTESIAN_POINT('Origin',(61.4,39.6748,48.));
#19260=CARTESIAN_POINT('Origin',(42.4,52.3748,48.));
#19261=CARTESIAN_POINT('',(39.8,39.6748,48.));
#19262=CARTESIAN_POINT('',(39.8,52.3748,48.));
#19263=CARTESIAN_POINT('Origin',(42.4,39.6748,48.));
#19264=CARTESIAN_POINT('Origin',(61.4,52.3748,-48.));
#19265=CARTESIAN_POINT('',(58.8,39.6748,-48.));
#19266=CARTESIAN_POINT('',(58.8,52.3748,-48.));
#19267=CARTESIAN_POINT('Origin',(61.4,39.6748,-48.));
#19268=CARTESIAN_POINT('Origin',(42.4,52.3748,-48.));
#19269=CARTESIAN_POINT('',(39.8,39.6748,-48.));
#19270=CARTESIAN_POINT('',(39.8,52.3748,-48.));
#19271=CARTESIAN_POINT('Origin',(42.4,39.6748,-48.));
#19272=CARTESIAN_POINT('Origin',(118.6,52.3748,48.));
#19273=CARTESIAN_POINT('',(116.,39.6748,48.));
#19274=CARTESIAN_POINT('',(116.,52.3748,48.));
#19275=CARTESIAN_POINT('Origin',(118.6,39.6748,48.));
#19276=CARTESIAN_POINT('Origin',(137.6,52.3748,48.));
#19277=CARTESIAN_POINT('',(135.,39.6748,48.));
#19278=CARTESIAN_POINT('',(135.,52.3748,48.));
#19279=CARTESIAN_POINT('Origin',(137.6,39.6748,48.));
#19280=CARTESIAN_POINT('Origin',(115.4,52.1748,19.05));
#19281=CARTESIAN_POINT('',(112.175,51.9748,19.05));
#19282=CARTESIAN_POINT('Origin',(115.4,51.9748,19.05));
#19283=CARTESIAN_POINT('',(111.975,52.1748,19.05));
#19284=CARTESIAN_POINT('Origin',(115.4,52.3748,19.05));
#19285=CARTESIAN_POINT('',(112.175,42.3748,19.05));
#19286=CARTESIAN_POINT('',(112.175,52.3748,19.05));
#19287=CARTESIAN_POINT('Origin',(115.4,42.3748,19.05));
#19288=CARTESIAN_POINT('Origin',(64.6,52.1748,19.05));
#19289=CARTESIAN_POINT('',(61.375,51.9748,19.05));
#19290=CARTESIAN_POINT('Origin',(64.6,51.9748,19.05));
#19291=CARTESIAN_POINT('',(61.175,52.1748,19.05));
#19292=CARTESIAN_POINT('Origin',(64.6,52.3748,19.05));
#19293=CARTESIAN_POINT('',(61.375,42.3748,19.05));
#19294=CARTESIAN_POINT('',(61.375,52.3748,19.05));
#19295=CARTESIAN_POINT('Origin',(64.6,42.3748,19.05));
#19296=CARTESIAN_POINT('Origin',(39.2,52.3748,-41.275));
#19297=CARTESIAN_POINT('',(35.975,42.3748,-41.275));
#19298=CARTESIAN_POINT('',(35.975,52.3748,-41.275));
#19299=CARTESIAN_POINT('Origin',(39.2,42.3748,-41.275));
#19300=CARTESIAN_POINT('Origin',(140.8,52.3748,-41.275));
#19301=CARTESIAN_POINT('',(137.575,42.3748,-41.275));
#19302=CARTESIAN_POINT('',(137.575,52.3748,-41.275));
#19303=CARTESIAN_POINT('Origin',(140.8,42.3748,-41.275));
#19304=CARTESIAN_POINT('Origin',(39.2,52.3748,41.275));
#19305=CARTESIAN_POINT('',(35.975,42.3748,41.275));
#19306=CARTESIAN_POINT('',(35.975,52.3748,41.275));
#19307=CARTESIAN_POINT('Origin',(39.2,42.3748,41.275));
#19308=CARTESIAN_POINT('Origin',(140.8,52.3748,41.275));
#19309=CARTESIAN_POINT('',(137.575,42.3748,41.275));
#19310=CARTESIAN_POINT('',(137.575,52.3748,41.275));
#19311=CARTESIAN_POINT('Origin',(140.8,42.3748,41.275));
#19312=CARTESIAN_POINT('Origin',(64.6,52.1748,-19.05));
#19313=CARTESIAN_POINT('',(61.375,51.9748,-19.05));
#19314=CARTESIAN_POINT('Origin',(64.6,51.9748,-19.05));
#19315=CARTESIAN_POINT('',(61.175,52.1748,-19.05));
#19316=CARTESIAN_POINT('Origin',(64.6,52.3748,-19.05));
#19317=CARTESIAN_POINT('',(61.375,42.3748,-19.05));
#19318=CARTESIAN_POINT('',(61.375,52.3748,-19.05));
#19319=CARTESIAN_POINT('Origin',(64.6,42.3748,-19.05));
#19320=CARTESIAN_POINT('Origin',(115.4,52.1748,-19.05));
#19321=CARTESIAN_POINT('',(112.175,51.9748,-19.05));
#19322=CARTESIAN_POINT('Origin',(115.4,51.9748,-19.05));
#19323=CARTESIAN_POINT('',(111.975,52.1748,-19.05));
#19324=CARTESIAN_POINT('Origin',(115.4,52.3748,-19.05));
#19325=CARTESIAN_POINT('',(112.175,42.3748,-19.05));
#19326=CARTESIAN_POINT('',(112.175,52.3748,-19.05));
#19327=CARTESIAN_POINT('Origin',(115.4,42.3748,-19.05));
#19328=CARTESIAN_POINT('Origin',(115.4,42.3748,19.05));
#19329=CARTESIAN_POINT('',(115.4,40.4370245036361,19.05));
#19330=CARTESIAN_POINT('',(112.175,42.3748,19.05));
#19331=CARTESIAN_POINT('Origin',(115.4,42.3748,-19.05));
#19332=CARTESIAN_POINT('',(115.4,40.4370245036361,-19.05));
#19333=CARTESIAN_POINT('',(112.175,42.3748,-19.05));
#19334=CARTESIAN_POINT('Origin',(64.6,42.3748,19.05));
#19335=CARTESIAN_POINT('',(64.6,40.4370245036361,19.05));
#19336=CARTESIAN_POINT('',(61.375,42.3748,19.05));
#19337=CARTESIAN_POINT('Origin',(64.6,42.3748,-19.05));
#19338=CARTESIAN_POINT('',(64.6,40.4370245036361,-19.05));
#19339=CARTESIAN_POINT('',(61.375,42.3748,-19.05));
#19340=CARTESIAN_POINT('Origin',(140.8,42.3748,41.275));
#19341=CARTESIAN_POINT('',(140.8,40.4370245036361,41.275));
#19342=CARTESIAN_POINT('',(137.575,42.3748,41.275));
#19343=CARTESIAN_POINT('Origin',(140.8,42.3748,-41.275));
#19344=CARTESIAN_POINT('',(140.8,40.4370245036361,-41.275));
#19345=CARTESIAN_POINT('',(137.575,42.3748,-41.275));
#19346=CARTESIAN_POINT('Origin',(39.2,42.3748,41.275));
#19347=CARTESIAN_POINT('',(39.2,40.4370245036361,41.275));
#19348=CARTESIAN_POINT('',(35.975,42.3748,41.275));
#19349=CARTESIAN_POINT('Origin',(39.2,42.3748,-41.275));
#19350=CARTESIAN_POINT('',(39.2,40.4370245036361,-41.275));
#19351=CARTESIAN_POINT('',(35.975,42.3748,-41.275));
#19352=CARTESIAN_POINT('Origin',(146.75,51.9748,28.575));
#19353=CARTESIAN_POINT('',(147.15,51.5748,57.15));
#19354=CARTESIAN_POINT('',(146.35,52.3748,56.35));
#19355=CARTESIAN_POINT('',(147.15,51.5748,-57.15));
#19356=CARTESIAN_POINT('',(147.15,51.5748,28.575));
#19357=CARTESIAN_POINT('',(146.35,52.3748,-56.35));
#19358=CARTESIAN_POINT('Origin',(61.425,51.9748,56.75));
#19359=CARTESIAN_POINT('',(32.85,51.5748,57.15));
#19360=CARTESIAN_POINT('',(33.65,52.3748,56.35));
#19361=CARTESIAN_POINT('',(61.425,51.5748,57.15));
#19362=CARTESIAN_POINT('Origin',(33.25,51.9748,-28.575));
#19363=CARTESIAN_POINT('',(32.85,51.5748,-57.15));
#19364=CARTESIAN_POINT('',(33.65,52.3748,-56.35));
#19365=CARTESIAN_POINT('',(32.85,51.5748,-28.575));
#19366=CARTESIAN_POINT('Origin',(118.575,51.9748,-56.75));
#19367=CARTESIAN_POINT('',(118.575,51.5748,-57.15));
#19368=CARTESIAN_POINT('Origin',(147.15,39.6748,-57.15));
#19369=CARTESIAN_POINT('',(147.15,39.6748,-57.15));
#19370=CARTESIAN_POINT('',(147.15,39.6748,-57.15));
#19371=CARTESIAN_POINT('',(32.85,39.6748,-57.15));
#19372=CARTESIAN_POINT('',(32.85,39.6748,-57.15));
#19373=CARTESIAN_POINT('',(32.85,39.6748,-57.15));
#19374=CARTESIAN_POINT('Origin',(147.15,39.6748,57.15));
#19375=CARTESIAN_POINT('',(147.15,39.6748,57.15));
#19376=CARTESIAN_POINT('',(147.15,39.6748,57.15));
#19377=CARTESIAN_POINT('',(147.15,39.6748,-57.15));
#19378=CARTESIAN_POINT('Origin',(32.85,39.6748,-57.15));
#19379=CARTESIAN_POINT('',(32.85,39.6748,57.15));
#19380=CARTESIAN_POINT('',(32.85,39.6748,57.15));
#19381=CARTESIAN_POINT('',(32.85,39.6748,57.15));
#19382=CARTESIAN_POINT('Origin',(32.85,39.6748,57.15));
#19383=CARTESIAN_POINT('',(147.15,39.6748,57.15));
#19384=CARTESIAN_POINT('Origin',(90.,39.6748,0.));
#19385=CARTESIAN_POINT('',(0.,0.,0.));
#19386=CARTESIAN_POINT('Origin',(160.,20.386522368915,36.261522368915));
#19387=CARTESIAN_POINT('',(160.,16.3443798161838,35.7040020338711));
#19388=CARTESIAN_POINT('',(160.,19.8290020338711,32.2193798161838));
#19389=CARTESIAN_POINT('Ctrl Pts',(160.,16.3443798161838,35.7040020338711));
#19390=CARTESIAN_POINT('Ctrl Pts',(160.313121048202,16.3443798161838,35.7040020338711));
#19391=CARTESIAN_POINT('Ctrl Pts',(160.644530562725,16.3694605042293,35.639628490954));
#19392=CARTESIAN_POINT('Ctrl Pts',(161.250438810992,16.4794607587991,35.3926861336962));
#19393=CARTESIAN_POINT('Ctrl Pts',(161.525274451059,16.5655176229446,35.2114538079158));
#19394=CARTESIAN_POINT('Ctrl Pts',(161.9591552462,16.7847783338415,34.8171144138708));
#19395=CARTESIAN_POINT('Ctrl Pts',(162.148303695899,16.9331965285742,34.5767521893323));
#19396=CARTESIAN_POINT('Ctrl Pts',(162.400811747278,17.2971590391485,34.083429001318));
#19397=CARTESIAN_POINT('Ctrl Pts',(162.464,17.5136583227266,33.8310855562043));
#19398=CARTESIAN_POINT('Ctrl Pts',(162.464,17.9560855562043,33.3886583227266));
#19399=CARTESIAN_POINT('Ctrl Pts',(162.400811747278,18.208429001318,33.1721590391485));
#19400=CARTESIAN_POINT('Ctrl Pts',(162.148303695899,18.7017521893323,32.8081965285742));
#19401=CARTESIAN_POINT('Ctrl Pts',(161.9591552462,18.9421144138708,32.6597783338415));
#19402=CARTESIAN_POINT('Ctrl Pts',(161.525274451059,19.3364538079158,32.4405176229446));
#19403=CARTESIAN_POINT('Ctrl Pts',(161.250438810992,19.5176861336962,32.3544607587991));
#19404=CARTESIAN_POINT('Ctrl Pts',(160.644530562725,19.764628490954,32.2444605042293));
#19405=CARTESIAN_POINT('Ctrl Pts',(160.313121048202,19.8290020338711,32.2193798161838));
#19406=CARTESIAN_POINT('Ctrl Pts',(160.,19.8290020338711,32.2193798161838));
#19407=CARTESIAN_POINT('Ctrl Pts',(160.,19.8290020338711,32.2193798161838));
#19408=CARTESIAN_POINT('Ctrl Pts',(159.686878951798,19.8290020338711,32.2193798161838));
#19409=CARTESIAN_POINT('Ctrl Pts',(159.355469437275,19.764628490954,32.2444605042293));
#19410=CARTESIAN_POINT('Ctrl Pts',(158.749561189008,19.5176861336961,32.3544607587991));
#19411=CARTESIAN_POINT('Ctrl Pts',(158.474725548941,19.3364538079158,32.4405176229446));
#19412=CARTESIAN_POINT('Ctrl Pts',(158.0408447538,18.9421144138708,32.6597783338415));
#19413=CARTESIAN_POINT('Ctrl Pts',(157.851696304101,18.7017521893323,32.8081965285742));
#19414=CARTESIAN_POINT('Ctrl Pts',(157.599188252722,18.208429001318,33.1721590391485));
#19415=CARTESIAN_POINT('Ctrl Pts',(157.536,17.9560855562043,33.3886583227266));
#19416=CARTESIAN_POINT('Ctrl Pts',(157.536,17.5136583227266,33.8310855562043));
#19417=CARTESIAN_POINT('Ctrl Pts',(157.599188252722,17.2971590391485,34.083429001318));
#19418=CARTESIAN_POINT('Ctrl Pts',(157.851696304101,16.9331965285742,34.5767521893323));
#19419=CARTESIAN_POINT('Ctrl Pts',(158.0408447538,16.7847783338415,34.8171144138708));
#19420=CARTESIAN_POINT('Ctrl Pts',(158.474725548941,16.5655176229446,35.2114538079158));
#19421=CARTESIAN_POINT('Ctrl Pts',(158.749561189008,16.4794607587991,35.3926861336961));
#19422=CARTESIAN_POINT('Ctrl Pts',(159.355469437275,16.3694605042293,35.639628490954));
#19423=CARTESIAN_POINT('Ctrl Pts',(159.686878951798,16.3443798161838,35.7040020338711));
#19424=CARTESIAN_POINT('Ctrl Pts',(160.,16.3443798161838,35.7040020338711));
#19425=CARTESIAN_POINT('',(160.,25.1340372978015,37.5244150801141));
#19426=CARTESIAN_POINT('',(160.,22.1288334777587,34.5192112600714));
#19427=CARTESIAN_POINT('Origin',(160.,23.3917261889578,39.2667261889578));
#19428=CARTESIAN_POINT('Origin',(160.,23.3917261889578,39.2667261889578));
#19429=CARTESIAN_POINT('',(160.,24.4523863607376,40.3273863607376));
#19430=CARTESIAN_POINT('',(160.,25.1340372978015,37.5244150801141));
#19431=CARTESIAN_POINT('Origin',(90.,20.386522368915,36.261522368915));
#19432=CARTESIAN_POINT('',(90.,16.3443798161838,35.7040020338711));
#19433=CARTESIAN_POINT('',(90.,19.8290020338711,32.2193798161838));
#19434=CARTESIAN_POINT('Ctrl Pts',(90.,16.3443798161838,35.7040020338711));
#19435=CARTESIAN_POINT('Ctrl Pts',(90.3131210482019,16.3443798161838,35.7040020338711));
#19436=CARTESIAN_POINT('Ctrl Pts',(90.6445305627248,16.3694605042293,35.639628490954));
#19437=CARTESIAN_POINT('Ctrl Pts',(91.2504388109923,16.4794607587991,35.3926861336961));
#19438=CARTESIAN_POINT('Ctrl Pts',(91.525274451059,16.5655176229446,35.2114538079158));
#19439=CARTESIAN_POINT('Ctrl Pts',(91.9591552462002,16.7847783338415,34.8171144138708));
#19440=CARTESIAN_POINT('Ctrl Pts',(92.1483036958993,16.9331965285742,34.5767521893323));
#19441=CARTESIAN_POINT('Ctrl Pts',(92.4008117472775,17.2971590391485,34.0834290013181));
#19442=CARTESIAN_POINT('Ctrl Pts',(92.464,17.5136583227266,33.8310855562043));
#19443=CARTESIAN_POINT('Ctrl Pts',(92.464,17.9560855562043,33.3886583227266));
#19444=CARTESIAN_POINT('Ctrl Pts',(92.4008117472775,18.208429001318,33.1721590391485));
#19445=CARTESIAN_POINT('Ctrl Pts',(92.1483036958993,18.7017521893323,32.8081965285742));
#19446=CARTESIAN_POINT('Ctrl Pts',(91.9591552462002,18.9421144138708,32.6597783338415));
#19447=CARTESIAN_POINT('Ctrl Pts',(91.525274451059,19.3364538079158,32.4405176229446));
#19448=CARTESIAN_POINT('Ctrl Pts',(91.2504388109923,19.5176861336961,32.3544607587991));
#19449=CARTESIAN_POINT('Ctrl Pts',(90.6445305627248,19.764628490954,32.2444605042293));
#19450=CARTESIAN_POINT('Ctrl Pts',(90.3131210482019,19.8290020338711,32.2193798161838));
#19451=CARTESIAN_POINT('Ctrl Pts',(90.,19.8290020338711,32.2193798161838));
#19452=CARTESIAN_POINT('Ctrl Pts',(90.,19.8290020338711,32.2193798161838));
#19453=CARTESIAN_POINT('Ctrl Pts',(89.6868789517981,19.8290020338711,32.2193798161838));
#19454=CARTESIAN_POINT('Ctrl Pts',(89.3554694372752,19.764628490954,32.2444605042293));
#19455=CARTESIAN_POINT('Ctrl Pts',(88.7495611890077,19.5176861336961,32.3544607587991));
#19456=CARTESIAN_POINT('Ctrl Pts',(88.474725548941,19.3364538079158,32.4405176229446));
#19457=CARTESIAN_POINT('Ctrl Pts',(88.0408447537999,18.9421144138708,32.6597783338415));
#19458=CARTESIAN_POINT('Ctrl Pts',(87.8516963041007,18.7017521893323,32.8081965285742));
#19459=CARTESIAN_POINT('Ctrl Pts',(87.5991882527224,18.208429001318,33.1721590391485));
#19460=CARTESIAN_POINT('Ctrl Pts',(87.536,17.9560855562043,33.3886583227266));
#19461=CARTESIAN_POINT('Ctrl Pts',(87.536,17.5136583227266,33.8310855562043));
#19462=CARTESIAN_POINT('Ctrl Pts',(87.5991882527224,17.2971590391485,34.0834290013181));
#19463=CARTESIAN_POINT('Ctrl Pts',(87.8516963041007,16.9331965285742,34.5767521893323));
#19464=CARTESIAN_POINT('Ctrl Pts',(88.0408447537999,16.7847783338415,34.8171144138708));
#19465=CARTESIAN_POINT('Ctrl Pts',(88.474725548941,16.5655176229446,35.2114538079158));
#19466=CARTESIAN_POINT('Ctrl Pts',(88.7495611890077,16.4794607587991,35.3926861336961));
#19467=CARTESIAN_POINT('Ctrl Pts',(89.3554694372752,16.3694605042293,35.639628490954));
#19468=CARTESIAN_POINT('Ctrl Pts',(89.6868789517981,16.3443798161838,35.7040020338711));
#19469=CARTESIAN_POINT('Ctrl Pts',(90.,16.3443798161838,35.7040020338711));
#19470=CARTESIAN_POINT('',(90.,25.1340372978015,37.5244150801141));
#19471=CARTESIAN_POINT('',(90.,22.1288334777587,34.5192112600714));
#19472=CARTESIAN_POINT('Origin',(90.,23.3917261889578,39.2667261889578));
#19473=CARTESIAN_POINT('Origin',(90.,23.3917261889578,39.2667261889578));
#19474=CARTESIAN_POINT('',(90.,24.4523863607376,40.3273863607376));
#19475=CARTESIAN_POINT('',(90.,25.1340372978015,37.5244150801141));
#19476=CARTESIAN_POINT('Origin',(20.,20.386522368915,36.261522368915));
#19477=CARTESIAN_POINT('',(20.,16.3443798161838,35.7040020338711));
#19478=CARTESIAN_POINT('',(20.,19.8290020338711,32.2193798161838));
#19479=CARTESIAN_POINT('Ctrl Pts',(20.,16.3443798161838,35.7040020338711));
#19480=CARTESIAN_POINT('Ctrl Pts',(20.3131210482019,16.3443798161838,35.7040020338711));
#19481=CARTESIAN_POINT('Ctrl Pts',(20.6445305627248,16.3694605042293,35.639628490954));
#19482=CARTESIAN_POINT('Ctrl Pts',(21.2504388109924,16.4794607587991,35.3926861336961));
#19483=CARTESIAN_POINT('Ctrl Pts',(21.525274451059,16.5655176229446,35.2114538079158));
#19484=CARTESIAN_POINT('Ctrl Pts',(21.9591552462002,16.7847783338415,34.8171144138708));
#19485=CARTESIAN_POINT('Ctrl Pts',(22.1483036958993,16.9331965285742,34.5767521893323));
#19486=CARTESIAN_POINT('Ctrl Pts',(22.4008117472775,17.2971590391485,34.083429001318));
#19487=CARTESIAN_POINT('Ctrl Pts',(22.464,17.5136583227266,33.8310855562043));
#19488=CARTESIAN_POINT('Ctrl Pts',(22.464,17.9560855562043,33.3886583227266));
#19489=CARTESIAN_POINT('Ctrl Pts',(22.4008117472775,18.208429001318,33.1721590391485));
#19490=CARTESIAN_POINT('Ctrl Pts',(22.1483036958993,18.7017521893323,32.8081965285742));
#19491=CARTESIAN_POINT('Ctrl Pts',(21.9591552462002,18.9421144138708,32.6597783338415));
#19492=CARTESIAN_POINT('Ctrl Pts',(21.525274451059,19.3364538079158,32.4405176229446));
#19493=CARTESIAN_POINT('Ctrl Pts',(21.2504388109924,19.5176861336961,32.3544607587991));
#19494=CARTESIAN_POINT('Ctrl Pts',(20.6445305627248,19.764628490954,32.2444605042293));
#19495=CARTESIAN_POINT('Ctrl Pts',(20.3131210482019,19.8290020338711,32.2193798161838));
#19496=CARTESIAN_POINT('Ctrl Pts',(20.,19.8290020338711,32.2193798161838));
#19497=CARTESIAN_POINT('Ctrl Pts',(20.,19.8290020338711,32.2193798161838));
#19498=CARTESIAN_POINT('Ctrl Pts',(19.6868789517981,19.8290020338711,32.2193798161838));
#19499=CARTESIAN_POINT('Ctrl Pts',(19.3554694372752,19.764628490954,32.2444605042293));
#19500=CARTESIAN_POINT('Ctrl Pts',(18.7495611890077,19.5176861336961,32.3544607587991));
#19501=CARTESIAN_POINT('Ctrl Pts',(18.474725548941,19.3364538079158,32.4405176229446));
#19502=CARTESIAN_POINT('Ctrl Pts',(18.0408447537999,18.9421144138708,32.6597783338415));
#19503=CARTESIAN_POINT('Ctrl Pts',(17.8516963041007,18.7017521893323,32.8081965285742));
#19504=CARTESIAN_POINT('Ctrl Pts',(17.5991882527225,18.208429001318,33.1721590391485));
#19505=CARTESIAN_POINT('Ctrl Pts',(17.536,17.9560855562043,33.3886583227266));
#19506=CARTESIAN_POINT('Ctrl Pts',(17.536,17.5136583227266,33.8310855562043));
#19507=CARTESIAN_POINT('Ctrl Pts',(17.5991882527225,17.2971590391485,34.0834290013181));
#19508=CARTESIAN_POINT('Ctrl Pts',(17.8516963041007,16.9331965285742,34.5767521893323));
#19509=CARTESIAN_POINT('Ctrl Pts',(18.0408447537999,16.7847783338415,34.8171144138708));
#19510=CARTESIAN_POINT('Ctrl Pts',(18.474725548941,16.5655176229446,35.2114538079158));
#19511=CARTESIAN_POINT('Ctrl Pts',(18.7495611890077,16.4794607587991,35.3926861336961));
#19512=CARTESIAN_POINT('Ctrl Pts',(19.3554694372752,16.3694605042293,35.639628490954));
#19513=CARTESIAN_POINT('Ctrl Pts',(19.6868789517981,16.3443798161838,35.7040020338711));
#19514=CARTESIAN_POINT('Ctrl Pts',(20.,16.3443798161838,35.7040020338711));
#19515=CARTESIAN_POINT('',(20.,25.1340372978015,37.5244150801141));
#19516=CARTESIAN_POINT('',(20.,22.1288334777587,34.5192112600714));
#19517=CARTESIAN_POINT('Origin',(20.,23.3917261889578,39.2667261889578));
#19518=CARTESIAN_POINT('Origin',(20.,23.3917261889578,39.2667261889578));
#19519=CARTESIAN_POINT('',(20.,24.4523863607376,40.3273863607376));
#19520=CARTESIAN_POINT('',(20.,25.1340372978015,37.5244150801141));
#19521=CARTESIAN_POINT('Origin',(0.,28.075,38.1));
#19522=CARTESIAN_POINT('',(-7.25114412958305E-15,16.375,38.1));
#19523=CARTESIAN_POINT('Origin',(0.,22.225,38.1));
#19524=CARTESIAN_POINT('Origin',(0.249999999999986,22.225,38.1));
#19525=CARTESIAN_POINT('',(0.499999999999999,15.875,38.1));
#19526=CARTESIAN_POINT('Origin',(0.500000000000007,22.225,38.1));
#19527=CARTESIAN_POINT('',(0.249999999999986,16.125,38.1));
#19528=CARTESIAN_POINT('Origin',(90.,22.225,38.1));
#19529=CARTESIAN_POINT('',(179.5,15.875,38.1));
#19530=CARTESIAN_POINT('Origin',(179.5,22.225,38.1));
#19531=CARTESIAN_POINT('',(90.,15.875,38.1));
#19532=CARTESIAN_POINT('Origin',(179.75,22.225,38.1));
#19533=CARTESIAN_POINT('',(180.,16.375,38.1));
#19534=CARTESIAN_POINT('',(179.75,16.125,38.1));
#19535=CARTESIAN_POINT('Origin',(180.,22.225,38.1));
#19536=CARTESIAN_POINT('Origin',(180.,22.225,38.1));
#19537=CARTESIAN_POINT('',(0.,0.,0.));
#19538=CARTESIAN_POINT('Origin',(61.4,39.5248,48.));
#19539=CARTESIAN_POINT('',(58.936,39.3748,48.));
#19540=CARTESIAN_POINT('Origin',(61.4,39.3748,48.));
#19541=CARTESIAN_POINT('',(58.636,39.6748,48.));
#19542=CARTESIAN_POINT('',(58.786,39.5248,48.));
#19543=CARTESIAN_POINT('Origin',(61.4,39.6748,48.));
#19544=CARTESIAN_POINT('Origin',(32.85,39.6748,20.7));
#19545=CARTESIAN_POINT('',(32.85,39.6748,21.2));
#19546=CARTESIAN_POINT('',(70.95,39.6748,21.2));
#19547=CARTESIAN_POINT('',(32.85,39.6748,21.2));
#19548=CARTESIAN_POINT('',(32.85,39.6748,54.999));
#19549=CARTESIAN_POINT('',(32.85,39.6748,55.499));
#19550=CARTESIAN_POINT('',(70.95,39.6748,54.999));
#19551=CARTESIAN_POINT('',(32.85,39.6748,54.999));
#19552=CARTESIAN_POINT('',(70.95,39.6748,55.499));
#19553=CARTESIAN_POINT('',(39.636,39.6748,48.));
#19554=CARTESIAN_POINT('Origin',(42.4,39.6748,48.));
#19555=CARTESIAN_POINT('Origin',(61.4,39.6748,48.));
#19556=CARTESIAN_POINT('',(58.936,30.1748,48.));
#19557=CARTESIAN_POINT('',(58.936,39.6748,48.));
#19558=CARTESIAN_POINT('',(60.2023331707725,30.1748,45.8466560501935));
#19559=CARTESIAN_POINT('Origin',(61.4,30.1748,48.));
#19560=CARTESIAN_POINT('',(62.5976668292275,30.1748,45.8466560501935));
#19561=CARTESIAN_POINT('Ctrl Pts',(62.5976668292275,30.1748,45.8466560501935));
#19562=CARTESIAN_POINT('Ctrl Pts',(62.5839393404939,30.1822399802705,45.8390209680664));
#19563=CARTESIAN_POINT('Ctrl Pts',(62.5701440730763,30.1895277245944,45.8315201115594));
#19564=CARTESIAN_POINT('Ctrl Pts',(62.3978378742979,30.2782518989111,45.7399529520181));
#19565=CARTESIAN_POINT('Ctrl Pts',(62.2093398392196,30.3494894405534,45.6635629490944));
#19566=CARTESIAN_POINT('Ctrl Pts',(61.8090152862429,30.4433961447374,45.5614192720633));
#19567=CARTESIAN_POINT('Ctrl Pts',(61.597114145254,30.4661106047668,45.536));
#19568=CARTESIAN_POINT('Ctrl Pts',(61.202885854746,30.4661106047668,45.536));
#19569=CARTESIAN_POINT('Ctrl Pts',(60.9909847137571,30.4433961447374,45.5614192720633));
#19570=CARTESIAN_POINT('Ctrl Pts',(60.5906601607804,30.3494894405534,45.6635629490944));
#19571=CARTESIAN_POINT('Ctrl Pts',(60.4021621257021,30.2782518989111,45.7399529520181));
#19572=CARTESIAN_POINT('Ctrl Pts',(60.2298559269237,30.1895277245944,45.8315201115594));
#19573=CARTESIAN_POINT('Ctrl Pts',(60.2160606595061,30.1822399802704,45.8390209680664));
#19574=CARTESIAN_POINT('Ctrl Pts',(60.2023331707725,30.1748,45.8466560501935));
#19575=CARTESIAN_POINT('Origin',(61.4,30.1748,48.));
#19576=CARTESIAN_POINT('Origin',(42.4,39.5248,48.));
#19577=CARTESIAN_POINT('',(39.936,39.3748,48.));
#19578=CARTESIAN_POINT('Origin',(42.4,39.3748,48.));
#19579=CARTESIAN_POINT('',(39.786,39.5248,48.));
#19580=CARTESIAN_POINT('Origin',(42.4,39.6748,48.));
#19581=CARTESIAN_POINT('',(39.936,30.1748,48.));
#19582=CARTESIAN_POINT('',(39.936,39.6748,48.));
#19583=CARTESIAN_POINT('',(41.2023331707725,30.1748,45.8466560501935));
#19584=CARTESIAN_POINT('Origin',(42.4,30.1748,48.));
#19585=CARTESIAN_POINT('',(43.5976668292275,30.1748,45.8466560501935));
#19586=CARTESIAN_POINT('Ctrl Pts',(43.5976668292275,30.1748,45.8466560501935));
#19587=CARTESIAN_POINT('Ctrl Pts',(43.5839393404939,30.1822399802704,45.8390209680664));
#19588=CARTESIAN_POINT('Ctrl Pts',(43.5701440730763,30.1895277245944,45.8315201115594));
#19589=CARTESIAN_POINT('Ctrl Pts',(43.3978378742979,30.2782518989111,45.7399529520181));
#19590=CARTESIAN_POINT('Ctrl Pts',(43.2093398392196,30.3494894405534,45.6635629490944));
#19591=CARTESIAN_POINT('Ctrl Pts',(42.8090152862429,30.4433961447374,45.5614192720633));
#19592=CARTESIAN_POINT('Ctrl Pts',(42.597114145254,30.4661106047668,45.536));
#19593=CARTESIAN_POINT('Ctrl Pts',(42.202885854746,30.4661106047668,45.536));
#19594=CARTESIAN_POINT('Ctrl Pts',(41.9909847137571,30.4433961447374,45.5614192720633));
#19595=CARTESIAN_POINT('Ctrl Pts',(41.5906601607804,30.3494894405534,45.6635629490944));
#19596=CARTESIAN_POINT('Ctrl Pts',(41.4021621257021,30.2782518989111,45.7399529520181));
#19597=CARTESIAN_POINT('Ctrl Pts',(41.2298559269237,30.1895277245944,45.8315201115594));
#19598=CARTESIAN_POINT('Ctrl Pts',(41.216060659506,30.1822399802704,45.8390209680664));
#19599=CARTESIAN_POINT('Ctrl Pts',(41.2023331707725,30.1748,45.8466560501935));
#19600=CARTESIAN_POINT('Origin',(42.4,30.1748,48.));
#19601=CARTESIAN_POINT('Origin',(61.4,30.1748,48.));
#19602=CARTESIAN_POINT('',(61.4,28.6942794347161,48.));
#19603=CARTESIAN_POINT('',(58.936,30.1748,48.));
#19604=CARTESIAN_POINT('Ctrl Pts',(60.2023331707725,30.1748,45.8466560501935));
#19605=CARTESIAN_POINT('Ctrl Pts',(60.2597361109102,30.1384432612634,45.8839661875916));
#19606=CARTESIAN_POINT('Ctrl Pts',(60.3174608135473,30.1032893210344,45.9195148810763));
#19607=CARTESIAN_POINT('Ctrl Pts',(60.5005858709669,29.9969713807309,46.0257192203701));
#19608=CARTESIAN_POINT('Ctrl Pts',(60.6580928550894,29.9150369491545,46.1049725011069));
#19609=CARTESIAN_POINT('Ctrl Pts',(60.9740384574878,29.7867651942036,46.2264525494457));
#19610=CARTESIAN_POINT('Ctrl Pts',(61.2000401339365,29.7272527548782,46.2808436974387));
#19611=CARTESIAN_POINT('Ctrl Pts',(61.5999598660636,29.7272527548782,46.2808436974387));
#19612=CARTESIAN_POINT('Ctrl Pts',(61.8259615425122,29.7867651942036,46.2264525494457));
#19613=CARTESIAN_POINT('Ctrl Pts',(62.1419071449106,29.9150369491545,46.1049725011069));
#19614=CARTESIAN_POINT('Ctrl Pts',(62.2994141290331,29.9969713807309,46.0257192203701));
#19615=CARTESIAN_POINT('Ctrl Pts',(62.4825391864527,30.1032893210343,45.9195148810763));
#19616=CARTESIAN_POINT('Ctrl Pts',(62.5402638890898,30.1384432612634,45.8839661875916));
#19617=CARTESIAN_POINT('Ctrl Pts',(62.5976668292275,30.1748,45.8466560501935));
#19618=CARTESIAN_POINT('Origin',(32.85,22.225,38.1));
#19619=CARTESIAN_POINT('',(70.55,11.261659419394,36.3635774380534));
#19620=CARTESIAN_POINT('',(70.55,20.4885774380534,27.136659419394));
#19621=CARTESIAN_POINT('Origin',(70.55,22.225,38.1));
#19622=CARTESIAN_POINT('',(33.25,11.261659419394,36.3635774380534));
#19623=CARTESIAN_POINT('',(32.85,11.261659419394,36.3635774380534));
#19624=CARTESIAN_POINT('',(33.25,20.4885774380534,27.136659419394));
#19625=CARTESIAN_POINT('Origin',(33.25,22.225,38.1));
#19626=CARTESIAN_POINT('',(32.85,20.4885774380534,27.136659419394));
#19627=CARTESIAN_POINT('Ctrl Pts',(41.2023331707725,30.1748,45.8466560501935));
#19628=CARTESIAN_POINT('Ctrl Pts',(41.3584359963022,30.0759306802366,45.9481180633722));
#19629=CARTESIAN_POINT('Ctrl Pts',(41.5172853281954,29.9848847225031,46.0375998429581));
#19630=CARTESIAN_POINT('Ctrl Pts',(41.7909111977588,29.8583912347539,46.1589138702689));
#19631=CARTESIAN_POINT('Ctrl Pts',(41.9011722141917,29.8148256477821,46.1997866389185));
#19632=CARTESIAN_POINT('Ctrl Pts',(42.1359436639152,29.7493650522022,46.2606327740154));
#19633=CARTESIAN_POINT('Ctrl Pts',(42.2603318169086,29.7272527548782,46.2808436974387));
#19634=CARTESIAN_POINT('Ctrl Pts',(42.5396681830914,29.7272527548782,46.2808436974387));
#19635=CARTESIAN_POINT('Ctrl Pts',(42.6640563360848,29.7493650522022,46.2606327740154));
#19636=CARTESIAN_POINT('Ctrl Pts',(42.8988277858083,29.8148256477821,46.1997866389185));
#19637=CARTESIAN_POINT('Ctrl Pts',(43.0090888022412,29.8583912347539,46.1589138702689));
#19638=CARTESIAN_POINT('Ctrl Pts',(43.2827146718046,29.9848847225031,46.0375998429581));
#19639=CARTESIAN_POINT('Ctrl Pts',(43.4415640036978,30.0759306802366,45.9481180633722));
#19640=CARTESIAN_POINT('Ctrl Pts',(43.5976668292275,30.1748,45.8466560501935));
#19641=CARTESIAN_POINT('Origin',(42.4,30.1748,48.));
#19642=CARTESIAN_POINT('',(42.4,28.6942794347161,48.));
#19643=CARTESIAN_POINT('',(39.936,30.1748,48.));
#19644=CARTESIAN_POINT('Origin',(70.75,22.225,38.1));
#19645=CARTESIAN_POINT('',(70.95,20.4260036520373,26.7415840831559));
#19646=CARTESIAN_POINT('',(70.75,20.4572905450454,26.9391217512749));
#19647=CARTESIAN_POINT('',(70.95,10.8665840831559,36.3010036520373));
#19648=CARTESIAN_POINT('Origin',(70.95,22.225,38.1));
#19649=CARTESIAN_POINT('',(70.75,11.0641217512749,36.3322905450454));
#19650=CARTESIAN_POINT('Origin',(70.95,21.3868,38.0995));
#19651=CARTESIAN_POINT('',(70.95,19.4691107383531,20.7));
#19652=CARTESIAN_POINT('',(70.95,19.4691107383531,20.7));
#19653=CARTESIAN_POINT('',(70.95,39.1748,20.7));
#19654=CARTESIAN_POINT('',(70.95,39.6748,20.7));
#19655=CARTESIAN_POINT('',(70.95,39.202675,20.727875));
#19656=CARTESIAN_POINT('',(70.95,39.1748,55.499));
#19657=CARTESIAN_POINT('',(70.95,39.202675,55.471125));
#19658=CARTESIAN_POINT('',(70.95,3.5988,55.499));
#19659=CARTESIAN_POINT('',(70.95,3.0988,55.499));
#19660=CARTESIAN_POINT('',(70.95,3.0988,54.999));
#19661=CARTESIAN_POINT('',(70.95,3.57092499999994,55.4711249999999));
#19662=CARTESIAN_POINT('',(70.95,3.0988,35.0707075174648));
#19663=CARTESIAN_POINT('',(70.95,3.0988,35.0707075174648));
#19664=CARTESIAN_POINT('',(70.95,22.225,38.1));
#19665=CARTESIAN_POINT('Origin',(32.85,22.225,38.1));
#19666=CARTESIAN_POINT('',(32.85,20.4260036520373,26.7415840831559));
#19667=CARTESIAN_POINT('',(33.05,20.4572905450454,26.9391217512749));
#19668=CARTESIAN_POINT('',(32.85,19.4691107383531,20.7));
#19669=CARTESIAN_POINT('',(32.85,19.4691107383531,20.7));
#19670=CARTESIAN_POINT('',(32.85,19.4691107383531,20.7));
#19671=CARTESIAN_POINT('Origin',(33.05,22.225,38.1));
#19672=CARTESIAN_POINT('',(32.85,10.8665840831559,36.3010036520373));
#19673=CARTESIAN_POINT('',(33.05,11.0641217512749,36.3322905450454));
#19674=CARTESIAN_POINT('Origin',(32.85,22.225,38.1));
#19675=CARTESIAN_POINT('Origin',(32.85,21.3868,38.0995));
#19676=CARTESIAN_POINT('',(32.85,3.0988,35.0707075174648));
#19677=CARTESIAN_POINT('',(32.85,22.225,38.1));
#19678=CARTESIAN_POINT('',(32.85,3.0988,54.999));
#19679=CARTESIAN_POINT('',(32.85,3.0988,35.0707075174648));
#19680=CARTESIAN_POINT('',(32.85,3.5988,55.499));
#19681=CARTESIAN_POINT('',(32.85,3.57092499999994,55.4711249999999));
#19682=CARTESIAN_POINT('',(32.85,39.1748,55.499));
#19683=CARTESIAN_POINT('',(32.85,3.0988,55.499));
#19684=CARTESIAN_POINT('',(32.85,39.202675,55.471125));
#19685=CARTESIAN_POINT('',(32.85,39.1748,20.7));
#19686=CARTESIAN_POINT('',(32.85,39.202675,20.727875));
#19687=CARTESIAN_POINT('',(32.85,39.6748,20.7));
#19688=CARTESIAN_POINT('Origin',(32.85,3.0988,35.0707075174648));
#19689=CARTESIAN_POINT('',(32.85,3.0988,35.0707075174648));
#19690=CARTESIAN_POINT('Origin',(32.85,39.4248,20.95));
#19691=CARTESIAN_POINT('',(32.85,39.1748,20.7));
#19692=CARTESIAN_POINT('Origin',(32.85,39.4248,55.249));
#19693=CARTESIAN_POINT('',(32.85,39.1748,55.499));
#19694=CARTESIAN_POINT('Origin',(32.85,39.6748,55.499));
#19695=CARTESIAN_POINT('',(32.85,3.5988,55.499));
#19696=CARTESIAN_POINT('Origin',(32.85,3.3488,55.249));
#19697=CARTESIAN_POINT('',(32.85,3.0988,54.999));
#19698=CARTESIAN_POINT('Origin',(32.85,3.0988,55.499));
#19699=CARTESIAN_POINT('Origin',(32.85,19.4691107383531,20.7));
#19700=CARTESIAN_POINT('',(0.,0.,0.));
#19701=CARTESIAN_POINT('Origin',(32.85,20.175708507973,25.1612827382037));
#19702=CARTESIAN_POINT('',(70.95,20.5511512240695,27.5317347556321));
#19703=CARTESIAN_POINT('',(70.55,20.4885774380534,27.136659419394));
#19704=CARTESIAN_POINT('',(70.75,20.5198643310615,27.334197087513));
#19705=CARTESIAN_POINT('',(70.95,20.856198430898,29.4577270197926));
#19706=CARTESIAN_POINT('',(70.95,21.3074181245908,32.306616044297));
#19707=CARTESIAN_POINT('',(32.85,20.856198430898,29.4577270197926));
#19708=CARTESIAN_POINT('',(51.9,20.856198430898,29.4577270197926));
#19709=CARTESIAN_POINT('',(32.85,20.5511512240695,27.531734755632));
#19710=CARTESIAN_POINT('',(32.85,21.3312780728969,32.4572618290548));
#19711=CARTESIAN_POINT('',(33.25,20.4885774380534,27.136659419394));
#19712=CARTESIAN_POINT('',(33.05,20.5198643310615,27.334197087513));
#19713=CARTESIAN_POINT('',(51.9,20.4885774380534,27.136659419394));
#19714=CARTESIAN_POINT('Origin',(32.85,22.225,38.1));
#19715=CARTESIAN_POINT('',(70.55,11.261659419394,36.3635774380534));
#19716=CARTESIAN_POINT('',(70.95,11.6567347556321,36.4261512240695));
#19717=CARTESIAN_POINT('',(70.75,11.459197087513,36.3948643310615));
#19718=CARTESIAN_POINT('',(33.25,11.261659419394,36.3635774380534));
#19719=CARTESIAN_POINT('',(51.9,11.261659419394,36.3635774380534));
#19720=CARTESIAN_POINT('',(32.85,11.656734755632,36.4261512240695));
#19721=CARTESIAN_POINT('',(33.05,11.459197087513,36.3948643310615));
#19722=CARTESIAN_POINT('',(32.85,13.5827270197925,36.731198430898));
#19723=CARTESIAN_POINT('',(32.85,27.4440761810895,38.926620459953));
#19724=CARTESIAN_POINT('',(70.95,13.5827270197925,36.731198430898));
#19725=CARTESIAN_POINT('',(51.9,13.5827270197925,36.731198430898));
#19726=CARTESIAN_POINT('',(70.95,26.4929361293956,38.7759746751952));
#19727=CARTESIAN_POINT('Origin',(70.75,22.225,38.1));
#19728=CARTESIAN_POINT('Origin',(70.95,22.225,38.1));
#19729=CARTESIAN_POINT('Origin',(70.55,22.225,38.1));
#19730=CARTESIAN_POINT('Origin',(70.95,30.975,38.1));
#19731=CARTESIAN_POINT('Origin',(70.95,22.225,38.1));
#19732=CARTESIAN_POINT('Origin',(51.9,22.225,38.1));
#19733=CARTESIAN_POINT('Origin',(32.85,22.225,38.1));
#19734=CARTESIAN_POINT('Origin',(32.85,32.925,38.1));
#19735=CARTESIAN_POINT('Origin',(32.85,22.225,38.1));
#19736=CARTESIAN_POINT('Origin',(33.05,22.225,38.1));
#19737=CARTESIAN_POINT('Origin',(33.25,22.225,38.1));
#19738=CARTESIAN_POINT('Origin',(51.9,22.225,38.1));
#19739=CARTESIAN_POINT('',(0.,0.,0.));
#19740=CARTESIAN_POINT('Origin',(40.9,31.483337699552,36.913331115663));
#19741=CARTESIAN_POINT('',(62.9,30.9136868437562,37.0659686024412));
#19742=CARTESIAN_POINT('',(40.9,30.9136868437562,37.0659686024412));
#19743=CARTESIAN_POINT('',(51.9,30.9136868437562,37.0659686024412));
#19744=CARTESIAN_POINT('',(62.9,28.6606288924974,37.6696736609815));
#19745=CARTESIAN_POINT('',(62.9,28.2957824727981,37.7674339645013));
#19746=CARTESIAN_POINT('',(40.9,28.6606288924974,37.6696736609815));
#19747=CARTESIAN_POINT('',(51.9,28.6606288924974,37.6696736609815));
#19748=CARTESIAN_POINT('',(40.9,28.2957824727981,37.7674339645013));
#19749=CARTESIAN_POINT('Origin',(40.9,29.5660362797969,36.1329752572208));
#19750=CARTESIAN_POINT('',(40.9,30.2666392309999,34.6511540367185));
#19751=CARTESIAN_POINT('Origin',(40.9,22.225,38.1));
#19752=CARTESIAN_POINT('',(40.9,28.0135812797411,35.2548590952589));
#19753=CARTESIAN_POINT('Origin',(40.9,22.225,38.1));
#19754=CARTESIAN_POINT('',(40.9,30.8362900867957,34.4985165499403));
#19755=CARTESIAN_POINT('Origin',(40.9,27.6487348600418,35.3526193987787));
#19756=CARTESIAN_POINT('',(62.9,30.2666392309999,34.6511540367185));
#19757=CARTESIAN_POINT('',(51.9,30.2666392309999,34.6511540367185));
#19758=CARTESIAN_POINT('',(62.9,28.0135812797411,35.2548590952589));
#19759=CARTESIAN_POINT('',(51.9,28.0135812797411,35.2548590952589));
#19760=CARTESIAN_POINT('',(62.9,30.8362900867957,34.4985165499403));
#19761=CARTESIAN_POINT('Origin',(62.9,29.5660362797969,36.1329752572208));
#19762=CARTESIAN_POINT('Origin',(62.9,22.225,38.1));
#19763=CARTESIAN_POINT('Origin',(62.9,22.225,38.1));
#19764=CARTESIAN_POINT('Origin',(40.9,27.8818542494924,45.5246212024587));
#19765=CARTESIAN_POINT('',(62.9,27.4648408804748,45.1076078334411));
#19766=CARTESIAN_POINT('',(40.9,27.4648408804748,45.1076078334411));
#19767=CARTESIAN_POINT('',(51.9,27.4648408804748,45.1076078334411));
#19768=CARTESIAN_POINT('',(62.9,25.8154879877562,43.4582549407226));
#19769=CARTESIAN_POINT('',(62.9,25.5484018715768,43.1911688245431));
#19770=CARTESIAN_POINT('',(40.9,25.8154879877562,43.4582549407226));
#19771=CARTESIAN_POINT('',(51.9,25.8154879877562,43.4582549407226));
#19772=CARTESIAN_POINT('',(40.9,25.5484018715768,43.1911688245431));
#19773=CARTESIAN_POINT('Origin',(40.9,27.5990115370178,43.4740115370178));
#19774=CARTESIAN_POINT('',(40.9,29.2326078334411,43.3398408804748));
#19775=CARTESIAN_POINT('Origin',(40.9,22.225,38.1));
#19776=CARTESIAN_POINT('',(40.9,27.5832549407226,41.6904879877562));
#19777=CARTESIAN_POINT('Origin',(40.9,22.225,38.1));
#19778=CARTESIAN_POINT('',(40.9,29.6496212024587,43.7568542494924));
#19779=CARTESIAN_POINT('Origin',(40.9,27.3161688245431,41.4234018715768));
#19780=CARTESIAN_POINT('',(62.9,29.2326078334411,43.3398408804748));
#19781=CARTESIAN_POINT('',(51.9,29.2326078334411,43.3398408804748));
#19782=CARTESIAN_POINT('',(62.9,27.5832549407226,41.6904879877562));
#19783=CARTESIAN_POINT('',(51.9,27.5832549407226,41.6904879877562));
#19784=CARTESIAN_POINT('',(62.9,29.6496212024587,43.7568542494924));
#19785=CARTESIAN_POINT('Origin',(62.9,27.5990115370178,43.4740115370178));
#19786=CARTESIAN_POINT('Origin',(62.9,22.225,38.1));
#19787=CARTESIAN_POINT('Origin',(62.9,22.225,38.1));
#19788=CARTESIAN_POINT('Origin',(40.9,18.6235165499403,46.7112900867957));
#19789=CARTESIAN_POINT('',(62.9,18.7761540367185,46.1416392309999));
#19790=CARTESIAN_POINT('',(40.9,18.7761540367185,46.1416392309999));
#19791=CARTESIAN_POINT('',(51.9,18.7761540367185,46.1416392309999));
#19792=CARTESIAN_POINT('',(62.9,19.3798590952589,43.8885812797411));
#19793=CARTESIAN_POINT('',(62.9,19.4776193987787,43.5237348600418));
#19794=CARTESIAN_POINT('',(40.9,19.3798590952589,43.8885812797411));
#19795=CARTESIAN_POINT('',(51.9,19.3798590952589,43.8885812797411));
#19796=CARTESIAN_POINT('',(40.9,19.4776193987787,43.5237348600418));
#19797=CARTESIAN_POINT('Origin',(40.9,20.2579752572208,45.4410362797969));
#19798=CARTESIAN_POINT('',(40.9,21.1909686024412,46.7886868437562));
#19799=CARTESIAN_POINT('Origin',(40.9,22.225,38.1));
#19800=CARTESIAN_POINT('',(40.9,21.7946736609815,44.5356288924974));
#19801=CARTESIAN_POINT('Origin',(40.9,22.225,38.1));
#19802=CARTESIAN_POINT('',(40.9,21.038331115663,47.358337699552));
#19803=CARTESIAN_POINT('Origin',(40.9,21.8924339645013,44.1707824727981));
#19804=CARTESIAN_POINT('',(62.9,21.1909686024412,46.7886868437562));
#19805=CARTESIAN_POINT('',(51.9,21.1909686024412,46.7886868437562));
#19806=CARTESIAN_POINT('',(62.9,21.7946736609815,44.5356288924974));
#19807=CARTESIAN_POINT('',(51.9,21.7946736609815,44.5356288924974));
#19808=CARTESIAN_POINT('',(62.9,21.038331115663,47.358337699552));
#19809=CARTESIAN_POINT('Origin',(62.9,20.2579752572208,45.4410362797969));
#19810=CARTESIAN_POINT('Origin',(62.9,22.225,38.1));
#19811=CARTESIAN_POINT('Origin',(62.9,22.225,38.1));
#19812=CARTESIAN_POINT('Origin',(40.9,12.966662300448,39.286668884337));
#19813=CARTESIAN_POINT('',(62.9,13.5363131562438,39.1340313975588));
#19814=CARTESIAN_POINT('',(40.9,13.5363131562438,39.1340313975588));
#19815=CARTESIAN_POINT('',(51.9,13.5363131562438,39.1340313975588));
#19816=CARTESIAN_POINT('',(62.9,15.7893711075026,38.5303263390185));
#19817=CARTESIAN_POINT('',(62.9,16.1542175272019,38.4325660354987));
#19818=CARTESIAN_POINT('',(40.9,15.7893711075026,38.5303263390185));
#19819=CARTESIAN_POINT('',(51.9,15.7893711075026,38.5303263390185));
#19820=CARTESIAN_POINT('',(40.9,16.1542175272019,38.4325660354987));
#19821=CARTESIAN_POINT('Origin',(40.9,14.8839637202031,40.0670247427792));
#19822=CARTESIAN_POINT('',(40.9,14.1833607690001,41.5488459632815));
#19823=CARTESIAN_POINT('Origin',(40.9,22.225,38.1));
#19824=CARTESIAN_POINT('',(40.9,16.4364187202589,40.9451409047411));
#19825=CARTESIAN_POINT('Origin',(40.9,22.225,38.1));
#19826=CARTESIAN_POINT('',(40.9,13.6137099132043,41.7014834500596));
#19827=CARTESIAN_POINT('Origin',(40.9,16.8012651399582,40.8473806012213));
#19828=CARTESIAN_POINT('',(62.9,14.1833607690001,41.5488459632815));
#19829=CARTESIAN_POINT('',(51.9,14.1833607690001,41.5488459632815));
#19830=CARTESIAN_POINT('',(62.9,16.4364187202589,40.9451409047411));
#19831=CARTESIAN_POINT('',(51.9,16.4364187202589,40.9451409047411));
#19832=CARTESIAN_POINT('',(62.9,13.6137099132043,41.7014834500596));
#19833=CARTESIAN_POINT('Origin',(62.9,14.8839637202031,40.0670247427792));
#19834=CARTESIAN_POINT('Origin',(62.9,22.225,38.1));
#19835=CARTESIAN_POINT('Origin',(62.9,22.225,38.1));
#19836=CARTESIAN_POINT('Origin',(40.9,25.8264834500596,29.4887099132043));
#19837=CARTESIAN_POINT('',(62.9,25.6738459632815,30.0583607690001));
#19838=CARTESIAN_POINT('',(40.9,25.6738459632815,30.0583607690001));
#19839=CARTESIAN_POINT('',(51.9,25.6738459632815,30.0583607690001));
#19840=CARTESIAN_POINT('',(62.9,25.0701409047411,32.3114187202589));
#19841=CARTESIAN_POINT('',(62.9,24.9723806012213,32.6762651399582));
#19842=CARTESIAN_POINT('',(40.9,25.0701409047411,32.3114187202589));
#19843=CARTESIAN_POINT('',(51.9,25.0701409047411,32.3114187202589));
#19844=CARTESIAN_POINT('',(40.9,24.9723806012213,32.6762651399582));
#19845=CARTESIAN_POINT('Origin',(40.9,24.1920247427792,30.7589637202031));
#19846=CARTESIAN_POINT('',(40.9,23.2590313975588,29.4113131562438));
#19847=CARTESIAN_POINT('Origin',(40.9,22.225,38.1));
#19848=CARTESIAN_POINT('',(40.9,22.6553263390185,31.6643711075026));
#19849=CARTESIAN_POINT('Origin',(40.9,22.225,38.1));
#19850=CARTESIAN_POINT('',(40.9,23.411668884337,28.841662300448));
#19851=CARTESIAN_POINT('Origin',(40.9,22.5575660354987,32.0292175272019));
#19852=CARTESIAN_POINT('',(62.9,23.2590313975588,29.4113131562438));
#19853=CARTESIAN_POINT('',(51.9,23.2590313975588,29.4113131562438));
#19854=CARTESIAN_POINT('',(62.9,22.6553263390185,31.6643711075026));
#19855=CARTESIAN_POINT('',(51.9,22.6553263390185,31.6643711075026));
#19856=CARTESIAN_POINT('',(62.9,23.411668884337,28.841662300448));
#19857=CARTESIAN_POINT('Origin',(62.9,24.1920247427792,30.7589637202031));
#19858=CARTESIAN_POINT('Origin',(62.9,22.225,38.1));
#19859=CARTESIAN_POINT('Origin',(62.9,22.225,38.1));
#19860=CARTESIAN_POINT('Origin',(32.85,22.225,38.1));
#19861=CARTESIAN_POINT('',(70.65,15.8544102031614,37.0909977004905));
#19862=CARTESIAN_POINT('',(33.15,15.8544102031614,37.0909977004905));
#19863=CARTESIAN_POINT('',(51.9,15.8544102031614,37.0909977004905));
#19864=CARTESIAN_POINT('',(70.65,13.5827270197925,36.731198430898));
#19865=CARTESIAN_POINT('',(70.65,25.3710786325259,38.5982899034296));
#19866=CARTESIAN_POINT('',(33.15,13.5827270197925,36.731198430898));
#19867=CARTESIAN_POINT('',(51.9,13.5827270197925,36.731198430898));
#19868=CARTESIAN_POINT('',(33.15,26.4929361293956,38.7759746751952));
#19869=CARTESIAN_POINT('Origin',(32.85,20.5433295008175,27.4823503386023));
#19870=CARTESIAN_POINT('',(33.15,21.2159977004905,31.7294102031614));
#19871=CARTESIAN_POINT('',(70.65,21.2159977004905,31.7294102031614));
#19872=CARTESIAN_POINT('',(51.9,21.2159977004905,31.7294102031614));
#19873=CARTESIAN_POINT('',(33.15,20.856198430898,29.4577270197926));
#19874=CARTESIAN_POINT('',(33.15,21.4912286210131,33.4671498444963));
#19875=CARTESIAN_POINT('',(70.65,20.856198430898,29.4577270197926));
#19876=CARTESIAN_POINT('',(51.9,20.856198430898,29.4577270197926));
#19877=CARTESIAN_POINT('',(70.65,21.4630861178828,33.2894650727307));
#19878=CARTESIAN_POINT('Origin',(70.65,28.675,38.1));
#19879=CARTESIAN_POINT('Origin',(70.65,22.225,38.1));
#19880=CARTESIAN_POINT('Origin',(70.65,22.225,38.1));
#19881=CARTESIAN_POINT('Origin',(51.9,22.225,38.1));
#19882=CARTESIAN_POINT('Origin',(33.15,22.225,38.1));
#19883=CARTESIAN_POINT('Origin',(51.9,22.225,38.1));
#19884=CARTESIAN_POINT('Origin',(33.15,22.225,38.1));
#19885=CARTESIAN_POINT('Origin',(33.15,30.975,38.1));
#19886=CARTESIAN_POINT('',(0.,0.,0.));
#19887=CARTESIAN_POINT('Origin',(42.8,14.9316563078761,40.0542456));
#19888=CARTESIAN_POINT('',(42.8,14.9316563078761,41.2448706));
#19889=CARTESIAN_POINT('',(42.8,14.9316563078761,38.8636206));
#19890=CARTESIAN_POINT('Origin',(42.8,14.9316563078761,40.0542456));
#19891=CARTESIAN_POINT('',(0.,0.,0.));
#19892=CARTESIAN_POINT('Origin',(42.4,48.4493818343519,48.));
#19893=CARTESIAN_POINT('',(41.7941388317924,46.4519835383214,49.8315225365138));
#19894=CARTESIAN_POINT('',(41.7941388317924,46.6231654538532,49.8315225365138));
#19895=CARTESIAN_POINT('',(41.7941388317924,48.4493818343519,49.8315225365138));
#19896=CARTESIAN_POINT('',(41.191723663621,46.9748,46.4961346962422));
#19897=CARTESIAN_POINT('Ctrl Pts',(41.191723663621,46.9748,46.4961346962422));
#19898=CARTESIAN_POINT('Ctrl Pts',(41.1983691281237,46.9742382770361,46.4907954165322));
#19899=CARTESIAN_POINT('Ctrl Pts',(41.2050496865336,46.9736765540721,46.4855004235829));
#19900=CARTESIAN_POINT('Ctrl Pts',(41.2117649567869,46.9731148311082,46.480250007738));
#19901=CARTESIAN_POINT('Ctrl Pts',(41.2650801043383,46.968655093588,46.438564910204));
#19902=CARTESIAN_POINT('Ctrl Pts',(41.3206975739893,46.9641953560677,46.3996058162976));
#19903=CARTESIAN_POINT('Ctrl Pts',(41.3783074070676,46.9597356185475,46.3636361032927));
#19904=CARTESIAN_POINT('Ctrl Pts',(41.4358295661938,46.955282668112,46.3277211310625));
#19905=CARTESIAN_POINT('Ctrl Pts',(41.4953376565687,46.9508297176764,46.2947867697778));
#19906=CARTESIAN_POINT('Ctrl Pts',(41.5564898960424,46.9463767672408,46.2650552569545));
#19907=CARTESIAN_POINT('Ctrl Pts',(41.617568923949,46.9419291478852,46.2353593387498));
#19908=CARTESIAN_POINT('Ctrl Pts',(41.6802877505718,46.9374815285296,46.2088588680115));
#19909=CARTESIAN_POINT('Ctrl Pts',(41.74427854964,46.933033909174,46.1857310187192));
#19910=CARTESIAN_POINT('Ctrl Pts',(41.8082284267617,46.9285891340592,46.1626179596253));
#19911=CARTESIAN_POINT('Ctrl Pts',(41.8734482003687,46.9241443589444,46.142873410735));
#19912=CARTESIAN_POINT('Ctrl Pts',(41.939549990011,46.9196995838296,46.126626480063));
#19913=CARTESIAN_POINT('Ctrl Pts',(42.0056322514933,46.9152561218151,46.1103843491501));
#19914=CARTESIAN_POINT('Ctrl Pts',(42.0725955334245,46.9108126598006,46.0976379027819));
#19915=CARTESIAN_POINT('Ctrl Pts',(42.1400384824014,46.9063691977861,46.0884659128679));
#19916=CARTESIAN_POINT('Ctrl Pts',(42.2074847113698,46.9019255196702,46.0792934768873));
#19917=CARTESIAN_POINT('Ctrl Pts',(42.2754101650517,46.8974818415542,46.0736959063333));
#19918=CARTESIAN_POINT('Ctrl Pts',(42.3434068477991,46.8930381634383,46.0717002898865));
#19919=CARTESIAN_POINT('Ctrl Pts',(42.4114747425737,46.888589831517,46.0697025834569));
#19920=CARTESIAN_POINT('Ctrl Pts',(42.4796135217653,46.8841414995957,46.071314373904));
#19921=CARTESIAN_POINT('Ctrl Pts',(42.5474146977834,46.8796931676744,46.0765106021146));
#19922=CARTESIAN_POINT('Ctrl Pts',(42.6152559711119,46.8752422050296,46.0817099033512));
#19923=CARTESIAN_POINT('Ctrl Pts',(42.6827587551109,46.8707912423849,46.0904977979093));
#19924=CARTESIAN_POINT('Ctrl Pts',(42.7495220026355,46.8663402797401,46.1027976052688));
#19925=CARTESIAN_POINT('Ctrl Pts',(42.8163991049541,46.8618817266401,46.1151183881214));
#19926=CARTESIAN_POINT('Ctrl Pts',(42.8825336747408,46.8574231735402,46.1309629220749));
#19927=CARTESIAN_POINT('Ctrl Pts',(42.9475380138215,46.8529646204403,46.1502041517183));
#19928=CARTESIAN_POINT('Ctrl Pts',(42.9770644780014,46.8509394431943,46.1589439602583));
#19929=CARTESIAN_POINT('Ctrl Pts',(43.0063580080931,46.8489142659483,46.1683839025424));
#19930=CARTESIAN_POINT('Ctrl Pts',(43.0353837115926,46.8468890887023,46.1785088262792));
#19931=CARTESIAN_POINT('Ctrl Pts',(43.0993551412968,46.8424256832301,46.200823732345));
#19932=CARTESIAN_POINT('Ctrl Pts',(43.1622728061311,46.837962277758,46.2265557417306));
#19933=CARTESIAN_POINT('Ctrl Pts',(43.2237472171988,46.8334988722859,46.2555851757517));
#19934=CARTESIAN_POINT('Ctrl Pts',(43.285130739502,46.8290420658751,46.2845716902987));
#19935=CARTESIAN_POINT('Ctrl Pts',(43.3450748018767,46.8245852594642,46.3168457449076));
#19936=CARTESIAN_POINT('Ctrl Pts',(43.4032074881356,46.8201284530534,46.3522387027701));
#19937=CARTESIAN_POINT('Ctrl Pts',(43.4612740279245,46.8156767178346,46.3875913886381));
#19938=CARTESIAN_POINT('Ctrl Pts',(43.517532866745,46.8112249826158,46.4260556750136));
#19939=CARTESIAN_POINT('Ctrl Pts',(43.571636046414,46.8067732473969,46.4674167129832));
#19940=CARTESIAN_POINT('Ctrl Pts',(43.62570659323,46.802324197285,46.508752803645));
#19941=CARTESIAN_POINT('Ctrl Pts',(43.6776236703527,46.7978751471731,46.5529818816755));
#19942=CARTESIAN_POINT('Ctrl Pts',(43.7270690426102,46.7934260970611,46.5998463252037));
#19943=CARTESIAN_POINT('Ctrl Pts',(43.7765015193754,46.788978207274,46.646698546353));
#19944=CARTESIAN_POINT('Ctrl Pts',(43.8234632143047,46.7845303174869,46.696184430213));
#19945=CARTESIAN_POINT('Ctrl Pts',(43.8676710594111,46.7800824276997,46.748007900078));
#19946=CARTESIAN_POINT('Ctrl Pts',(43.9118825092414,46.77563417523,46.7998355956478));
#19947=CARTESIAN_POINT('Ctrl Pts',(43.9533393462278,46.7711859227603,46.8540008797944));
#19948=CARTESIAN_POINT('Ctrl Pts',(43.9917984724335,46.7667376702906,46.9101742432579));
#19949=CARTESIAN_POINT('Ctrl Pts',(44.0302994859557,46.7622845730577,46.9664087872965));
#19950=CARTESIAN_POINT('Ctrl Pts',(44.0657959949355,46.7578314758248,47.0246553685409));
#19951=CARTESIAN_POINT('Ctrl Pts',(44.0980885597473,46.7533783785919,47.0845559546562));
#19952=CARTESIAN_POINT('Ctrl Pts',(44.130401043843,46.748922534519,47.1444934897343));
#19953=CARTESIAN_POINT('Ctrl Pts',(44.1595054403871,46.7444666904462,47.2060866154888));
#19954=CARTESIAN_POINT('Ctrl Pts',(44.1852498026584,46.7400108463733,47.2689557475719));
#19955=CARTESIAN_POINT('Ctrl Pts',(44.2110387609674,46.7355472836011,47.3319337856032));
#19956=CARTESIAN_POINT('Ctrl Pts',(44.2334559068194,46.731083720829,47.3961917773044));
#19957=CARTESIAN_POINT('Ctrl Pts',(44.2523989130009,46.7266201580569,47.4613342186354));
#19958=CARTESIAN_POINT('Ctrl Pts',(44.2608256584626,46.7246345541367,47.490312658836));
#19959=CARTESIAN_POINT('Ctrl Pts',(44.2685655868985,46.7226489502166,47.5194659812589));
#19960=CARTESIAN_POINT('Ctrl Pts',(44.2756129660321,46.7206633462965,47.5487588687272));
#19961=CARTESIAN_POINT('Ctrl Pts',(44.2914115935473,46.7162120721231,47.6144268864664));
#19962=CARTESIAN_POINT('Ctrl Pts',(44.3037895859002,46.7117607979497,47.6810596925127));
#19963=CARTESIAN_POINT('Ctrl Pts',(44.3126351888968,46.7073095237764,47.7482676200929));
#19964=CARTESIAN_POINT('Ctrl Pts',(44.3214672302742,46.7028650740655,47.8153725079679));
#19965=CARTESIAN_POINT('Ctrl Pts',(44.3267775648675,46.6984206243546,47.8830502810582));
#19966=CARTESIAN_POINT('Ctrl Pts',(44.3285050353862,46.6939761746436,47.9508992322864));
#19967=CARTESIAN_POINT('Ctrl Pts',(44.3302304290408,46.6895370683051,48.0186666116147));
#19968=CARTESIAN_POINT('Ctrl Pts',(44.3283814998983,46.6850979619664,48.0866042680409));
#19969=CARTESIAN_POINT('Ctrl Pts',(44.3229488844025,46.6806588556279,48.1543053624323));
#19970=CARTESIAN_POINT('Ctrl Pts',(44.3175197527825,46.6762225960388,48.221963040865));
#19971=CARTESIAN_POINT('Ctrl Pts',(44.3085115324534,46.6717863364497,48.2893839659275));
#19972=CARTESIAN_POINT('Ctrl Pts',(44.2959669172311,46.6673500768606,48.3561628920383));
#19973=CARTESIAN_POINT('Ctrl Pts',(44.2834259846457,46.6629151195939,48.4229222143167));
#19974=CARTESIAN_POINT('Ctrl Pts',(44.2673508091051,46.6584801623272,48.4890394255097));
#19975=CARTESIAN_POINT('Ctrl Pts',(44.2478354859469,46.6540452050604,48.5541178338364));
#19976=CARTESIAN_POINT('Ctrl Pts',(44.2283191059579,46.6496100076235,48.6191997664122));
#19977=CARTESIAN_POINT('Ctrl Pts',(44.2053623532084,46.6451748101866,48.6832423110911));
#19978=CARTESIAN_POINT('Ctrl Pts',(44.1791091169869,46.6407396127497,48.7458641342458));
#19979=CARTESIAN_POINT('Ctrl Pts',(44.1528277688164,46.6362996661061,48.8085530128095));
#19980=CARTESIAN_POINT('Ctrl Pts',(44.1232430846532,46.6318597194626,48.8698176765481));
#19981=CARTESIAN_POINT('Ctrl Pts',(44.0905466184338,46.627419772819,48.9292979542656));
#19982=CARTESIAN_POINT('Ctrl Pts',(44.0578304684092,46.6229771532553,48.9888140400788));
#19983=CARTESIAN_POINT('Ctrl Pts',(44.0219990696359,46.6185345336915,49.0465431816973));
#19984=CARTESIAN_POINT('Ctrl Pts',(43.9832878497896,46.6140919141278,49.1021534111043));
#19985=CARTESIAN_POINT('Ctrl Pts',(43.944509152903,46.6096415506898,49.1578605740024));
#19986=CARTESIAN_POINT('Ctrl Pts',(43.9028409206391,46.6051911872518,49.2114410632156));
#19987=CARTESIAN_POINT('Ctrl Pts',(43.8585588644388,46.6007408238138,49.2625959749132));
#19988=CARTESIAN_POINT('Ctrl Pts',(43.8376527412443,46.5986397505061,49.2867468607962));
#19989=CARTESIAN_POINT('Ctrl Pts',(43.8161645536072,46.5965386771983,49.3103576451171));
#19990=CARTESIAN_POINT('Ctrl Pts',(43.7941259842674,46.5944376038905,49.3333999013388));
#19991=CARTESIAN_POINT('Ctrl Pts',(43.7473774321868,46.5899807748905,49.3822774894631));
#19992=CARTESIAN_POINT('Ctrl Pts',(43.697961986577,46.5855239458904,49.4287911969137));
#19993=CARTESIAN_POINT('Ctrl Pts',(43.6461482113789,46.5810671168903,49.4726361370608));
#19994=CARTESIAN_POINT('Ctrl Pts',(43.594412953924,46.5766170416957,49.5164146353063));
#19995=CARTESIAN_POINT('Ctrl Pts',(43.5402869531792,46.572166966501,49.5575320759062));
#19996=CARTESIAN_POINT('Ctrl Pts',(43.4840761815292,46.5677168913064,49.595719708953));
#19997=CARTESIAN_POINT('Ctrl Pts',(43.4279319327049,46.5632720825681,49.6338621487179));
#19998=CARTESIAN_POINT('Ctrl Pts',(43.369708219006,46.5588272738298,49.6690813906766));
#19999=CARTESIAN_POINT('Ctrl Pts',(43.3097432645744,46.5543824650915,49.7011495376544));
#20000=CARTESIAN_POINT('Ctrl Pts',(43.249816114471,46.5499404585401,49.7331974675776));
#20001=CARTESIAN_POINT('Ctrl Pts',(43.1881503353395,46.5454984519887,49.7620980108258));
#20002=CARTESIAN_POINT('Ctrl Pts',(43.1251108919607,46.5410564454373,49.7876679644889));
#20003=CARTESIAN_POINT('Ctrl Pts',(43.0620894213714,46.5366157053192,49.8132306280593));
#20004=CARTESIAN_POINT('Ctrl Pts',(42.9976955211072,46.5321749652011,49.835464401591));
#20005=CARTESIAN_POINT('Ctrl Pts',(42.9323146994587,46.527734225083,49.8542339705766));
#20006=CARTESIAN_POINT('Ctrl Pts',(42.8669299404626,46.5232932175357,49.8730046698985));
#20007=CARTESIAN_POINT('Ctrl Pts',(42.8005586171901,46.5188522099884,49.8883106168319));
#20008=CARTESIAN_POINT('Ctrl Pts',(42.7336002041476,46.5144112024411,49.9000666990116));
#20009=CARTESIAN_POINT('Ctrl Pts',(42.6665701630067,46.5099654441701,49.9118353571436));
#20010=CARTESIAN_POINT('Ctrl Pts',(42.5989522658176,46.5055196858991,49.9200464867793));
#20011=CARTESIAN_POINT('Ctrl Pts',(42.5311539333469,46.501073927628,49.9246665172615));
#20012=CARTESIAN_POINT('Ctrl Pts',(42.463314692732,46.4966254868762,49.9292893353768));
#20013=CARTESIAN_POINT('Ctrl Pts',(42.3952952937105,46.4921770461244,49.9303167347623));
#20014=CARTESIAN_POINT('Ctrl Pts',(42.3275031536886,46.4877286053727,49.9277673003179));
#20015=CARTESIAN_POINT('Ctrl Pts',(42.2595937096817,46.4832724672709,49.925213454465));
#20016=CARTESIAN_POINT('Ctrl Pts',(42.1919128006937,46.4788163291692,49.9190704673553));
#20017=CARTESIAN_POINT('Ctrl Pts',(42.1248618177861,46.4743601910674,49.9094086879419));
#20018=CARTESIAN_POINT('Ctrl Pts',(42.0940240884677,46.4723107478732,49.9049650940472));
#20019=CARTESIAN_POINT('Ctrl Pts',(42.0633194436199,46.4702613046789,49.8997779097643));
#20020=CARTESIAN_POINT('Ctrl Pts',(42.0327859245322,46.4682118614847,49.8938575394359));
#20021=CARTESIAN_POINT('Ctrl Pts',(41.9663867181945,46.4637550741376,49.8809829051726));
#20022=CARTESIAN_POINT('Ctrl Pts',(41.9005331589857,46.4592982867905,49.8645864316223));
#20023=CARTESIAN_POINT('Ctrl Pts',(41.8356269390523,46.4548414994434,49.8447291413583));
#20024=CARTESIAN_POINT('Ctrl Pts',(41.821753010091,46.4538888457361,49.8404845768964));
#20025=CARTESIAN_POINT('Ctrl Pts',(41.8079223464408,46.4529361920287,49.8360820743412));
#20026=CARTESIAN_POINT('Ctrl Pts',(41.7941388317924,46.4519835383214,49.8315225365139));
#20027=CARTESIAN_POINT('',(43.6084517554458,46.9748,46.4962756530334));
#20028=CARTESIAN_POINT('Origin',(42.4,46.9748,48.));
#20029=CARTESIAN_POINT('Ctrl Pts',(43.6084517554457,46.9748,46.4962756530334));
#20030=CARTESIAN_POINT('Ctrl Pts',(43.6626868745532,46.97024365882,46.5398611180319));
#20031=CARTESIAN_POINT('Ctrl Pts',(43.714603934413,46.9656873176399,46.5864184202764));
#20032=CARTESIAN_POINT('Ctrl Pts',(43.7638757919844,46.9611309764599,46.6356740195471));
#20033=CARTESIAN_POINT('Ctrl Pts',(43.8145915454213,46.9564411131738,46.6863730382389));
#20034=CARTESIAN_POINT('Ctrl Pts',(43.8625042214584,46.9517512498878,46.7399306831323));
#20035=CARTESIAN_POINT('Ctrl Pts',(43.907295865415,46.9470613866017,46.7960059256778));
#20036=CARTESIAN_POINT('Ctrl Pts',(43.9507783555296,46.9425085969302,46.8504422214749));
#20037=CARTESIAN_POINT('Ctrl Pts',(43.9913194768775,46.9379558072587,46.9072505616738));
#20038=CARTESIAN_POINT('Ctrl Pts',(44.0286688300753,46.9334030175871,46.9660849170066));
#20039=CARTESIAN_POINT('Ctrl Pts',(44.0660184763803,46.9288501921866,47.0249197340549));
#20040=CARTESIAN_POINT('Ctrl Pts',(44.1001760571108,46.9242973667861,47.0857802079187));
#20041=CARTESIAN_POINT('Ctrl Pts',(44.1309352046544,46.9197445413856,47.1482923775215));
#20042=CARTESIAN_POINT('Ctrl Pts',(44.1617030842414,46.9151904235088,47.2108222933565));
#20043=CARTESIAN_POINT('Ctrl Pts',(44.1890704094519,46.910636305632,47.2750044223297));
#20044=CARTESIAN_POINT('Ctrl Pts',(44.212877998293,46.9060821877551,47.3404426331202));
#20045=CARTESIAN_POINT('Ctrl Pts',(44.237930877054,46.9012898602417,47.4093036829401));
#20046=CARTESIAN_POINT('Ctrl Pts',(44.2590412424677,46.8964975327283,47.4795552736269));
#20047=CARTESIAN_POINT('Ctrl Pts',(44.2760831146131,46.8917052052149,47.5507175677107));
#20048=CARTESIAN_POINT('Ctrl Pts',(44.2923129273951,46.8871412360882,47.6184889193717));
#20049=CARTESIAN_POINT('Ctrl Pts',(44.3048531194064,46.8825772669614,47.6870856827015));
#20050=CARTESIAN_POINT('Ctrl Pts',(44.3136478030715,46.8780132978347,47.7560847632889));
#20051=CARTESIAN_POINT('Ctrl Pts',(44.3224506437573,46.8734450956517,47.8251478401448));
#20052=CARTESIAN_POINT('Ctrl Pts',(44.3275010239818,46.8688768934686,47.8946135174533));
#20053=CARTESIAN_POINT('Ctrl Pts',(44.32879511488,46.8643086912856,47.9640561310493));
#20054=CARTESIAN_POINT('Ctrl Pts',(44.3300915836412,46.8597320951334,48.0336263438916));
#20055=CARTESIAN_POINT('Ctrl Pts',(44.3276180036356,46.8551554989812,48.1031729479443));
#20056=CARTESIAN_POINT('Ctrl Pts',(44.3214224949418,46.850578902829,48.1722734826715));
#20057=CARTESIAN_POINT('Ctrl Pts',(44.3205179072987,46.8499106877507,48.182362644504));
#20058=CARTESIAN_POINT('Ctrl Pts',(44.3195340645117,46.8492424726725,48.1924423136961));
#20059=CARTESIAN_POINT('Ctrl Pts',(44.3184712072634,46.8485742575942,48.2025111942618));
#20060=CARTESIAN_POINT('Ctrl Pts',(44.3114461192161,46.8441576063768,48.2690627209386));
#20061=CARTESIAN_POINT('Ctrl Pts',(44.3009370448108,46.8397409551594,48.3354066300998));
#20062=CARTESIAN_POINT('Ctrl Pts',(44.2869621236117,46.8353243039421,48.4011439903015));
#20063=CARTESIAN_POINT('Ctrl Pts',(44.2730105785239,46.8309150405396,48.4667713903945));
#20064=CARTESIAN_POINT('Ctrl Pts',(44.2556047870564,46.8265057771371,48.5317937659605));
#20065=CARTESIAN_POINT('Ctrl Pts',(44.2348146748757,46.8220965137346,48.5958168055374));
#20066=CARTESIAN_POINT('Ctrl Pts',(44.2140529332195,46.8176932672845,48.6597524782355));
#20067=CARTESIAN_POINT('Ctrl Pts',(44.1899161925483,46.8132900208344,48.7226910456546));
#20068=CARTESIAN_POINT('Ctrl Pts',(44.1625250745046,46.8088867743843,48.7842499082835));
#20069=CARTESIAN_POINT('Ctrl Pts',(44.1351541789645,46.8044867787933,48.8457633228104));
#20070=CARTESIAN_POINT('Ctrl Pts',(44.1045338724111,46.8000867832024,48.9058985926058));
#20071=CARTESIAN_POINT('Ctrl Pts',(44.0708335511412,46.7956867876115,48.9642913466795));
#20072=CARTESIAN_POINT('Ctrl Pts',(44.037145927091,46.7912884498004,49.0226621002024));
#20073=CARTESIAN_POINT('Ctrl Pts',(44.0003808416171,46.7868901119892,49.0792912040808));
#20074=CARTESIAN_POINT('Ctrl Pts',(43.9607535563198,46.7824917741781,49.1338390067973));
#20075=CARTESIAN_POINT('Ctrl Pts',(43.9211268759037,46.7780935035043,49.1883859768819));
#20076=CARTESIAN_POINT('Ctrl Pts',(43.8786383805713,46.7736952328306,49.2408513026502));
#20077=CARTESIAN_POINT('Ctrl Pts',(43.8335454064445,46.7692969621568,49.2909260724619));
#20078=CARTESIAN_POINT('Ctrl Pts',(43.7884060269328,46.7648941652027,49.3410523744471));
#20079=CARTESIAN_POINT('Ctrl Pts',(43.7406571573197,46.7604913682486,49.3887828354145));
#20080=CARTESIAN_POINT('Ctrl Pts',(43.6905942279537,46.7560885712944,49.4338441671509));
#20081=CARTESIAN_POINT('Ctrl Pts',(43.6405030602585,46.7516832909134,49.4789309160319));
#20082=CARTESIAN_POINT('Ctrl Pts',(43.5880956285632,46.7472780105323,49.5213452243093));
#20083=CARTESIAN_POINT('Ctrl Pts',(43.5336994733685,46.7428727301512,49.5608549134958));
#20084=CARTESIAN_POINT('Ctrl Pts',(43.4792064486823,46.7384596047805,49.6004349621312));
#20085=CARTESIAN_POINT('Ctrl Pts',(43.4227180557824,46.7340464794098,49.6370997956782));
#20086=CARTESIAN_POINT('Ctrl Pts',(43.3645889023727,46.7296333540392,49.6706617869334));
#20087=CARTESIAN_POINT('Ctrl Pts',(43.3326038970716,46.7272050744222,49.6891289485079));
#20088=CARTESIAN_POINT('Ctrl Pts',(43.3001225346997,46.7247767948053,49.7066575081409));
#20089=CARTESIAN_POINT('Ctrl Pts',(43.267206383005,46.7223485151883,49.7232224598627));
#20090=CARTESIAN_POINT('Ctrl Pts',(43.2067712897334,46.7178901171805,49.7536362339769));
#20091=CARTESIAN_POINT('Ctrl Pts',(43.1446140584476,46.7134317191727,49.78092739701));
#20092=CARTESIAN_POINT('Ctrl Pts',(43.0810899461359,46.7089733211649,49.8048986237938));
#20093=CARTESIAN_POINT('Ctrl Pts',(43.0176540189975,46.7045211123755,49.8288365733429));
#20094=CARTESIAN_POINT('Ctrl Pts',(42.9528554307497,46.700068903586,49.8494635543898));
#20095=CARTESIAN_POINT('Ctrl Pts',(42.8870727057927,46.6956166947966,49.8666287087077));
#20096=CARTESIAN_POINT('Ctrl Pts',(42.8213586597274,46.69116913423,49.8837759421539));
#20097=CARTESIAN_POINT('Ctrl Pts',(42.7546629897453,46.6867215736633,49.8974683956888));
#20098=CARTESIAN_POINT('Ctrl Pts',(42.6873810988408,46.6822740130967,49.9076044298882));
#20099=CARTESIAN_POINT('Ctrl Pts',(42.6201462984294,46.677829565371,49.9177333698927));
#20100=CARTESIAN_POINT('Ctrl Pts',(42.5523265776817,46.6733851176453,49.9243107586995));
#20101=CARTESIAN_POINT('Ctrl Pts',(42.4843275100686,46.6689406699196,49.9272860265009));
#20102=CARTESIAN_POINT('Ctrl Pts',(42.4163336383048,46.6644965617967,49.9302610669604));
#20103=CARTESIAN_POINT('Ctrl Pts',(42.3481609384597,46.6600524536739,49.9296344979394));
#20104=CARTESIAN_POINT('Ctrl Pts',(42.2802185983989,46.6556083455511,49.9254077419421));
#20105=CARTESIAN_POINT('Ctrl Pts',(42.2122796417916,46.6511644587399,49.9211811964325));
#20106=CARTESIAN_POINT('Ctrl Pts',(42.1445715136807,46.6467205719288,49.9133548591172));
#20107=CARTESIAN_POINT('Ctrl Pts',(42.077499663665,46.6422766851176,49.9019821476459));
#20108=CARTESIAN_POINT('Ctrl Pts',(42.0103781655728,46.6378295088425,49.8906010178405));
#20109=CARTESIAN_POINT('Ctrl Pts',(41.9438943701589,46.6333823325674,49.8756683666818));
#20110=CARTESIAN_POINT('Ctrl Pts',(41.8784436240851,46.6289351562923,49.8572887507446));
#20111=CARTESIAN_POINT('Ctrl Pts',(41.8501386723655,46.6270119221459,49.8493402677565));
#20112=CARTESIAN_POINT('Ctrl Pts',(41.8220267426197,46.6250886879995,49.8407477586424));
#20113=CARTESIAN_POINT('Ctrl Pts',(41.7941388317924,46.6231654538532,49.8315225365138));
#20114=CARTESIAN_POINT('Origin',(42.4,48.4493818343519,48.));
#20115=CARTESIAN_POINT('',(41.7941388553004,45.6566247686891,49.8315225442902));
#20116=CARTESIAN_POINT('',(41.7941388200938,45.8276962776015,49.831522532644));
#20117=CARTESIAN_POINT('',(41.7941388317924,48.4493818343519,49.8315225365138));
#20118=CARTESIAN_POINT('',(40.4708703631671,46.2939681656965,48.0011837199365));
#20119=CARTESIAN_POINT('Ctrl Pts',(41.7941388553004,45.6566247686891,49.8315225442902));
#20120=CARTESIAN_POINT('Ctrl Pts',(41.8667773820973,45.6618057094251,49.8555511106498));
#20121=CARTESIAN_POINT('Ctrl Pts',(41.9407833165274,45.6671213473477,49.8752379473992));
#20122=CARTESIAN_POINT('Ctrl Pts',(42.163798922572,45.6831907125301,49.9205651215141));
#20123=CARTESIAN_POINT('Ctrl Pts',(42.3148481722396,45.6941784801436,49.933160764554));
#20124=CARTESIAN_POINT('Ctrl Pts',(42.4915432862791,45.7063529406678,49.9271286627289));
#20125=CARTESIAN_POINT('Ctrl Pts',(42.5172487699093,45.708105795493,49.9257356877976));
#20126=CARTESIAN_POINT('Ctrl Pts',(42.5514406513741,45.7104064074252,49.9231955921762));
#20127=CARTESIAN_POINT('Ctrl Pts',(42.5599570597291,45.7109768727416,49.9225059954215));
#20128=CARTESIAN_POINT('Ctrl Pts',(42.5738205620841,45.7119010266578,49.9212906679015));
#20129=CARTESIAN_POINT('Ctrl Pts',(42.5791704236636,45.7122565647407,49.9207991512443));
#20130=CARTESIAN_POINT('Ctrl Pts',(42.5896336402088,45.712949700618,49.9197937514975));
#20131=CARTESIAN_POINT('Ctrl Pts',(42.5947470824736,45.7132873930716,49.9192817772434));
#20132=CARTESIAN_POINT('Ctrl Pts',(42.607262953155,45.7141115047742,49.917978114168));
#20133=CARTESIAN_POINT('Ctrl Pts',(42.6146630639592,45.7145966789292,49.9171639866282));
#20134=CARTESIAN_POINT('Ctrl Pts',(42.6415435548888,45.7163520574611,49.914049120686));
#20135=CARTESIAN_POINT('Ctrl Pts',(42.6609940294344,45.7176088764566,49.9114940528079));
#20136=CARTESIAN_POINT('Ctrl Pts',(42.7099017374203,45.7207430747346,49.904308909853));
#20137=CARTESIAN_POINT('Ctrl Pts',(42.739297635972,45.7226029760218,49.8992916624861));
#20138=CARTESIAN_POINT('Ctrl Pts',(42.8753828009737,45.7311506314811,49.872804212946));
#20139=CARTESIAN_POINT('Ctrl Pts',(42.9802553459919,45.7375670261326,49.8430115451974));
#20140=CARTESIAN_POINT('Ctrl Pts',(43.1919143385604,45.7510930623965,49.7630104419844));
#20141=CARTESIAN_POINT('Ctrl Pts',(43.297730851187,45.7581957959159,49.7115513754023));
#20142=CARTESIAN_POINT('Ctrl Pts',(43.4128454085964,45.7667400469537,49.6419438002967));
#20143=CARTESIAN_POINT('Ctrl Pts',(43.4273668852352,45.767833400047,49.6328969710675));
#20144=CARTESIAN_POINT('Ctrl Pts',(43.4510482080652,45.7696432095943,49.617702647737));
#20145=CARTESIAN_POINT('Ctrl Pts',(43.4602792570892,45.7703555039366,49.6116674845667));
#20146=CARTESIAN_POINT('Ctrl Pts',(43.4768407465366,45.7716460848175,49.6006358904844));
#20147=CARTESIAN_POINT('Ctrl Pts',(43.4841894858888,45.772223308108,49.5956673843802));
#20148=CARTESIAN_POINT('Ctrl Pts',(43.4998595479494,45.7734641069394,49.5849145815395));
#20149=CARTESIAN_POINT('Ctrl Pts',(43.5081700514879,45.7741282513336,49.5791150643047));
#20150=CARTESIAN_POINT('Ctrl Pts',(43.5307441189072,45.7759492575661,49.5630957048825));
#20151=CARTESIAN_POINT('Ctrl Pts',(43.5449142635461,45.7771110754136,49.5527465148691));
#20152=CARTESIAN_POINT('Ctrl Pts',(43.6258229299448,45.7838558533716,49.4919450555198));
#20153=CARTESIAN_POINT('Ctrl Pts',(43.6893552659555,45.7896000345881,49.4373939781315));
#20154=CARTESIAN_POINT('Ctrl Pts',(43.8280745170499,45.8032152007495,49.3016685120338));
#20155=CARTESIAN_POINT('Ctrl Pts',(43.9002284775379,45.811160177054,49.2178052421473));
#20156=CARTESIAN_POINT('Ctrl Pts',(44.0094480011836,45.8244327431891,49.0663235900971));
#20157=CARTESIAN_POINT('Ctrl Pts',(44.0503806153536,45.8297952656205,49.0018060615622));
#20158=CARTESIAN_POINT('Ctrl Pts',(44.0924439243999,45.8356546707957,48.9258968836376));
#20159=CARTESIAN_POINT('Ctrl Pts',(44.0974283197573,45.8363552918139,48.9167271063238));
#20160=CARTESIAN_POINT('Ctrl Pts',(44.1053551849102,45.8374792884526,48.9018577386052));
#20161=CARTESIAN_POINT('Ctrl Pts',(44.108343998255,45.8379054101292,48.8961832814476));
#20162=CARTESIAN_POINT('Ctrl Pts',(44.1136052465023,45.8386595396243,48.8860724905562));
#20163=CARTESIAN_POINT('Ctrl Pts',(44.11588884507,45.8389882347199,48.8816421454806));
#20164=CARTESIAN_POINT('Ctrl Pts',(44.1208197829061,45.8397009691612,48.871984040447));
#20165=CARTESIAN_POINT('Ctrl Pts',(44.1234604871542,45.8400845958303,48.8667530464358));
#20166=CARTESIAN_POINT('Ctrl Pts',(44.1308873316673,45.8411692855527,48.8518730010199));
#20167=CARTESIAN_POINT('Ctrl Pts',(44.1356166465556,45.8418669200859,48.8421956031449));
#20168=CARTESIAN_POINT('Ctrl Pts',(44.1672825819906,45.8465894448482,48.7759991903492));
#20169=CARTESIAN_POINT('Ctrl Pts',(44.1915379209984,45.8504665523758,48.7182312241847));
#20170=CARTESIAN_POINT('Ctrl Pts',(44.2563329770538,45.8619940556464,48.5400793803369));
#20171=CARTESIAN_POINT('Ctrl Pts',(44.2878427137848,45.8694188045737,48.4167853804526));
#20172=CARTESIAN_POINT('Ctrl Pts',(44.3192963450539,45.8820215632709,48.210862351945));
#20173=CARTESIAN_POINT('Ctrl Pts',(44.3264795799396,45.8870308556702,48.1297514046474));
#20174=CARTESIAN_POINT('Ctrl Pts',(44.3289694501331,45.8933372653506,48.0306140795009));
#20175=CARTESIAN_POINT('Ctrl Pts',(44.329169976939,45.8944782417602,48.0127877788413));
#20176=CARTESIAN_POINT('Ctrl Pts',(44.3290965247083,45.8962905197872,47.9846633791191));
#20177=CARTESIAN_POINT('Ctrl Pts',(44.3289871651644,45.8969566601649,47.9743655820161));
#20178=CARTESIAN_POINT('Ctrl Pts',(44.3286304185727,45.898200462519,47.9552150643824));
#20179=CARTESIAN_POINT('Ctrl Pts',(44.3284045119398,45.8987774345346,47.9463621791805));
#20180=CARTESIAN_POINT('Ctrl Pts',(44.3277675385058,45.9000629162437,47.9267080744489));
#20181=CARTESIAN_POINT('Ctrl Pts',(44.3273266323984,45.9007723449724,47.9159081881672));
#20182=CARTESIAN_POINT('Ctrl Pts',(44.3257743046911,45.9028521901391,47.8843863806755));
#20183=CARTESIAN_POINT('Ctrl Pts',(44.324419284977,45.9042301828235,47.8636785425948));
#20184=CARTESIAN_POINT('Ctrl Pts',(44.3205852726379,45.9073822709052,47.8167253958323));
#20185=CARTESIAN_POINT('Ctrl Pts',(44.3179018728869,45.9091624325726,47.7905014050236));
#20186=CARTESIAN_POINT('Ctrl Pts',(44.3071442517798,45.9151626978326,47.7030976412943));
#20187=CARTESIAN_POINT('Ctrl Pts',(44.2966729435862,45.9194511780744,47.6422560960795));
#20188=CARTESIAN_POINT('Ctrl Pts',(44.2729714913163,45.9271587243291,47.5354622887866));
#20189=CARTESIAN_POINT('Ctrl Pts',(44.2609144470359,45.9305512245677,47.489299886513));
#20190=CARTESIAN_POINT('Ctrl Pts',(44.2119857711351,45.9426592758852,47.3268547189059));
#20191=CARTESIAN_POINT('Ctrl Pts',(44.1658142057005,45.951428728634,47.2136653319055));
#20192=CARTESIAN_POINT('Ctrl Pts',(44.1018918143267,45.9608075272988,47.091507115101));
#20193=CARTESIAN_POINT('Ctrl Pts',(44.0943503647751,45.9618798451371,47.0775185903944));
#20194=CARTESIAN_POINT('Ctrl Pts',(44.0835502060202,45.9633671080864,47.0580649207555));
#20195=CARTESIAN_POINT('Ctrl Pts',(44.0804362601628,45.9637905095421,47.0525207294839));
#20196=CARTESIAN_POINT('Ctrl Pts',(44.0749968940717,45.9645206737539,47.0429474410594));
#20197=CARTESIAN_POINT('Ctrl Pts',(44.0726842319738,45.96482823164,47.0389112127462));
#20198=CARTESIAN_POINT('Ctrl Pts',(44.0677506554542,45.9654781951372,47.0303725208013));
#20199=CARTESIAN_POINT('Ctrl Pts',(44.0651260554681,45.9658203513396,47.0258722271055));
#20200=CARTESIAN_POINT('Ctrl Pts',(44.0585289953391,45.9666715556365,47.0146650879303));
#20201=CARTESIAN_POINT('Ctrl Pts',(44.0545340049802,45.967179163553,47.0079714979918));
#20202=CARTESIAN_POINT('Ctrl Pts',(44.0390527350458,45.9691171294027,46.9823863695682));
#20203=CARTESIAN_POINT('Ctrl Pts',(44.0272820706572,45.9705301891106,46.9636677498552));
#20204=CARTESIAN_POINT('Ctrl Pts',(43.9959630396975,45.9741491133502,46.9157116801642));
#20205=CARTESIAN_POINT('Ctrl Pts',(43.9759318279895,45.9763298248796,46.8867981518588));
#20206=CARTESIAN_POINT('Ctrl Pts',(43.8996140899327,45.984229705434,46.782831684283));
#20207=CARTESIAN_POINT('Ctrl Pts',(43.8386639034537,45.9897811464425,46.7113614646491));
#20208=CARTESIAN_POINT('Ctrl Pts',(43.6856272587649,46.0027877866331,46.5563648316089));
#20209=CARTESIAN_POINT('Ctrl Pts',(43.590209373986,46.0102638299392,46.4767417427015));
#20210=CARTESIAN_POINT('Ctrl Pts',(43.4737487735197,46.01922156021,46.3972222869714));
#20211=CARTESIAN_POINT('Ctrl Pts',(43.4595522659272,46.0203104333083,46.3878021858034));
#20212=CARTESIAN_POINT('Ctrl Pts',(43.4359817098638,46.0221143472094,46.3726077265948));
#20213=CARTESIAN_POINT('Ctrl Pts',(43.4266795027096,46.0228252730752,46.366723261316));
#20214=CARTESIAN_POINT('Ctrl Pts',(43.4097920020359,46.0241143857542,46.356241705648));
#20215=CARTESIAN_POINT('Ctrl Pts',(43.4022243435893,46.0246915202163,46.3516166773702));
#20216=CARTESIAN_POINT('Ctrl Pts',(43.3859288005859,46.0259332503235,46.3418112392476));
#20217=CARTESIAN_POINT('Ctrl Pts',(43.3771914190204,46.0265984230905,46.3366472142057));
#20218=CARTESIAN_POINT('Ctrl Pts',(43.3531769689252,46.0284251734035,46.3227085525852));
#20219=CARTESIAN_POINT('Ctrl Pts',(43.3378201183847,46.0295917594998,46.3140740455062));
#20220=CARTESIAN_POINT('Ctrl Pts',(43.2476104723796,46.0364372790108,46.2649668870141));
#20221=CARTESIAN_POINT('Ctrl Pts',(43.1702741269578,46.0422832705227,46.2292776725919));
#20222=CARTESIAN_POINT('Ctrl Pts',(42.9813282326039,46.0564902560166,46.1568076039486));
#20223=CARTESIAN_POINT('Ctrl Pts',(42.8682119539161,46.0649456452814,46.124879865722));
#20224=CARTESIAN_POINT('Ctrl Pts',(42.6859905278963,46.0780816973697,46.0909727782788));
#20225=CARTESIAN_POINT('Ctrl Pts',(42.6184533488154,46.0828437093803,46.0820699415558));
#20226=CARTESIAN_POINT('Ctrl Pts',(42.5402670456198,46.0881377491668,46.075948357268));
#20227=CARTESIAN_POINT('Ctrl Pts',(42.5299473831055,46.08883210117,46.075223842332));
#20228=CARTESIAN_POINT('Ctrl Pts',(42.5132480335645,46.0899480651109,46.0741863471328));
#20229=CARTESIAN_POINT('Ctrl Pts',(42.5068719079531,46.0903723614325,46.0738219861943));
#20230=CARTESIAN_POINT('Ctrl Pts',(42.495517170928,46.0911246142364,46.0732296807967));
#20231=CARTESIAN_POINT('Ctrl Pts',(42.4905393713068,46.0914532427062,46.0729893573087));
#20232=CARTESIAN_POINT('Ctrl Pts',(42.4796827908146,46.0921674562491,46.0725073734404));
#20233=CARTESIAN_POINT('Ctrl Pts',(42.4738038103962,46.0925526162157,46.0722733149012));
#20234=CARTESIAN_POINT('Ctrl Pts',(42.4570569256685,46.0936454741309,46.0716832991742));
#20235=CARTESIAN_POINT('Ctrl Pts',(42.4461867476324,46.0943496658085,46.0713923185081));
#20236=CARTESIAN_POINT('Ctrl Pts',(42.3699953405961,46.0992529352522,46.0699973354233));
#20237=CARTESIAN_POINT('Ctrl Pts',(42.3046499611367,46.1032910748266,46.0721201064787));
#20238=CARTESIAN_POINT('Ctrl Pts',(42.1098528306854,46.1151579926013,46.0883800309589));
#20239=CARTESIAN_POINT('Ctrl Pts',(41.9816010256449,46.1227646625686,46.1122975347731));
#20240=CARTESIAN_POINT('Ctrl Pts',(41.7841648662026,46.1352491303514,46.1702434568717));
#20241=CARTESIAN_POINT('Ctrl Pts',(41.7129219812569,46.1399188927578,46.1957872283272));
#20242=CARTESIAN_POINT('Ctrl Pts',(41.62720463498,46.1458468374139,46.2323352684189));
#20243=CARTESIAN_POINT('Ctrl Pts',(41.6111373411609,46.1469716954382,46.2394469754652));
#20244=CARTESIAN_POINT('Ctrl Pts',(41.5858611883222,46.1487641513322,46.251050182646));
#20245=CARTESIAN_POINT('Ctrl Pts',(41.5765868643382,46.149426782356,46.2553973892012));
#20246=CARTESIAN_POINT('Ctrl Pts',(41.5595118850458,46.150656134477,46.2635675239652));
#20247=CARTESIAN_POINT('Ctrl Pts',(41.5517015491145,46.1512221221055,46.2673697020795));
#20248=CARTESIAN_POINT('Ctrl Pts',(41.5344715870287,46.1524789889194,46.2759019103531));
#20249=CARTESIAN_POINT('Ctrl Pts',(41.5250645661024,46.1531707204732,46.2806566266772));
#20250=CARTESIAN_POINT('Ctrl Pts',(41.5055594783753,46.1546167333823,46.2907168689194));
#20251=CARTESIAN_POINT('Ctrl Pts',(41.4954685841182,46.1553714522756,46.2960353357381));
#20252=CARTESIAN_POINT('Ctrl Pts',(41.469487169611,46.157332121533,46.3100248186557));
#20253=CARTESIAN_POINT('Ctrl Pts',(41.4536707705822,46.1585427881257,46.3188304092879));
#20254=CARTESIAN_POINT('Ctrl Pts',(41.4071462348321,46.162155785298,46.3455969504621));
#20255=CARTESIAN_POINT('Ctrl Pts',(41.3768097755785,46.1645797823264,46.3641853586077));
#20256=CARTESIAN_POINT('Ctrl Pts',(41.205262518966,46.1786855298452,46.4759388274663));
#20257=CARTESIAN_POINT('Ctrl Pts',(41.0762883891773,46.1909742825748,46.5865173654446));
#20258=CARTESIAN_POINT('Ctrl Pts',(40.9279603339567,46.206612720103,46.7520163552216));
#20259=CARTESIAN_POINT('Ctrl Pts',(40.8941542568313,46.2102978522744,46.7930229208938));
#20260=CARTESIAN_POINT('Ctrl Pts',(40.8556297705303,46.2146002309119,46.843895616358));
#20261=CARTESIAN_POINT('Ctrl Pts',(40.8492491898741,46.2153164410881,46.8524684364828));
#20262=CARTESIAN_POINT('Ctrl Pts',(40.8394523048512,46.2164212671498,46.8658622887984));
#20263=CARTESIAN_POINT('Ctrl Pts',(40.8359864729835,46.2168131431537,46.870646580369));
#20264=CARTESIAN_POINT('Ctrl Pts',(40.8296411320068,46.2175323831199,46.8794910276876));
#20265=CARTESIAN_POINT('Ctrl Pts',(40.8267553565651,46.2178601624578,46.8835464074671));
#20266=CARTESIAN_POINT('Ctrl Pts',(40.8202268490702,46.2186032897646,46.8927964956614));
#20267=CARTESIAN_POINT('Ctrl Pts',(40.8165940252868,46.2190179635082,46.89799803517));
#20268=CARTESIAN_POINT('Ctrl Pts',(40.8055056070785,46.2202875649612,46.9140426613678));
#20269=CARTESIAN_POINT('Ctrl Pts',(40.7981350544288,46.221136972461,46.9249444527828));
#20270=CARTESIAN_POINT('Ctrl Pts',(40.7811727483579,46.2231069568287,46.9505952283035));
#20271=CARTESIAN_POINT('Ctrl Pts',(40.7716699154517,46.2242224034717,46.9654018999921));
#20272=CARTESIAN_POINT('Ctrl Pts',(40.7387771931728,46.2281337404714,47.0182292473946));
#20273=CARTESIAN_POINT('Ctrl Pts',(40.7165043999262,46.2308760644686,47.0569315369129));
#20274=CARTESIAN_POINT('Ctrl Pts',(40.629871036275,46.2420985689469,47.2203382254642));
#20275=CARTESIAN_POINT('Ctrl Pts',(40.5778687477796,46.250277495711,47.3511018331962));
#20276=CARTESIAN_POINT('Ctrl Pts',(40.5241453152251,46.2625830210372,47.5455898767062));
#20277=CARTESIAN_POINT('Ctrl Pts',(40.5106235816986,46.26639096728,47.6055700443864));
#20278=CARTESIAN_POINT('Ctrl Pts',(40.4968945368282,46.2714233410843,47.6836907565701));
#20279=CARTESIAN_POINT('Ctrl Pts',(40.4940460341359,46.2725644777965,47.7013339870714));
#20280=CARTESIAN_POINT('Ctrl Pts',(40.4898039573857,46.274436801096,47.730147659409));
#20281=CARTESIAN_POINT('Ctrl Pts',(40.4882622667632,46.2751632992933,47.7412954631389));
#20282=CARTESIAN_POINT('Ctrl Pts',(40.4856781407055,46.2764689072934,47.7612672717363));
#20283=CARTESIAN_POINT('Ctrl Pts',(40.4845989544873,46.277046836753,47.7700862619979));
#20284=CARTESIAN_POINT('Ctrl Pts',(40.4826279140193,46.278169330505,47.787171515488));
#20285=CARTESIAN_POINT('Ctrl Pts',(40.481728501575,46.2787136420374,47.7954367223339));
#20286=CARTESIAN_POINT('Ctrl Pts',(40.4798858795933,46.2799029464669,47.813451703841));
#20287=CARTESIAN_POINT('Ctrl Pts',(40.4789634486876,46.2805485803986,47.8232033239643));
#20288=CARTESIAN_POINT('Ctrl Pts',(40.4761992387617,46.2826605122948,47.8550073051383));
#20289=CARTESIAN_POINT('Ctrl Pts',(40.4746626862145,46.2841363078213,47.8770837311232));
#20290=CARTESIAN_POINT('Ctrl Pts',(40.4717266466095,46.2879129183618,47.9331868341155));
#20291=CARTESIAN_POINT('Ctrl Pts',(40.4708478359641,46.2902291322323,47.967231647312));
#20292=CARTESIAN_POINT('Ctrl Pts',(40.4708704245423,46.2925701609289,48.0012798415654));
#20293=CARTESIAN_POINT('Ctrl Pts',(41.7941388317924,46.4519835383214,49.8315225365139));
#20294=CARTESIAN_POINT('Ctrl Pts',(41.727826215268,46.4474003125196,49.8095865578331));
#20295=CARTESIAN_POINT('Ctrl Pts',(41.6626060745432,46.4428170867179,49.7840113396514));
#20296=CARTESIAN_POINT('Ctrl Pts',(41.5989029229069,46.4382338609161,49.7549319160506));
#20297=CARTESIAN_POINT('Ctrl Pts',(41.5371339006962,46.4337897891696,49.7267353901937));
#20298=CARTESIAN_POINT('Ctrl Pts',(41.4767915503687,46.4293457174232,49.6952446309924));
#20299=CARTESIAN_POINT('Ctrl Pts',(41.4182454283156,46.4249016456767,49.6606325655836));
#20300=CARTESIAN_POINT('Ctrl Pts',(41.3597310685853,46.420459984919,49.6260392778419));
#20301=CARTESIAN_POINT('Ctrl Pts',(41.3030114280562,46.4160183241613,49.588328293954));
#20302=CARTESIAN_POINT('Ctrl Pts',(41.248431409697,46.4115766634036,49.5477184300536));
#20303=CARTESIAN_POINT('Ctrl Pts',(41.1938621552395,46.4071358786002,49.5071165749556));
#20304=CARTESIAN_POINT('Ctrl Pts',(41.1414320807568,46.4026950937967,49.4636172698326));
#20305=CARTESIAN_POINT('Ctrl Pts',(41.0914555183565,46.3982543089933,49.4174815330227));
#20306=CARTESIAN_POINT('Ctrl Pts',(41.0414715553891,46.3938128665951,49.371338964398));
#20307=CARTESIAN_POINT('Ctrl Pts',(40.9939421862332,46.3893714241968,49.3225595260854));
#20308=CARTESIAN_POINT('Ctrl Pts',(40.9491458165153,46.3849299817986,49.2714419747535));
#20309=CARTESIAN_POINT('Ctrl Pts',(40.9042989929577,46.3804835370347,49.2202668500788));
#20310=CARTESIAN_POINT('Ctrl Pts',(40.862191634198,46.3760370922708,49.166748731578));
#20311=CARTESIAN_POINT('Ctrl Pts',(40.8230619659899,46.3715906475069,49.1112195974659));
#20312=CARTESIAN_POINT('Ctrl Pts',(40.7839056121508,46.3671411703589,49.0556525936237));
#20313=CARTESIAN_POINT('Ctrl Pts',(40.7477312506203,46.3626916932108,48.9980722635646));
#20314=CARTESIAN_POINT('Ctrl Pts',(40.7147323498353,46.3582422160628,48.9388373150915));
#20315=CARTESIAN_POINT('Ctrl Pts',(40.6816785786209,46.3537853403435,48.8795038710027));
#20316=CARTESIAN_POINT('Ctrl Pts',(40.6518110148748,46.3493284646241,48.8185107635707));
#20317=CARTESIAN_POINT('Ctrl Pts',(40.6252755672461,46.3448715889048,48.7562378889518));
#20318=CARTESIAN_POINT('Ctrl Pts',(40.6195490420395,46.3439097656295,48.7427989904948));
#20319=CARTESIAN_POINT('Ctrl Pts',(40.6139775172925,46.3429479423542,48.729300546802));
#20320=CARTESIAN_POINT('Ctrl Pts',(40.6085621529345,46.3419861190789,48.7157464613962));
#20321=CARTESIAN_POINT('Ctrl Pts',(40.580284191365,46.3369636681749,48.644969708278));
#20322=CARTESIAN_POINT('Ctrl Pts',(40.556173274459,46.3319412172709,48.5724370836976));
#20323=CARTESIAN_POINT('Ctrl Pts',(40.5364232936375,46.3269187663669,48.4986225189492));
#20324=CARTESIAN_POINT('Ctrl Pts',(40.5167501656455,46.3219158592573,48.425095187804));
#20325=CARTESIAN_POINT('Ctrl Pts',(40.5014042471389,46.3169129521476,48.3502961023876));
#20326=CARTESIAN_POINT('Ctrl Pts',(40.4905304824803,46.3119100450379,48.2747157049807));
#20327=CARTESIAN_POINT('Ctrl Pts',(40.4797262149631,46.3069391128471,48.1996183621309));
#20328=CARTESIAN_POINT('Ctrl Pts',(40.4733372415611,46.3019681806564,48.1237499091596));
#20329=CARTESIAN_POINT('Ctrl Pts',(40.4714575774903,46.2969972484656,48.0476096784313));
#20330=CARTESIAN_POINT('Ctrl Pts',(40.4710757806877,46.2959875542092,48.0321440975915));
#20331=CARTESIAN_POINT('Ctrl Pts',(40.470879863975,46.2949778599529,48.0166673571739));
#20332=CARTESIAN_POINT('Ctrl Pts',(40.4708703631671,46.2939681656965,48.0011837199365));
#20333=CARTESIAN_POINT('',(40.4708700795635,46.4650068343519,48.0005540547159));
#20334=CARTESIAN_POINT('Ctrl Pts',(41.7941388317924,46.6231654538532,49.8315225365138));
#20335=CARTESIAN_POINT('Ctrl Pts',(41.7287833055596,46.6186583403414,49.8099031599117));
#20336=CARTESIAN_POINT('Ctrl Pts',(41.6646598591436,46.6141512268296,49.7848056142629));
#20337=CARTESIAN_POINT('Ctrl Pts',(41.6021507757283,46.6096441133178,49.7564108779636));
#20338=CARTESIAN_POINT('Ctrl Pts',(41.5396416923129,46.605136999806,49.7280161416644));
#20339=CARTESIAN_POINT('Ctrl Pts',(41.4787474022242,46.6006298862943,49.6963245113389));
#20340=CARTESIAN_POINT('Ctrl Pts',(41.4198212647442,46.5961227727825,49.6615631808187));
#20341=CARTESIAN_POINT('Ctrl Pts',(41.3614665912009,46.5916593691241,49.6271389646527));
#20342=CARTESIAN_POINT('Ctrl Pts',(41.3048151949058,46.5871959654657,49.5895705731172));
#20343=CARTESIAN_POINT('Ctrl Pts',(41.250225540661,46.5827325618073,49.5490517259122));
#20344=CARTESIAN_POINT('Ctrl Pts',(41.1957165968945,46.5782757572646,49.5085927855813));
#20345=CARTESIAN_POINT('Ctrl Pts',(41.1432637369315,46.5738189527219,49.4651923385466));
#20346=CARTESIAN_POINT('Ctrl Pts',(41.0931985951083,46.5693621481793,49.4190886670935));
#20347=CARTESIAN_POINT('Ctrl Pts',(41.0431904209025,46.5649104149003,49.3730374556198));
#20348=CARTESIAN_POINT('Ctrl Pts',(40.9955649291494,46.5604586816213,49.324289460263));
#20349=CARTESIAN_POINT('Ctrl Pts',(40.9506212007339,46.5560069483423,49.2731235812512));
#20350=CARTESIAN_POINT('Ctrl Pts',(40.905704581011,46.5515579002136,49.2219885639444));
#20351=CARTESIAN_POINT('Ctrl Pts',(40.8634668395876,46.547108852085,49.1684389249248));
#20352=CARTESIAN_POINT('Ctrl Pts',(40.8241695250672,46.5426598039564,49.1127896796669));
#20353=CARTESIAN_POINT('Ctrl Pts',(40.78488245976,46.5382119161931,49.0571549484027));
#20354=CARTESIAN_POINT('Ctrl Pts',(40.7485345823357,46.5337640284298,48.9994220997049));
#20355=CARTESIAN_POINT('Ctrl Pts',(40.7153454172212,46.5293161406666,48.9399369625791));
#20356=CARTESIAN_POINT('Ctrl Pts',(40.6821535461303,46.5248678902585,48.8804469755157));
#20357=CARTESIAN_POINT('Ctrl Pts',(40.6521211360122,46.5204196398504,48.8192048471323));
#20358=CARTESIAN_POINT('Ctrl Pts',(40.6254219621436,46.5159713894423,48.756581353496));
#20359=CARTESIAN_POINT('Ctrl Pts',(40.5986937094228,46.5115182943144,48.6938896547785));
#20360=CARTESIAN_POINT('Ctrl Pts',(40.5753061307835,46.5070651991865,48.629814041767));
#20361=CARTESIAN_POINT('Ctrl Pts',(40.5553845982352,46.5026121040586,48.5647447002603));
#20362=CARTESIAN_POINT('Ctrl Pts',(40.5354507774457,46.4981562621186,48.4996352218936));
#20363=CARTESIAN_POINT('Ctrl Pts',(40.5189873765866,46.4937004201785,48.4335312723801));
#20364=CARTESIAN_POINT('Ctrl Pts',(40.5060689709932,46.4892445782385,48.3668348596646));
#20365=CARTESIAN_POINT('Ctrl Pts',(40.493128187358,46.4847810176202,48.3000229113981));
#20366=CARTESIAN_POINT('Ctrl Pts',(40.4837447224647,46.4803174570019,48.2326169384692));
#20367=CARTESIAN_POINT('Ctrl Pts',(40.4779413739301,46.4758538963836,48.1650248310114));
#20368=CARTESIAN_POINT('Ctrl Pts',(40.4753597451538,46.4738682743813,48.1349563750796));
#20369=CARTESIAN_POINT('Ctrl Pts',(40.4734859041685,46.471882652379,48.1048510896329));
#20370=CARTESIAN_POINT('Ctrl Pts',(40.4723185475692,46.4698970303766,48.0747447312809));
#20371=CARTESIAN_POINT('Ctrl Pts',(40.4713602244183,46.4682669650351,48.0500293870446));
#20372=CARTESIAN_POINT('Ctrl Pts',(40.47087718529,46.4666368996935,48.0252950581875));
#20373=CARTESIAN_POINT('Ctrl Pts',(40.4708700795635,46.4650068343519,48.0005540547159));
#20374=CARTESIAN_POINT('Ctrl Pts',(40.4708701150492,46.4632498880547,48.0006662504151));
#20375=CARTESIAN_POINT('Ctrl Pts',(40.4708552840327,46.460507586754,47.9577230019347));
#20376=CARTESIAN_POINT('Ctrl Pts',(40.4722743616713,46.4578329855591,47.9147871563977));
#20377=CARTESIAN_POINT('Ctrl Pts',(40.4865662148564,46.4446308769824,47.6999814642341));
#20378=CARTESIAN_POINT('Ctrl Pts',(40.5209937658437,46.4347081789134,47.530337677286));
#20379=CARTESIAN_POINT('Ctrl Pts',(40.5951923604088,46.4207891607846,47.3165354800588));
#20380=CARTESIAN_POINT('Ctrl Pts',(40.6150138033227,46.4174174900997,47.266325807559));
#20381=CARTESIAN_POINT('Ctrl Pts',(40.6431677001459,46.4129912787833,47.2029301328526));
#20382=CARTESIAN_POINT('Ctrl Pts',(40.6495916749533,46.4120022547676,47.1889199940303));
#20383=CARTESIAN_POINT('Ctrl Pts',(40.660300513753,46.4103859051362,47.166284840379));
#20384=CARTESIAN_POINT('Ctrl Pts',(40.6644833878878,46.4097621385383,47.1576121123378));
#20385=CARTESIAN_POINT('Ctrl Pts',(40.6726595190762,46.4085570646184,47.1409792055157));
#20386=CARTESIAN_POINT('Ctrl Pts',(40.6766433236021,46.4079761017127,47.1330146346165));
#20387=CARTESIAN_POINT('Ctrl Pts',(40.6859209663589,46.4066370447662,47.1147830456223));
#20388=CARTESIAN_POINT('Ctrl Pts',(40.6912521191776,46.4058776421258,47.1045355061669));
#20389=CARTESIAN_POINT('Ctrl Pts',(40.7081867888205,46.4034958406936,47.0726856492009));
#20390=CARTESIAN_POINT('Ctrl Pts',(40.7201099752349,46.4018620918835,47.0512570125377));
#20391=CARTESIAN_POINT('Ctrl Pts',(40.805821197561,46.3904026808009,46.9038982882746));
#20392=CARTESIAN_POINT('Ctrl Pts',(40.893271933691,46.3800615731715,46.7864927129354));
#20393=CARTESIAN_POINT('Ctrl Pts',(41.047707628527,46.3639232627292,46.6218785812438));
#20394=CARTESIAN_POINT('Ctrl Pts',(41.1058815170792,46.3582164254853,46.5671105782759));
#20395=CARTESIAN_POINT('Ctrl Pts',(41.1867019593298,46.3509008272281,46.4999707734454));
#20396=CARTESIAN_POINT('Ctrl Pts',(41.2064355536179,46.3491590650644,46.4842216991207));
#20397=CARTESIAN_POINT('Ctrl Pts',(41.2359194179308,46.346627730218,46.4616240404142));
#20398=CARTESIAN_POINT('Ctrl Pts',(41.2454323531625,46.345821565881,46.4544716890596));
#20399=CARTESIAN_POINT('Ctrl Pts',(41.2606977153002,46.3445454324041,46.4432139565821));
#20400=CARTESIAN_POINT('Ctrl Pts',(41.2664073929846,46.3440719693008,46.4390514787571));
#20401=CARTESIAN_POINT('Ctrl Pts',(41.2771912670167,46.3431851458396,46.4312801801213));
#20402=CARTESIAN_POINT('Ctrl Pts',(41.2822602985823,46.3427713336254,46.4276643848327));
#20403=CARTESIAN_POINT('Ctrl Pts',(41.2913076407346,46.3420382782745,46.4212766811355));
#20404=CARTESIAN_POINT('Ctrl Pts',(41.2952789741683,46.3417183893128,46.4184951717373));
#20405=CARTESIAN_POINT('Ctrl Pts',(41.3039411618193,46.3410247574061,46.4124767531489));
#20406=CARTESIAN_POINT('Ctrl Pts',(41.3086358880727,46.3406514062176,46.4092456464545));
#20407=CARTESIAN_POINT('Ctrl Pts',(41.3214191017703,46.3396416000418,46.4005309338823));
#20408=CARTESIAN_POINT('Ctrl Pts',(41.3295351781033,46.3390078011307,46.3950878147536));
#20409=CARTESIAN_POINT('Ctrl Pts',(41.3702073480632,46.3358661096318,46.3682564629621));
#20410=CARTESIAN_POINT('Ctrl Pts',(41.4033670899543,46.3334139538375,46.3477944422935));
#20411=CARTESIAN_POINT('Ctrl Pts',(41.5380249657494,46.3237890605195,46.2702312815312));
#20412=CARTESIAN_POINT('Ctrl Pts',(41.6439863349158,46.3169361054216,46.2213632729674));
#20413=CARTESIAN_POINT('Ctrl Pts',(41.8592105471828,46.3032767390657,46.1448381501431));
#20414=CARTESIAN_POINT('Ctrl Pts',(41.9677566965841,46.2965019188156,46.1165882636696));
#20415=CARTESIAN_POINT('Ctrl Pts',(42.099027387672,46.2880679421048,46.0943748592831));
#20416=CARTESIAN_POINT('Ctrl Pts',(42.1199792489612,46.2867152793351,46.0911836095156));
#20417=CARTESIAN_POINT('Ctrl Pts',(42.1517897084826,46.2846498068543,46.0868734412592));
#20418=CARTESIAN_POINT('Ctrl Pts',(42.1626126699525,46.2839450149413,46.0855003718904));
#20419=CARTESIAN_POINT('Ctrl Pts',(42.1822605533313,46.2826615730958,46.083176882453));
#20420=CARTESIAN_POINT('Ctrl Pts',(42.1910815536594,46.2820839192053,46.0821954195086));
#20421=CARTESIAN_POINT('Ctrl Pts',(42.2101047262249,46.2808349054589,46.0802116190892));
#20422=CARTESIAN_POINT('Ctrl Pts',(42.2203087040767,46.2801629219421,46.0792296665749));
#20423=CARTESIAN_POINT('Ctrl Pts',(42.2480238825849,46.2783320361356,46.0767853498229));
#20424=CARTESIAN_POINT('Ctrl Pts',(42.2655476681068,46.2771682256669,46.0754808739473));
#20425=CARTESIAN_POINT('Ctrl Pts',(42.3592648261936,46.270909488596,46.069790748067));
#20426=CARTESIAN_POINT('Ctrl Pts',(42.4356408428096,46.2656825054002,46.0696906456074));
#20427=CARTESIAN_POINT('Ctrl Pts',(42.6407527808226,46.2513188618444,46.0815991318318));
#20428=CARTESIAN_POINT('Ctrl Pts',(42.7686100326898,46.2419975556876,46.1020152387178));
#20429=CARTESIAN_POINT('Ctrl Pts',(42.9561618963193,46.2282753272947,46.151640133866));
#20430=CARTESIAN_POINT('Ctrl Pts',(43.0180011237031,46.2237487159198,46.1713866711326));
#20431=CARTESIAN_POINT('Ctrl Pts',(43.0889124536931,46.2186412460737,46.1980398364184));
#20432=CARTESIAN_POINT('Ctrl Pts',(43.0990589248348,46.2179125068184,46.2019517712064));
#20433=CARTESIAN_POINT('Ctrl Pts',(43.114651996241,46.2167963765403,46.2081155720415));
#20434=CARTESIAN_POINT('Ctrl Pts',(43.1201220697898,46.2164055613946,46.2103068738502));
#20435=CARTESIAN_POINT('Ctrl Pts',(43.1302073933846,46.2156864605986,46.2144007622343));
#20436=CARTESIAN_POINT('Ctrl Pts',(43.1348253009995,46.2153577749367,46.2162961979812));
#20437=CARTESIAN_POINT('Ctrl Pts',(43.1453481982665,46.2146100792474,46.2206631587664));
#20438=CARTESIAN_POINT('Ctrl Pts',(43.1512482805549,46.214191766579,46.2231461638364));
#20439=CARTESIAN_POINT('Ctrl Pts',(43.166688881263,46.2130991568552,46.2297348813172));
#20440=CARTESIAN_POINT('Ctrl Pts',(43.1762089422018,46.2124276302207,46.2338884178587));
#20441=CARTESIAN_POINT('Ctrl Pts',(43.2525176021799,46.2070585405321,46.2679175848093));
#20442=CARTESIAN_POINT('Ctrl Pts',(43.317599017047,46.2025625092259,46.3014976049751));
#20443=CARTESIAN_POINT('Ctrl Pts',(43.4778469462884,46.191318972357,46.396087673145));
#20444=CARTESIAN_POINT('Ctrl Pts',(43.5698467549764,46.1846858618212,46.4619010824607));
#20445=CARTESIAN_POINT('Ctrl Pts',(43.7195425691231,46.1727664267429,46.5902300419548));
#20446=CARTESIAN_POINT('Ctrl Pts',(43.7798511681422,46.1675811720529,46.6492031789765));
#20447=CARTESIAN_POINT('Ctrl Pts',(43.8478445496594,46.1611011175132,46.7250106967588));
#20448=CARTESIAN_POINT('Ctrl Pts',(43.8594019872309,46.1599754040952,46.738256218486));
#20449=CARTESIAN_POINT('Ctrl Pts',(43.877339452542,46.1581883652133,46.7593898434653));
#20450=CARTESIAN_POINT('Ctrl Pts',(43.8838412148424,46.1575320641356,46.7671737100688));
#20451=CARTESIAN_POINT('Ctrl Pts',(43.8959146901998,46.1562969448355,46.7818618701515));
#20452=CARTESIAN_POINT('Ctrl Pts',(43.9015007599331,46.1557187314165,46.7887540599727));
#20453=CARTESIAN_POINT('Ctrl Pts',(43.9139198585538,46.1544178075405,46.8042948922488));
#20454=CARTESIAN_POINT('Ctrl Pts',(43.9207266591163,46.1536940724038,46.8129640011806));
#20455=CARTESIAN_POINT('Ctrl Pts',(43.9378928225782,46.1518410059216,46.8352167389674));
#20456=CARTESIAN_POINT('Ctrl Pts',(43.9481465462219,46.1507075758894,46.8488802763014));
#20457=CARTESIAN_POINT('Ctrl Pts',(44.0242677010004,46.1420869247016,46.953172000813));
#20458=CARTESIAN_POINT('Ctrl Pts',(44.0822980429427,46.1343003987884,47.04923195623));
#20459=CARTESIAN_POINT('Ctrl Pts',(44.1944689927516,46.1162361746765,47.2776894348219));
#20460=CARTESIAN_POINT('Ctrl Pts',(44.2429110816477,46.105900733293,47.4121792535044));
#20461=CARTESIAN_POINT('Ctrl Pts',(44.2809943344811,46.0947049451618,47.5712285788929));
#20462=CARTESIAN_POINT('Ctrl Pts',(44.2855559377303,46.0932797267022,47.5917555718817));
#20463=CARTESIAN_POINT('Ctrl Pts',(44.2913176355134,46.0913599927763,47.6198439561263));
#20464=CARTESIAN_POINT('Ctrl Pts',(44.2928095117034,46.0908504021819,47.6273430889051));
#20465=CARTESIAN_POINT('Ctrl Pts',(44.2952368644038,46.0899998818677,47.6399352908648));
#20466=CARTESIAN_POINT('Ctrl Pts',(44.296196480144,46.0896576129552,47.6450235533307));
#20467=CARTESIAN_POINT('Ctrl Pts',(44.297983297468,46.089008665436,47.6547119987486));
#20468=CARTESIAN_POINT('Ctrl Pts',(44.2988142841292,46.0887017667262,47.6593114078387));
#20469=CARTESIAN_POINT('Ctrl Pts',(44.3007533065816,46.0879731721839,47.6702711646044));
#20470=CARTESIAN_POINT('Ctrl Pts',(44.3018461546069,46.0875523279078,47.6766341939783));
#20471=CARTESIAN_POINT('Ctrl Pts',(44.3056160557135,46.0860628734684,47.6992645805628));
#20472=CARTESIAN_POINT('Ctrl Pts',(44.3081165955785,46.0850036634006,47.7155611740648));
#20473=CARTESIAN_POINT('Ctrl Pts',(44.3247345871394,46.0773911685787,47.8339713894062));
#20474=CARTESIAN_POINT('Ctrl Pts',(44.3308578064202,46.071209084178,47.9370524185077));
#20475=CARTESIAN_POINT('Ctrl Pts',(44.3264794976112,46.0586467317207,48.1474271025378));
#20476=CARTESIAN_POINT('Ctrl Pts',(44.3152990680754,46.0522858907156,48.2543340425677));
#20477=CARTESIAN_POINT('Ctrl Pts',(44.2849069673674,46.042271368237,48.4144484971756));
#20478=CARTESIAN_POINT('Ctrl Pts',(44.2721633146581,46.0387952519515,48.4686634857562));
#20479=CARTESIAN_POINT('Ctrl Pts',(44.2528655649094,46.0342470983823,48.5372855510325));
#20480=CARTESIAN_POINT('Ctrl Pts',(44.2484543780888,46.0332447615468,48.5522707251424));
#20481=CARTESIAN_POINT('Ctrl Pts',(44.241007556239,46.0316098728776,48.5764789451563));
#20482=CARTESIAN_POINT('Ctrl Pts',(44.2380833586545,46.0309809837329,48.5857357401003));
#20483=CARTESIAN_POINT('Ctrl Pts',(44.2323307493011,46.0297681788473,48.6034787423235));
#20484=CARTESIAN_POINT('Ctrl Pts',(44.2295129293274,46.0291846262352,48.6119681398054));
#20485=CARTESIAN_POINT('Ctrl Pts',(44.2229194993601,46.0278426240446,48.6313799220639));
#20486=CARTESIAN_POINT('Ctrl Pts',(44.2191046083557,46.0270828871039,48.6422885029913));
#20487=CARTESIAN_POINT('Ctrl Pts',(44.2066279741783,46.024649767361,48.6769621189402));
#20488=CARTESIAN_POINT('Ctrl Pts',(44.1975970492132,46.0229641677198,48.7005905311966));
#20489=CARTESIAN_POINT('Ctrl Pts',(44.1373302123194,46.0121654241522,48.8494280982201));
#20490=CARTESIAN_POINT('Ctrl Pts',(44.0735155958563,46.0026203357195,48.969111649272));
#20491=CARTESIAN_POINT('Ctrl Pts',(43.9562593991378,45.9876772060383,49.1423984061069));
#20492=CARTESIAN_POINT('Ctrl Pts',(43.9113000960647,45.9823794645922,49.201245268887));
#20493=CARTESIAN_POINT('Ctrl Pts',(43.8407992349202,45.9747807173391,49.2832800448694));
#20494=CARTESIAN_POINT('Ctrl Pts',(43.8178423605574,45.9724032487436,49.3085997964914));
#20495=CARTESIAN_POINT('Ctrl Pts',(43.7792581395926,45.9685785780702,49.3489471498493));
#20496=CARTESIAN_POINT('Ctrl Pts',(43.7640293725413,45.9671099460054,49.3643443102512));
#20497=CARTESIAN_POINT('Ctrl Pts',(43.7430175918665,45.9651422122111,49.3848848430884));
#20498=CARTESIAN_POINT('Ctrl Pts',(43.7374588396382,45.9646270503943,49.3902539832684));
#20499=CARTESIAN_POINT('Ctrl Pts',(43.7281119385911,45.96377004313,49.3991741101396));
#20500=CARTESIAN_POINT('Ctrl Pts',(43.7243414957307,45.9634268112735,49.4027434251052));
#20501=CARTESIAN_POINT('Ctrl Pts',(43.717159191793,45.9627777500421,49.4094878292393));
#20502=CARTESIAN_POINT('Ctrl Pts',(43.713750173869,45.9624716885591,49.4126658341993));
#20503=CARTESIAN_POINT('Ctrl Pts',(43.7056351133436,45.9617477737817,49.4201761941979));
#20504=CARTESIAN_POINT('Ctrl Pts',(43.7009189381864,45.9613307444905,49.424497592443));
#20505=CARTESIAN_POINT('Ctrl Pts',(43.6842415877539,45.9598685792411,49.439627027631));
#20506=CARTESIAN_POINT('Ctrl Pts',(43.6721661282368,45.9588323915648,49.4503088697083));
#20507=CARTESIAN_POINT('Ctrl Pts',(43.5721064605865,45.9504149280176,49.5366092719332));
#20508=CARTESIAN_POINT('Ctrl Pts',(43.4775865689455,45.9435081149933,49.6043117570513));
#20509=CARTESIAN_POINT('Ctrl Pts',(43.2556401245294,45.9281528071371,49.7347671176079));
#20510=CARTESIAN_POINT('Ctrl Pts',(43.1262459069658,45.9197209442377,49.7927903907055));
#20511=CARTESIAN_POINT('Ctrl Pts',(42.971863046181,45.909441680981,49.8425386709255));
#20512=CARTESIAN_POINT('Ctrl Pts',(42.9519434963435,45.9081123185111,49.8486033702171));
#20513=CARTESIAN_POINT('Ctrl Pts',(42.9215261486687,45.9060759294906,49.8573287771559));
#20514=CARTESIAN_POINT('Ctrl Pts',(42.9110972565773,45.9053765979035,49.860225603688));
#20515=CARTESIAN_POINT('Ctrl Pts',(42.8920909661993,45.9040997799575,49.8653330769768));
#20516=CARTESIAN_POINT('Ctrl Pts',(42.883521613515,45.903523253257,49.8675727166403));
#20517=CARTESIAN_POINT('Ctrl Pts',(42.8649659909922,45.9022728997538,49.8722860426369));
#20518=CARTESIAN_POINT('Ctrl Pts',(42.8549747884349,45.9015984219757,49.8747390040079));
#20519=CARTESIAN_POINT('Ctrl Pts',(42.827665385168,45.8997512544549,49.8812126286772));
#20520=CARTESIAN_POINT('Ctrl Pts',(42.8103108184844,45.8985734896732,49.8850739062596));
#20521=CARTESIAN_POINT('Ctrl Pts',(42.7142400244263,45.8920302070028,49.9050595489422));
#20522=CARTESIAN_POINT('Ctrl Pts',(42.6346392862302,45.8865171976895,49.9164915909003));
#20523=CARTESIAN_POINT('Ctrl Pts',(42.4273863164452,45.8719478317822,49.9331507666779));
#20524=CARTESIAN_POINT('Ctrl Pts',(42.2995080821002,45.8627327477398,49.9307303290074));
#20525=CARTESIAN_POINT('Ctrl Pts',(42.1103304009486,45.8492658560347,49.9082960729596));
#20526=CARTESIAN_POINT('Ctrl Pts',(42.0482340021057,45.8448784174493,49.8978316008014));
#20527=CARTESIAN_POINT('Ctrl Pts',(41.9762203374174,45.8399081365241,49.8820386963221));
#20528=CARTESIAN_POINT('Ctrl Pts',(41.9657056821016,45.8391854442231,49.8796402090588));
#20529=CARTESIAN_POINT('Ctrl Pts',(41.9495059548467,45.8380772443336,49.8758017091104));
#20530=CARTESIAN_POINT('Ctrl Pts',(41.943806608933,45.8376883654177,49.8744237858168));
#20531=CARTESIAN_POINT('Ctrl Pts',(41.9332744837574,45.8369717093823,49.8718265651099));
#20532=CARTESIAN_POINT('Ctrl Pts',(41.9284401570581,45.836643543229,49.8706145281224));
#20533=CARTESIAN_POINT('Ctrl Pts',(41.9173997080052,45.8358958385496,49.8678010046056));
#20534=CARTESIAN_POINT('Ctrl Pts',(41.9111968286981,45.8354770066366,49.8661873156985));
#20535=CARTESIAN_POINT('Ctrl Pts',(41.8949264291925,45.8343814082306,49.8618678569942));
#20536=CARTESIAN_POINT('Ctrl Pts',(41.8848724392048,45.8337074435762,49.8591113028894));
#20537=CARTESIAN_POINT('Ctrl Pts',(41.8477587930746,45.8312291232269,49.8486114673626));
#20538=CARTESIAN_POINT('Ctrl Pts',(41.8208516596979,45.8294512529434,49.840359045563));
#20539=CARTESIAN_POINT('Ctrl Pts',(41.7941388200938,45.8276962776015,49.831522532644));
#20540=CARTESIAN_POINT('Origin',(42.4,48.4493818343519,48.));
#20541=CARTESIAN_POINT('',(41.7941389732838,44.8639880114013,49.8315225833187));
#20542=CARTESIAN_POINT('',(41.7941386463292,45.0367815693785,49.8315224751633));
#20543=CARTESIAN_POINT('',(41.7941388317924,48.4493818343519,49.8315225365138));
#20544=CARTESIAN_POINT('Ctrl Pts',(41.7941389732838,44.8639880114013,49.8315225833187));
#20545=CARTESIAN_POINT('Ctrl Pts',(41.8398698956634,44.8668818440374,49.846650206553));
#20546=CARTESIAN_POINT('Ctrl Pts',(41.8861705002305,44.8697991318275,49.8600661076338));
#20547=CARTESIAN_POINT('Ctrl Pts',(41.987195043301,44.8761965318852,49.8852747529153));
#20548=CARTESIAN_POINT('Ctrl Pts',(42.0420030289712,44.8796874134856,49.8964456470235));
#20549=CARTESIAN_POINT('Ctrl Pts',(42.1126738968819,44.8842529772068,49.9076769320419));
#20550=CARTESIAN_POINT('Ctrl Pts',(42.1281616255028,44.885257362061,49.9099454027151));
#20551=CARTESIAN_POINT('Ctrl Pts',(42.1533100192657,44.8868951995562,49.9133167836511));
#20552=CARTESIAN_POINT('Ctrl Pts',(42.1629546314003,44.8875249740215,49.9145355960799));
#20553=CARTESIAN_POINT('Ctrl Pts',(42.1814988482933,44.8887392262738,49.9167368015385));
#20554=CARTESIAN_POINT('Ctrl Pts',(42.1903969080519,44.8893233383791,49.9177302362292));
#20555=CARTESIAN_POINT('Ctrl Pts',(42.2108006020702,44.8906662690512,49.9198645323047));
#20556=CARTESIAN_POINT('Ctrl Pts',(42.2223101304359,44.8914263733883,49.9209639598153));
#20557=CARTESIAN_POINT('Ctrl Pts',(42.2590193849076,44.8938592523921,49.9241378174312));
#20558=CARTESIAN_POINT('Ctrl Pts',(42.2842494384544,44.895544220105,49.9258202351666));
#20559=CARTESIAN_POINT('Ctrl Pts',(42.4449077647045,44.9063602266949,49.9333650423089));
#20560=CARTESIAN_POINT('Ctrl Pts',(42.5805804297497,44.9159247602421,49.9254337762438));
#20561=CARTESIAN_POINT('Ctrl Pts',(42.7593907784112,44.9288673617393,49.895909178815));
#20562=CARTESIAN_POINT('Ctrl Pts',(42.8042264033753,44.9321375976747,49.8868583536638));
#20563=CARTESIAN_POINT('Ctrl Pts',(42.9173064871559,44.9404014453769,49.8598152675831));
#20564=CARTESIAN_POINT('Ctrl Pts',(42.9849703497119,44.9453623117601,49.8396550121707));
#20565=CARTESIAN_POINT('Ctrl Pts',(43.0659262760286,44.9512060781462,49.8106141096855));
#20566=CARTESIAN_POINT('Ctrl Pts',(43.0804062625858,44.95224755208,49.8052225941129));
#20567=CARTESIAN_POINT('Ctrl Pts',(43.1011378809499,44.9537316834185,49.7972184306798));
#20568=CARTESIAN_POINT('Ctrl Pts',(43.1074425310783,44.9541820811108,49.7947460779557));
#20569=CARTESIAN_POINT('Ctrl Pts',(43.1184018790699,44.9549632048007,49.7903816744217));
#20570=CARTESIAN_POINT('Ctrl Pts',(43.1230623923128,44.9552948062442,49.7885045650316));
#20571=CARTESIAN_POINT('Ctrl Pts',(43.132939267181,44.9559962884962,49.7844815494626));
#20572=CARTESIAN_POINT('Ctrl Pts',(43.1381535870893,44.9563658846647,49.7823309607466));
#20573=CARTESIAN_POINT('Ctrl Pts',(43.1523623512064,44.9573711935071,49.7763976625225));
#20574=CARTESIAN_POINT('Ctrl Pts',(43.1613377958191,44.958004229339,49.7725694720773));
#20575=CARTESIAN_POINT('Ctrl Pts',(43.204591086721,44.9610469837814,49.753732007587));
#20576=CARTESIAN_POINT('Ctrl Pts',(43.2384588597062,44.9634054542435,49.7377945640908));
#20577=CARTESIAN_POINT('Ctrl Pts',(43.3037695258554,44.9679469868955,49.704706439237));
#20578=CARTESIAN_POINT('Ctrl Pts',(43.3352402502694,44.9701323076176,49.687646086652));
#20579=CARTESIAN_POINT('Ctrl Pts',(43.4661496168624,44.9792840951103,49.6118925269568));
#20580=CARTESIAN_POINT('Ctrl Pts',(43.5606875930777,44.9860608158762,49.5452113235434));
#20581=CARTESIAN_POINT('Ctrl Pts',(43.7133358743848,44.9981628238264,49.4155855601737));
#20582=CARTESIAN_POINT('Ctrl Pts',(43.7742775071717,45.0033789981259,49.3565000032995));
#20583=CARTESIAN_POINT('Ctrl Pts',(43.8429345203681,45.009893874573,49.280543786691));
#20584=CARTESIAN_POINT('Ctrl Pts',(43.8545587634623,45.0110210802375,49.2673244219021));
#20585=CARTESIAN_POINT('Ctrl Pts',(43.8725951222502,45.0128098567852,49.2462379802009));
#20586=CARTESIAN_POINT('Ctrl Pts',(43.8791290314647,45.0134663816525,49.2384759986026));
#20587=CARTESIAN_POINT('Ctrl Pts',(43.8912592133246,45.0147015357312,49.2238329853458));
#20588=CARTESIAN_POINT('Ctrl Pts',(43.8968698714679,45.015279556801,49.2169641740026));
#20589=CARTESIAN_POINT('Ctrl Pts',(43.909339580745,45.0165795360476,49.2014815140065));
#20590=CARTESIAN_POINT('Ctrl Pts',(43.9161726023265,45.0173025145723,49.192847194696));
#20591=CARTESIAN_POINT('Ctrl Pts',(43.9333973444211,45.0191526479047,49.1706946071235));
#20592=CARTESIAN_POINT('Ctrl Pts',(43.9436842617619,45.0202838823947,49.1570964294876));
#20593=CARTESIAN_POINT('Ctrl Pts',(44.0188823405807,45.0287544838903,49.0549050312242));
#20594=CARTESIAN_POINT('Ctrl Pts',(44.0762912976276,45.0363808800105,48.9610643696934));
#20595=CARTESIAN_POINT('Ctrl Pts',(44.190009037151,45.0544133392815,48.7336725165721));
#20596=CARTESIAN_POINT('Ctrl Pts',(44.2399044534812,45.064895377592,48.5976303356733));
#20597=CARTESIAN_POINT('Ctrl Pts',(44.2791559136267,45.0762321124881,48.4367631672591));
#20598=CARTESIAN_POINT('Ctrl Pts',(44.2838272226617,45.0776645053495,48.416153935323));
#20599=CARTESIAN_POINT('Ctrl Pts',(44.2897297771956,45.0795922974452,48.3879724506852));
#20600=CARTESIAN_POINT('Ctrl Pts',(44.2912557022966,45.0801029279679,48.3804643567441));
#20601=CARTESIAN_POINT('Ctrl Pts',(44.2937386974416,45.0809547573062,48.3678629581893));
#20602=CARTESIAN_POINT('Ctrl Pts',(44.2947200348704,45.0812973032588,48.3627745880688));
#20603=CARTESIAN_POINT('Ctrl Pts',(44.296547800727,45.0819466513567,48.353087607425));
#20604=CARTESIAN_POINT('Ctrl Pts',(44.2973980300129,45.0822536748889,48.3484897930068));
#20605=CARTESIAN_POINT('Ctrl Pts',(44.2993818293171,45.082982183284,48.3375394228986));
#20606=CARTESIAN_POINT('Ctrl Pts',(44.3005002682169,45.0834028197149,48.3311841315293));
#20607=CARTESIAN_POINT('Ctrl Pts',(44.3043565644849,45.0848897192833,48.3086085232795));
#20608=CARTESIAN_POINT('Ctrl Pts',(44.3069189175436,45.0859466357359,48.292358394215));
#20609=CARTESIAN_POINT('Ctrl Pts',(44.3242207553804,45.0936442291906,48.1727035328114));
#20610=CARTESIAN_POINT('Ctrl Pts',(44.3307502617323,45.0999036508947,48.0682727491889));
#20611=CARTESIAN_POINT('Ctrl Pts',(44.3268654816146,45.1122671283403,47.8611978901689));
#20612=CARTESIAN_POINT('Ctrl Pts',(44.3167544488062,45.1183552977951,47.7589035174432));
#20613=CARTESIAN_POINT('Ctrl Pts',(44.2881772097921,45.1282390460147,47.6003073763412));
#20614=CARTESIAN_POINT('Ctrl Pts',(44.2751848995508,45.1318877252281,47.5432200318192));
#20615=CARTESIAN_POINT('Ctrl Pts',(44.2553946794159,45.1366326841936,47.4715065336293));
#20616=CARTESIAN_POINT('Ctrl Pts',(44.2509812895333,45.1376514500592,47.4562509753491));
#20617=CARTESIAN_POINT('Ctrl Pts',(44.2435490814129,45.1393069480025,47.4317000659151));
#20618=CARTESIAN_POINT('Ctrl Pts',(44.240647036601,45.1399398509009,47.422369918148));
#20619=CARTESIAN_POINT('Ctrl Pts',(44.2349547552747,45.1411562109915,47.4045476517151));
#20620=CARTESIAN_POINT('Ctrl Pts',(44.2321761233734,45.1417392723439,47.3960520706386));
#20621=CARTESIAN_POINT('Ctrl Pts',(44.225700997738,45.143074264455,47.37671056611));
#20622=CARTESIAN_POINT('Ctrl Pts',(44.2219667386075,45.1438274296275,47.3658777363236));
#20623=CARTESIAN_POINT('Ctrl Pts',(44.2098735791232,45.1462154013271,47.3317851696141));
#20624=CARTESIAN_POINT('Ctrl Pts',(44.2011643454327,45.1478617745234,47.3086532448387));
#20625=CARTESIAN_POINT('Ctrl Pts',(44.1375653207158,45.1594056495137,47.1490989193369));
#20626=CARTESIAN_POINT('Ctrl Pts',(44.0676873412533,45.1698235696639,47.0191997957208));
#20627=CARTESIAN_POINT('Ctrl Pts',(43.9660478771651,45.1825406483707,46.8730578478913));
#20628=CARTESIAN_POINT('Ctrl Pts',(43.9477267553262,45.184756026245,46.8480249589085));
#20629=CARTESIAN_POINT('Ctrl Pts',(43.8949592907188,45.1909123904709,46.7794592000886));
#20630=CARTESIAN_POINT('Ctrl Pts',(43.8592238160372,45.1948328481501,46.7369521738713));
#20631=CARTESIAN_POINT('Ctrl Pts',(43.8012738187346,45.2007603701703,46.6737693665352));
#20632=CARTESIAN_POINT('Ctrl Pts',(43.780322902934,45.2028245805512,46.6519773964961));
#20633=CARTESIAN_POINT('Ctrl Pts',(43.752668615284,45.2054399702573,46.6245341028403));
#20634=CARTESIAN_POINT('Ctrl Pts',(43.746428216339,45.2060232392672,46.6184248545794));
#20635=CARTESIAN_POINT('Ctrl Pts',(43.7362521307988,45.2069629153701,46.6085970712434));
#20636=CARTESIAN_POINT('Ctrl Pts',(43.7323419845155,45.207321286438,46.6048524431727));
#20637=CARTESIAN_POINT('Ctrl Pts',(43.7247503434539,45.2080117828091,46.5976431838188));
#20638=CARTESIAN_POINT('Ctrl Pts',(43.7210709392342,45.2083440580805,46.59417650947));
#20639=CARTESIAN_POINT('Ctrl Pts',(43.712898802311,45.2090769073386,46.5865372712635));
#20640=CARTESIAN_POINT('Ctrl Pts',(43.7083996761453,45.2094769643848,46.5823715435207));
#20641=CARTESIAN_POINT('Ctrl Pts',(43.6923501818983,45.2108923429771,46.5676528580662));
#20642=CARTESIAN_POINT('Ctrl Pts',(43.6806910166339,45.2118991493485,46.5572186980029));
#20643=CARTESIAN_POINT('Ctrl Pts',(43.5696242051618,45.2213052624814,46.4602288497678));
#20644=CARTESIAN_POINT('Ctrl Pts',(43.4617034051146,45.2290836469037,46.3839207644328));
#20645=CARTESIAN_POINT('Ctrl Pts',(43.2367002990596,45.2444939674408,46.2571711885206));
#20646=CARTESIAN_POINT('Ctrl Pts',(43.1207562332192,45.2520884585251,46.2061147256893));
#20647=CARTESIAN_POINT('Ctrl Pts',(42.9806556589149,45.2614289947194,46.1602106864278));
#20648=CARTESIAN_POINT('Ctrl Pts',(42.9605455471921,45.2627727428097,46.1539841965971));
#20649=CARTESIAN_POINT('Ctrl Pts',(42.9299027869332,45.2648266811414,46.1450434610457));
#20650=CARTESIAN_POINT('Ctrl Pts',(42.9194420228465,45.2655289666295,46.1420870036765));
#20651=CARTESIAN_POINT('Ctrl Pts',(42.9004111326687,45.2668088848935,46.1368817131461));
#20652=CARTESIAN_POINT('Ctrl Pts',(42.8918493814899,45.2673855341446,46.1346031966285));
#20653=CARTESIAN_POINT('Ctrl Pts',(42.8733483998171,45.2686335387352,46.1298158035444));
#20654=CARTESIAN_POINT('Ctrl Pts',(42.8634042985811,45.2693055255943,46.1273270212236));
#20655=CARTESIAN_POINT('Ctrl Pts',(42.836320049723,45.2711392637996,46.1207773842127));
#20656=CARTESIAN_POINT('Ctrl Pts',(42.8191437063512,45.2723059699003,46.1168719258258));
#20657=CARTESIAN_POINT('Ctrl Pts',(42.7263409440724,45.2786316853696,46.0971035178727));
#20658=CARTESIAN_POINT('Ctrl Pts',(42.6498760283478,45.2839265978606,46.0855620508922));
#20659=CARTESIAN_POINT('Ctrl Pts',(42.4437516039078,45.2984055918514,46.0670097080172));
#20660=CARTESIAN_POINT('Ctrl Pts',(42.3137299875012,45.3077734802555,46.068441327191));
#20661=CARTESIAN_POINT('Ctrl Pts',(42.1210276436757,45.3214899659038,46.0900676012835));
#20662=CARTESIAN_POINT('Ctrl Pts',(42.05759392552,45.3259712159887,46.1004139302229));
#20663=CARTESIAN_POINT('Ctrl Pts',(41.984198889962,45.3310326835872,46.1161822519496));
#20664=CARTESIAN_POINT('Ctrl Pts',(41.9736284047895,45.3317585785719,46.118546533356));
#20665=CARTESIAN_POINT('Ctrl Pts',(41.9573578297607,45.3328705877415,46.1223299127065));
#20666=CARTESIAN_POINT('Ctrl Pts',(41.9516435718611,45.3332601110679,46.123686176777));
#20667=CARTESIAN_POINT('Ctrl Pts',(41.941092378712,45.3339773593169,46.126241428692));
#20668=CARTESIAN_POINT('Ctrl Pts',(41.9362539046264,45.3343054786297,46.1274330590362));
#20669=CARTESIAN_POINT('Ctrl Pts',(41.9252154842975,45.3350522851958,46.1301970346632));
#20670=CARTESIAN_POINT('Ctrl Pts',(41.9190187001121,45.3354702725699,46.1317814748847));
#20671=CARTESIAN_POINT('Ctrl Pts',(41.9027879344318,45.3365620512477,46.1360175894782));
#20672=CARTESIAN_POINT('Ctrl Pts',(41.8927671132211,45.3372330724177,46.1387195066591));
#20673=CARTESIAN_POINT('Ctrl Pts',(41.8124288367972,45.3425919004022,46.1610781569515));
#20674=CARTESIAN_POINT('Ctrl Pts',(41.7432485468824,45.3470787376706,46.1846340526797));
#20675=CARTESIAN_POINT('Ctrl Pts',(41.5707376055398,45.3583252030467,46.2545319286104));
#20676=CARTESIAN_POINT('Ctrl Pts',(41.469850011165,45.3649689275563,46.3061414331288));
#20677=CARTESIAN_POINT('Ctrl Pts',(41.3026373631626,45.3769035993675,46.4111477645204));
#20678=CARTESIAN_POINT('Ctrl Pts',(41.234237734677,45.3820928212337,46.4606326341144));
#20679=CARTESIAN_POINT('Ctrl Pts',(41.15576186563,45.3885773448957,46.525644855577));
#20680=CARTESIAN_POINT('Ctrl Pts',(41.14237800653,45.3897031330683,46.5370445954906));
#20681=CARTESIAN_POINT('Ctrl Pts',(41.1215225280144,45.3914901699157,46.5553060003055));
#20682=CARTESIAN_POINT('Ctrl Pts',(41.1139458138287,45.392146389433,46.5620465853046));
#20683=CARTESIAN_POINT('Ctrl Pts',(41.0998426445514,45.3933812784833,46.5747940224455));
#20684=CARTESIAN_POINT('Ctrl Pts',(41.0933037633589,45.3939593425192,46.5807867784933));
#20685=CARTESIAN_POINT('Ctrl Pts',(41.0787353997711,45.3952598270551,46.5943244301228));
#20686=CARTESIAN_POINT('Ctrl Pts',(41.070728815373,45.3959832713719,46.6018934015217));
#20687=CARTESIAN_POINT('Ctrl Pts',(41.0504815651611,45.3978353961448,46.6213651492942));
#20688=CARTESIAN_POINT('Ctrl Pts',(41.0383334891037,45.3989681713086,46.6333623967398));
#20689=CARTESIAN_POINT('Ctrl Pts',(40.9478693913633,45.4075703633746,46.7251069955365));
#20690=CARTESIAN_POINT('Ctrl Pts',(40.8764711158507,45.415337690854,46.8113505889491));
#20691=CARTESIAN_POINT('Ctrl Pts',(40.7318838554259,45.4333869109945,47.0205801787319));
#20692=CARTESIAN_POINT('Ctrl Pts',(40.6640738924162,45.4437280551725,47.1465141219001));
#20693=CARTESIAN_POINT('Ctrl Pts',(40.6028994213088,45.4549293865162,47.2982776550209));
#20694=CARTESIAN_POINT('Ctrl Pts',(40.5953568393628,45.4563547774798,47.3179091763951));
#20695=CARTESIAN_POINT('Ctrl Pts',(40.5855108314491,45.458274765749,47.3448434580625));
#20696=CARTESIAN_POINT('Ctrl Pts',(40.5829279363366,45.4587844399407,47.3520415464154));
#20697=CARTESIAN_POINT('Ctrl Pts',(40.5786676517651,45.4596351228711,47.3641400644745));
#20698=CARTESIAN_POINT('Ctrl Pts',(40.57696709049,45.4599774710929,47.3690321772976));
#20699=CARTESIAN_POINT('Ctrl Pts',(40.5737679546114,45.4606267876403,47.3783562437979));
#20700=CARTESIAN_POINT('Ctrl Pts',(40.5722657729137,45.4609339750591,47.3827868767312));
#20701=CARTESIAN_POINT('Ctrl Pts',(40.5687267477025,45.4616633089054,47.3933513343301));
#20702=CARTESIAN_POINT('Ctrl Pts',(40.5667045658399,45.4620846023614,47.3994900648957));
#20703=CARTESIAN_POINT('Ctrl Pts',(40.5596265980289,45.463576027856,47.4213456367223));
#20704=CARTESIAN_POINT('Ctrl Pts',(40.5547415929671,45.4646367393974,47.4371176091156));
#20705=CARTESIAN_POINT('Ctrl Pts',(40.5221195590718,45.4719605146159,47.5474346375059));
#20706=CARTESIAN_POINT('Ctrl Pts',(40.5014554624994,45.47788559347,47.6439326661028));
#20707=CARTESIAN_POINT('Ctrl Pts',(40.476742447857,45.4889088324802,47.8267677989799));
#20708=CARTESIAN_POINT('Ctrl Pts',(40.4709350396174,45.4940039414054,47.9126108422634));
#20709=CARTESIAN_POINT('Ctrl Pts',(40.4708124784275,45.5039038220345,48.075923570566));
#20710=CARTESIAN_POINT('Ctrl Pts',(40.4754090259402,45.5086773032843,48.1532199463386));
#20711=CARTESIAN_POINT('Ctrl Pts',(40.4867339793363,45.514718890139,48.2475200081008));
#20712=CARTESIAN_POINT('Ctrl Pts',(40.4890744726845,45.5158468482015,48.2649841811214));
#20713=CARTESIAN_POINT('Ctrl Pts',(40.4931546312366,45.5176430285859,48.2925549525971));
#20714=CARTESIAN_POINT('Ctrl Pts',(40.4947362608742,45.5183062448043,48.3026842220854));
#20715=CARTESIAN_POINT('Ctrl Pts',(40.4978350721116,45.5195474011195,48.3215425885675));
#20716=CARTESIAN_POINT('Ctrl Pts',(40.4993318027835,45.5201246761939,48.3302748080384));
#20717=CARTESIAN_POINT('Ctrl Pts',(40.5027985178214,45.521414444566,48.3496958998813));
#20718=CARTESIAN_POINT('Ctrl Pts',(40.5047987807237,45.5221278867066,48.3603789902236));
#20719=CARTESIAN_POINT('Ctrl Pts',(40.5109365138345,45.5242311736102,48.3916944021243));
#20720=CARTESIAN_POINT('Ctrl Pts',(40.515321310221,45.5256288560924,48.4122760432403));
#20721=CARTESIAN_POINT('Ctrl Pts',(40.5480012623231,45.5353790668902,48.55423449777));
#20722=CARTESIAN_POINT('Ctrl Pts',(40.5876591792554,45.5441016591821,48.6726704756848));
#20723=CARTESIAN_POINT('Ctrl Pts',(40.693027897489,45.5625175856761,48.9086875280277));
#20724=CARTESIAN_POINT('Ctrl Pts',(40.7601877728224,45.5721842801089,49.0249330887395));
#20725=CARTESIAN_POINT('Ctrl Pts',(40.847931341814,45.5823327182408,49.1458029629038));
#20726=CARTESIAN_POINT('Ctrl Pts',(40.8571635717543,45.583374836433,49.1582043612549));
#20727=CARTESIAN_POINT('Ctrl Pts',(40.8702465856935,45.5848148615061,49.1753443249718));
#20728=CARTESIAN_POINT('Ctrl Pts',(40.8739719874032,45.5852208686908,49.1801772316496));
#20729=CARTESIAN_POINT('Ctrl Pts',(40.8808210891446,45.5859598430739,49.1889758094864));
#20730=CARTESIAN_POINT('Ctrl Pts',(40.8839375426987,45.5862933085585,49.1929470510635));
#20731=CARTESIAN_POINT('Ctrl Pts',(40.8904371595074,45.5869829664163,49.201162789556));
#20732=CARTESIAN_POINT('Ctrl Pts',(40.8938226897472,45.5873389861354,49.2054052962811));
#20733=CARTESIAN_POINT('Ctrl Pts',(40.9027409297488,45.5882686227461,49.2164847660254));
#20734=CARTESIAN_POINT('Ctrl Pts',(40.9083026444419,45.5888402038468,49.2232983757347));
#20735=CARTESIAN_POINT('Ctrl Pts',(40.9335853435197,45.5914032329968,49.2538431622364));
#20736=CARTESIAN_POINT('Ctrl Pts',(40.9538285760658,45.5933598586195,49.2771386338879));
#20737=CARTESIAN_POINT('Ctrl Pts',(41.0132396447128,45.5988706950909,49.3422825298116));
#20738=CARTESIAN_POINT('Ctrl Pts',(41.0537265186962,45.6023544840896,49.3828866008304));
#20739=CARTESIAN_POINT('Ctrl Pts',(41.1903645942287,45.613506546293,49.5082222576587));
#20740=CARTESIAN_POINT('Ctrl Pts',(41.2931519328122,45.6210213861649,49.585193767332));
#20741=CARTESIAN_POINT('Ctrl Pts',(41.4548054575174,45.6325787446976,49.68280693578));
#20742=CARTESIAN_POINT('Ctrl Pts',(41.5082504530253,45.6363581631205,49.7117282288967));
#20743=CARTESIAN_POINT('Ctrl Pts',(41.578001678198,45.6412903976384,49.7453193950468));
#20744=CARTESIAN_POINT('Ctrl Pts',(41.5931295142146,45.642359986001,49.7523644092311));
#20745=CARTESIAN_POINT('Ctrl Pts',(41.6174174375653,45.6440779445414,49.7632940863347));
#20746=CARTESIAN_POINT('Ctrl Pts',(41.6265196983154,45.6447219326147,49.7673057796177));
#20747=CARTESIAN_POINT('Ctrl Pts',(41.6438219097779,45.6459465636218,49.7747722167485));
#20748=CARTESIAN_POINT('Ctrl Pts',(41.6520155563738,45.6465267082801,49.7782409828505));
#20749=CARTESIAN_POINT('Ctrl Pts',(41.6706870478752,45.6478493449199,49.7859936473494));
#20750=CARTESIAN_POINT('Ctrl Pts',(41.6811791120757,45.6485930122819,49.7902422216799));
#20751=CARTESIAN_POINT('Ctrl Pts',(41.7134026637587,45.6508786629668,49.8029616348139));
#20752=CARTESIAN_POINT('Ctrl Pts',(41.7352502195506,45.6524306791987,49.811130643188));
#20753=CARTESIAN_POINT('Ctrl Pts',(41.7694986777515,45.6548682623836,49.823233306061));
#20754=CARTESIAN_POINT('Ctrl Pts',(41.7817990312338,45.6557446311092,49.8274405743698));
#20755=CARTESIAN_POINT('Ctrl Pts',(41.7941388553004,45.6566247686891,49.8315225442902));
#20756=CARTESIAN_POINT('Ctrl Pts',(41.7941388200938,45.8276962776015,49.831522532644));
#20757=CARTESIAN_POINT('Ctrl Pts',(41.7489977681372,45.8247306088719,49.8165900322171));
#20758=CARTESIAN_POINT('Ctrl Pts',(41.7044115598008,45.8218301431025,49.7999895810198));
#20759=CARTESIAN_POINT('Ctrl Pts',(41.5580371350285,45.8122670972022,49.7392359799271));
#20760=CARTESIAN_POINT('Ctrl Pts',(41.4594588335036,45.805747466061,49.6879651314237));
#20761=CARTESIAN_POINT('Ctrl Pts',(41.2950929966855,45.7939753970559,49.5835860715604));
#20762=CARTESIAN_POINT('Ctrl Pts',(41.2273653028119,45.7888183151641,49.5341087327945));
#20763=CARTESIAN_POINT('Ctrl Pts',(41.1496054568406,45.7823701883531,49.4691371783181));
#20764=CARTESIAN_POINT('Ctrl Pts',(41.1362923021391,45.7812463033521,49.457701404249));
#20765=CARTESIAN_POINT('Ctrl Pts',(41.1155416898174,45.77946171098,49.4393790612813));
#20766=CARTESIAN_POINT('Ctrl Pts',(41.1079990952252,45.7788060107802,49.4326126092577));
#20767=CARTESIAN_POINT('Ctrl Pts',(41.0939561691918,45.7775717500974,49.4198136174763));
#20768=CARTESIAN_POINT('Ctrl Pts',(41.0874434241676,45.776993791775,49.4137950442593));
#20769=CARTESIAN_POINT('Ctrl Pts',(41.0729289061825,45.7756930858404,49.4001951188175));
#20770=CARTESIAN_POINT('Ctrl Pts',(41.0649502044251,45.7749693110674,49.3925897075417));
#20771=CARTESIAN_POINT('Ctrl Pts',(41.0447652354103,45.7731154485877,49.3730162083826));
#20772=CARTESIAN_POINT('Ctrl Pts',(41.0326522821825,45.7719812515221,49.3609536957905));
#20773=CARTESIAN_POINT('Ctrl Pts',(40.9416560245141,45.7632913007043,49.2678951898616));
#20774=CARTESIAN_POINT('Ctrl Pts',(40.8698837376074,45.7554303064388,49.1802802796323));
#20775=CARTESIAN_POINT('Ctrl Pts',(40.7265461758084,45.7373683076527,48.9700948195896));
#20776=CARTESIAN_POINT('Ctrl Pts',(40.6599691194015,45.7271186641324,48.8448829963908));
#20777=CARTESIAN_POINT('Ctrl Pts',(40.5999204901637,45.7160055748317,48.6940429483817));
#20778=CARTESIAN_POINT('Ctrl Pts',(40.5924858079949,45.714584924637,48.6744437636442));
#20779=CARTESIAN_POINT('Ctrl Pts',(40.5827800386299,45.712670323389,48.6475434192508));
#20780=CARTESIAN_POINT('Ctrl Pts',(40.58023102428,45.7121613976206,48.640345022382));
#20781=CARTESIAN_POINT('Ctrl Pts',(40.5760261330969,45.7113116896684,48.6282425307444));
#20782=CARTESIAN_POINT('Ctrl Pts',(40.574347147764,45.710969573438,48.6233466209235));
#20783=CARTESIAN_POINT('Ctrl Pts',(40.5711881457038,45.710320503492,48.6140127384059));
#20784=CARTESIAN_POINT('Ctrl Pts',(40.5697045414466,45.7100133321267,48.6095760632656));
#20785=CARTESIAN_POINT('Ctrl Pts',(40.5662086038631,45.7092837849661,48.5989937308895));
#20786=CARTESIAN_POINT('Ctrl Pts',(40.564210987921,45.7088622642186,48.5928432172652));
#20787=CARTESIAN_POINT('Ctrl Pts',(40.5572145463655,45.7073687434576,48.5709271951168));
#20788=CARTESIAN_POINT('Ctrl Pts',(40.5523874076705,45.7063062012436,48.5551070554506));
#20789=CARTESIAN_POINT('Ctrl Pts',(40.5203611666367,45.699012211015,48.4450972738243));
#20790=CARTESIAN_POINT('Ctrl Pts',(40.5001697562934,45.6931151635944,48.3490038090651));
#20791=CARTESIAN_POINT('Ctrl Pts',(40.4764463287328,45.6822542611877,48.1687912774779));
#20792=CARTESIAN_POINT('Ctrl Pts',(40.47093461263,45.6772914720765,48.085179266282));
#20793=CARTESIAN_POINT('Ctrl Pts',(40.4708094838832,45.6673906846146,47.9216505663629));
#20794=CARTESIAN_POINT('Ctrl Pts',(40.475702984479,45.6624718590081,47.8419070117054));
#20795=CARTESIAN_POINT('Ctrl Pts',(40.4877035742627,45.656267122446,47.7450883727929));
#20796=CARTESIAN_POINT('Ctrl Pts',(40.4901296537454,45.6551311012319,47.7275063591347));
#20797=CARTESIAN_POINT('Ctrl Pts',(40.4943432878256,45.6533250808875,47.699798893423));
#20798=CARTESIAN_POINT('Ctrl Pts',(40.4959698308078,45.6526601847964,47.6896496865439));
#20799=CARTESIAN_POINT('Ctrl Pts',(40.4991483174403,45.6514177228355,47.6707829985948));
#20800=CARTESIAN_POINT('Ctrl Pts',(40.5006793288481,45.6508408377371,47.6620622293506));
#20801=CARTESIAN_POINT('Ctrl Pts',(40.5042156487209,45.6495542969478,47.6427025689079));
#20802=CARTESIAN_POINT('Ctrl Pts',(40.5062505783723,45.6488437124804,47.6320694620345));
#20803=CARTESIAN_POINT('Ctrl Pts',(40.5124652258416,45.6467564699514,47.6010143447037));
#20804=CARTESIAN_POINT('Ctrl Pts',(40.5168864683117,45.6453721507834,47.5806428188978));
#20805=CARTESIAN_POINT('Ctrl Pts',(40.5276790478715,45.6422031985392,47.5345327916235));
#20806=CARTESIAN_POINT('Ctrl Pts',(40.5342525579553,45.6404124040772,47.5088464234966));
#20807=CARTESIAN_POINT('Ctrl Pts',(40.558027952774,45.6343629303525,47.4233220039839));
#20808=CARTESIAN_POINT('Ctrl Pts',(40.5775952014722,45.6300346199068,47.3641871325198));
#20809=CARTESIAN_POINT('Ctrl Pts',(40.6495160875748,45.6159416073177,47.1776187010271));
#20810=CARTESIAN_POINT('Ctrl Pts',(40.7126590167087,45.6059566083774,47.0548102430191));
#20811=CARTESIAN_POINT('Ctrl Pts',(40.81081958499,45.5934885436024,46.9055952513964));
#20812=CARTESIAN_POINT('Ctrl Pts',(40.8343864089518,45.5906716136456,46.8721388424947));
#20813=CARTESIAN_POINT('Ctrl Pts',(40.8649789972531,45.5872481534987,46.8315173034448));
#20814=CARTESIAN_POINT('Ctrl Pts',(40.8710180937537,45.5865829558754,46.8236260663398));
#20815=CARTESIAN_POINT('Ctrl Pts',(40.8806392180626,45.5855402262731,46.8112534862332));
#20816=CARTESIAN_POINT('Ctrl Pts',(40.8841806207593,45.5851599724916,46.8067409873243));
#20817=CARTESIAN_POINT('Ctrl Pts',(40.8905355334103,45.5844840406398,46.7987174259746));
#20818=CARTESIAN_POINT('Ctrl Pts',(40.8933411902295,45.5841878306637,46.7952004191194));
#20819=CARTESIAN_POINT('Ctrl Pts',(40.9001131840279,45.5834781154442,46.7867720961225));
#20820=CARTESIAN_POINT('Ctrl Pts',(40.9040913511106,45.5830654649129,46.781870399162));
#20821=CARTESIAN_POINT('Ctrl Pts',(40.9163258306319,45.5818090525843,46.766946014074));
#20822=CARTESIAN_POINT('Ctrl Pts',(40.9246595387772,45.5809706381401,46.7569868388791));
#20823=CARTESIAN_POINT('Ctrl Pts',(40.944323590172,45.579030372814,46.7339637661276));
#20824=CARTESIAN_POINT('Ctrl Pts',(40.9557304350497,45.5779334347124,46.7209663708862));
#20825=CARTESIAN_POINT('Ctrl Pts',(40.9964310881122,45.5741110696445,46.6758294039647));
#20826=CARTESIAN_POINT('Ctrl Pts',(41.0266368444325,45.5714365422141,46.6445267970164));
#20827=CARTESIAN_POINT('Ctrl Pts',(41.1511360491969,45.5609083055487,46.5239453851308));
#20828=CARTESIAN_POINT('Ctrl Pts',(41.2532761570946,45.5533199073216,46.4432646421649));
#20829=CARTESIAN_POINT('Ctrl Pts',(41.4277418456405,45.5407746083559,46.332007670501));
#20830=CARTESIAN_POINT('Ctrl Pts',(41.495152913795,45.5360182048485,46.2944989036598));
#20831=CARTESIAN_POINT('Ctrl Pts',(41.5804869479239,45.5299959864769,46.2535033004219));
#20832=CARTESIAN_POINT('Ctrl Pts',(41.5964555366025,45.5288691984128,46.2460990260106));
#20833=CARTESIAN_POINT('Ctrl Pts',(41.6218765272562,45.5270745653844,46.2347319171563));
#20834=CARTESIAN_POINT('Ctrl Pts',(41.63126328474,45.5264117132499,46.2306240085761));
#20835=CARTESIAN_POINT('Ctrl Pts',(41.6488248249132,45.5251710452032,46.223104710125));
#20836=CARTESIAN_POINT('Ctrl Pts',(41.6569912749836,45.5245938922403,46.2196744553361));
#20837=CARTESIAN_POINT('Ctrl Pts',(41.675231641057,45.5233041496136,46.2121600901749));
#20838=CARTESIAN_POINT('Ctrl Pts',(41.6853169737672,45.5225906095605,46.2081046679377));
#20839=CARTESIAN_POINT('Ctrl Pts',(41.715038898919,45.5204862375377,46.196443992078));
#20840=CARTESIAN_POINT('Ctrl Pts',(41.7347658445182,45.5190875539711,46.1890749761293));
#20841=CARTESIAN_POINT('Ctrl Pts',(41.8757045399072,45.5090771493632,46.1390408054126));
#20842=CARTESIAN_POINT('Ctrl Pts',(42.000770137031,45.5000700780431,46.1082655919083));
#20843=CARTESIAN_POINT('Ctrl Pts',(42.2561085335451,45.4816810415333,46.0718927286004));
#20844=CARTESIAN_POINT('Ctrl Pts',(42.3857958121912,45.4723477900513,46.0665818330857));
#20845=CARTESIAN_POINT('Ctrl Pts',(42.5304771985306,45.4624946242331,46.0752254011924));
#20846=CARTESIAN_POINT('Ctrl Pts',(42.5458982312289,45.4614519024199,46.0763328513661));
#20847=CARTESIAN_POINT('Ctrl Pts',(42.5675668540677,45.4599988110093,46.0781510478549));
#20848=CARTESIAN_POINT('Ctrl Pts',(42.573826343241,45.4595804713035,46.0787070888152));
#20849=CARTESIAN_POINT('Ctrl Pts',(42.5851541006439,45.4588261112817,46.0797691657242));
#20850=CARTESIAN_POINT('Ctrl Pts',(42.5902232876689,45.4584895171886,46.0802647055171));
#20851=CARTESIAN_POINT('Ctrl Pts',(42.6006092098813,45.4578019859752,46.0813215270133));
#20852=CARTESIAN_POINT('Ctrl Pts',(42.6059256638783,45.4574511642822,46.081884841704));
#20853=CARTESIAN_POINT('Ctrl Pts',(42.619618840437,45.4565503054413,46.0833933156804));
#20854=CARTESIAN_POINT('Ctrl Pts',(42.6279919413212,45.4560020790462,46.0843713046243));
#20855=CARTESIAN_POINT('Ctrl Pts',(42.6634995861571,45.453687369906,46.0887547548131));
#20856=CARTESIAN_POINT('Ctrl Pts',(42.6905679904396,45.4519479713485,46.0926822902659));
#20857=CARTESIAN_POINT('Ctrl Pts',(42.7646240909343,45.4472358358481,46.1050409072191));
#20858=CARTESIAN_POINT('Ctrl Pts',(42.8113984083784,45.444311379968,46.1146425615657));
#20859=CARTESIAN_POINT('Ctrl Pts',(43.0035449543937,45.4323386791839,46.1615784116989));
#20860=CARTESIAN_POINT('Ctrl Pts',(43.144662755547,45.4236015350582,46.2140718997319));
#20861=CARTESIAN_POINT('Ctrl Pts',(43.3262628813893,45.4110603700198,46.3069303546737));
#20862=CARTESIAN_POINT('Ctrl Pts',(43.3731994891942,45.4076941509458,46.3334677644867));
#20863=CARTESIAN_POINT('Ctrl Pts',(43.4325736486908,45.4032352545222,46.3704015101339));
#20864=CARTESIAN_POINT('Ctrl Pts',(43.4460802380752,45.4022069742332,46.3790386529662));
#20865=CARTESIAN_POINT('Ctrl Pts',(43.4676688787885,45.4005399064253,46.3932262745587));
#20866=CARTESIAN_POINT('Ctrl Pts',(43.4758191912984,45.3999050501457,46.398671894573));
#20867=CARTESIAN_POINT('Ctrl Pts',(43.4913117944252,45.3986875439046,46.4091949182841));
#20868=CARTESIAN_POINT('Ctrl Pts',(43.4986610548828,45.3981053098013,46.4142616474892));
#20869=CARTESIAN_POINT('Ctrl Pts',(43.515462585929,45.3967632773241,46.4260178314029));
#20870=CARTESIAN_POINT('Ctrl Pts',(43.5248902415259,45.3960021714471,46.4327416989466));
#20871=CARTESIAN_POINT('Ctrl Pts',(43.5542449384474,45.3936065263311,46.4540789782047));
#20872=CARTESIAN_POINT('Ctrl Pts',(43.5739514148156,45.3919604951448,46.4689901494618));
#20873=CARTESIAN_POINT('Ctrl Pts',(43.6725807221521,45.3835238981142,46.5466432882947));
#20874=CARTESIAN_POINT('Ctrl Pts',(43.7467729208159,45.37650581243,46.6151156927379));
#20875=CARTESIAN_POINT('Ctrl Pts',(43.8881086712195,45.3617527021093,46.7676992699086));
#20876=CARTESIAN_POINT('Ctrl Pts',(43.9542684869372,45.3540253734483,46.8522709551391));
#20877=CARTESIAN_POINT('Ctrl Pts',(44.0415902873666,45.3428296613133,46.9853920178565));
#20878=CARTESIAN_POINT('Ctrl Pts',(44.0683515555887,45.3392233670434,47.030024653293));
#20879=CARTESIAN_POINT('Ctrl Pts',(44.0983698816432,45.3349998218833,47.085016266002));
#20880=CARTESIAN_POINT('Ctrl Pts',(44.1033845808426,45.3342876447707,47.0943861359691));
#20881=CARTESIAN_POINT('Ctrl Pts',(44.1110594187255,45.3331877933222,47.109015740703));
#20882=CARTESIAN_POINT('Ctrl Pts',(44.1137732235806,45.3327969021908,47.1142468599179));
#20883=CARTESIAN_POINT('Ctrl Pts',(44.1187358001713,45.332078519209,47.123920893659));
#20884=CARTESIAN_POINT('Ctrl Pts',(44.120991339839,45.3317506208461,47.1283600740341));
#20885=CARTESIAN_POINT('Ctrl Pts',(44.1260907057081,45.3310060767611,47.1384932164202));
#20886=CARTESIAN_POINT('Ctrl Pts',(44.1289235608454,45.3305901150827,47.1441925531458));
#20887=CARTESIAN_POINT('Ctrl Pts',(44.1375674299662,45.3293132745692,47.1618009944639));
#20888=CARTESIAN_POINT('Ctrl Pts',(44.1432841331289,45.3284579993905,47.1737563305823));
#20889=CARTESIAN_POINT('Ctrl Pts',(44.1563689329494,45.3264723093262,47.2018610565474));
#20890=CARTESIAN_POINT('Ctrl Pts',(44.1636383415871,45.3253471308104,47.2180553407334));
#20891=CARTESIAN_POINT('Ctrl Pts',(44.1886366498586,45.3213893528808,47.275867645118));
#20892=CARTESIAN_POINT('Ctrl Pts',(44.2051251860031,45.3186116335538,47.3180085415979));
#20893=CARTESIAN_POINT('Ctrl Pts',(44.2645540311461,45.307734891404,47.4872034281112));
#20894=CARTESIAN_POINT('Ctrl Pts',(44.295679724053,45.2999042048776,47.618002197373));
#20895=CARTESIAN_POINT('Ctrl Pts',(44.322143666168,45.287433565727,47.821295973615));
#20896=CARTESIAN_POINT('Ctrl Pts',(44.3274124934296,45.2830440644208,47.8920611610014));
#20897=CARTESIAN_POINT('Ctrl Pts',(44.3291048587296,45.2774356689934,47.9801647132384));
#20898=CARTESIAN_POINT('Ctrl Pts',(44.3292050461932,45.2763330349727,47.9973820917729));
#20899=CARTESIAN_POINT('Ctrl Pts',(44.3289978932785,45.2745683623532,48.0247564996777));
#20900=CARTESIAN_POINT('Ctrl Pts',(44.3288407820625,45.2739110362639,48.0349140006813));
#20901=CARTESIAN_POINT('Ctrl Pts',(44.3283963518383,45.2726753780757,48.0539319003905));
#20902=CARTESIAN_POINT('Ctrl Pts',(44.3281281688722,45.2720976623275,48.0627925126045));
#20903=CARTESIAN_POINT('Ctrl Pts',(44.3273909172916,45.2707996919707,48.0826286071421));
#20904=CARTESIAN_POINT('Ctrl Pts',(44.3268891508784,45.2700784287953,48.0936024919549));
#20905=CARTESIAN_POINT('Ctrl Pts',(44.3251211584243,45.2679281089409,48.1261704397063));
#20906=CARTESIAN_POINT('Ctrl Pts',(44.32358546829,45.2664906714876,48.1477475401696));
#20907=CARTESIAN_POINT('Ctrl Pts',(44.309487861616,45.2557309063079,48.3077725119865));
#20908=CARTESIAN_POINT('Ctrl Pts',(44.282358252401,45.2459408543432,48.4445011344404));
#20909=CARTESIAN_POINT('Ctrl Pts',(44.2057510946412,45.2276560812585,48.6888554031354));
#20910=CARTESIAN_POINT('Ctrl Pts',(44.1606086885483,45.2192499903552,48.797195512021));
#20911=CARTESIAN_POINT('Ctrl Pts',(44.0984035199583,45.2101851302243,48.9150009324215));
#20912=CARTESIAN_POINT('Ctrl Pts',(44.0907158883632,45.2090996016342,48.9291291886891));
#20913=CARTESIAN_POINT('Ctrl Pts',(44.0797278534584,45.2075971985535,48.9487348063231));
#20914=CARTESIAN_POINT('Ctrl Pts',(44.076575811688,45.2071716466355,48.954293951014));
#20915=CARTESIAN_POINT('Ctrl Pts',(44.0710780736071,45.2064388474913,48.9638787968176));
#20916=CARTESIAN_POINT('Ctrl Pts',(44.0687453346064,45.2061307912994,48.9679118102561));
#20917=CARTESIAN_POINT('Ctrl Pts',(44.0637790958118,45.2054810748599,48.9764264933086));
#20918=CARTESIAN_POINT('Ctrl Pts',(44.0611420482365,45.205139656731,48.9809060471412));
#20919=CARTESIAN_POINT('Ctrl Pts',(44.0545314160587,45.2042924862137,48.9920324178202));
#20920=CARTESIAN_POINT('Ctrl Pts',(44.0505358027342,45.203788145542,48.9986661572501));
#20921=CARTESIAN_POINT('Ctrl Pts',(44.0351714953321,45.2018771466587,49.0238307303909));
#20922=CARTESIAN_POINT('Ctrl Pts',(44.0235292984774,45.2004871776679,49.0421937905191));
#20923=CARTESIAN_POINT('Ctrl Pts',(43.9926964132392,45.1969411641667,49.0890550040385));
#20924=CARTESIAN_POINT('Ctrl Pts',(43.9730499196481,45.1948090219009,49.1172452265651));
#20925=CARTESIAN_POINT('Ctrl Pts',(43.9082961687356,45.1881195133178,49.2050614472613));
#20926=CARTESIAN_POINT('Ctrl Pts',(43.860470482017,45.183662345675,49.2625995486546));
#20927=CARTESIAN_POINT('Ctrl Pts',(43.717904714341,45.1712090064643,49.4151448160633));
#20928=CARTESIAN_POINT('Ctrl Pts',(43.6164413348958,45.1632180832521,49.5032540561617));
#20929=CARTESIAN_POINT('Ctrl Pts',(43.4859211967136,45.1531706934503,49.5946659543404));
#20930=CARTESIAN_POINT('Ctrl Pts',(43.4648871807527,45.1515591450046,49.6087882235412));
#20931=CARTESIAN_POINT('Ctrl Pts',(43.4338520340445,45.1491890314014,49.6287499393738));
#20932=CARTESIAN_POINT('Ctrl Pts',(43.4240662209804,45.1484427960548,49.6349204135836));
#20933=CARTESIAN_POINT('Ctrl Pts',(43.4066104754436,45.1471132972055,49.6457089812219));
#20934=CARTESIAN_POINT('Ctrl Pts',(43.3989627180196,45.1465313585298,49.6503624400774));
#20935=CARTESIAN_POINT('Ctrl Pts',(43.3829497462801,45.1453138735764,49.6599538275377));
#20936=CARTESIAN_POINT('Ctrl Pts',(43.3745790892171,45.1446779968262,49.6648821298427));
#20937=CARTESIAN_POINT('Ctrl Pts',(43.3526465185876,45.1430131288837,49.6775730524158));
#20938=CARTESIAN_POINT('Ctrl Pts',(43.3390271023177,45.1419805192434,49.6852343493212));
#20939=CARTESIAN_POINT('Ctrl Pts',(43.2764859092685,45.1372431103501,49.7194219773386));
#20940=CARTESIAN_POINT('Ctrl Pts',(43.2265279131259,45.1334699055616,49.7439868200236));
#20941=CARTESIAN_POINT('Ctrl Pts',(43.0774150120444,45.1222336249694,49.8094601941863));
#20942=CARTESIAN_POINT('Ctrl Pts',(42.9758352934972,45.1145999424436,49.8443010347653));
#20943=CARTESIAN_POINT('Ctrl Pts',(42.7718302572124,45.0995693186419,49.8957679647394));
#20944=CARTESIAN_POINT('Ctrl Pts',(42.6698857023353,45.0922009072282,49.9129453151854));
#20945=CARTESIAN_POINT('Ctrl Pts',(42.5506247950813,45.0840505529895,49.9233113329774));
#20946=CARTESIAN_POINT('Ctrl Pts',(42.5341834004405,45.0829374128404,49.9245282985785));
#20947=CARTESIAN_POINT('Ctrl Pts',(42.5112819606707,45.0814032999862,49.9259284996786));
#20948=CARTESIAN_POINT('Ctrl Pts',(42.5048341004224,45.0809731796702,49.9262902364359));
#20949=CARTESIAN_POINT('Ctrl Pts',(42.4937144086169,45.0802346665316,49.9268580727464));
#20950=CARTESIAN_POINT('Ctrl Pts',(42.4890434708682,45.0799254357074,49.9270795739557));
#20951=CARTESIAN_POINT('Ctrl Pts',(42.4791981290499,45.079275792214,49.9275105785724));
#20952=CARTESIAN_POINT('Ctrl Pts',(42.4740236063068,45.0789356074953,49.9277162345491));
#20953=CARTESIAN_POINT('Ctrl Pts',(42.4612038369691,45.0780957795509,49.9281740479059));
#20954=CARTESIAN_POINT('Ctrl Pts',(42.4535576966618,45.0775974950056,49.9284015781585));
#20955=CARTESIAN_POINT('Ctrl Pts',(42.4248635830673,45.075736691758,49.9290846462127));
#20956=CARTESIAN_POINT('Ctrl Pts',(42.4038090765643,45.0743897555934,49.9292411329202));
#20957=CARTESIAN_POINT('Ctrl Pts',(42.2397012633488,45.064005512162,49.9277740885052));
#20958=CARTESIAN_POINT('Ctrl Pts',(42.0972143712163,45.0556417455269,49.9105864390193));
#20959=CARTESIAN_POINT('Ctrl Pts',(41.9026455049927,45.0436772849884,49.8647804534868));
#20960=CARTESIAN_POINT('Ctrl Pts',(41.8479982187459,45.0402578482943,49.8493390370101));
#20961=CARTESIAN_POINT('Ctrl Pts',(41.7941386463292,45.0367815693785,49.8315224751633));
#20962=CARTESIAN_POINT('Origin',(42.4,48.4493818343519,48.));
#20963=CARTESIAN_POINT('',(41.7941388317924,44.0726550104672,49.8315225365138));
#20964=CARTESIAN_POINT('',(41.7941385063105,44.2430936274184,49.8315224288456));
#20965=CARTESIAN_POINT('',(41.7941388317924,48.4493818343519,49.8315225365138));
#20966=CARTESIAN_POINT('',(40.4708695925604,44.7082214075913,47.9993794804437));
#20967=CARTESIAN_POINT('Ctrl Pts',(41.7941388317924,44.0726550104672,49.8315225365139));
#20968=CARTESIAN_POINT('Ctrl Pts',(41.7945517649514,44.0726835015639,49.8316591333403));
#20969=CARTESIAN_POINT('Ctrl Pts',(41.7949647447895,44.0727119845503,49.8317955906776));
#20970=CARTESIAN_POINT('Ctrl Pts',(41.802644360629,44.073241433279,49.8343302189699));
#20971=CARTESIAN_POINT('Ctrl Pts',(41.8099253057731,44.0737399005649,49.8366853220383));
#20972=CARTESIAN_POINT('Ctrl Pts',(41.8372994073923,44.0756015690712,49.8453601986768));
#20973=CARTESIAN_POINT('Ctrl Pts',(41.857482462897,44.0769491718269,49.8513943474694));
#20974=CARTESIAN_POINT('Ctrl Pts',(42.0156298450244,44.0873438253,49.8958673529716));
#20975=CARTESIAN_POINT('Ctrl Pts',(42.1574054013445,44.0957159842479,49.9191697108434));
#20976=CARTESIAN_POINT('Ctrl Pts',(42.4114178390357,44.1109409903733,49.9322925708581));
#20977=CARTESIAN_POINT('Ctrl Pts',(42.5226388205094,44.117681368905,49.9284293729212));
#20978=CARTESIAN_POINT('Ctrl Pts',(42.6498408732625,44.1258206152839,49.9129593041016));
#20979=CARTESIAN_POINT('Ctrl Pts',(42.6667522275056,44.1269112056682,49.9106744831074));
#20980=CARTESIAN_POINT('Ctrl Pts',(42.6945261795634,44.1287173643948,49.9065461500971));
#20981=CARTESIAN_POINT('Ctrl Pts',(42.705407473475,44.1294287994772,49.9048333679679));
#20982=CARTESIAN_POINT('Ctrl Pts',(42.7250226997228,44.1307184363763,49.9015734189465));
#20983=CARTESIAN_POINT('Ctrl Pts',(42.7337618230621,44.1312955816007,49.9000590159322));
#20984=CARTESIAN_POINT('Ctrl Pts',(42.7524718432505,44.132536891767,49.896683693981));
#20985=CARTESIAN_POINT('Ctrl Pts',(42.7624390922706,44.133201630543,49.8948042993963));
#20986=CARTESIAN_POINT('Ctrl Pts',(42.7896488916594,44.1350260328383,49.8894511542574));
#20987=CARTESIAN_POINT('Ctrl Pts',(42.8068591359874,44.136190683925,49.885820121738));
#20988=CARTESIAN_POINT('Ctrl Pts',(42.9064655863125,44.1429955197182,49.8633781252769));
#20989=CARTESIAN_POINT('Ctrl Pts',(42.9875927801679,44.1488004029118,49.8394065883173));
#20990=CARTESIAN_POINT('Ctrl Pts',(43.1738108736867,44.162728713393,49.7708037158923));
#20991=CARTESIAN_POINT('Ctrl Pts',(43.2770394165051,44.1709359854015,49.7220128398442));
#20992=CARTESIAN_POINT('Ctrl Pts',(43.4374301565022,44.1841297680354,49.6280229484996));
#20993=CARTESIAN_POINT('Ctrl Pts',(43.497434281177,44.1891738650293,49.5881940683947));
#20994=CARTESIAN_POINT('Ctrl Pts',(43.5634021499765,44.1947343333016,49.5388781643702));
#20995=CARTESIAN_POINT('Ctrl Pts',(43.5716758815666,44.1954319769836,49.5325880749808));
#20996=CARTESIAN_POINT('Ctrl Pts',(43.5849621858427,44.1965521446186,49.5223167011967));
#20997=CARTESIAN_POINT('Ctrl Pts',(43.5900063542189,44.1969773855264,49.5183768967088));
#20998=CARTESIAN_POINT('Ctrl Pts',(43.5989429662581,44.1977305742534,49.5113249665319));
#20999=CARTESIAN_POINT('Ctrl Pts',(43.6028430539011,44.198059202322,49.5082227887224));
#21000=CARTESIAN_POINT('Ctrl Pts',(43.611310724128,44.1987725191218,49.5014337612527));
#21001=CARTESIAN_POINT('Ctrl Pts',(43.6158735218903,44.1991567896593,49.4977411628335));
#21002=CARTESIAN_POINT('Ctrl Pts',(43.6287960694453,44.2002450515145,49.4871851816739));
#21003=CARTESIAN_POINT('Ctrl Pts',(43.6371152099097,44.2009455793342,49.4802721085683));
#21004=CARTESIAN_POINT('Ctrl Pts',(43.6941082232893,44.2057478818581,49.432095736227));
#21005=CARTESIAN_POINT('Ctrl Pts',(43.7407722777431,44.2096961072876,49.3885048882845));
#21006=CARTESIAN_POINT('Ctrl Pts',(43.8751461366115,44.2214273440893,49.2498758732937));
#21007=CARTESIAN_POINT('Ctrl Pts',(43.9555462062299,44.2289822161182,49.1482700154086));
#21008=CARTESIAN_POINT('Ctrl Pts',(44.0452292177111,44.2390689315626,49.0080414560762));
#21009=CARTESIAN_POINT('Ctrl Pts',(44.0643628533311,44.2413423243037,48.9761264469234));
#21010=CARTESIAN_POINT('Ctrl Pts',(44.1050799187064,44.2464903734566,48.9035287460759));
#21011=CARTESIAN_POINT('Ctrl Pts',(44.1261528171007,44.2493781097702,48.8625877646023));
#21012=CARTESIAN_POINT('Ctrl Pts',(44.1521891002928,44.253284623858,48.8072208933931));
#21013=CARTESIAN_POINT('Ctrl Pts',(44.1584760468713,44.2542575818108,48.7934319033404));
#21014=CARTESIAN_POINT('Ctrl Pts',(44.1684844117886,44.2558568639184,48.7707774337306));
#21015=CARTESIAN_POINT('Ctrl Pts',(44.1723032397453,44.2564798316299,48.7619555025706));
#21016=CARTESIAN_POINT('Ctrl Pts',(44.1795663281646,44.2576899213225,48.7448268922273));
#21017=CARTESIAN_POINT('Ctrl Pts',(44.1830187624535,44.258276745691,48.736523932966));
#21018=CARTESIAN_POINT('Ctrl Pts',(44.1909499317449,44.2596525986001,48.7170671943265));
#21019=CARTESIAN_POINT('Ctrl Pts',(44.1953826840854,44.2604431577854,48.7058951945795));
#21020=CARTESIAN_POINT('Ctrl Pts',(44.2094832602642,44.2630303332213,48.6693649098499));
#21021=CARTESIAN_POINT('Ctrl Pts',(44.218720071881,44.2648412161951,48.643844875651));
#21022=CARTESIAN_POINT('Ctrl Pts',(44.2393548408045,44.2691802610036,48.5828420036908));
#21023=CARTESIAN_POINT('Ctrl Pts',(44.2502686464073,44.2717231095403,48.5472080555882));
#21024=CARTESIAN_POINT('Ctrl Pts',(44.2890834621037,44.2818317589567,48.405992315646));
#21025=CARTESIAN_POINT('Ctrl Pts',(44.3090289062391,44.289613377377,48.2984457100565));
#21026=CARTESIAN_POINT('Ctrl Pts',(44.3296688283109,44.304599254482,48.0896821927224));
#21027=CARTESIAN_POINT('Ctrl Pts',(44.3317210339586,44.3117745488965,47.9889303963974));
#21028=CARTESIAN_POINT('Ctrl Pts',(44.324952285594,44.3197453285775,47.8720474256524));
#21029=CARTESIAN_POINT('Ctrl Pts',(44.3237911858304,44.3208560714008,47.855636982994));
#21030=CARTESIAN_POINT('Ctrl Pts',(44.3218825318956,44.3223874926704,47.8328122899058));
#21031=CARTESIAN_POINT('Ctrl Pts',(44.3213125314514,44.3228172770178,47.8263844585079));
#21032=CARTESIAN_POINT('Ctrl Pts',(44.3202739063996,44.3235554267425,47.8153041862278));
#21033=CARTESIAN_POINT('Ctrl Pts',(44.3198206050515,44.3238646276584,47.8106504163863));
#21034=CARTESIAN_POINT('Ctrl Pts',(44.3188292537852,44.3245144675831,47.8008425114936));
#21035=CARTESIAN_POINT('Ctrl Pts',(44.3182873484585,44.3248548770546,47.7956888151571));
#21036=CARTESIAN_POINT('Ctrl Pts',(44.3168928297472,44.3256957009547,47.7829213722241));
#21037=CARTESIAN_POINT('Ctrl Pts',(44.3160156040515,44.3261947505044,47.7753103000479));
#21038=CARTESIAN_POINT('Ctrl Pts',(44.3125488483363,44.3280611945961,47.7467296357037));
#21039=CARTESIAN_POINT('Ctrl Pts',(44.3096601119123,44.329412887069,47.7257969355128));
#21040=CARTESIAN_POINT('Ctrl Pts',(44.2843377234375,44.3398865984824,47.5621990192405));
#21041=CARTESIAN_POINT('Ctrl Pts',(44.2462890266302,44.3483231044245,47.4223959231744));
#21042=CARTESIAN_POINT('Ctrl Pts',(44.1524526307382,44.3635493628966,47.1860485052103));
#21043=CARTESIAN_POINT('Ctrl Pts',(44.1032821457636,44.3702176376007,47.0876226233518));
#21044=CARTESIAN_POINT('Ctrl Pts',(44.0371176264346,44.3782763389708,46.9793731511841));
#21045=CARTESIAN_POINT('Ctrl Pts',(44.0280330427057,44.379366057995,46.9649436394998));
#21046=CARTESIAN_POINT('Ctrl Pts',(44.0127690762492,44.3811710698602,46.9413972856629));
#21047=CARTESIAN_POINT('Ctrl Pts',(44.0067006515745,44.381882238631,46.9322093800622));
#21048=CARTESIAN_POINT('Ctrl Pts',(43.9956028970884,44.3831715900713,46.9157156221107));
#21049=CARTESIAN_POINT('Ctrl Pts',(43.9906011726788,44.383748718273,46.9083914976581));
#21050=CARTESIAN_POINT('Ctrl Pts',(43.979769747539,44.3849902108442,46.8927633311796));
#21051=CARTESIAN_POINT('Ctrl Pts',(43.9739247048349,44.3856551506623,46.8844702994348));
#21052=CARTESIAN_POINT('Ctrl Pts',(43.9577605398998,44.3874806757288,46.861916299017));
#21053=CARTESIAN_POINT('Ctrl Pts',(43.9473114243264,44.3886462588372,46.8477501437749));
#21054=CARTESIAN_POINT('Ctrl Pts',(43.8854058013768,44.3954708708344,46.7661837195868));
#21055=CARTESIAN_POINT('Ctrl Pts',(43.8297510505488,44.4012957498589,46.7021011777299));
#21056=CARTESIAN_POINT('Ctrl Pts',(43.6887826724702,44.415351384451,46.5598910765366));
#21057=CARTESIAN_POINT('Ctrl Pts',(43.6003000883232,44.423670631537,46.4853543489963));
#21058=CARTESIAN_POINT('Ctrl Pts',(43.4763390821255,44.4344002144715,46.3986505827933));
#21059=CARTESIAN_POINT('Ctrl Pts',(43.446417292435,44.4369248192642,46.378939588558));
#21060=CARTESIAN_POINT('Ctrl Pts',(43.3841735015363,44.442022002074,46.3403785128319));
#21061=CARTESIAN_POINT('Ctrl Pts',(43.351815786948,44.444590828384,46.3216114542265));
#21062=CARTESIAN_POINT('Ctrl Pts',(43.3103530828235,44.4477634934056,46.2991487463523));
#21063=CARTESIAN_POINT('Ctrl Pts',(43.3017403166854,44.448416204538,46.2945668780081));
#21064=CARTESIAN_POINT('Ctrl Pts',(43.288093890278,44.4494400083192,46.2874394589912));
#21065=CARTESIAN_POINT('Ctrl Pts',(43.2830833315075,44.4498137290852,46.2848503866386));
#21066=CARTESIAN_POINT('Ctrl Pts',(43.2735875603142,44.4505177538206,46.2799963439574));
#21067=CARTESIAN_POINT('Ctrl Pts',(43.2691048910654,44.4508483172728,46.2777269405711));
#21068=CARTESIAN_POINT('Ctrl Pts',(43.2585588003516,44.4516219113889,46.2724395194864));
#21069=CARTESIAN_POINT('Ctrl Pts',(43.2524882877063,44.45206404655,46.2694358867045));
#21070=CARTESIAN_POINT('Ctrl Pts',(43.2325139868229,44.4535089116539,46.259683398226));
#21071=CARTESIAN_POINT('Ctrl Pts',(43.2185444873535,44.4545037020621,46.2530694428768));
#21072=CARTESIAN_POINT('Ctrl Pts',(43.1403384798965,44.459994223197,46.2171864080761));
#21073=CARTESIAN_POINT('Ctrl Pts',(43.0746057385242,44.4643168939365,46.1912892287205));
#21074=CARTESIAN_POINT('Ctrl Pts',(42.9637164660441,44.4713639536715,46.1544909620969));
#21075=CARTESIAN_POINT('Ctrl Pts',(42.919328167095,44.47412240224,46.1415118242177));
#21076=CARTESIAN_POINT('Ctrl Pts',(42.743713150388,44.4849290864673,46.0969458894735));
#21077=CARTESIAN_POINT('Ctrl Pts',(42.6098052784933,44.4929709445296,46.0775718515764));
#21078=CARTESIAN_POINT('Ctrl Pts',(42.44969242427,44.5030745136266,46.0713440982121));
#21079=CARTESIAN_POINT('Ctrl Pts',(42.4243901517884,44.5046843019646,46.0708582348964));
#21080=CARTESIAN_POINT('Ctrl Pts',(42.3875208851583,44.507052428667,46.0708756926531));
#21081=CARTESIAN_POINT('Ctrl Pts',(42.3759557178011,44.5077984699511,46.0709851777651));
#21082=CARTESIAN_POINT('Ctrl Pts',(42.35544004121,44.5091278837904,46.0713639172474));
#21083=CARTESIAN_POINT('Ctrl Pts',(42.3464890329019,44.5097099339637,46.0715915107311));
#21084=CARTESIAN_POINT('Ctrl Pts',(42.3278255715669,44.5109279188057,46.0721960994265));
#21085=CARTESIAN_POINT('Ctrl Pts',(42.3181137561512,44.5115641859912,46.0725842004427));
#21086=CARTESIAN_POINT('Ctrl Pts',(42.2927783195184,44.5132306786596,46.073788478204));
#21087=CARTESIAN_POINT('Ctrl Pts',(42.2771612238085,44.5142645338645,46.0747213381197));
#21088=CARTESIAN_POINT('Ctrl Pts',(42.20587711682,44.5190148876253,46.0798502070654));
#21089=CARTESIAN_POINT('Ctrl Pts',(42.1504021385761,44.522800243875,46.0862709823012));
#21090=CARTESIAN_POINT('Ctrl Pts',(41.9888247749733,44.5340915716555,46.1121170755786));
#21091=CARTESIAN_POINT('Ctrl Pts',(41.8839873006605,44.5417702927968,46.1380405103852));
#21092=CARTESIAN_POINT('Ctrl Pts',(41.6848329192596,44.556789476346,46.2054043888763));
#21093=CARTESIAN_POINT('Ctrl Pts',(41.5905490290221,44.5641011349641,46.2459103208958));
#21094=CARTESIAN_POINT('Ctrl Pts',(41.4853714957469,44.5721968629705,46.3013923774642));
#21095=CARTESIAN_POINT('Ctrl Pts',(41.4709199992101,44.5733075912384,46.3092535516756));
#21096=CARTESIAN_POINT('Ctrl Pts',(41.4509416833998,44.5748389957339,46.3204546722301));
#21097=CARTESIAN_POINT('Ctrl Pts',(41.4453288843561,44.5752687776135,46.3236386844582));
#21098=CARTESIAN_POINT('Ctrl Pts',(41.4356767925214,44.5760069242515,46.3291782947736));
#21099=CARTESIAN_POINT('Ctrl Pts',(41.4316299366663,44.5763161245325,46.3315205003515));
#21100=CARTESIAN_POINT('Ctrl Pts',(41.4232059934553,44.5769590977154,46.3364370133502));
#21101=CARTESIAN_POINT('Ctrl Pts',(41.4188304862275,44.5772926886366,46.3390139290042));
#21102=CARTESIAN_POINT('Ctrl Pts',(41.4080943399973,44.57811041484,46.3453941134969));
#21103=CARTESIAN_POINT('Ctrl Pts',(41.4017452622689,44.5785933003072,46.3492168643332));
#21104=CARTESIAN_POINT('Ctrl Pts',(41.3880624276663,44.5796328068658,46.3575630463935));
#21105=CARTESIAN_POINT('Ctrl Pts',(41.3807365939153,44.5801886375716,46.3620992361198));
#21106=CARTESIAN_POINT('Ctrl Pts',(41.3600242338606,44.5817588096497,46.3751172072606));
#21107=CARTESIAN_POINT('Ctrl Pts',(41.3467111677523,44.5827664619391,46.3837152615999));
#21108=CARTESIAN_POINT('Ctrl Pts',(41.1990018193309,44.5939464344257,46.4817115180934));
#21109=CARTESIAN_POINT('Ctrl Pts',(41.0762131346019,44.6032845415953,46.5874849409357));
#21110=CARTESIAN_POINT('Ctrl Pts',(40.907236097218,44.6184783622448,46.7746720786511));
#21111=CARTESIAN_POINT('Ctrl Pts',(40.8512799600288,44.6240381896742,46.8462081153635));
#21112=CARTESIAN_POINT('Ctrl Pts',(40.7903682408413,44.6309625312971,46.9365335290933));
#21113=CARTESIAN_POINT('Ctrl Pts',(40.7803842250836,44.6321296057193,46.9518015264769));
#21114=CARTESIAN_POINT('Ctrl Pts',(40.7650546850809,44.6339742433446,46.975986143251));
#21115=CARTESIAN_POINT('Ctrl Pts',(40.7595619862318,44.6346463304575,46.9848085512758));
#21116=CARTESIAN_POINT('Ctrl Pts',(40.7499849206053,44.6358383244086,47.0004719768261));
#21117=CARTESIAN_POINT('Ctrl Pts',(40.745871114163,44.6363571323165,47.0072947783096));
#21118=CARTESIAN_POINT('Ctrl Pts',(40.7365191483165,44.6375524082843,47.0230246749955));
#21119=CARTESIAN_POINT('Ctrl Pts',(40.7313100928021,44.6382299178428,47.0319487017033));
#21120=CARTESIAN_POINT('Ctrl Pts',(40.7169888416897,44.6401260153166,47.0569425978092));
#21121=CARTESIAN_POINT('Ctrl Pts',(40.7080356097415,44.6413502667593,47.0731017939553));
#21122=CARTESIAN_POINT('Ctrl Pts',(40.6485241769207,44.6497623631535,47.1842468064908));
#21123=CARTESIAN_POINT('Ctrl Pts',(40.6057664372364,44.657224115982,47.2831738533788));
#21124=CARTESIAN_POINT('Ctrl Pts',(40.5280735476161,44.6744967608975,47.5142206047727));
#21125=CARTESIAN_POINT('Ctrl Pts',(40.4984575253915,44.6843669344272,47.6475406060921));
#21126=CARTESIAN_POINT('Ctrl Pts',(40.4797929190569,44.6958314494759,47.8123153779151));
#21127=CARTESIAN_POINT('Ctrl Pts',(40.4771361854944,44.6978557787251,47.8418363665111));
#21128=CARTESIAN_POINT('Ctrl Pts',(40.4745608733765,44.7004508831506,47.8803853438536));
#21129=CARTESIAN_POINT('Ctrl Pts',(40.4740239663874,44.7010520645172,47.8893662706633));
#21130=CARTESIAN_POINT('Ctrl Pts',(40.4732615496555,44.7020134619446,47.9038155566487));
#21131=CARTESIAN_POINT('Ctrl Pts',(40.4729964530498,44.7023758062247,47.9092815615021));
#21132=CARTESIAN_POINT('Ctrl Pts',(40.472544355564,44.7030507216995,47.9195019668547));
#21133=CARTESIAN_POINT('Ctrl Pts',(40.4723516813883,44.7033635983286,47.9242559915644));
#21134=CARTESIAN_POINT('Ctrl Pts',(40.4719917587624,44.7040047678499,47.9340302465868));
#21135=CARTESIAN_POINT('Ctrl Pts',(40.471826524601,44.7043329499244,47.9390505388711));
#21136=CARTESIAN_POINT('Ctrl Pts',(40.4714351338557,44.7052121787776,47.9525450201787));
#21137=CARTESIAN_POINT('Ctrl Pts',(40.4712452191392,44.7057612865506,47.9610202659963));
#21138=CARTESIAN_POINT('Ctrl Pts',(40.4709536582931,44.706949616164,47.9794572211443));
#21139=CARTESIAN_POINT('Ctrl Pts',(40.4708732945297,44.7075877611935,47.9894190445852));
#21140=CARTESIAN_POINT('Ctrl Pts',(40.4708700992302,44.7082223988407,47.9993812464564));
#21141=CARTESIAN_POINT('Ctrl Pts',(40.4708700998153,44.7082222827967,47.9993794248603));
#21142=CARTESIAN_POINT('Ctrl Pts',(40.470843159349,44.7135573880865,48.0831269933827));
#21143=CARTESIAN_POINT('Ctrl Pts',(40.476269768031,44.7186402214411,48.1668007065684));
#21144=CARTESIAN_POINT('Ctrl Pts',(40.4953914375786,44.7274943353322,48.3131877603739));
#21145=CARTESIAN_POINT('Ctrl Pts',(40.5068014281716,44.7312842329043,48.376058029797));
#21146=CARTESIAN_POINT('Ctrl Pts',(40.5434819363403,44.7409453478977,48.5333012428052));
#21147=CARTESIAN_POINT('Ctrl Pts',(40.5728348466523,44.7468497865584,48.6265253016374));
#21148=CARTESIAN_POINT('Ctrl Pts',(40.6197968579192,44.7547875813334,48.7438047007647));
#21149=CARTESIAN_POINT('Ctrl Pts',(40.6310757220145,44.7566114082301,48.7702437413479));
#21150=CARTESIAN_POINT('Ctrl Pts',(40.6480159447999,44.7592438900717,48.8076172154725));
#21151=CARTESIAN_POINT('Ctrl Pts',(40.6531981583057,44.76003617279,48.8187655407772));
#21152=CARTESIAN_POINT('Ctrl Pts',(40.662373983148,44.7614172562074,48.8380215095631));
#21153=CARTESIAN_POINT('Ctrl Pts',(40.666318710524,44.7620043475128,48.8461521179976));
#21154=CARTESIAN_POINT('Ctrl Pts',(40.6745331466187,44.7632136095346,48.8627845633017));
#21155=CARTESIAN_POINT('Ctrl Pts',(40.6788089047951,44.7638359798315,48.8712831187825));
#21156=CARTESIAN_POINT('Ctrl Pts',(40.6898478927262,44.7654252497102,48.8928259725496));
#21157=CARTESIAN_POINT('Ctrl Pts',(40.6966975125556,44.7663951765853,48.9058250731414));
#21158=CARTESIAN_POINT('Ctrl Pts',(40.7238531785901,44.7701798115556,48.9559633918994));
#21159=CARTESIAN_POINT('Ctrl Pts',(40.7452295745284,44.7730323046731,48.9925061891765));
#21160=CARTESIAN_POINT('Ctrl Pts',(40.8646202275298,44.7883415948761,49.1820112465663));
#21161=CARTESIAN_POINT('Ctrl Pts',(40.982670866585,44.8015449302295,49.3212488597038));
#21162=CARTESIAN_POINT('Ctrl Pts',(41.1456183604631,44.8168885332624,49.4660815434753));
#21163=CARTESIAN_POINT('Ctrl Pts',(41.1735149550632,44.8194267695809,49.4894976162129));
#21164=CARTESIAN_POINT('Ctrl Pts',(41.2140892001972,44.8229772335842,49.5216417714577));
#21165=CARTESIAN_POINT('Ctrl Pts',(41.2262328547696,44.8240225963962,49.5310286828503));
#21166=CARTESIAN_POINT('Ctrl Pts',(41.2452161736383,44.8256286127212,49.5453439387762));
#21167=CARTESIAN_POINT('Ctrl Pts',(41.2519780084274,44.8261952492517,49.5503738541882));
#21168=CARTESIAN_POINT('Ctrl Pts',(41.2645224556339,44.8272361706353,49.5595781996076));
#21169=CARTESIAN_POINT('Ctrl Pts',(41.2702956417047,44.8277112486902,49.5637651618043));
#21170=CARTESIAN_POINT('Ctrl Pts',(41.2802024523039,44.8285195347021,49.5708665080266));
#21171=CARTESIAN_POINT('Ctrl Pts',(41.2843245262642,44.8288538133343,49.5737968017262));
#21172=CARTESIAN_POINT('Ctrl Pts',(41.292279506086,44.8294949373911,49.579404863982));
#21173=CARTESIAN_POINT('Ctrl Pts',(41.2961106872475,44.8298019477392,49.5820849545345));
#21174=CARTESIAN_POINT('Ctrl Pts',(41.3052518239312,44.8305303895725,49.5884302363828));
#21175=CARTESIAN_POINT('Ctrl Pts',(41.3105705392294,44.8309509729924,49.5920827986583));
#21176=CARTESIAN_POINT('Ctrl Pts',(41.3295105755805,44.8324375477525,49.6049502790138));
#21177=CARTESIAN_POINT('Ctrl Pts',(41.343231743482,44.8334941975171,49.6140179371061));
#21178=CARTESIAN_POINT('Ctrl Pts',(41.4428992067248,44.841037386174,49.6780673625323));
#21179=CARTESIAN_POINT('Ctrl Pts',(41.5329829214778,44.8471604959084,49.7263368111641));
#21180=CARTESIAN_POINT('Ctrl Pts',(41.6813591843261,44.8568322662279,49.7912809908678));
#21181=CARTESIAN_POINT('Ctrl Pts',(41.7373092069277,44.8603918488044,49.812723502758));
#21182=CARTESIAN_POINT('Ctrl Pts',(41.7941389732838,44.8639880114013,49.8315225833187));
#21183=CARTESIAN_POINT('',(40.4708703960799,44.8789297818532,47.9987638045903));
#21184=CARTESIAN_POINT('Ctrl Pts',(41.7941386463292,45.0367815693785,49.8315224751633));
#21185=CARTESIAN_POINT('Ctrl Pts',(41.7423736161058,45.0334404792981,49.8143987806909));
#21186=CARTESIAN_POINT('Ctrl Pts',(41.6913362171882,45.0300469117126,49.7950810982887));
#21187=CARTESIAN_POINT('Ctrl Pts',(41.6255247393307,45.0254997752931,49.7669238847977));
#21188=CARTESIAN_POINT('Ctrl Pts',(41.6099743193676,45.0244125305486,49.7600259482308));
#21189=CARTESIAN_POINT('Ctrl Pts',(41.584524662545,45.0226108849182,49.7483316256625));
#21190=CARTESIAN_POINT('Ctrl Pts',(41.5745714042614,45.021900582945,49.7436545312493));
#21191=CARTESIAN_POINT('Ctrl Pts',(41.5566674567981,45.0206123168968,49.7350537105253));
#21192=CARTESIAN_POINT('Ctrl Pts',(41.5487027395109,45.0200354014174,49.7311597634824));
#21193=CARTESIAN_POINT('Ctrl Pts',(41.5406123916929,45.0194454123174,49.72713506268));
#21194=CARTESIAN_POINT('Ctrl Pts',(41.5404595371123,45.0194342639373,49.7270589968815));
#21195=CARTESIAN_POINT('Ctrl Pts',(41.5401928483905,45.0194148105832,49.7269262390483));
#21196=CARTESIAN_POINT('Ctrl Pts',(41.5400790096714,45.0194065059214,49.7268695560072));
#21197=CARTESIAN_POINT('Ctrl Pts',(41.5397866977003,45.0193851793683,49.7267239707617));
#21198=CARTESIAN_POINT('Ctrl Pts',(41.5396082326431,45.0193721569003,49.7266350521522));
#21199=CARTESIAN_POINT('Ctrl Pts',(41.5392621224038,45.0193468976411,49.7264625388534));
#21200=CARTESIAN_POINT('Ctrl Pts',(41.5390944755497,45.0193346609603,49.7263789473821));
#21201=CARTESIAN_POINT('Ctrl Pts',(41.5298426356076,45.0186592650582,49.721764145441));
#21202=CARTESIAN_POINT('Ctrl Pts',(41.5207944894213,45.0179936003734,49.7171614003344));
#21203=CARTESIAN_POINT('Ctrl Pts',(41.5021393074035,45.0166103008725,49.7074855077566));
#21204=CARTESIAN_POINT('Ctrl Pts',(41.4925379759166,45.0158923237027,49.7024021995704));
#21205=CARTESIAN_POINT('Ctrl Pts',(41.4682097558261,45.0140574616954,49.689257634042));
#21206=CARTESIAN_POINT('Ctrl Pts',(41.453544473358,45.0129366572529,49.6810848637387));
#21207=CARTESIAN_POINT('Ctrl Pts',(41.4113018213129,45.0096645778771,49.6568156234321));
#21208=CARTESIAN_POINT('Ctrl Pts',(41.3840161638718,45.0074961329812,49.6402252111127));
#21209=CARTESIAN_POINT('Ctrl Pts',(41.2869797716641,44.9995823233978,49.577874055057));
#21210=CARTESIAN_POINT('Ctrl Pts',(41.2198093055301,44.9937112261261,49.5282826336761));
#21211=CARTESIAN_POINT('Ctrl Pts',(41.0543020183072,44.9782968045226,49.3886559448686));
#21212=CARTESIAN_POINT('Ctrl Pts',(40.961695074283,44.968675125656,49.2924981652693));
#21213=CARTESIAN_POINT('Ctrl Pts',(40.8681808394641,44.9583011375594,49.17278486676));
#21214=CARTESIAN_POINT('Ctrl Pts',(40.8568513114721,44.9570319208137,49.1578369806458));
#21215=CARTESIAN_POINT('Ctrl Pts',(40.8412830214561,44.9552728724764,49.1366620335644));
#21216=CARTESIAN_POINT('Ctrl Pts',(40.8368603963706,44.954771410025,49.1305723249656));
#21217=CARTESIAN_POINT('Ctrl Pts',(40.8294993284876,44.9539340182063,49.1203107748375));
#21218=CARTESIAN_POINT('Ctrl Pts',(40.8265416266556,44.9535967919329,49.1161529200378));
#21219=CARTESIAN_POINT('Ctrl Pts',(40.8205269280826,44.9529095357372,49.1076262015717));
#21220=CARTESIAN_POINT('Ctrl Pts',(40.8174714929276,44.9525596108576,49.1032563225958));
#21221=CARTESIAN_POINT('Ctrl Pts',(40.8096688190126,44.951663775415,49.0919978381912));
#21222=CARTESIAN_POINT('Ctrl Pts',(40.8049481398534,44.9511196372045,49.0850908319305));
#21223=CARTESIAN_POINT('Ctrl Pts',(40.78530927915,44.9488458096467,49.0559513484828));
#21224=CARTESIAN_POINT('Ctrl Pts',(40.7708090234979,44.9471420299663,49.0334390691465));
#21225=CARTESIAN_POINT('Ctrl Pts',(40.7325473109733,44.9425550373151,48.9712280651652));
#21226=CARTESIAN_POINT('Ctrl Pts',(40.7097367402525,44.9397170417819,48.9309635449529));
#21227=CARTESIAN_POINT('Ctrl Pts',(40.6236849915747,44.9284124548377,48.7654571738873));
#21228=CARTESIAN_POINT('Ctrl Pts',(40.572743179318,44.9202308619044,48.6343137386726));
#21229=CARTESIAN_POINT('Ctrl Pts',(40.520525839078,44.9078969428999,48.4392296233924));
#21230=CARTESIAN_POINT('Ctrl Pts',(40.5074473200863,44.9040687749348,48.3789313774694));
#21231=CARTESIAN_POINT('Ctrl Pts',(40.494301056645,44.8990005486979,48.3003003637516));
#21232=CARTESIAN_POINT('Ctrl Pts',(40.4915731296504,44.8978448374018,48.2824457756304));
#21233=CARTESIAN_POINT('Ctrl Pts',(40.4876769970517,44.8960143892589,48.2543037785179));
#21234=CARTESIAN_POINT('Ctrl Pts',(40.4863401773526,44.8953449909518,48.2440404794934));
#21235=CARTESIAN_POINT('Ctrl Pts',(40.4841150665476,44.8941527027561,48.2258133805476));
#21236=CARTESIAN_POINT('Ctrl Pts',(40.4831936780118,44.8936308726527,48.217853808289));
#21237=CARTESIAN_POINT('Ctrl Pts',(40.4814094996555,44.8925596589843,48.2015524177631));
#21238=CARTESIAN_POINT('Ctrl Pts',(40.4805514656363,44.8920101369802,48.1932102618167));
#21239=CARTESIAN_POINT('Ctrl Pts',(40.4787714133191,44.890789076234,48.1747200752781));
#21240=CARTESIAN_POINT('Ctrl Pts',(40.4778753571803,44.8901167350987,48.1645698564228));
#21241=CARTESIAN_POINT('Ctrl Pts',(40.4753866197878,44.8880573703142,48.1335770792281));
#21242=CARTESIAN_POINT('Ctrl Pts',(40.4740522934086,44.8866623321658,48.1127158922622));
#21243=CARTESIAN_POINT('Ctrl Pts',(40.4715795845198,44.883169774431,48.0608334712548));
#21244=CARTESIAN_POINT('Ctrl Pts',(40.4708505080496,44.8810601831904,48.0297998266257));
#21245=CARTESIAN_POINT('Ctrl Pts',(40.4708703960799,44.8789297818532,47.9987638045903));
#21246=CARTESIAN_POINT('Ctrl Pts',(40.4708703945825,44.8789299424055,47.9987661435421));
#21247=CARTESIAN_POINT('Ctrl Pts',(40.4709724326017,44.867978938071,47.8392301113058));
#21248=CARTESIAN_POINT('Ctrl Pts',(40.49086526861,44.8564531196928,47.6803279747953));
#21249=CARTESIAN_POINT('Ctrl Pts',(40.5414990586299,44.8418592094896,47.4806989108018));
#21250=CARTESIAN_POINT('Ctrl Pts',(40.5545395419476,44.8385973656448,47.4361067117574));
#21251=CARTESIAN_POINT('Ctrl Pts',(40.5776381127016,44.8335470830323,47.3665488398514));
#21252=CARTESIAN_POINT('Ctrl Pts',(40.5866299052588,44.8317183841791,47.3412494416397));
#21253=CARTESIAN_POINT('Ctrl Pts',(40.5991158523297,44.8293558957583,47.3083144027753));
#21254=CARTESIAN_POINT('Ctrl Pts',(40.6021353196467,44.8287969673646,47.3005035552415));
#21255=CARTESIAN_POINT('Ctrl Pts',(40.6071611758204,44.8278868696172,47.287750074268));
#21256=CARTESIAN_POINT('Ctrl Pts',(40.6091373336753,44.8275339513328,47.2827957625002));
#21257=CARTESIAN_POINT('Ctrl Pts',(40.6130436461375,44.8268459665086,47.2731192882896));
#21258=CARTESIAN_POINT('Ctrl Pts',(40.6149720185738,44.8265108037601,47.2683964966507));
#21259=CARTESIAN_POINT('Ctrl Pts',(40.6193293622951,44.8257632488342,47.2578446840405));
#21260=CARTESIAN_POINT('Ctrl Pts',(40.6217682892586,44.8253514512753,47.2520197738926));
#21261=CARTESIAN_POINT('Ctrl Pts',(40.6303464607727,44.8239255053821,47.2318115647412));
#21262=CARTESIAN_POINT('Ctrl Pts',(40.6366321584293,44.8229197364394,47.2174905662762));
#21263=CARTESIAN_POINT('Ctrl Pts',(40.6948957382308,44.813926014354,47.0890143868371));
#21264=CARTESIAN_POINT('Ctrl Pts',(40.7577251613764,44.8064976170915,46.9800893579967));
#21265=CARTESIAN_POINT('Ctrl Pts',(40.8747699017995,44.7944934605443,46.8163790832072));
#21266=CARTESIAN_POINT('Ctrl Pts',(40.922436338929,44.7899663925866,46.7573857842215));
#21267=CARTESIAN_POINT('Ctrl Pts',(41.0022410071904,44.7827240258423,46.6697211024814));
#21268=CARTESIAN_POINT('Ctrl Pts',(41.0320777430282,44.7800811408751,46.6390589734195));
#21269=CARTESIAN_POINT('Ctrl Pts',(41.0777320774882,44.7761069848767,46.5951608436356));
#21270=CARTESIAN_POINT('Ctrl Pts',(41.09278325985,44.7748074163053,46.5811448773585));
#21271=CARTESIAN_POINT('Ctrl Pts',(41.1172707599401,44.7727077256139,46.559062025718));
#21272=CARTESIAN_POINT('Ctrl Pts',(41.1265661011602,44.7719139744075,46.5508407117222));
#21273=CARTESIAN_POINT('Ctrl Pts',(41.1444160274693,44.7703954528834,46.5353576055527));
#21274=CARTESIAN_POINT('Ctrl Pts',(41.1529559442039,44.7696713870429,46.5280796319701));
#21275=CARTESIAN_POINT('Ctrl Pts',(41.1617175441333,44.7689308296643,46.5207437141244));
#21276=CARTESIAN_POINT('Ctrl Pts',(41.1618763910715,44.7689174041986,46.5206107581764));
#21277=CARTESIAN_POINT('Ctrl Pts',(41.162106970917,44.7688979171034,46.5204178244549));
#21278=CARTESIAN_POINT('Ctrl Pts',(41.1621786868627,44.7688918562982,46.5203578262343));
#21279=CARTESIAN_POINT('Ctrl Pts',(41.162329086151,44.768879146191,46.5202320193915));
#21280=CARTESIAN_POINT('Ctrl Pts',(41.1624077703205,44.7688724968508,46.520166211881));
#21281=CARTESIAN_POINT('Ctrl Pts',(41.1625729614176,44.7688585374881,46.5200280766852));
#21282=CARTESIAN_POINT('Ctrl Pts',(41.1626594695308,44.7688512274045,46.5199557502314));
#21283=CARTESIAN_POINT('Ctrl Pts',(41.1628413039679,44.7688358625589,46.5198037518062));
#21284=CARTESIAN_POINT('Ctrl Pts',(41.1629366316815,44.7688278077278,46.5197240814297));
#21285=CARTESIAN_POINT('Ctrl Pts',(41.1631372704251,44.7688108550905,46.5195564300118));
#21286=CARTESIAN_POINT('Ctrl Pts',(41.1632425832294,44.7688019571948,46.5194684509292));
#21287=CARTESIAN_POINT('Ctrl Pts',(41.1698795621611,44.7682412188554,46.513925072767));
#21288=CARTESIAN_POINT('Ctrl Pts',(41.1764471568338,44.767687627967,46.5085130181536));
#21289=CARTESIAN_POINT('Ctrl Pts',(41.1907538015829,44.7664843441529,46.4968816552194));
#21290=CARTESIAN_POINT('Ctrl Pts',(41.1985054530697,44.7658340288824,46.4906783065771));
#21291=CARTESIAN_POINT('Ctrl Pts',(41.2193524546871,44.7640892629676,46.4742576209772));
#21292=CARTESIAN_POINT('Ctrl Pts',(41.232532213674,44.7629905295507,46.4641493002873));
#21293=CARTESIAN_POINT('Ctrl Pts',(41.2937017116993,44.7579095101366,46.4184771977336));
#21294=CARTESIAN_POINT('Ctrl Pts',(41.3431918427926,44.7538484104954,46.384987464447));
#21295=CARTESIAN_POINT('Ctrl Pts',(41.5173078070522,44.7397210808718,46.2785972171422));
#21296=CARTESIAN_POINT('Ctrl Pts',(41.6485130949886,44.7293007448234,46.2174086845285));
#21297=CARTESIAN_POINT('Ctrl Pts',(41.829756994872,44.7157477688924,46.156479905103));
#21298=CARTESIAN_POINT('Ctrl Pts',(41.8747585697353,44.7124517287111,46.1431571282205));
#21299=CARTESIAN_POINT('Ctrl Pts',(41.9463844072569,44.7073552214268,46.1247650644032));
#21300=CARTESIAN_POINT('Ctrl Pts',(41.972704982429,44.705513672462,46.1185929948208));
#21301=CARTESIAN_POINT('Ctrl Pts',(42.0073594651518,44.7031372922652,46.1112315029435));
#21302=CARTESIAN_POINT('Ctrl Pts',(42.0155822616169,44.7025769631413,46.1095407875614));
#21303=CARTESIAN_POINT('Ctrl Pts',(42.0290518657282,44.7016651673307,46.1068627793161));
#21304=CARTESIAN_POINT('Ctrl Pts',(42.034292092779,44.7013119395573,46.1058435167623));
#21305=CARTESIAN_POINT('Ctrl Pts',(42.0445449277631,44.7006238436473,46.1038933997009));
#21306=CARTESIAN_POINT('Ctrl Pts',(42.0495570874368,44.7002888760953,46.1029606451076));
#21307=CARTESIAN_POINT('Ctrl Pts',(42.0607741642925,44.699542267448,46.1009191385484));
#21308=CARTESIAN_POINT('Ctrl Pts',(42.0669809948305,44.699131216029,46.0998208950556));
#21309=CARTESIAN_POINT('Ctrl Pts',(42.0885391201781,44.6977103589045,46.0961152523012));
#21310=CARTESIAN_POINT('Ctrl Pts',(42.1039170009502,44.6967088542671,46.0936632230954));
#21311=CARTESIAN_POINT('Ctrl Pts',(42.245132941704,44.6876079878924,46.0728961948677));
#21312=CARTESIAN_POINT('Ctrl Pts',(42.3724823942881,44.6800844028492,46.0668768769691));
#21313=CARTESIAN_POINT('Ctrl Pts',(42.590101708618,44.6670852938379,46.0781175326622));
#21314=CARTESIAN_POINT('Ctrl Pts',(42.6802434599076,44.6616600025727,46.0891800762485));
#21315=CARTESIAN_POINT('Ctrl Pts',(42.8022201465067,44.6539949589518,46.1129682779991));
#21316=CARTESIAN_POINT('Ctrl Pts',(42.834998342928,44.6519032179486,46.1202537368055));
#21317=CARTESIAN_POINT('Ctrl Pts',(42.8918753760804,44.6482056126073,46.1344628457622));
#21318=CARTESIAN_POINT('Ctrl Pts',(42.9160607879954,44.6466115165172,46.1410079531934));
#21319=CARTESIAN_POINT('Ctrl Pts',(42.9512885878612,44.6442543345026,46.1512817915509));
#21320=CARTESIAN_POINT('Ctrl Pts',(42.9624362058356,44.6435031972122,46.1546426833999));
#21321=CARTESIAN_POINT('Ctrl Pts',(42.9820834559204,44.6421697809823,46.1607606895917));
#21322=CARTESIAN_POINT('Ctrl Pts',(42.9905957108091,44.6415888768626,46.1634763566809));
#21323=CARTESIAN_POINT('Ctrl Pts',(43.0083767254189,44.6403685924171,46.1692854421108));
#21324=CARTESIAN_POINT('Ctrl Pts',(43.0176414395447,44.6397288468269,46.1723903374381));
#21325=CARTESIAN_POINT('Ctrl Pts',(43.0419094953359,44.6380425636779,46.1807289252985));
#21326=CARTESIAN_POINT('Ctrl Pts',(43.0568721994432,44.6369922338485,46.1860777493972));
#21327=CARTESIAN_POINT('Ctrl Pts',(43.1210795103002,44.632437955839,46.2099289940278));
#21328=CARTESIAN_POINT('Ctrl Pts',(43.1696179032668,44.6288737845812,46.2302550332506));
#21329=CARTESIAN_POINT('Ctrl Pts',(43.340194777772,44.6159006237209,46.3100312165716));
#21330=CARTESIAN_POINT('Ctrl Pts',(43.456705972987,44.6061575130016,46.3803319823137));
#21331=CARTESIAN_POINT('Ctrl Pts',(43.6330693481546,44.5903969107667,46.5139297301077));
#21332=CARTESIAN_POINT('Ctrl Pts',(43.6977740300256,44.5843595749388,46.570087095085));
#21333=CARTESIAN_POINT('Ctrl Pts',(43.7666334402729,44.5778133642753,46.6383886392784));
#21334=CARTESIAN_POINT('Ctrl Pts',(43.774654288143,44.5770489016747,46.6464867709188));
#21335=CARTESIAN_POINT('Ctrl Pts',(43.7867813649554,44.5758907456385,46.6589497032574));
#21336=CARTESIAN_POINT('Ctrl Pts',(43.7909396458804,44.5754931970663,46.6632631685653));
#21337=CARTESIAN_POINT('Ctrl Pts',(43.7985124028554,44.5747685462889,46.6711921341488));
#21338=CARTESIAN_POINT('Ctrl Pts',(43.8019330077403,44.5744409830497,46.6748014759003));
#21339=CARTESIAN_POINT('Ctrl Pts',(43.8096167161664,44.573704605809,46.6829721917727));
#21340=CARTESIAN_POINT('Ctrl Pts',(43.813871656335,44.5732964123506,46.6875410573083));
#21341=CARTESIAN_POINT('Ctrl Pts',(43.8247971803144,44.572246948537,46.6993874492504));
#21342=CARTESIAN_POINT('Ctrl Pts',(43.8314343143005,44.5716081115383,46.706695772081));
#21343=CARTESIAN_POINT('Ctrl Pts',(43.8749240403026,44.5674109059882,46.7553283990281));
#21344=CARTESIAN_POINT('Ctrl Pts',(43.9100426959746,44.5639674134161,46.7981761250351));
#21345=CARTESIAN_POINT('Ctrl Pts',(44.0208473927045,44.5526879625133,46.9459072870236));
#21346=CARTESIAN_POINT('Ctrl Pts',(44.0878315025941,44.545132787662,47.0568744611161));
#21347=CARTESIAN_POINT('Ctrl Pts',(44.1802984631841,44.5320972491625,47.25195153617));
#21348=CARTESIAN_POINT('Ctrl Pts',(44.2120701610644,44.5267761860267,47.3325885493896));
#21349=CARTESIAN_POINT('Ctrl Pts',(44.2436797458177,44.5201433879846,47.431932817233));
#21350=CARTESIAN_POINT('Ctrl Pts',(44.2488098709077,44.5190109955122,47.4488581334481));
#21351=CARTESIAN_POINT('Ctrl Pts',(44.2565201293395,44.5172159666035,47.4756157603817));
#21352=CARTESIAN_POINT('Ctrl Pts',(44.2592565759015,44.5165584388225,47.4854022932371));
#21353=CARTESIAN_POINT('Ctrl Pts',(44.264235076308,44.5153225945993,47.5037654625107));
#21354=CARTESIAN_POINT('Ctrl Pts',(44.2664955895562,44.5147448961752,47.5123368522467));
#21355=CARTESIAN_POINT('Ctrl Pts',(44.2714239707434,44.5134472182802,47.5315606062156));
#21356=CARTESIAN_POINT('Ctrl Pts',(44.2740601004344,44.5127262323699,47.5422207132381));
#21357=CARTESIAN_POINT('Ctrl Pts',(44.2805352691786,44.5108842733074,47.5693989816944));
#21358=CARTESIAN_POINT('Ctrl Pts',(44.2842477076333,44.5097592803214,47.5859460415572));
#21359=CARTESIAN_POINT('Ctrl Pts',(44.3087666296874,44.5018152040406,47.7023988192331));
#21360=CARTESIAN_POINT('Ctrl Pts',(44.3218317882982,44.4947504316987,47.8037525765928));
#21361=CARTESIAN_POINT('Ctrl Pts',(44.3346266640926,44.47624343602,48.0650494290505));
#21362=CARTESIAN_POINT('Ctrl Pts',(44.3226228709961,44.4646164912893,48.2248010721459));
#21363=CARTESIAN_POINT('Ctrl Pts',(44.2879385884095,44.4526840284092,48.396841743561));
#21364=CARTESIAN_POINT('Ctrl Pts',(44.2846027761546,44.4516114426936,48.4123928946114));
#21365=CARTESIAN_POINT('Ctrl Pts',(44.279555525584,44.4500914339533,48.4345808366251));
#21366=CARTESIAN_POINT('Ctrl Pts',(44.2780005638145,44.4496357588842,48.4412520404267));
#21367=CARTESIAN_POINT('Ctrl Pts',(44.2752412150599,44.4488486907401,48.4528115336905));
#21368=CARTESIAN_POINT('Ctrl Pts',(44.2740531782585,44.4485163808613,48.4577036018745));
#21369=CARTESIAN_POINT('Ctrl Pts',(44.2715035002255,44.4478168916883,48.4680262258863));
#21370=CARTESIAN_POINT('Ctrl Pts',(44.270137360466,44.4474499721514,48.4734555464257));
#21371=CARTESIAN_POINT('Ctrl Pts',(44.2663715167304,44.4464593097702,48.4881511426683));
#21372=CARTESIAN_POINT('Ctrl Pts',(44.263926414207,44.4458381152197,48.4974057782156));
#21373=CARTESIAN_POINT('Ctrl Pts',(44.252132506195,44.4429405619229,48.540736818069));
#21374=CARTESIAN_POINT('Ctrl Pts',(44.2419168429715,44.4407097468855,48.5745727475855));
#21375=CARTESIAN_POINT('Ctrl Pts',(44.193164862755,44.4310957552315,48.7213451880885));
#21376=CARTESIAN_POINT('Ctrl Pts',(44.1451256246305,44.4240747086526,48.830855492058));
#21377=CARTESIAN_POINT('Ctrl Pts',(44.0323095037777,44.4101622090856,49.0343892116458));
#21378=CARTESIAN_POINT('Ctrl Pts',(43.9687221775344,44.4033061481595,49.1284951405384));
#21379=CARTESIAN_POINT('Ctrl Pts',(43.8840127041285,44.3947944864602,49.2327567923794));
#21380=CARTESIAN_POINT('Ctrl Pts',(43.8705141988492,44.393454759686,49.2488278307978));
#21381=CARTESIAN_POINT('Ctrl Pts',(43.8496400426422,44.3914058476817,49.2728724001446));
#21382=CARTESIAN_POINT('Ctrl Pts',(43.8424545416399,44.3907045097692,49.281009479908));
#21383=CARTESIAN_POINT('Ctrl Pts',(43.8292827701946,44.3894257482372,49.2956742481131));
#21384=CARTESIAN_POINT('Ctrl Pts',(43.8233194548827,44.388849301627,49.3022222234888));
#21385=CARTESIAN_POINT('Ctrl Pts',(43.8103529791841,44.3876010879183,49.3162645009454));
#21386=CARTESIAN_POINT('Ctrl Pts',(43.8033347412038,44.3869286848072,49.3237444464706));
#21387=CARTESIAN_POINT('Ctrl Pts',(43.784078419096,44.3850921848582,49.3439423338812));
#21388=CARTESIAN_POINT('Ctrl Pts',(43.7717251609623,44.38392310633,49.3565486037799));
#21389=CARTESIAN_POINT('Ctrl Pts',(43.7038721156012,44.3775483195533,49.4239167968687));
#21390=CARTESIAN_POINT('Ctrl Pts',(43.6452711664185,44.3722041151454,49.4754383911357));
#21391=CARTESIAN_POINT('Ctrl Pts',(43.4816054935064,44.3576977433641,49.6026217872984));
#21392=CARTESIAN_POINT('Ctrl Pts',(43.3717717206397,44.3483569994922,49.6715031069482));
#21393=CARTESIAN_POINT('Ctrl Pts',(43.1986480350866,44.3346946891759,49.7572089242787));
#21394=CARTESIAN_POINT('Ctrl Pts',(43.1400299648216,44.3302390817495,49.7826887915561));
#21395=CARTESIAN_POINT('Ctrl Pts',(43.0701284780476,44.3252027094052,49.8090293991536));
#21396=CARTESIAN_POINT('Ctrl Pts',(43.0599749813627,44.3244778422603,49.8127582799106));
#21397=CARTESIAN_POINT('Ctrl Pts',(43.0442646965057,44.3233671372757,49.8183783979983));
#21398=CARTESIAN_POINT('Ctrl Pts',(43.0387299356031,44.3229779013409,49.8203299341357));
#21399=CARTESIAN_POINT('Ctrl Pts',(43.0284804045336,44.322261025031,49.8238913774928));
#21400=CARTESIAN_POINT('Ctrl Pts',(43.0237683138959,44.3219329918874,49.8255082764228));
#21401=CARTESIAN_POINT('Ctrl Pts',(43.0129909110555,44.3211861907937,49.829159813866));
#21402=CARTESIAN_POINT('Ctrl Pts',(43.0069217026778,44.3207681239778,49.8311825499965));
#21403=CARTESIAN_POINT('Ctrl Pts',(42.9909732043189,44.3196757787265,49.8364098382488));
#21404=CARTESIAN_POINT('Ctrl Pts',(42.9810777472447,44.3190042761616,49.8395649174088));
#21405=CARTESIAN_POINT('Ctrl Pts',(42.9009088509373,44.3136108155313,49.8644146051119));
#21406=CARTESIAN_POINT('Ctrl Pts',(42.8294640369798,44.3090928128288,49.8821569444686));
#21407=CARTESIAN_POINT('Ctrl Pts',(42.6464502019643,44.2978433315819,49.9166375385295));
#21408=CARTESIAN_POINT('Ctrl Pts',(42.5341129617762,44.2912241062349,49.9277582219177));
#21409=CARTESIAN_POINT('Ctrl Pts',(42.3372064641162,44.2793209738718,49.9299473170228));
#21410=CARTESIAN_POINT('Ctrl Pts',(42.2530061754285,44.2741375029644,49.9253648643706));
#21411=CARTESIAN_POINT('Ctrl Pts',(42.1519353140055,44.2676596671101,49.9131950365065));
#21412=CARTESIAN_POINT('Ctrl Pts',(42.134519211903,44.2665343998929,49.9108561574548));
#21413=CARTESIAN_POINT('Ctrl Pts',(42.1071100756304,44.2647481254039,49.9067933334878));
#21414=CARTESIAN_POINT('Ctrl Pts',(42.0970942450684,44.2640921420708,49.9052279185289));
#21415=CARTESIAN_POINT('Ctrl Pts',(42.0783417785628,44.2628576602189,49.9021454122809));
#21416=CARTESIAN_POINT('Ctrl Pts',(42.0696023287689,44.2622797664983,49.9006468781169));
#21417=CARTESIAN_POINT('Ctrl Pts',(42.050029776578,44.2609796181628,49.8971517437394));
#21418=CARTESIAN_POINT('Ctrl Pts',(42.0392028921651,44.2602563399303,49.8951225117285));
#21419=CARTESIAN_POINT('Ctrl Pts',(42.0116430755937,44.2584045554499,49.8897123771522));
#21420=CARTESIAN_POINT('Ctrl Pts',(41.9949368460913,44.2572719552437,49.8862019452984));
#21421=CARTESIAN_POINT('Ctrl Pts',(41.9160554454613,44.2518749764341,49.8685305509943));
#21422=CARTESIAN_POINT('Ctrl Pts',(41.8546007877818,44.2475229709969,49.8515231493321));
#21423=CARTESIAN_POINT('Ctrl Pts',(41.7941385063105,44.2430936274184,49.8315224288456));
#21424=CARTESIAN_POINT('Origin',(42.4,48.4493818343519,48.));
#21425=CARTESIAN_POINT('',(41.7941388354972,43.276409063163,49.8315225377394));
#21426=CARTESIAN_POINT('',(41.7941388168303,43.4464579097838,49.8315225315644));
#21427=CARTESIAN_POINT('',(41.7941388317924,48.4493818343519,49.8315225365138));
#21428=CARTESIAN_POINT('Ctrl Pts',(41.7941388354972,43.2764090631631,49.8315225377394));
#21429=CARTESIAN_POINT('Ctrl Pts',(41.7975715031584,43.276665280169,49.8326580520362));
#21430=CARTESIAN_POINT('Ctrl Pts',(41.8010075428829,43.2769216588947,49.8337839754625));
#21431=CARTESIAN_POINT('Ctrl Pts',(41.9411257165846,43.2873726318826,49.8792620926758));
#21432=CARTESIAN_POINT('Ctrl Pts',(42.0823349862631,43.2977977663472,49.9082147047067));
#21433=CARTESIAN_POINT('Ctrl Pts',(42.2464553596324,43.3090798354582,49.9231254082622));
#21434=CARTESIAN_POINT('Ctrl Pts',(42.2674885771241,43.3105094144422,49.9246890932136));
#21435=CARTESIAN_POINT('Ctrl Pts',(42.2961871406248,43.3124340705385,49.9263499310011));
#21436=CARTESIAN_POINT('Ctrl Pts',(42.3038327654162,43.3129443168211,49.9267467488836));
#21437=CARTESIAN_POINT('Ctrl Pts',(42.316656105874,43.3137956853094,49.9273357760045));
#21438=CARTESIAN_POINT('Ctrl Pts',(42.3218325387782,43.3141381515784,49.9275526577141));
#21439=CARTESIAN_POINT('Ctrl Pts',(42.3316832862201,43.3147874879727,49.9279256353647));
#21440=CARTESIAN_POINT('Ctrl Pts',(42.3363573765215,43.3150945785567,49.9280855910779));
#21441=CARTESIAN_POINT('Ctrl Pts',(42.3474859909983,43.3158234209757,49.9284259197283));
#21442=CARTESIAN_POINT('Ctrl Pts',(42.3539409808172,43.3162443225578,49.9285908894053));
#21443=CARTESIAN_POINT('Ctrl Pts',(42.3768669786843,43.3177330343508,49.9290616376128));
#21444=CARTESIAN_POINT('Ctrl Pts',(42.393341487202,43.3187914684695,49.9291888570559));
#21445=CARTESIAN_POINT('Ctrl Pts',(42.5076464392224,43.3260690142513,49.9286072159227));
#21446=CARTESIAN_POINT('Ctrl Pts',(42.6053101363888,43.3319548300672,49.9206681557122));
#21447=CARTESIAN_POINT('Ctrl Pts',(42.8081114099056,43.3442245502955,49.8885281861765));
#21448=CARTESIAN_POINT('Ctrl Pts',(42.9126655714818,43.3505844924173,49.8628650763818));
#21449=CARTESIAN_POINT('Ctrl Pts',(43.0714281067766,43.3608467820581,49.8095107231967));
#21450=CARTESIAN_POINT('Ctrl Pts',(43.1273914950086,43.3645857997682,49.7877486620164));
#21451=CARTESIAN_POINT('Ctrl Pts',(43.1968771704807,43.369433303414,49.7569250218533));
#21452=CARTESIAN_POINT('Ctrl Pts',(43.2114267590251,43.3704599693332,49.7502529380138));
#21453=CARTESIAN_POINT('Ctrl Pts',(43.2347463648457,43.3721251730052,49.7392058740867));
#21454=CARTESIAN_POINT('Ctrl Pts',(43.2435692097062,43.3727597976222,49.7349436730388));
#21455=CARTESIAN_POINT('Ctrl Pts',(43.2603710078212,43.3739773655123,49.7266684823949));
#21456=CARTESIAN_POINT('Ctrl Pts',(43.2683553322433,43.3745598966194,49.7226669241696));
#21457=CARTESIAN_POINT('Ctrl Pts',(43.2864710827563,43.3758907466995,49.7134297855369));
#21458=CARTESIAN_POINT('Ctrl Pts',(43.2965843682175,43.3766402732126,49.708159556855));
#21459=CARTESIAN_POINT('Ctrl Pts',(43.3282057995978,43.3790049089169,49.6913228324035));
#21460=CARTESIAN_POINT('Ctrl Pts',(43.3495406807893,43.3806312659304,49.6794378023391));
#21461=CARTESIAN_POINT('Ctrl Pts',(43.5010307337941,43.3924088401268,49.591237764396));
#21462=CARTESIAN_POINT('Ctrl Pts',(43.6220386995323,43.4031117889145,49.5003035490512));
#21463=CARTESIAN_POINT('Ctrl Pts',(43.7510454448362,43.4158447357743,49.3773056551403));
#21464=CARTESIAN_POINT('Ctrl Pts',(43.7704886522386,43.4178028154307,49.3579600671733));
#21465=CARTESIAN_POINT('Ctrl Pts',(43.8459060223926,43.4255393036476,49.2796512083813));
#21466=CARTESIAN_POINT('Ctrl Pts',(43.8985483732908,43.4312627900929,49.2175825798966));
#21467=CARTESIAN_POINT('Ctrl Pts',(43.9538804706296,43.4375138174259,49.1432961389503));
#21468=CARTESIAN_POINT('Ctrl Pts',(43.9605595460669,43.4382726417457,49.1341624648564));
#21469=CARTESIAN_POINT('Ctrl Pts',(43.9706424125512,43.4394241240661,49.1201163645016));
#21470=CARTESIAN_POINT('Ctrl Pts',(43.9741042464648,43.4398205700947,49.1152461978355));
#21471=CARTESIAN_POINT('Ctrl Pts',(43.9804070353457,43.4405442674723,49.1062915130103));
#21472=CARTESIAN_POINT('Ctrl Pts',(43.9832548257231,43.4408719701686,49.1022120790014));
#21473=CARTESIAN_POINT('Ctrl Pts',(43.9896539119269,43.4416099848318,49.0929694708962));
#21474=CARTESIAN_POINT('Ctrl Pts',(43.9931958522108,43.4420196646912,49.0877999831043));
#21475=CARTESIAN_POINT('Ctrl Pts',(44.0022939659063,43.4430753428977,49.0743814581237));
#21476=CARTESIAN_POINT('Ctrl Pts',(44.0078117318297,43.4437188605155,49.0661064280149));
#21477=CARTESIAN_POINT('Ctrl Pts',(44.0445890219552,43.4480331072836,49.0100162853374));
#21478=CARTESIAN_POINT('Ctrl Pts',(44.073778560978,43.4515814793416,48.9608707693914));
#21479=CARTESIAN_POINT('Ctrl Pts',(44.1227695663135,43.4579136050964,48.8693589383856));
#21480=CARTESIAN_POINT('Ctrl Pts',(44.1432939914581,43.460716116266,48.8274335797468));
#21481=CARTESIAN_POINT('Ctrl Pts',(44.1944880052587,43.4682400723816,48.7124773144469));
#21482=CARTESIAN_POINT('Ctrl Pts',(44.2222138335924,43.4729334213454,48.6382379025086));
#21483=CARTESIAN_POINT('Ctrl Pts',(44.2694315330769,43.4827055493593,48.4833402694934));
#21484=CARTESIAN_POINT('Ctrl Pts',(44.2884417178294,43.4877827075432,48.4027127371394));
#21485=CARTESIAN_POINT('Ctrl Pts',(44.3056706737414,43.4943425595646,48.3006536923249));
#21486=CARTESIAN_POINT('Ctrl Pts',(44.3087950133277,43.4956677845776,48.2801337236734));
#21487=CARTESIAN_POINT('Ctrl Pts',(44.3130421231307,43.4976991307694,48.2488558941182));
#21488=CARTESIAN_POINT('Ctrl Pts',(44.3144065851741,43.4983976145959,48.2381319795386));
#21489=CARTESIAN_POINT('Ctrl Pts',(44.3167248023132,43.4996735525186,48.2186024455147));
#21490=CARTESIAN_POINT('Ctrl Pts',(44.3177081907035,43.5002500535302,48.2098005907817));
#21491=CARTESIAN_POINT('Ctrl Pts',(44.3197039522671,43.5015011173647,48.190749473044));
#21492=CARTESIAN_POINT('Ctrl Pts',(44.3206949225203,43.5021763371244,48.1804982920261));
#21493=CARTESIAN_POINT('Ctrl Pts',(44.3231769383866,43.504027484259,48.1524822227429));
#21494=CARTESIAN_POINT('Ctrl Pts',(44.3245038607183,43.5052085244415,48.1347041878618));
#21495=CARTESIAN_POINT('Ctrl Pts',(44.3305079942351,43.5118153346209,48.0358128695151));
#21496=CARTESIAN_POINT('Ctrl Pts',(44.3303030574671,43.5173921330822,47.9544959544679));
#21497=CARTESIAN_POINT('Ctrl Pts',(44.3166421118602,43.531990720408,47.7467081781516));
#21498=CARTESIAN_POINT('Ctrl Pts',(44.2958141403414,43.5411643913227,47.6211082510863));
#21499=CARTESIAN_POINT('Ctrl Pts',(44.246511159677,43.554569705622,47.4379818211263));
#21500=CARTESIAN_POINT('Ctrl Pts',(44.2272838235973,43.558937474795,47.3783059990936));
#21501=CARTESIAN_POINT('Ctrl Pts',(44.2013845006594,43.5638884526781,47.3095852724974));
#21502=CARTESIAN_POINT('Ctrl Pts',(44.1975007585216,43.5646103904829,47.2995361169574));
#21503=CARTESIAN_POINT('Ctrl Pts',(44.1913745711189,43.5657176461611,47.2840711990845));
#21504=CARTESIAN_POINT('Ctrl Pts',(44.1891913623335,43.5661063288004,47.2786324284739));
#21505=CARTESIAN_POINT('Ctrl Pts',(44.1851054964215,43.5668228148672,47.2685864590024));
#21506=CARTESIAN_POINT('Ctrl Pts',(44.1832097740388,43.5671510057109,47.2639766960238));
#21507=CARTESIAN_POINT('Ctrl Pts',(44.1788341179247,43.567898976042,47.2534527054526));
#21508=CARTESIAN_POINT('Ctrl Pts',(44.1763425445749,43.5683180468312,47.2475434568451));
#21509=CARTESIAN_POINT('Ctrl Pts',(44.1697193537832,43.5694145677293,47.2320515254324));
#21510=CARTESIAN_POINT('Ctrl Pts',(44.165539305244,43.5700892085273,47.2224895987797));
#21511=CARTESIAN_POINT('Ctrl Pts',(44.1301719690914,43.5756592964805,47.1433424305889));
#21512=CARTESIAN_POINT('Ctrl Pts',(44.0949576401499,43.5803353358937,47.0756198223535));
#21513=CARTESIAN_POINT('Ctrl Pts',(43.9875507532231,43.5929630077305,46.8959490133234));
#21514=CARTESIAN_POINT('Ctrl Pts',(43.9076500297772,43.6007492419639,46.7891169228497));
#21515=CARTESIAN_POINT('Ctrl Pts',(43.7743141058009,43.612765729854,46.6447009128769));
#21516=CARTESIAN_POINT('Ctrl Pts',(43.728964592965,43.6167144621358,46.6002047598228));
#21517=CARTESIAN_POINT('Ctrl Pts',(43.6693359420291,43.6217996257477,46.5472116584798));
#21518=CARTESIAN_POINT('Ctrl Pts',(43.6570285595474,43.6228437416178,46.5365496683462));
#21519=CARTESIAN_POINT('Ctrl Pts',(43.6370552901654,43.624530388685,46.5196845054426));
#21520=CARTESIAN_POINT('Ctrl Pts',(43.6294740703362,43.6251688187024,46.5133819391931));
#21521=CARTESIAN_POINT('Ctrl Pts',(43.6149453274925,43.6263891603908,46.5014907731391));
#21522=CARTESIAN_POINT('Ctrl Pts',(43.6080066993058,43.6269706243822,46.4958916722165));
#21523=CARTESIAN_POINT('Ctrl Pts',(43.5920470790329,43.6283051425013,46.4831947812085));
#21524=CARTESIAN_POINT('Ctrl Pts',(43.5830011229461,43.6290594519708,46.476129059341));
#21525=CARTESIAN_POINT('Ctrl Pts',(43.5547221313414,43.6314114199397,46.4544441207616));
#21526=CARTESIAN_POINT('Ctrl Pts',(43.5352777860506,43.6330199771991,46.4401056335424));
#21527=CARTESIAN_POINT('Ctrl Pts',(43.3901208153211,43.6449707105291,46.3372169280715));
#21528=CARTESIAN_POINT('Ctrl Pts',(43.2545127101431,43.6558890937721,46.2636311230716));
#21529=CARTESIAN_POINT('Ctrl Pts',(43.0430540585999,43.6721392356012,46.1797061094291));
#21530=CARTESIAN_POINT('Ctrl Pts',(42.9729532240893,43.6773992446181,46.1564397796033));
#21531=CARTESIAN_POINT('Ctrl Pts',(42.8783742674408,43.6842070487545,46.1309672092805));
#21532=CARTESIAN_POINT('Ctrl Pts',(42.8549435506806,43.6858704171769,46.1251261397517));
#21533=CARTESIAN_POINT('Ctrl Pts',(42.8150663185979,43.6886555811409,46.1159767449595));
#21534=CARTESIAN_POINT('Ctrl Pts',(42.7986755027144,43.6897874034543,46.1124403148853));
#21535=CARTESIAN_POINT('Ctrl Pts',(42.7753813670654,43.6913756209772,46.1077314278336));
#21536=CARTESIAN_POINT('Ctrl Pts',(42.7685151143263,43.6918412816118,46.1063822629051));
#21537=CARTESIAN_POINT('Ctrl Pts',(42.75667298781,43.6926399413582,46.1041222290622));
#21538=CARTESIAN_POINT('Ctrl Pts',(42.751700636494,43.6929739341083,46.1031935240198));
#21539=CARTESIAN_POINT('Ctrl Pts',(42.7412807160417,43.6936709459347,46.1012897392622));
#21540=CARTESIAN_POINT('Ctrl Pts',(42.735832553949,43.6940337471013,46.1003185322283));
#21541=CARTESIAN_POINT('Ctrl Pts',(42.7212422164955,43.6950011411089,46.097782341282));
#21542=CARTESIAN_POINT('Ctrl Pts',(42.7120926693597,43.6956033871048,46.0962597979347));
#21543=CARTESIAN_POINT('Ctrl Pts',(42.6712269806596,43.698275088917,46.0897620248764));
#21544=CARTESIAN_POINT('Ctrl Pts',(42.6393985648793,43.7003072126593,46.0855126511284));
#21545=CARTESIAN_POINT('Ctrl Pts',(42.4666167549632,43.7111477721222,46.0668216580508));
#21546=CARTESIAN_POINT('Ctrl Pts',(42.32449354293,43.7194068259032,46.0671463247065));
#21547=CARTESIAN_POINT('Ctrl Pts',(42.0934278812835,43.7333759436952,46.0932214078828));
#21548=CARTESIAN_POINT('Ctrl Pts',(42.0040214398104,43.7389123784923,46.1097647864302));
#21549=CARTESIAN_POINT('Ctrl Pts',(41.8933814627704,43.7461334256677,46.1384329404577));
#21550=CARTESIAN_POINT('Ctrl Pts',(41.8707543316497,43.7476297257804,46.1447390465631));
#21551=CARTESIAN_POINT('Ctrl Pts',(41.8373717383794,43.7498689715142,46.1547030468463));
#21552=CARTESIAN_POINT('Ctrl Pts',(41.8265238041166,43.7506016445557,46.1580454810828));
#21553=CARTESIAN_POINT('Ctrl Pts',(41.8072231524517,43.7519144733605,46.1641793671379));
#21554=CARTESIAN_POINT('Ctrl Pts',(41.7987590002781,43.7524934031783,46.1669339775062));
#21555=CARTESIAN_POINT('Ctrl Pts',(41.7808943672514,43.7537222309119,46.1728849639977));
#21556=CARTESIAN_POINT('Ctrl Pts',(41.7714989212474,43.7543725844009,46.1760955268901));
#21557=CARTESIAN_POINT('Ctrl Pts',(41.7464588137315,43.7561170165039,46.1848685542025));
#21558=CARTESIAN_POINT('Ctrl Pts',(41.7308607701812,43.7572153730897,46.1905606091011));
#21559=CARTESIAN_POINT('Ctrl Pts',(41.6600562232286,43.7622561306587,46.2174393917042));
#21560=CARTESIAN_POINT('Ctrl Pts',(41.605773630995,43.7662756351905,46.2409541444119));
#21561=CARTESIAN_POINT('Ctrl Pts',(41.4063900519842,43.7816363555379,46.3384370620226));
#21562=CARTESIAN_POINT('Ctrl Pts',(41.2697669650518,43.7934630219118,46.4281812999105));
#21563=CARTESIAN_POINT('Ctrl Pts',(41.119281008156,43.8073865329362,46.5568979715536));
#21564=CARTESIAN_POINT('Ctrl Pts',(41.0931300570314,43.8098408413477,46.5805367731922));
#21565=CARTESIAN_POINT('Ctrl Pts',(41.0516260388392,43.8137748127579,46.620173721828));
#21566=CARTESIAN_POINT('Ctrl Pts',(41.0358757247195,43.8152773185176,46.6357427067194));
#21567=CARTESIAN_POINT('Ctrl Pts',(41.0149444024027,43.8172830071215,46.6571580946363));
#21568=CARTESIAN_POINT('Ctrl Pts',(41.0095263875965,43.8178030069971,46.6627690814153));
#21569=CARTESIAN_POINT('Ctrl Pts',(41.0005457322842,43.8186660962003,46.6721831975122));
#21570=CARTESIAN_POINT('Ctrl Pts',(40.9969642539146,43.8190106079839,46.6759681251936));
#21571=CARTESIAN_POINT('Ctrl Pts',(40.9902148208032,43.8196603669834,46.6831591056424));
#21572=CARTESIAN_POINT('Ctrl Pts',(40.9870437832673,43.8199658576736,46.6865621738041));
#21573=CARTESIAN_POINT('Ctrl Pts',(40.9795686500598,43.8206866123096,46.6946426775067));
#21574=CARTESIAN_POINT('Ctrl Pts',(40.9752752694262,43.8211010701009,46.6993300171964));
#21575=CARTESIAN_POINT('Ctrl Pts',(40.9603405142738,43.8225448662081,46.7157978603576));
#21576=CARTESIAN_POINT('Ctrl Pts',(40.9498211094351,43.8235655489159,46.7276887979375));
#21577=CARTESIAN_POINT('Ctrl Pts',(40.8599396168127,43.8323334603467,46.8318523969784));
#21578=CARTESIAN_POINT('Ctrl Pts',(40.7893164547205,43.8395559995996,46.9313271379131));
#21579=CARTESIAN_POINT('Ctrl Pts',(40.6814586929775,43.8524401583583,47.1184969720259));
#21580=CARTESIAN_POINT('Ctrl Pts',(40.6404386083731,43.8580679703413,47.2035241520015));
#21581=CARTESIAN_POINT('Ctrl Pts',(40.5868032419785,43.8670638828887,47.3392931371805));
#21582=CARTESIAN_POINT('Ctrl Pts',(40.5697481469518,43.8702994585477,47.3881229960178));
#21583=CARTESIAN_POINT('Ctrl Pts',(40.5502276297423,43.8745739027082,47.452170175346));
#21584=CARTESIAN_POINT('Ctrl Pts',(40.5459529064536,43.8755533413091,47.4668164558257));
#21585=CARTESIAN_POINT('Ctrl Pts',(40.5392627949576,43.8771605686069,47.4907923315399));
#21586=CARTESIAN_POINT('Ctrl Pts',(40.5367427427505,43.8777849354326,47.5000922249669));
#21587=CARTESIAN_POINT('Ctrl Pts',(40.5320079699338,43.8789958283477,47.5180985226308));
#21588=CARTESIAN_POINT('Ctrl Pts',(40.5297841856181,43.8795820425237,47.5268023020959));
#21589=CARTESIAN_POINT('Ctrl Pts',(40.5247905371157,43.8809400616988,47.5469323931288));
#21590=CARTESIAN_POINT('Ctrl Pts',(40.5220642015217,43.881713249832,47.5583690313814));
#21591=CARTESIAN_POINT('Ctrl Pts',(40.5137854507118,43.8841656192465,47.5945608943863));
#21592=CARTESIAN_POINT('Ctrl Pts',(40.5086169290759,43.8858569821936,47.6194002513415));
#21593=CARTESIAN_POINT('Ctrl Pts',(40.48182717801,43.8956329924862,47.7622164937813));
#21594=CARTESIAN_POINT('Ctrl Pts',(40.4707597676826,43.904048456566,47.8818850716964));
#21595=CARTESIAN_POINT('Ctrl Pts',(40.4709920943087,43.9219279601681,48.1327081996855));
#21596=CARTESIAN_POINT('Ctrl Pts',(40.4844403931585,43.9313714468035,48.2632860319756));
#21597=CARTESIAN_POINT('Ctrl Pts',(40.5142033584017,43.9413399992729,48.4068913570787));
#21598=CARTESIAN_POINT('Ctrl Pts',(40.5175808668798,43.9423997147379,48.4222413956722));
#21599=CARTESIAN_POINT('Ctrl Pts',(40.5225389177756,43.9438597933432,48.443531478295));
#21600=CARTESIAN_POINT('Ctrl Pts',(40.5239607021994,43.9442685483249,48.4495073338339));
#21601=CARTESIAN_POINT('Ctrl Pts',(40.5266052257117,43.9450109428346,48.4603913107921));
#21602=CARTESIAN_POINT('Ctrl Pts',(40.5278187706747,43.94534509744,48.4653016078481));
#21603=CARTESIAN_POINT('Ctrl Pts',(40.5303699830078,43.9460342273896,48.475452848679));
#21604=CARTESIAN_POINT('Ctrl Pts',(40.5317103964827,43.9463890431988,48.4806930111191));
#21605=CARTESIAN_POINT('Ctrl Pts',(40.5352666837976,43.9473119554533,48.4943562195065));
#21606=CARTESIAN_POINT('Ctrl Pts',(40.5375176211088,43.9478780697811,48.5027701340294));
#21607=CARTESIAN_POINT('Ctrl Pts',(40.5477724777889,43.9503802395638,48.5400881904193));
#21608=CARTESIAN_POINT('Ctrl Pts',(40.5563932912281,43.9522834667221,48.5688203482902));
#21609=CARTESIAN_POINT('Ctrl Pts',(40.5826649485588,43.9575918865548,48.6494954479266));
#21610=CARTESIAN_POINT('Ctrl Pts',(40.6018665558886,43.9609326955394,48.7009051404092));
#21611=CARTESIAN_POINT('Ctrl Pts',(40.6396821521477,43.9667802799114,48.7903205942545));
#21612=CARTESIAN_POINT('Ctrl Pts',(40.6574025647953,43.969300264196,48.8286614973622));
#21613=CARTESIAN_POINT('Ctrl Pts',(40.7373939556336,43.9799241627006,48.9877996358042));
#21614=CARTESIAN_POINT('Ctrl Pts',(40.811069001086,43.9880180878657,49.1024063658033));
#21615=CARTESIAN_POINT('Ctrl Pts',(40.9119972172458,43.9981789058822,49.2280183104509));
#21616=CARTESIAN_POINT('Ctrl Pts',(40.9282116708058,43.9997866312463,49.2474054158674));
#21617=CARTESIAN_POINT('Ctrl Pts',(40.9523906063301,44.0021522802368,49.2751875261074));
#21618=CARTESIAN_POINT('Ctrl Pts',(40.9600575903462,44.0028979438915,49.2838387868735));
#21619=CARTESIAN_POINT('Ctrl Pts',(40.9737998162352,44.0042269242847,49.2990672614106));
#21620=CARTESIAN_POINT('Ctrl Pts',(40.9798440171197,44.004808921621,49.3056721233109));
#21621=CARTESIAN_POINT('Ctrl Pts',(40.9925472469137,44.0060270394181,49.3193611443136));
#21622=CARTESIAN_POINT('Ctrl Pts',(40.9992142781201,44.0066634940976,49.3264374982621));
#21623=CARTESIAN_POINT('Ctrl Pts',(41.0167572925841,44.0083310244023,49.3447777986177));
#21624=CARTESIAN_POINT('Ctrl Pts',(41.0277172412236,44.0093657381083,49.3559600733581));
#21625=CARTESIAN_POINT('Ctrl Pts',(41.0784704061255,44.0141264708654,49.4064971859246));
#21626=CARTESIAN_POINT('Ctrl Pts',(41.1198248272775,44.017921718802,49.4442386385832));
#21627=CARTESIAN_POINT('Ctrl Pts',(41.2458654885061,44.0292586188345,49.5495964244485));
#21628=CARTESIAN_POINT('Ctrl Pts',(41.3346683030235,44.0369748263556,49.6119364515818));
#21629=CARTESIAN_POINT('Ctrl Pts',(41.5160905809453,44.0519778066981,49.7177290844786));
#21630=CARTESIAN_POINT('Ctrl Pts',(41.6078838972144,44.059235648291,49.7619435905247));
#21631=CARTESIAN_POINT('Ctrl Pts',(41.7181180814542,44.0672850269316,49.8046748981993));
#21632=CARTESIAN_POINT('Ctrl Pts',(41.7335686520541,44.0683984323564,49.8104374449469));
#21633=CARTESIAN_POINT('Ctrl Pts',(41.7551725661135,44.0699329204703,49.8181809214312));
#21634=CARTESIAN_POINT('Ctrl Pts',(41.761264320146,44.0703631547713,49.8203299197638));
#21635=CARTESIAN_POINT('Ctrl Pts',(41.7717856096138,44.0711018678385,49.8239822133983));
#21636=CARTESIAN_POINT('Ctrl Pts',(41.7762099821123,44.0714111850153,49.825500054735));
#21637=CARTESIAN_POINT('Ctrl Pts',(41.7851339228988,44.0720323508474,49.8285253023926));
#21638=CARTESIAN_POINT('Ctrl Pts',(41.7896335991051,44.0723441634992,49.8300322214975));
#21639=CARTESIAN_POINT('Ctrl Pts',(41.7941388317924,44.0726550104672,49.8315225365139));
#21640=CARTESIAN_POINT('Ctrl Pts',(41.7941385063105,44.2430936274184,49.8315224288456));
#21641=CARTESIAN_POINT('Ctrl Pts',(41.7396043809166,44.2390985684784,49.8134827225619));
#21642=CARTESIAN_POINT('Ctrl Pts',(41.6858775400372,44.2350409321712,49.7930079174364));
#21643=CARTESIAN_POINT('Ctrl Pts',(41.5524897688099,44.2246986259723,49.7352205757266));
#21644=CARTESIAN_POINT('Ctrl Pts',(41.4743401861913,44.2183834409544,49.6948209815617));
#21645=CARTESIAN_POINT('Ctrl Pts',(41.3476670832953,44.2079215730936,49.6179535927229));
#21646=CARTESIAN_POINT('Ctrl Pts',(41.29760689443,44.2037234975787,49.5842693549995));
#21647=CARTESIAN_POINT('Ctrl Pts',(41.2406316978823,44.1989385276753,49.5419214419756));
#21648=CARTESIAN_POINT('Ctrl Pts',(41.2321138654314,44.1982230057054,49.53547991934));
#21649=CARTESIAN_POINT('Ctrl Pts',(41.2190217033042,44.1971235299003,49.5254071314635));
#21650=CARTESIAN_POINT('Ctrl Pts',(41.2144097947295,44.1967362822372,49.5218253912312));
#21651=CARTESIAN_POINT('Ctrl Pts',(41.2058908338311,44.1960211926425,49.5151470911945));
#21652=CARTESIAN_POINT('Ctrl Pts',(41.2019795332078,44.1956929745052,49.5120563384701));
#21653=CARTESIAN_POINT('Ctrl Pts',(41.1930443539432,44.1949433550565,49.5049392257877));
#21654=CARTESIAN_POINT('Ctrl Pts',(41.1880286149247,44.1945226760866,49.5009028514761));
#21655=CARTESIAN_POINT('Ctrl Pts',(41.1748679765853,44.1934188970424,49.490202945857));
#21656=CARTESIAN_POINT('Ctrl Pts',(41.1667571001944,44.1927386677006,49.4834976429441));
#21657=CARTESIAN_POINT('Ctrl Pts',(41.0955846346437,44.1867657717694,49.4236718643789));
#21658=CARTESIAN_POINT('Ctrl Pts',(41.0359257461182,44.1817300279545,49.3666184424669));
#21659=CARTESIAN_POINT('Ctrl Pts',(40.9649099835989,44.175418843928,49.2894038944256));
#21660=CARTESIAN_POINT('Ctrl Pts',(40.9500136096402,44.1740754465618,49.272629266521));
#21661=CARTESIAN_POINT('Ctrl Pts',(40.8821675541652,44.167845645648,49.1934905513447));
#21662=CARTESIAN_POINT('Ctrl Pts',(40.8329271506569,44.1629955559193,49.1280591072135));
#21663=CARTESIAN_POINT('Ctrl Pts',(40.742098263753,44.1529974307122,48.9898908856949));
#21664=CARTESIAN_POINT('Ctrl Pts',(40.7007948009494,44.1478552448536,48.9171811423939));
#21665=CARTESIAN_POINT('Ctrl Pts',(40.6566815879319,44.1414239047763,48.8262511841174));
#21666=CARTESIAN_POINT('Ctrl Pts',(40.6492427093973,44.140300843664,48.8103696575544));
#21667=CARTESIAN_POINT('Ctrl Pts',(40.637850242419,44.1385172799369,48.7851582022315));
#21668=CARTESIAN_POINT('Ctrl Pts',(40.633751751813,44.1378617751561,48.7758945095482));
#21669=CARTESIAN_POINT('Ctrl Pts',(40.6262025635197,44.1366277126542,48.7584615019133));
#21670=CARTESIAN_POINT('Ctrl Pts',(40.6227348563843,44.1360497556231,48.750299807015));
#21671=CARTESIAN_POINT('Ctrl Pts',(40.6150819524767,44.1347488282835,48.7319369486293));
#21672=CARTESIAN_POINT('Ctrl Pts',(40.6109277242812,44.1340248289547,48.7217232965608));
#21673=CARTESIAN_POINT('Ctrl Pts',(40.6005524540698,44.1321699507473,48.6955743749994));
#21674=CARTESIAN_POINT('Ctrl Pts',(40.5944555058039,44.131034954445,48.6795912219813));
#21675=CARTESIAN_POINT('Ctrl Pts',(40.5482043034027,44.122056771913,48.553325976131));
#21676=CARTESIAN_POINT('Ctrl Pts',(40.5179846001232,44.1138830551309,48.4396885679311));
#21677=CARTESIAN_POINT('Ctrl Pts',(40.4799840558294,44.0978022847672,48.2166639866494));
#21678=CARTESIAN_POINT('Ctrl Pts',(40.4708152443879,44.0899511801632,48.107941920363));
#21679=CARTESIAN_POINT('Ctrl Pts',(40.470892390324,44.0792642431648,47.955174391841));
#21680=CARTESIAN_POINT('Ctrl Pts',(40.4724097294795,44.0762390376702,47.9113324877965));
#21681=CARTESIAN_POINT('Ctrl Pts',(40.4761166126907,44.072602088951,47.8574582923058));
#21682=CARTESIAN_POINT('Ctrl Pts',(40.4768926373583,44.0719228833635,47.8473451304902));
#21683=CARTESIAN_POINT('Ctrl Pts',(40.4782363620645,44.0708630782726,47.8314754460039));
#21684=CARTESIAN_POINT('Ctrl Pts',(40.4787502369596,44.070479613273,47.825714729279));
#21685=CARTESIAN_POINT('Ctrl Pts',(40.4797092734487,44.0698008980635,47.8154837068449));
#21686=CARTESIAN_POINT('Ctrl Pts',(40.4801441411887,44.0695050894838,47.8110126486227));
#21687=CARTESIAN_POINT('Ctrl Pts',(40.4812210748171,44.0688000360116,47.8003277305434));
#21688=CARTESIAN_POINT('Ctrl Pts',(40.4818777082651,44.0683916128377,47.7941154314454));
#21689=CARTESIAN_POINT('Ctrl Pts',(40.4839554061722,44.0671609518959,47.7753319779812));
#21690=CARTESIAN_POINT('Ctrl Pts',(40.4854699979236,44.0663437474693,47.7627712129868));
#21691=CARTESIAN_POINT('Ctrl Pts',(40.5001076258453,44.0590945534547,47.6506691373463));
#21692=CARTESIAN_POINT('Ctrl Pts',(40.5208614714453,44.0530386114581,47.552264448604));
#21693=CARTESIAN_POINT('Ctrl Pts',(40.593792426295,44.0375753268503,47.3041768244243));
#21694=CARTESIAN_POINT('Ctrl Pts',(40.6568812889464,44.0282546936184,47.1585207093695));
#21695=CARTESIAN_POINT('Ctrl Pts',(40.7490479257255,44.0167688779226,47.0017708137638));
#21696=CARTESIAN_POINT('Ctrl Pts',(40.7614356743688,44.0152593297112,46.9815643702612));
#21697=CARTESIAN_POINT('Ctrl Pts',(40.7803229166398,44.013004184184,46.9519931169555));
#21698=CARTESIAN_POINT('Ctrl Pts',(40.7865384954973,44.0122690801958,46.942448939493));
#21699=CARTESIAN_POINT('Ctrl Pts',(40.7977626646186,44.0109536966941,46.9255432323975));
#21700=CARTESIAN_POINT('Ctrl Pts',(40.8027384309435,44.0103746635257,46.9181602244851));
#21701=CARTESIAN_POINT('Ctrl Pts',(40.8133558779722,44.0091475041356,46.9026390558817));
#21702=CARTESIAN_POINT('Ctrl Pts',(40.8190094541697,44.0084989360779,46.894509385194));
#21703=CARTESIAN_POINT('Ctrl Pts',(40.8342442795958,44.0067638449538,46.8729580681041));
#21704=CARTESIAN_POINT('Ctrl Pts',(40.843935284495,44.0056731218927,46.8596153874515));
#21705=CARTESIAN_POINT('Ctrl Pts',(40.8934581210256,44.0001619490616,46.7932385307542));
#21706=CARTESIAN_POINT('Ctrl Pts',(40.9358309704575,43.9956424667775,46.7421649727376));
#21707=CARTESIAN_POINT('Ctrl Pts',(41.0867129800117,43.980164491468,46.5782765625424));
#21708=CARTESIAN_POINT('Ctrl Pts',(41.2062731361509,43.968806573042,46.476508076267));
#21709=CARTESIAN_POINT('Ctrl Pts',(41.3795019024677,43.9542145375196,46.3620911372923));
#21710=CARTESIAN_POINT('Ctrl Pts',(41.4233161831185,43.9506679324602,46.335592734507));
#21711=CARTESIAN_POINT('Ctrl Pts',(41.4774028104587,43.9465040608731,46.3057541561646));
#21712=CARTESIAN_POINT('Ctrl Pts',(41.4867112498932,43.9457948849207,46.3007183209059));
#21713=CARTESIAN_POINT('Ctrl Pts',(41.501258237666,43.9446986714798,46.2930025152234));
#21714=CARTESIAN_POINT('Ctrl Pts',(41.5064682295816,43.9443084499135,46.2902695692181));
#21715=CARTESIAN_POINT('Ctrl Pts',(41.516111693892,43.9435906767285,46.2852671276505));
#21716=CARTESIAN_POINT('Ctrl Pts',(41.5205414455149,43.9432627241665,46.2829909688371));
#21717=CARTESIAN_POINT('Ctrl Pts',(41.5306639730694,43.9425172703144,46.2778391179925));
#21718=CARTESIAN_POINT('Ctrl Pts',(41.5363622301048,43.9421004599446,46.2749744823581));
#21719=CARTESIAN_POINT('Ctrl Pts',(41.5540043644087,43.940818375033,46.266214735048));
#21720=CARTESIAN_POINT('Ctrl Pts',(41.5659954668941,43.9399587707146,46.2604148704296));
#21721=CARTESIAN_POINT('Ctrl Pts',(41.5942106864125,43.9379613872016,46.2471265332531));
#21722=CARTESIAN_POINT('Ctrl Pts',(41.6104809093452,43.936828929371,46.239738240181));
#21723=CARTESIAN_POINT('Ctrl Pts',(41.6687133144725,43.9328359275574,46.2142648480355));
#21724=CARTESIAN_POINT('Ctrl Pts',(41.7112148782668,43.9300313216531,46.1974446269455));
#21725=CARTESIAN_POINT('Ctrl Pts',(41.8827669088913,43.9189934961097,46.1365071921942));
#21726=CARTESIAN_POINT('Ctrl Pts',(42.0157339164397,43.9110340671312,46.104616951551));
#21727=CARTESIAN_POINT('Ctrl Pts',(42.2186752124673,43.8985663858154,46.078196792599));
#21728=CARTESIAN_POINT('Ctrl Pts',(42.286808694316,43.8943336019554,46.072983538407));
#21729=CARTESIAN_POINT('Ctrl Pts',(42.3721104073123,43.8889018105405,46.070996305141));
#21730=CARTESIAN_POINT('Ctrl Pts',(42.3891546993872,43.8878100300894,46.0708251936027));
#21731=CARTESIAN_POINT('Ctrl Pts',(42.4163180270974,43.8860588096875,46.0709124740152));
#21732=CARTESIAN_POINT('Ctrl Pts',(42.4264368854148,43.8854039583007,46.0710246125147));
#21733=CARTESIAN_POINT('Ctrl Pts',(42.4453371591557,43.8841759556817,46.0713828097941));
#21734=CARTESIAN_POINT('Ctrl Pts',(42.4541187185341,43.8836034356067,46.0716092500855));
#21735=CARTESIAN_POINT('Ctrl Pts',(42.4738922441569,43.8823097353178,46.0722542987999));
#21736=CARTESIAN_POINT('Ctrl Pts',(42.4848827167647,43.8815875040528,46.0727069584259));
#21737=CARTESIAN_POINT('Ctrl Pts',(42.5175444788061,43.8794314257994,46.0743320996273));
#21738=CARTESIAN_POINT('Ctrl Pts',(42.5391998942937,43.877989130819,46.0757762887909));
#21739=CARTESIAN_POINT('Ctrl Pts',(42.5886386083864,43.8746659511311,46.0799122391407));
#21740=CARTESIAN_POINT('Ctrl Pts',(42.6163965576802,43.872778013412,46.0828422265461));
#21741=CARTESIAN_POINT('Ctrl Pts',(42.7108900058775,43.8662743529486,46.0948947136178));
#21742=CARTESIAN_POINT('Ctrl Pts',(42.7772015130253,43.8615769427655,46.1069082975719));
#21743=CARTESIAN_POINT('Ctrl Pts',(42.9234178890359,43.850956840166,46.1413858726562));
#21744=CARTESIAN_POINT('Ctrl Pts',(43.0027805898271,43.8450107319942,46.1655879590356));
#21745=CARTESIAN_POINT('Ctrl Pts',(43.1598118098149,43.8330571387581,46.2247699007983));
#21746=CARTESIAN_POINT('Ctrl Pts',(43.2372314064008,43.8270649837217,46.2599417066109));
#21747=CARTESIAN_POINT('Ctrl Pts',(43.3213789463785,43.82061606856,46.3050915762605));
#21748=CARTESIAN_POINT('Ctrl Pts',(43.3306290300838,43.8199081243847,46.3101528624677));
#21749=CARTESIAN_POINT('Ctrl Pts',(43.345465030567,43.8187747914756,46.3184293178073));
#21750=CARTESIAN_POINT('Ctrl Pts',(43.3510769955171,43.8183465838505,46.3215969986883));
#21751=CARTESIAN_POINT('Ctrl Pts',(43.3610024518412,43.8175902679387,46.3272652031216));
#21752=CARTESIAN_POINT('Ctrl Pts',(43.3653222372219,43.8172614556712,46.329754391276));
#21753=CARTESIAN_POINT('Ctrl Pts',(43.3746768542666,43.8165501944101,46.3351932142708));
#21754=CARTESIAN_POINT('Ctrl Pts',(43.3797079769292,43.8161681448506,46.3381489578728));
#21755=CARTESIAN_POINT('Ctrl Pts',(43.3938912827197,43.8150922444615,46.3465683306048));
#21756=CARTESIAN_POINT('Ctrl Pts',(43.4030118766294,43.8144017353067,46.3520851493039));
#21757=CARTESIAN_POINT('Ctrl Pts',(43.4630022523947,43.8098656645753,46.3890544099371));
#21758=CARTESIAN_POINT('Ctrl Pts',(43.5124369929753,43.8061548070958,46.4227856938001));
#21759=CARTESIAN_POINT('Ctrl Pts',(43.6300530378476,43.7971859385698,46.5113259929496));
#21760=CARTESIAN_POINT('Ctrl Pts',(43.6962272156501,43.7920109907518,46.5685751417703));
#21761=CARTESIAN_POINT('Ctrl Pts',(43.8452587444114,43.779475606459,46.7163457783542));
#21762=CARTESIAN_POINT('Ctrl Pts',(43.92380328119,43.7720859501231,46.8106477428373));
#21763=CARTESIAN_POINT('Ctrl Pts',(44.0024487612938,43.7632293631749,46.9257614385125));
#21764=CARTESIAN_POINT('Ctrl Pts',(44.0118359322739,43.7621447488908,46.9398983927712));
#21765=CARTESIAN_POINT('Ctrl Pts',(44.0269902834931,43.7603465658684,46.9633873254915));
#21766=CARTESIAN_POINT('Ctrl Pts',(44.032866364946,43.7596370684299,46.9726681911334));
#21767=CARTESIAN_POINT('Ctrl Pts',(44.0433406826263,43.7583496625795,46.9895285549876));
#21768=CARTESIAN_POINT('Ctrl Pts',(44.0479665739168,43.7577727963455,46.9970905787663));
#21769=CARTESIAN_POINT('Ctrl Pts',(44.0577817747028,43.7565306615202,47.0133869257393));
#21770=CARTESIAN_POINT('Ctrl Pts',(44.0629545151425,43.7558648089082,47.0221308652526));
#21771=CARTESIAN_POINT('Ctrl Pts',(44.0769362061054,43.7540336284165,47.0461971466891));
#21772=CARTESIAN_POINT('Ctrl Pts',(44.0856038540458,43.7528632486421,47.0616000138322));
#21773=CARTESIAN_POINT('Ctrl Pts',(44.1353635423867,43.7459302643111,47.1529399073332));
#21774=CARTESIAN_POINT('Ctrl Pts',(44.1715260081066,43.7399953975201,47.2314368932607));
#21775=CARTESIAN_POINT('Ctrl Pts',(44.2476315743987,43.7250031603343,47.4308292315819));
#21776=CARTESIAN_POINT('Ctrl Pts',(44.2811064191148,43.715817018117,47.5537562068724));
#21777=CARTESIAN_POINT('Ctrl Pts',(44.3118394863456,43.7027851189303,47.7359243846737));
#21778=CARTESIAN_POINT('Ctrl Pts',(44.3188779749747,43.6987748366,47.7931792030661));
#21779=CARTESIAN_POINT('Ctrl Pts',(44.3241129056797,43.6942132499683,47.8606035209589));
#21780=CARTESIAN_POINT('Ctrl Pts',(44.3248072924222,43.6935448041562,47.8705444108917));
#21781=CARTESIAN_POINT('Ctrl Pts',(44.3258131360316,43.6924622958709,47.8867496155983));
#21782=CARTESIAN_POINT('Ctrl Pts',(44.3261711187319,43.6920457949093,47.8930107080291));
#21783=CARTESIAN_POINT('Ctrl Pts',(44.3267582758952,43.6913020052596,47.9042407013748));
#21784=CARTESIAN_POINT('Ctrl Pts',(44.3269987707252,43.6909741042078,47.9092088310919));
#21785=CARTESIAN_POINT('Ctrl Pts',(44.3274855348091,43.6902551967842,47.9201396151387));
#21786=CARTESIAN_POINT('Ctrl Pts',(44.3277233543404,43.6898646634689,47.9261025070023));
#21787=CARTESIAN_POINT('Ctrl Pts',(44.3283308542687,43.688739996444,47.943343184428));
#21788=CARTESIAN_POINT('Ctrl Pts',(44.3286292704426,43.6880097017303,47.9546234610542));
#21789=CARTESIAN_POINT('Ctrl Pts',(44.3302423000544,43.682141972275,48.0458788371182));
#21790=CARTESIAN_POINT('Ctrl Pts',(44.3266809532286,43.6772467427395,48.1258728991357));
#21791=CARTESIAN_POINT('Ctrl Pts',(44.3134586082108,43.6697669502737,48.2493376308208));
#21792=CARTESIAN_POINT('Ctrl Pts',(44.3072489656745,43.6671322529295,48.2930778549741));
#21793=CARTESIAN_POINT('Ctrl Pts',(44.2761556763671,43.6565024838846,48.4685645688254));
#21794=CARTESIAN_POINT('Ctrl Pts',(44.2390770143016,43.6485104838561,48.5977484454606));
#21795=CARTESIAN_POINT('Ctrl Pts',(44.1794290439232,43.6384619120511,48.7455310813909));
#21796=CARTESIAN_POINT('Ctrl Pts',(44.1694859274379,43.636850407855,48.768832733965));
#21797=CARTESIAN_POINT('Ctrl Pts',(44.1543381675142,43.6344803498472,48.8024798959907));
#21798=CARTESIAN_POINT('Ctrl Pts',(44.1494944116956,43.6337341251294,48.8129856599655));
#21799=CARTESIAN_POINT('Ctrl Pts',(44.1407353023115,43.6324046412208,48.8315427266547));
#21800=CARTESIAN_POINT('Ctrl Pts',(44.1368578101212,43.6318227067984,48.8396116017844));
#21801=CARTESIAN_POINT('Ctrl Pts',(44.1286561801086,43.6306052267388,48.8563788437636));
#21802=CARTESIAN_POINT('Ctrl Pts',(44.1243222328192,43.6299693506033,48.8650721037106));
#21803=CARTESIAN_POINT('Ctrl Pts',(44.1128454799523,43.6283044754593,48.8876638446211));
#21804=CARTESIAN_POINT('Ctrl Pts',(44.1055992480987,43.6272718578881,48.9015086907929));
#21805=CARTESIAN_POINT('Ctrl Pts',(44.0717820977166,43.6225343157168,48.9642532402107));
#21806=CARTESIAN_POINT('Ctrl Pts',(44.0432734267204,43.6187609802245,49.0120726617762));
#21807=CARTESIAN_POINT('Ctrl Pts',(43.9539045223643,43.6075241113913,49.1482244551945));
#21808=CARTESIAN_POINT('Ctrl Pts',(43.8877043217979,43.5998899468667,49.2327894441272));
#21809=CARTESIAN_POINT('Ctrl Pts',(43.7446787911724,43.5848593983462,49.3870945477004));
#21810=CARTESIAN_POINT('Ctrl Pts',(43.6685586271243,43.5774915480332,49.4570365471399));
#21811=CARTESIAN_POINT('Ctrl Pts',(43.5742072607798,43.5693416658177,49.5307029889878));
#21812=CARTESIAN_POINT('Ctrl Pts',(43.561083112113,43.5682284851432,49.5406817916319));
#21813=CARTESIAN_POINT('Ctrl Pts',(43.5426417328059,43.5666943274142,49.5543339834343));
#21814=CARTESIAN_POINT('Ctrl Pts',(43.5374319833061,43.5662642019595,49.5581504253169));
#21815=CARTESIAN_POINT('Ctrl Pts',(43.5284170179191,43.5655256839152,49.5646850981975));
#21816=CARTESIAN_POINT('Ctrl Pts',(43.5246209434617,43.5652164532757,49.5674157577201));
#21817=CARTESIAN_POINT('Ctrl Pts',(43.5166001163627,43.5645668129532,49.573141301285));
#21818=CARTESIAN_POINT('Ctrl Pts',(43.5123731681496,43.5642266311973,49.5761330240599));
#21819=CARTESIAN_POINT('Ctrl Pts',(43.5018729310297,43.5633868186809,49.5835015344439));
#21820=CARTESIAN_POINT('Ctrl Pts',(43.4955854759229,43.562888546501,49.587858159757));
#21821=CARTESIAN_POINT('Ctrl Pts',(43.4718977907813,43.5610278414858,49.6040638515419));
#21822=CARTESIAN_POINT('Ctrl Pts',(43.4543291698906,43.5596809891024,49.6156657461265));
#21823=CARTESIAN_POINT('Ctrl Pts',(43.3159409335616,43.5492983452555,49.7038350541132));
#21824=CARTESIAN_POINT('Ctrl Pts',(43.187118939986,43.5409358818335,49.7670473995798));
#21825=CARTESIAN_POINT('Ctrl Pts',(42.9477406500279,43.5257104959986,49.8530810500426));
#21826=CARTESIAN_POINT('Ctrl Pts',(42.8399578479711,43.5189586897117,49.881584824778));
#21827=CARTESIAN_POINT('Ctrl Pts',(42.7135155694936,43.5108068347728,49.9035602775646));
#21828=CARTESIAN_POINT('Ctrl Pts',(42.6966658470497,43.509716278299,49.9062589247028));
#21829=CARTESIAN_POINT('Ctrl Pts',(42.668886008522,43.5079102735847,49.9103309049066));
#21830=CARTESIAN_POINT('Ctrl Pts',(42.6579757671994,43.5071989591367,49.9118348116516));
#21831=CARTESIAN_POINT('Ctrl Pts',(42.6382595782198,43.505909608294,49.9143807227299));
#21832=CARTESIAN_POINT('Ctrl Pts',(42.6294581275232,43.5053326285677,49.9154555963193));
#21833=CARTESIAN_POINT('Ctrl Pts',(42.610577385004,43.5040917509735,49.9176294006394));
#21834=CARTESIAN_POINT('Ctrl Pts',(42.6004962501935,43.5034272801634,49.9187096185345));
#21835=CARTESIAN_POINT('Ctrl Pts',(42.5729143611864,43.5016038194823,49.9214453391665));
#21836=CARTESIAN_POINT('Ctrl Pts',(42.5553991093112,43.5004398486277,49.9229411456379));
#21837=CARTESIAN_POINT('Ctrl Pts',(42.453703013485,43.4936448672338,49.9302275443369));
#21838=CARTESIAN_POINT('Ctrl Pts',(42.3692466707364,43.4878497115731,49.9307286396926));
#21839=CARTESIAN_POINT('Ctrl Pts',(42.1721038684476,43.4739896791129,49.9189595077675));
#21840=CARTESIAN_POINT('Ctrl Pts',(42.0599847530573,43.465843539056,49.9022957655123));
#21841=CARTESIAN_POINT('Ctrl Pts',(41.8974319923271,43.453975712517,49.8633003986517));
#21842=CARTESIAN_POINT('Ctrl Pts',(41.8454383540773,43.4501740579362,49.8484922372584));
#21843=CARTESIAN_POINT('Ctrl Pts',(41.7941388168303,43.4464579097838,49.8315225315644));
#21844=CARTESIAN_POINT('Origin',(42.4,48.4493818343519,48.));
#21845=CARTESIAN_POINT('',(41.7941388473837,42.4816651137235,49.8315225416714));
#21846=CARTESIAN_POINT('',(41.7941387803776,42.6541583936299,49.831522519506));
#21847=CARTESIAN_POINT('',(41.7941388317924,48.4493818343519,49.8315225365138));
#21848=CARTESIAN_POINT('',(40.4708700154104,43.1171846258035,47.9997561613629));
#21849=CARTESIAN_POINT('Ctrl Pts',(41.7941388473837,42.4816651137235,49.8315225416714));
#21850=CARTESIAN_POINT('Ctrl Pts',(41.8064630223161,42.482483011755,49.835599334973));
#21851=CARTESIAN_POINT('Ctrl Pts',(41.818829501791,42.4833047422321,49.8395521181629));
#21852=CARTESIAN_POINT('Ctrl Pts',(41.8482097833632,42.4852602051173,49.8486172222061));
#21853=CARTESIAN_POINT('Ctrl Pts',(41.8652541673143,42.4863971510643,49.8536194156301));
#21854=CARTESIAN_POINT('Ctrl Pts',(41.8922720476968,42.4882044730286,49.8611449844618));
#21855=CARTESIAN_POINT('Ctrl Pts',(41.9022010913276,42.4888697366671,49.8638252510529));
#21856=CARTESIAN_POINT('Ctrl Pts',(41.9207205486733,42.4901127853861,49.8686658931034));
#21857=CARTESIAN_POINT('Ctrl Pts',(41.9293053652268,42.4906898883104,49.8708467518466));
#21858=CARTESIAN_POINT('Ctrl Pts',(41.9484177902461,42.4919767901498,49.8755621332616));
#21859=CARTESIAN_POINT('Ctrl Pts',(41.9589522682066,42.4926875174423,49.8780672772906));
#21860=CARTESIAN_POINT('Ctrl Pts',(41.9898249471174,42.4947747934622,49.8851348578991));
#21861=CARTESIAN_POINT('Ctrl Pts',(42.0102161316325,42.496158999751,49.8894563991354));
#21862=CARTESIAN_POINT('Ctrl Pts',(42.1556092623919,42.506071652407,49.9178161415338));
#21863=CARTESIAN_POINT('Ctrl Pts',(42.2826279827468,42.5149879083897,49.9297560378969));
#21864=CARTESIAN_POINT('Ctrl Pts',(42.5410790763416,42.533410577361,49.9284331585886));
#21865=CARTESIAN_POINT('Ctrl Pts',(42.6718821183329,42.5428755706923,49.914377978479));
#21866=CARTESIAN_POINT('Ctrl Pts',(42.8156057942993,42.5528617198913,49.8838950852006));
#21867=CARTESIAN_POINT('Ctrl Pts',(42.8309188965244,42.5539199469981,49.8804514914747));
#21868=CARTESIAN_POINT('Ctrl Pts',(42.8521615097783,42.5553783311235,49.8754013476342));
#21869=CARTESIAN_POINT('Ctrl Pts',(42.8581274511205,42.5557868551339,49.8739529040816));
#21870=CARTESIAN_POINT('Ctrl Pts',(42.8689950331896,42.5565289618442,49.8712594127245));
#21871=CARTESIAN_POINT('Ctrl Pts',(42.8738988856499,42.55686305821,49.8700235237476));
#21872=CARTESIAN_POINT('Ctrl Pts',(42.8840389987243,42.5575522307446,49.8674255209777));
#21873=CARTESIAN_POINT('Ctrl Pts',(42.8892744601708,42.5579071462862,49.866060645613));
#21874=CARTESIAN_POINT('Ctrl Pts',(42.9029295318001,42.5588306151888,49.8624393739717));
#21875=CARTESIAN_POINT('Ctrl Pts',(42.9113398282644,42.5593971820126,49.8601478765829));
#21876=CARTESIAN_POINT('Ctrl Pts',(42.9486849695732,42.5619043257611,49.8497002694421));
#21877=CARTESIAN_POINT('Ctrl Pts',(42.9774441082996,42.5638119138052,49.840924991343));
#21878=CARTESIAN_POINT('Ctrl Pts',(43.0582494066556,42.5691367100614,49.8141886655199));
#21879=CARTESIAN_POINT('Ctrl Pts',(43.1097504510469,42.5724890569018,49.7946665351987));
#21880=CARTESIAN_POINT('Ctrl Pts',(43.1964598878373,42.5781711377423,49.7574805842364));
#21881=CARTESIAN_POINT('Ctrl Pts',(43.23208958716,42.5805173647586,49.7408944211078));
#21882=CARTESIAN_POINT('Ctrl Pts',(43.3910934682799,42.5911362585437,49.6608782824261));
#21883=CARTESIAN_POINT('Ctrl Pts',(43.507897169724,42.599387191362,49.5853520924081));
#21884=CARTESIAN_POINT('Ctrl Pts',(43.6351270256294,42.6097204451805,49.4821055622656));
#21885=CARTESIAN_POINT('Ctrl Pts',(43.6543521249132,42.6113212602249,49.4658704991461));
#21886=CARTESIAN_POINT('Ctrl Pts',(43.6819227125147,42.613678607839,49.4416483203481));
#21887=CARTESIAN_POINT('Ctrl Pts',(43.6905232361527,42.6144230043342,49.4339544929466));
#21888=CARTESIAN_POINT('Ctrl Pts',(43.7056707729474,42.6157505314537,49.42015720745));
#21889=CARTESIAN_POINT('Ctrl Pts',(43.7122453637348,42.6163323526687,49.4140844253525));
#21890=CARTESIAN_POINT('Ctrl Pts',(43.725880055521,42.6175509224679,49.4013134348597));
#21891=CARTESIAN_POINT('Ctrl Pts',(43.7329321885743,42.6181880110101,49.3946071271564));
#21892=CARTESIAN_POINT('Ctrl Pts',(43.7512285187791,42.6198590490037,49.3769424676549));
#21893=CARTESIAN_POINT('Ctrl Pts',(43.7623900170183,42.6208966648458,49.3658998813309));
#21894=CARTESIAN_POINT('Ctrl Pts',(43.8130568548912,42.6256926970787,49.3145339353961));
#21895=CARTESIAN_POINT('Ctrl Pts',(43.8509115752256,42.629521613006,49.2726286309728));
#21896=CARTESIAN_POINT('Ctrl Pts',(43.9569880798478,42.6410150481259,49.1443082197007));
#21897=CARTESIAN_POINT('Ctrl Pts',(44.0197109432773,42.6488604211206,49.0536530190111));
#21898=CARTESIAN_POINT('Ctrl Pts',(44.1237531765662,42.6638239032473,48.8718416577719));
#21899=CARTESIAN_POINT('Ctrl Pts',(44.1664044254,42.6709132787453,48.7818262140145));
#21900=CARTESIAN_POINT('Ctrl Pts',(44.2078072408997,42.6788065946554,48.6735330225806));
#21901=CARTESIAN_POINT('Ctrl Pts',(44.2134912060516,42.6799185687593,48.6580755600456));
#21902=CARTESIAN_POINT('Ctrl Pts',(44.2211270870521,42.6814514089007,48.6364592440801));
#21903=CARTESIAN_POINT('Ctrl Pts',(44.2232468848637,42.6818814019582,48.6303610365154));
#21904=CARTESIAN_POINT('Ctrl Pts',(44.2268493476047,42.6826198129632,48.6198273047643));
#21905=CARTESIAN_POINT('Ctrl Pts',(44.2283465546226,42.6829290677816,48.6153968670267));
#21906=CARTESIAN_POINT('Ctrl Pts',(44.2314685482322,42.6835789063445,48.6060464984561));
#21907=CARTESIAN_POINT('Ctrl Pts',(44.2330896510122,42.6839192611931,48.601125389497));
#21908=CARTESIAN_POINT('Ctrl Pts',(44.2370573240605,42.6847597576228,48.5889155922338));
#21909=CARTESIAN_POINT('Ctrl Pts',(44.2393803946537,42.685258536684,48.5816192528417));
#21910=CARTESIAN_POINT('Ctrl Pts',(44.247941034534,42.6871227609294,48.5541675070197));
#21911=CARTESIAN_POINT('Ctrl Pts',(44.2538915288623,42.688472552249,48.533923197382));
#21912=CARTESIAN_POINT('Ctrl Pts',(44.2978072444465,42.6989094084934,48.3749197776708));
#21913=CARTESIAN_POINT('Ctrl Pts',(44.320480197986,42.7073159210129,48.232387985803));
#21914=CARTESIAN_POINT('Ctrl Pts',(44.3321664322069,42.722541611044,47.978335406385));
#21915=CARTESIAN_POINT('Ctrl Pts',(44.3277596444973,42.7292435571353,47.8678089781625));
#21916=CARTESIAN_POINT('Ctrl Pts',(44.3117883733165,42.7373398321595,47.7413521500286));
#21917=CARTESIAN_POINT('Ctrl Pts',(44.3094268111809,42.7384299325873,47.72445922697));
#21918=CARTESIAN_POINT('Ctrl Pts',(44.3051723834534,42.7402354464551,47.6967146062724));
#21919=CARTESIAN_POINT('Ctrl Pts',(44.3034099956255,42.7409467318035,47.6858436361289));
#21920=CARTESIAN_POINT('Ctrl Pts',(44.3000604084328,42.7422362081907,47.6662461024846));
#21921=CARTESIAN_POINT('Ctrl Pts',(44.2985059111952,42.7428133438314,47.6575142038897));
#21922=CARTESIAN_POINT('Ctrl Pts',(44.2950444127382,42.7440547564853,47.638818406935));
#21923=CARTESIAN_POINT('Ctrl Pts',(44.2931189243271,42.74471960824,47.6288582466368));
#21924=CARTESIAN_POINT('Ctrl Pts',(44.2876389165738,42.7465446414545,47.6016640647011));
#21925=CARTESIAN_POINT('Ctrl Pts',(44.2839270831589,42.7477098162639,47.58446310994));
#21926=CARTESIAN_POINT('Ctrl Pts',(44.2609892347393,42.7545257504976,47.484799866778));
#21927=CARTESIAN_POINT('Ctrl Pts',(44.2365886640935,42.7603418541486,47.4036355026783));
#21928=CARTESIAN_POINT('Ctrl Pts',(44.1667398428654,42.7743399988669,47.2168350097494));
#21929=CARTESIAN_POINT('Ctrl Pts',(44.117025452517,42.7826083957699,47.1131302550583));
#21930=CARTESIAN_POINT('Ctrl Pts',(44.0401625750332,42.7932829239806,46.9837899621869));
#21931=CARTESIAN_POINT('Ctrl Pts',(44.0210826420139,42.7957991132616,46.9536217668829));
#21932=CARTESIAN_POINT('Ctrl Pts',(43.9798584843873,42.8009476791142,46.892276905242));
#21933=CARTESIAN_POINT('Ctrl Pts',(43.9576012310408,42.8035745978824,46.8611926597074));
#21934=CARTESIAN_POINT('Ctrl Pts',(43.9284785441651,42.8068078953192,46.8229730549326));
#21935=CARTESIAN_POINT('Ctrl Pts',(43.9224639535176,42.8074653514169,46.815203557688));
#21936=CARTESIAN_POINT('Ctrl Pts',(43.9128942978015,42.8084948916057,46.8030349289609));
#21937=CARTESIAN_POINT('Ctrl Pts',(43.9093788994098,42.8088696519123,46.7986050284478));
#21938=CARTESIAN_POINT('Ctrl Pts',(43.9027059310309,42.8095744652772,46.7902716638738));
#21939=CARTESIAN_POINT('Ctrl Pts',(43.8995526296431,42.8099047869644,46.7863650985981));
#21940=CARTESIAN_POINT('Ctrl Pts',(43.8921279384753,42.8106762528692,46.7772399057708));
#21941=CARTESIAN_POINT('Ctrl Pts',(43.8878443922079,42.8111165167494,46.7720313111644));
#21942=CARTESIAN_POINT('Ctrl Pts',(43.8737599049004,42.8125488809768,46.7550871212149));
#21943=CARTESIAN_POINT('Ctrl Pts',(43.8638464552114,42.8135332301481,46.7434452164594));
#21944=CARTESIAN_POINT('Ctrl Pts',(43.808414130964,42.8189157287396,46.6798945131296));
#21945=CARTESIAN_POINT('Ctrl Pts',(43.760267661785,42.823148195664,46.6303347779063));
#21946=CARTESIAN_POINT('Ctrl Pts',(43.6210540467661,42.8345930374396,46.5016347278824));
#21947=CARTESIAN_POINT('Ctrl Pts',(43.525072526141,42.8416630246131,46.4282862707686));
#21948=CARTESIAN_POINT('Ctrl Pts',(43.3594117468947,42.8535227856353,46.3246869083624));
#21949=CARTESIAN_POINT('Ctrl Pts',(43.2937017392239,42.8581464911346,46.2887314308566));
#21950=CARTESIAN_POINT('Ctrl Pts',(43.2102812569007,42.8640196517993,46.2492023898993));
#21951=CARTESIAN_POINT('Ctrl Pts',(43.1943875344759,42.8651385908506,46.241933903511));
#21952=CARTESIAN_POINT('Ctrl Pts',(43.1690469699447,42.8669235979914,46.2307589892593));
#21953=CARTESIAN_POINT('Ctrl Pts',(43.1596638104627,42.8675847658357,46.2267098701942));
#21954=CARTESIAN_POINT('Ctrl Pts',(43.1420845385212,42.8688240642544,46.2192890091701));
#21955=CARTESIAN_POINT('Ctrl Pts',(43.1338964723469,42.8694015471476,46.2158988093074));
#21956=CARTESIAN_POINT('Ctrl Pts',(43.1155758638925,42.870694335968,46.2084607763376));
#21957=CARTESIAN_POINT('Ctrl Pts',(43.1054318185329,42.8714106119728,46.2044422738388));
#21958=CARTESIAN_POINT('Ctrl Pts',(43.0754312418341,42.8735306290427,46.1928511928368));
#21959=CARTESIAN_POINT('Ctrl Pts',(43.0554835867018,42.8749423978768,46.1855206312639));
#21960=CARTESIAN_POINT('Ctrl Pts',(42.9002203639791,42.8859514841693,46.1313573344985));
#21961=CARTESIAN_POINT('Ctrl Pts',(42.7602161300534,42.8960487230764,46.0994014203309));
#21962=CARTESIAN_POINT('Ctrl Pts',(42.5053847581452,42.9143663694379,46.0704192086731));
#21963=CARTESIAN_POINT('Ctrl Pts',(42.3918532351142,42.9224898657566,46.0675594961786));
#21964=CARTESIAN_POINT('Ctrl Pts',(42.2625137749523,42.9313100999593,46.0757069478478));
#21965=CARTESIAN_POINT('Ctrl Pts',(42.2463212854115,42.9324062335398,46.0769323704122));
#21966=CARTESIAN_POINT('Ctrl Pts',(42.2237530503901,42.9339208920289,46.078927186937));
#21967=CARTESIAN_POINT('Ctrl Pts',(42.2173632876267,42.9343482729947,46.0795241281049));
#21968=CARTESIAN_POINT('Ctrl Pts',(42.2063322541284,42.9350834170212,46.0806102169387));
#21969=CARTESIAN_POINT('Ctrl Pts',(42.2016896094386,42.9353920003094,46.0810843360712));
#21970=CARTESIAN_POINT('Ctrl Pts',(42.191885273169,42.9360418733012,46.082121542847));
#21971=CARTESIAN_POINT('Ctrl Pts',(42.18672404891,42.9363829260291,46.0826886309725));
#21972=CARTESIAN_POINT('Ctrl Pts',(42.1739040138135,42.937227587697,46.084149636133));
#21973=CARTESIAN_POINT('Ctrl Pts',(42.1662480526417,42.937729804059,46.0850686582135));
#21974=CARTESIAN_POINT('Ctrl Pts',(42.1372798205406,42.9396224125798,46.0887223269825));
#21975=CARTESIAN_POINT('Ctrl Pts',(42.1160073187364,42.9409965285494,46.0917671823678));
#21976=CARTESIAN_POINT('Ctrl Pts',(42.0614196160911,42.9444924872656,46.1005137564378));
#21977=CARTESIAN_POINT('Ctrl Pts',(42.0281944181947,42.9465912712206,46.1067368003444));
#21978=CARTESIAN_POINT('Ctrl Pts',(41.9019273335135,42.9545142015236,46.1338390643839));
#21979=CARTESIAN_POINT('Ctrl Pts',(41.810312831732,42.9601567612324,46.1607326924264));
#21980=CARTESIAN_POINT('Ctrl Pts',(41.6044397705594,42.9732894552609,46.2381404684115));
#21981=CARTESIAN_POINT('Ctrl Pts',(41.4923596724948,42.9807983524011,46.2931759880739));
#21982=CARTESIAN_POINT('Ctrl Pts',(41.3705879936912,42.9898893550905,46.3683757352764));
#21983=CARTESIAN_POINT('Ctrl Pts',(41.3549432338029,42.9910758019406,46.3783517221726));
#21984=CARTESIAN_POINT('Ctrl Pts',(41.330639386907,42.9929494413156,46.3943469969767));
#21985=CARTESIAN_POINT('Ctrl Pts',(41.3218813497263,42.9936309571743,46.400214434503));
#21986=CARTESIAN_POINT('Ctrl Pts',(41.3060331481791,42.9948760279561,46.4110211633118));
#21987=CARTESIAN_POINT('Ctrl Pts',(41.2989271978326,42.9954386782114,46.4159369025948));
#21988=CARTESIAN_POINT('Ctrl Pts',(41.2915315015136,42.9960289460104,46.421126889021));
#21989=CARTESIAN_POINT('Ctrl Pts',(41.2912084655882,42.9960547376362,46.4213537299554));
#21990=CARTESIAN_POINT('Ctrl Pts',(41.2905851640724,42.9961045209791,46.4217917078338));
#21991=CARTESIAN_POINT('Ctrl Pts',(41.2902848890574,42.9961285121799,46.4220028313765));
#21992=CARTESIAN_POINT('Ctrl Pts',(41.2897027831224,42.9961750366911,46.4224123587304));
#21993=CARTESIAN_POINT('Ctrl Pts',(41.2894209450126,42.9961975696148,46.4226107524406));
#21994=CARTESIAN_POINT('Ctrl Pts',(41.2888723150507,42.9962414464674,46.4229971683064));
#21995=CARTESIAN_POINT('Ctrl Pts',(41.2886055177166,42.9962627900947,46.4231851826609));
#21996=CARTESIAN_POINT('Ctrl Pts',(41.2880842408237,42.9963045045029,46.4235527289544));
#21997=CARTESIAN_POINT('Ctrl Pts',(41.2878297569839,42.9963248750503,46.4237322548371));
#21998=CARTESIAN_POINT('Ctrl Pts',(41.287330871325,42.9963648206045,46.4240843751918));
#21999=CARTESIAN_POINT('Ctrl Pts',(41.2870864661852,42.9963843954257,46.4242569648979));
#22000=CARTESIAN_POINT('Ctrl Pts',(41.2866058715751,42.9964228977067,46.4245965103033));
#22001=CARTESIAN_POINT('Ctrl Pts',(41.2863696794509,42.9964418250248,46.4247634622974));
#22002=CARTESIAN_POINT('Ctrl Pts',(41.2859039247204,42.9964791583864,46.4250928373308));
#22003=CARTESIAN_POINT('Ctrl Pts',(41.2856743600918,42.996497564315,46.4252552574391));
#22004=CARTESIAN_POINT('Ctrl Pts',(41.2852204896007,42.9965339640057,46.42557652595));
#22005=CARTESIAN_POINT('Ctrl Pts',(41.2849961820487,42.9965519576894,46.4257353721817));
#22006=CARTESIAN_POINT('Ctrl Pts',(41.2845516204484,42.9965876289632,46.4260503367831));
#22007=CARTESIAN_POINT('Ctrl Pts',(41.2843313652555,42.9966053064839,46.4262064534278));
#22008=CARTESIAN_POINT('Ctrl Pts',(41.2838938314484,42.9966404314073,46.426516714931));
#22009=CARTESIAN_POINT('Ctrl Pts',(41.2836765520593,42.9966578787562,46.4266708585142));
#22010=CARTESIAN_POINT('Ctrl Pts',(41.2742044384064,42.9974186691157,46.4333935693888));
#22011=CARTESIAN_POINT('Ctrl Pts',(41.2650078885551,42.9981651442654,46.4400435094194));
#22012=CARTESIAN_POINT('Ctrl Pts',(41.2453618047822,42.9997769446754,46.4545151066457));
#22013=CARTESIAN_POINT('Ctrl Pts',(41.2349319553795,43.0006432467611,46.462362411183));
#22014=CARTESIAN_POINT('Ctrl Pts',(41.1483491824757,43.0079253367884,46.5288930173265));
#22015=CARTESIAN_POINT('Ctrl Pts',(41.0766131644606,43.0145608886104,46.593078650251));
#22016=CARTESIAN_POINT('Ctrl Pts',(40.9286095496375,43.0296205056926,46.7468761745433));
#22017=CARTESIAN_POINT('Ctrl Pts',(40.8551378749106,43.0380906247425,46.8386608009726));
#22018=CARTESIAN_POINT('Ctrl Pts',(40.7590899929671,43.0503765464944,46.9840297805876));
#22019=CARTESIAN_POINT('Ctrl Pts',(40.7298316237233,43.0543335495474,47.0328805340369));
#22020=CARTESIAN_POINT('Ctrl Pts',(40.6980501352524,43.0588429169013,47.0917005152954));
#22021=CARTESIAN_POINT('Ctrl Pts',(40.6933940371286,43.0595094574922,47.1004793533341));
#22022=CARTESIAN_POINT('Ctrl Pts',(40.6859138250224,43.0605895713322,47.1148500830018));
#22023=CARTESIAN_POINT('Ctrl Pts',(40.6830488155163,43.0610055648211,47.1204203142092));
#22024=CARTESIAN_POINT('Ctrl Pts',(40.6779570038355,43.0617489135434,47.1304396358338));
#22025=CARTESIAN_POINT('Ctrl Pts',(40.675720241656,43.0620768765117,47.1348834620457));
#22026=CARTESIAN_POINT('Ctrl Pts',(40.6708338981159,43.0627964791208,47.1446855098964));
#22027=CARTESIAN_POINT('Ctrl Pts',(40.6681920168422,43.0631876410548,47.1500474150047));
#22028=CARTESIAN_POINT('Ctrl Pts',(40.6606167884098,43.0643156220048,47.1656038928636));
#22029=CARTESIAN_POINT('Ctrl Pts',(40.6557481378535,43.065048568306,47.1758299467089));
#22030=CARTESIAN_POINT('Ctrl Pts',(40.6164593051054,43.0710349805492,47.260259532205));
#22031=CARTESIAN_POINT('Ctrl Pts',(40.5866959650059,43.076035075355,47.3365504427054));
#22032=CARTESIAN_POINT('Ctrl Pts',(40.5105069092393,43.0911449539596,47.5757446024541));
#22033=CARTESIAN_POINT('Ctrl Pts',(40.4805893457751,43.1010078668195,47.7430221298709));
#22034=CARTESIAN_POINT('Ctrl Pts',(40.4720391729479,43.1127741992305,47.9303851764094));
#22035=CARTESIAN_POINT('Ctrl Pts',(40.4714643159154,43.1139324325308,47.9487237418962));
#22036=CARTESIAN_POINT('Ctrl Pts',(40.470965094922,43.1157911205326,47.9779627812974));
#22037=CARTESIAN_POINT('Ctrl Pts',(40.4708713927328,43.1164864610854,47.9888594717965));
#22038=CARTESIAN_POINT('Ctrl Pts',(40.4708700154104,43.1171846258035,47.9997561613629));
#22039=CARTESIAN_POINT('Ctrl Pts',(40.4708700152961,43.1171846838461,47.9997570672691));
#22040=CARTESIAN_POINT('Ctrl Pts',(40.4708691867194,43.1176062557005,48.0063367990707));
#22041=CARTESIAN_POINT('Ctrl Pts',(40.4709020206306,43.1180288511859,48.0129164416807));
#22042=CARTESIAN_POINT('Ctrl Pts',(40.4710492573248,43.1189669100671,48.0274849697494));
#22043=CARTESIAN_POINT('Ctrl Pts',(40.4711796306079,43.1194828568839,48.0354735207403));
#22044=CARTESIAN_POINT('Ctrl Pts',(40.471550273897,43.1205484984144,48.0519213408788));
#22045=CARTESIAN_POINT('Ctrl Pts',(40.4717965903867,43.1210983704599,48.0603802871184));
#22046=CARTESIAN_POINT('Ctrl Pts',(40.4724376332605,43.1222694301181,48.0783337627932));
#22047=CARTESIAN_POINT('Ctrl Pts',(40.4728468721927,43.1228910588557,48.0878275159865));
#22048=CARTESIAN_POINT('Ctrl Pts',(40.4740376087615,43.1244407069268,48.1114014448298));
#22049=CARTESIAN_POINT('Ctrl Pts',(40.4749033753785,43.1253713453995,48.1254766201613));
#22050=CARTESIAN_POINT('Ctrl Pts',(40.4788213904405,43.1289648396312,48.1795007139328));
#22051=CARTESIAN_POINT('Ctrl Pts',(40.48296337304,43.1316614393306,48.2193579752236));
#22052=CARTESIAN_POINT('Ctrl Pts',(40.5089853044917,43.1448817626614,48.411382869605));
#22053=CARTESIAN_POINT('Ctrl Pts',(40.547758894432,43.155920687225,48.5606788678566));
#22054=CARTESIAN_POINT('Ctrl Pts',(40.6315878158932,43.172280749307,48.7746319405569));
#22055=CARTESIAN_POINT('Ctrl Pts',(40.6635289140438,43.1776496924322,48.8438049889268));
#22056=CARTESIAN_POINT('Ctrl Pts',(40.7070441711018,43.1839165395718,48.9250404774965));
#22057=CARTESIAN_POINT('Ctrl Pts',(40.714786517364,43.1849973794551,48.9390712873937));
#22058=CARTESIAN_POINT('Ctrl Pts',(40.7260978020611,43.186526987497,48.958979254092));
#22059=CARTESIAN_POINT('Ctrl Pts',(40.7295244689828,43.1869841450365,48.9649358952295));
#22060=CARTESIAN_POINT('Ctrl Pts',(40.7355187414656,43.1877729916333,48.9752282217527));
#22061=CARTESIAN_POINT('Ctrl Pts',(40.7380716139452,43.1881056084452,48.9795723488135));
#22062=CARTESIAN_POINT('Ctrl Pts',(40.7434929548609,43.1888049052147,48.988715440387));
#22063=CARTESIAN_POINT('Ctrl Pts',(40.7463652855857,43.1891713311604,48.9935119757252));
#22064=CARTESIAN_POINT('Ctrl Pts',(40.7541911191952,43.1901589284921,49.0064524544127));
#22065=CARTESIAN_POINT('Ctrl Pts',(40.7591842738233,43.1907775794305,49.0145724109104));
#22066=CARTESIAN_POINT('Ctrl Pts',(40.7827271010708,43.1936433646494,49.0522297485454));
#22067=CARTESIAN_POINT('Ctrl Pts',(40.8020167110844,43.1958461637218,49.0812996071235));
#22068=CARTESIAN_POINT('Ctrl Pts',(40.8909163817015,43.2054566028717,49.2076935405672));
#22069=CARTESIAN_POINT('Ctrl Pts',(40.9687081603729,43.2124968292755,49.2989480374893));
#22070=CARTESIAN_POINT('Ctrl Pts',(41.1109009360525,43.224359327367,49.4373481161009));
#22071=CARTESIAN_POINT('Ctrl Pts',(41.1706495506119,43.229102887719,49.4887719939867));
#22072=CARTESIAN_POINT('Ctrl Pts',(41.2702041073036,43.2368377477768,49.5643665915635));
#22073=CARTESIAN_POINT('Ctrl Pts',(41.3080296069225,43.2397407203512,49.5910002257988));
#22074=CARTESIAN_POINT('Ctrl Pts',(41.3559653126048,43.2433964880269,49.6222374983448));
#22075=CARTESIAN_POINT('Ctrl Pts',(41.3652080920163,43.2441003231359,49.6281488349178));
#22076=CARTESIAN_POINT('Ctrl Pts',(41.3831864221297,43.245467650845,49.6394321772678));
#22077=CARTESIAN_POINT('Ctrl Pts',(41.3919153895778,43.2461307540997,49.6448140100018));
#22078=CARTESIAN_POINT('Ctrl Pts',(41.4081058405409,43.2473594724225,49.654618918038));
#22079=CARTESIAN_POINT('Ctrl Pts',(41.4155550812215,43.2479243426073,49.6590617786114));
#22080=CARTESIAN_POINT('Ctrl Pts',(41.4321154461181,43.2491792140088,49.6687878742903));
#22081=CARTESIAN_POINT('Ctrl Pts',(41.4412403328401,43.2498700689745,49.6740470041675));
#22082=CARTESIAN_POINT('Ctrl Pts',(41.4665210914475,43.2517827426571,49.688343079832));
#22083=CARTESIAN_POINT('Ctrl Pts',(41.4827643282326,43.2530101556091,49.6972224101654));
#22084=CARTESIAN_POINT('Ctrl Pts',(41.5938307375592,43.2613951900539,49.7558765560863));
#22085=CARTESIAN_POINT('Ctrl Pts',(41.6925074132272,43.2688232141108,49.7979032234379));
#22086=CARTESIAN_POINT('Ctrl Pts',(41.7941388354972,43.276409063163,49.8315225377394));
#22087=CARTESIAN_POINT('',(40.470870769445,43.2895297265089,48.001722996834));
#22088=CARTESIAN_POINT('Ctrl Pts',(41.7941388168303,43.4464579097838,49.8315225315644));
#22089=CARTESIAN_POINT('Ctrl Pts',(41.7761768129493,43.4451567388353,49.8255807641355));
#22090=CARTESIAN_POINT('Ctrl Pts',(41.7582998990573,43.4438661233107,49.81937399617));
#22091=CARTESIAN_POINT('Ctrl Pts',(41.7307636638786,43.4418880138451,49.8093570494479));
#22092=CARTESIAN_POINT('Ctrl Pts',(41.7210418610757,43.4411915573444,49.805731448244));
#22093=CARTESIAN_POINT('Ctrl Pts',(41.7053766573696,43.4400729799323,49.7997449413589));
#22094=CARTESIAN_POINT('Ctrl Pts',(41.6994150688083,43.4396481531526,49.7974326688846));
#22095=CARTESIAN_POINT('Ctrl Pts',(41.6888295573247,43.4388954987841,49.7932662864778));
#22096=CARTESIAN_POINT('Ctrl Pts',(41.6842012080984,43.4385669935767,49.7914238650287));
#22097=CARTESIAN_POINT('Ctrl Pts',(41.6741337302187,43.4378537215749,49.7873710254473));
#22098=CARTESIAN_POINT('Ctrl Pts',(41.6686975308336,43.4374693744035,49.7851536978842));
#22099=CARTESIAN_POINT('Ctrl Pts',(41.6536181768234,43.4364052498043,49.7789226593268));
#22100=CARTESIAN_POINT('Ctrl Pts',(41.6439971969751,43.4357286040933,49.7748553257913));
#22101=CARTESIAN_POINT('Ctrl Pts',(41.6221561935667,43.4341967064757,49.7654120708336));
#22102=CARTESIAN_POINT('Ctrl Pts',(41.6099578614026,43.4333441432331,49.7599869909483));
#22103=CARTESIAN_POINT('Ctrl Pts',(41.5707951915101,43.4306136532361,49.7420805769805));
#22104=CARTESIAN_POINT('Ctrl Pts',(41.5440614684296,43.4287599847571,49.729102302794));
#22105=CARTESIAN_POINT('Ctrl Pts',(41.4215373756617,43.420264083815,49.6660827417399));
#22106=CARTESIAN_POINT('Ctrl Pts',(41.3297544440341,43.413890009113,49.6086636124085));
#22107=CARTESIAN_POINT('Ctrl Pts',(41.1485050237377,43.4003540529157,49.4728615919337));
#22108=CARTESIAN_POINT('Ctrl Pts',(41.0605016272557,43.3931965071083,49.3933052886631));
#22109=CARTESIAN_POINT('Ctrl Pts',(40.9687728368603,43.3845917004353,49.29360880437));
#22110=CARTESIAN_POINT('Ctrl Pts',(40.9573634452525,43.3834989610702,49.2808726213637));
#22111=CARTESIAN_POINT('Ctrl Pts',(40.9388792798639,43.3816900835254,49.2596786596117));
#22112=CARTESIAN_POINT('Ctrl Pts',(40.9317048888039,43.3809781021997,49.2513087318448));
#22113=CARTESIAN_POINT('Ctrl Pts',(40.9188895869558,43.379688035779,49.2360959254372));
#22114=CARTESIAN_POINT('Ctrl Pts',(40.9132233362289,43.3791110126694,49.2292747211909));
#22115=CARTESIAN_POINT('Ctrl Pts',(40.9011845171979,43.3778705881727,49.2145770254516));
#22116=CARTESIAN_POINT('Ctrl Pts',(40.8948265896499,43.3772066178663,49.2066889410113));
#22117=CARTESIAN_POINT('Ctrl Pts',(40.8776292788225,43.3753859514126,49.1850053777982));
#22118=CARTESIAN_POINT('Ctrl Pts',(40.8669157078838,43.3742242998406,49.1711118121825));
#22119=CARTESIAN_POINT('Ctrl Pts',(40.8103085637684,43.3679346890437,49.095594492469));
#22120=CARTESIAN_POINT('Ctrl Pts',(40.7679438016097,43.3626723101874,49.0314242661745));
#22121=CARTESIAN_POINT('Ctrl Pts',(40.6756291536202,43.3497659340359,48.8716060407526));
#22122=CARTESIAN_POINT('Ctrl Pts',(40.6296510097581,43.3420310535434,48.7739594924638));
#22123=CARTESIAN_POINT('Ctrl Pts',(40.562192431016,43.3282549881674,48.5927389771338));
#22124=CARTESIAN_POINT('Ctrl Pts',(40.5376908329482,43.3222110482301,48.5105724067162));
#22125=CARTESIAN_POINT('Ctrl Pts',(40.5163946678963,43.3157142083722,48.416755034115));
#22126=CARTESIAN_POINT('Ctrl Pts',(40.5141441680002,43.3150060121356,48.4064499953036));
#22127=CARTESIAN_POINT('Ctrl Pts',(40.5106547889467,43.3138723557064,48.3898188948568));
#22128=CARTESIAN_POINT('Ctrl Pts',(40.5093629332993,43.3134440741202,48.3835043445843));
#22129=CARTESIAN_POINT('Ctrl Pts',(40.5071279229701,43.3126876777404,48.3722938544672));
#22130=CARTESIAN_POINT('Ctrl Pts',(40.5061720742926,43.3123588583899,48.3674006040953));
#22131=CARTESIAN_POINT('Ctrl Pts',(40.5041388603734,43.3116476394694,48.3567732254181));
#22132=CARTESIAN_POINT('Ctrl Pts',(40.5030685311495,43.3112656389007,48.3510378894507));
#22133=CARTESIAN_POINT('Ctrl Pts',(40.5009102771965,43.3104791041233,48.3391747527503));
#22134=CARTESIAN_POINT('Ctrl Pts',(40.4998259514978,43.3100747707399,48.3330463573078));
#22135=CARTESIAN_POINT('Ctrl Pts',(40.4971135140632,43.3090388467933,48.3172716149712));
#22136=CARTESIAN_POINT('Ctrl Pts',(40.4955290628552,43.3084095354203,48.3076178063816));
#22137=CARTESIAN_POINT('Ctrl Pts',(40.4786997314613,43.3014391903391,48.1999615826876));
#22138=CARTESIAN_POINT('Ctrl Pts',(40.4709593710398,43.29546088323,48.100924529371));
#22139=CARTESIAN_POINT('Ctrl Pts',(40.470870769445,43.2895297265089,48.001722996834));
#22140=CARTESIAN_POINT('Ctrl Pts',(40.470870770631,43.2895298058776,48.0017243243157));
#22141=CARTESIAN_POINT('Ctrl Pts',(40.4707541166506,43.2817267810287,47.871214882825));
#22142=CARTESIAN_POINT('Ctrl Pts',(40.4838808354969,43.2740228213524,47.7410348150679));
#22143=CARTESIAN_POINT('Ctrl Pts',(40.5174173845313,43.2636492378451,47.5771820820791));
#22144=CARTESIAN_POINT('Ctrl Pts',(40.5258104418137,43.2613439678219,47.5414091936409));
#22145=CARTESIAN_POINT('Ctrl Pts',(40.539745682672,43.257882335434,47.4888163225953));
#22146=CARTESIAN_POINT('Ctrl Pts',(40.54450649835,43.2567507473241,47.4717967160789));
#22147=CARTESIAN_POINT('Ctrl Pts',(40.5523712283617,43.2549567065817,47.4451002905912));
#22148=CARTESIAN_POINT('Ctrl Pts',(40.5553190002772,43.2542993530091,47.4353782080099));
#22149=CARTESIAN_POINT('Ctrl Pts',(40.5609824999741,43.2530636630526,47.4172172141841));
#22150=CARTESIAN_POINT('Ctrl Pts',(40.5636798844698,43.2524859431979,47.408772827317));
#22151=CARTESIAN_POINT('Ctrl Pts',(40.5698499344321,43.2511879896419,47.3899065929289));
#22152=CARTESIAN_POINT('Ctrl Pts',(40.57335358815,43.2504667475821,47.3794952817078));
#22153=CARTESIAN_POINT('Ctrl Pts',(40.5824958604471,43.248623691456,47.3530770795669));
#22154=CARTESIAN_POINT('Ctrl Pts',(40.588257039099,43.2474978493109,47.3371139053633));
#22155=CARTESIAN_POINT('Ctrl Pts',(40.6373551515685,43.238182795715,47.2064954311846));
#22156=CARTESIAN_POINT('Ctrl Pts',(40.6913106955539,43.2296306559741,47.0961542600228));
#22157=CARTESIAN_POINT('Ctrl Pts',(40.8092856755564,43.2135679449637,46.9037256890813));
#22158=CARTESIAN_POINT('Ctrl Pts',(40.8701884658898,43.2061387072989,46.8202258639562));
#22159=CARTESIAN_POINT('Ctrl Pts',(40.9572393556313,43.1967956922784,46.7190228101481));
#22160=CARTESIAN_POINT('Ctrl Pts',(40.9775400292117,43.1946947414766,46.6965167149004));
#22161=CARTESIAN_POINT('Ctrl Pts',(41.0118382876095,43.1912826196213,46.660248453157));
#22162=CARTESIAN_POINT('Ctrl Pts',(41.0255301015716,43.1899545898043,46.6462054371001));
#22163=CARTESIAN_POINT('Ctrl Pts',(41.0446247040912,43.1881516244909,46.6272094235261));
#22164=CARTESIAN_POINT('Ctrl Pts',(41.0498445463117,43.1876636600574,46.6220753232572));
#22165=CARTESIAN_POINT('Ctrl Pts',(41.0588279843742,43.1868324188253,46.6133395100025));
#22166=CARTESIAN_POINT('Ctrl Pts',(41.0625771321628,43.1864880244398,46.6097231338673));
#22167=CARTESIAN_POINT('Ctrl Pts',(41.0697008787049,43.1858384654623,46.6029071510149));
#22168=CARTESIAN_POINT('Ctrl Pts',(41.0730724669884,43.1855330576821,46.5997044940125));
#22169=CARTESIAN_POINT('Ctrl Pts',(41.0810789557544,43.1848124783659,46.5921540495342));
#22170=CARTESIAN_POINT('Ctrl Pts',(41.0857238593242,43.1843981127126,46.5878168780077));
#22171=CARTESIAN_POINT('Ctrl Pts',(41.1020451130176,43.1829545401866,46.5727272104199));
#22172=CARTESIAN_POINT('Ctrl Pts',(41.1138330371377,43.1819339870904,46.5620955917117));
#22173=CARTESIAN_POINT('Ctrl Pts',(41.2169495263108,43.1731812997313,46.4713768782964));
#22174=CARTESIAN_POINT('Ctrl Pts',(41.3155352466535,43.1659718170732,46.3999245034361));
#22175=CARTESIAN_POINT('Ctrl Pts',(41.5015704577851,43.1530912092974,46.2902368834838));
#22176=CARTESIAN_POINT('Ctrl Pts',(41.5863513956463,43.1474532602462,46.2483037481745));
#22177=CARTESIAN_POINT('Ctrl Pts',(41.7057053763789,43.1395145355678,46.1998113215623));
#22178=CARTESIAN_POINT('Ctrl Pts',(41.7378922896855,43.1373744343821,46.1877258828294));
#22179=CARTESIAN_POINT('Ctrl Pts',(41.7945001357346,43.133599070185,46.168180298256));
#22180=CARTESIAN_POINT('Ctrl Pts',(41.8187785817019,43.1319762905807,46.1603328913135));
#22181=CARTESIAN_POINT('Ctrl Pts',(41.8544329281658,43.1295845879111,46.1495847334892));
#22182=CARTESIAN_POINT('Ctrl Pts',(41.8656916408498,43.1288281282393,46.1463024368184));
#22183=CARTESIAN_POINT('Ctrl Pts',(41.8855908458022,43.1274886557041,46.1406974910744));
#22184=CARTESIAN_POINT('Ctrl Pts',(41.8942189570669,43.1269070605278,46.1383318959328));
#22185=CARTESIAN_POINT('Ctrl Pts',(41.9122661716195,43.1256887140195,46.1335185570328));
#22186=CARTESIAN_POINT('Ctrl Pts',(41.9216879455063,43.1250516211692,46.1310819073807));
#22187=CARTESIAN_POINT('Ctrl Pts',(41.9463657675858,43.1233800128109,46.1248985842091));
#22188=CARTESIAN_POINT('Ctrl Pts',(41.9616495967122,43.1223418244375,46.1212668536184));
#22189=CARTESIAN_POINT('Ctrl Pts',(42.0266915923158,43.1179103568648,46.1066484971889));
#22190=CARTESIAN_POINT('Ctrl Pts',(42.0768263219138,43.1144607999057,46.0974498608068));
#22191=CARTESIAN_POINT('Ctrl Pts',(42.1522507269199,43.1092182382893,46.0866782822063));
#22192=CARTESIAN_POINT('Ctrl Pts',(42.1773055905031,43.1074682575869,46.0836005604724));
#22193=CARTESIAN_POINT('Ctrl Pts',(42.3370708368975,43.0962598243401,46.0671504191077));
#22194=CARTESIAN_POINT('Ctrl Pts',(42.4728099022343,43.0864769656933,46.0674987858754));
#22195=CARTESIAN_POINT('Ctrl Pts',(42.6706589276612,43.0724040328661,46.0888909297531));
#22196=CARTESIAN_POINT('Ctrl Pts',(42.7335719570051,43.0679641415169,46.0988620099974));
#22197=CARTESIAN_POINT('Ctrl Pts',(42.8064609701078,43.0629430612375,46.1141450608485));
#22198=CARTESIAN_POINT('Ctrl Pts',(42.8170205135377,43.0622187366912,46.1164519447807));
#22199=CARTESIAN_POINT('Ctrl Pts',(42.8332814056699,43.0611086834193,46.1201478246893));
#22200=CARTESIAN_POINT('Ctrl Pts',(42.8389965376927,43.0607195626893,46.1214742430067));
#22201=CARTESIAN_POINT('Ctrl Pts',(42.8495534762029,43.0600027907616,46.1239752001683));
#22202=CARTESIAN_POINT('Ctrl Pts',(42.8543967739232,43.0596747477524,46.1251424186548));
#22203=CARTESIAN_POINT('Ctrl Pts',(42.8654512653732,43.0589277871756,46.1278518672668));
#22204=CARTESIAN_POINT('Ctrl Pts',(42.8716593472753,43.0585095719483,46.12940625085));
#22205=CARTESIAN_POINT('Ctrl Pts',(42.887929383402,43.0574165781021,46.1335661005816));
#22206=CARTESIAN_POINT('Ctrl Pts',(42.8979783751301,43.0567445806947,46.1362220804298));
#22207=CARTESIAN_POINT('Ctrl Pts',(42.9772609843494,43.0514635730865,46.1578637423645));
#22208=CARTESIAN_POINT('Ctrl Pts',(43.0454156983398,43.0470486348728,46.1806217332715));
#22209=CARTESIAN_POINT('Ctrl Pts',(43.2181792678902,43.0358099784963,46.2492455385647));
#22210=CARTESIAN_POINT('Ctrl Pts',(43.320263931079,43.0291105944545,46.3006843022093));
#22211=CARTESIAN_POINT('Ctrl Pts',(43.4890424145211,43.0171053161274,46.4054226642243));
#22212=CARTESIAN_POINT('Ctrl Pts',(43.5578619437439,43.0119041918912,46.4546704792855));
#22213=CARTESIAN_POINT('Ctrl Pts',(43.6368243346242,43.0054064745744,46.5194199031533));
#22214=CARTESIAN_POINT('Ctrl Pts',(43.6502702307908,43.0042802737057,46.5307565977705));
#22215=CARTESIAN_POINT('Ctrl Pts',(43.6712215619849,43.0024928520106,46.5489172560233));
#22216=CARTESIAN_POINT('Ctrl Pts',(43.6788316058072,43.0018366661885,46.5556194729273));
#22217=CARTESIAN_POINT('Ctrl Pts',(43.6929959229987,43.0006020064794,46.5682937738862));
#22218=CARTESIAN_POINT('Ctrl Pts',(43.6995625741055,43.0000241391273,46.5742516749651));
#22219=CARTESIAN_POINT('Ctrl Pts',(43.7141912966492,42.9987243184008,46.5877092961627));
#22220=CARTESIAN_POINT('Ctrl Pts',(43.722230645678,42.9980013436831,46.5952331483834));
#22221=CARTESIAN_POINT('Ctrl Pts',(43.7425577409355,42.9961508609826,46.6145859204196));
#22222=CARTESIAN_POINT('Ctrl Pts',(43.754753613385,42.9950192688974,46.6265095286991));
#22223=CARTESIAN_POINT('Ctrl Pts',(43.844868604185,42.9864940747393,46.7169807953295));
#22224=CARTESIAN_POINT('Ctrl Pts',(43.9160460750823,42.9788089208104,46.8019264271976));
#22225=CARTESIAN_POINT('Ctrl Pts',(44.0620329650053,42.9607686655669,47.0101343461055));
#22226=CARTESIAN_POINT('Ctrl Pts',(44.1311215009206,42.9503446010809,47.1366294302752));
#22227=CARTESIAN_POINT('Ctrl Pts',(44.1935074225809,42.9390637437029,47.2891425625455));
#22228=CARTESIAN_POINT('Ctrl Pts',(44.2011704915683,42.9376343655986,47.3087893796055));
#22229=CARTESIAN_POINT('Ctrl Pts',(44.2111742375575,42.9357100251437,47.3357342243179));
#22230=CARTESIAN_POINT('Ctrl Pts',(44.2137955466328,42.9351998969627,47.3429255297551));
#22231=CARTESIAN_POINT('Ctrl Pts',(44.218118838154,42.9343487403253,47.3550090901977));
#22232=CARTESIAN_POINT('Ctrl Pts',(44.219844022777,42.9340063683103,47.3598928853407));
#22233=CARTESIAN_POINT('Ctrl Pts',(44.2230889836003,42.9333572270065,47.369198151321));
#22234=CARTESIAN_POINT('Ctrl Pts',(44.2246123838327,42.9330502372792,47.3736182758472));
#22235=CARTESIAN_POINT('Ctrl Pts',(44.2282006310545,42.932321660967,47.3841536972047));
#22236=CARTESIAN_POINT('Ctrl Pts',(44.2302509025028,42.931900923855,47.3902739526123));
#22237=CARTESIAN_POINT('Ctrl Pts',(44.2374220894991,42.9304129336969,47.4120427594252));
#22238=CARTESIAN_POINT('Ctrl Pts',(44.2423735143219,42.92935504673,47.4277469711916));
#22239=CARTESIAN_POINT('Ctrl Pts',(44.2758104687147,42.9219750827021,47.5387328765873));
#22240=CARTESIAN_POINT('Ctrl Pts',(44.2970954680145,42.9159977488544,47.636041036543));
#22241=CARTESIAN_POINT('Ctrl Pts',(44.3259242975384,42.903481070421,47.8435725494755));
#22242=CARTESIAN_POINT('Ctrl Pts',(44.3317105371758,42.8969663731238,47.953667049074));
#22243=CARTESIAN_POINT('Ctrl Pts',(44.3262170847473,42.8867405391596,48.1200699951871));
#22244=CARTESIAN_POINT('Ctrl Pts',(44.3218793116618,42.8832171891892,48.1763747317665));
#22245=CARTESIAN_POINT('Ctrl Pts',(44.3131886726569,42.8786148635724,48.2479880662432));
#22246=CARTESIAN_POINT('Ctrl Pts',(44.3111074462546,42.8776076409016,48.2635474975751));
#22247=CARTESIAN_POINT('Ctrl Pts',(44.3074291192456,42.8759664392421,48.2887063750635));
#22248=CARTESIAN_POINT('Ctrl Pts',(44.3059488364976,42.8753361689039,48.2983223806951));
#22249=CARTESIAN_POINT('Ctrl Pts',(44.3029677354521,42.8741218269356,48.3167592289698));
#22250=CARTESIAN_POINT('Ctrl Pts',(44.3014781600874,42.8735381273917,48.3255816540619));
#22251=CARTESIAN_POINT('Ctrl Pts',(44.2979277685529,42.8721973773524,48.3457539669727));
#22252=CARTESIAN_POINT('Ctrl Pts',(44.2958264309725,42.8714390533499,48.357096281264));
#22253=CARTESIAN_POINT('Ctrl Pts',(44.288820679913,42.8690170229253,48.3931049021154));
#22254=CARTESIAN_POINT('Ctrl Pts',(44.2835357626495,42.8673412732813,48.4176936123286));
#22255=CARTESIAN_POINT('Ctrl Pts',(44.2459200630748,42.856306514292,48.5774365601054));
#22256=CARTESIAN_POINT('Ctrl Pts',(44.1995515044912,42.8464892464088,48.7088404387417));
#22257=CARTESIAN_POINT('Ctrl Pts',(44.1226160467818,42.8337793922827,48.8692866059474));
#22258=CARTESIAN_POINT('Ctrl Pts',(44.1046803404323,42.8309898770007,48.9039525649023));
#22259=CARTESIAN_POINT('Ctrl Pts',(44.058920322573,42.8242946922188,48.9861846784148));
#22260=CARTESIAN_POINT('Ctrl Pts',(44.0300839366676,42.8204047383894,49.0331524742518));
#22261=CARTESIAN_POINT('Ctrl Pts',(43.9824571725836,42.8145173885406,49.103755521919));
#22262=CARTESIAN_POINT('Ctrl Pts',(43.9650575277466,42.8124636692133,49.1282916885228));
#22263=CARTESIAN_POINT('Ctrl Pts',(43.9418833676139,42.8098595726407,49.1594025219305));
#22264=CARTESIAN_POINT('Ctrl Pts',(43.9366291621493,42.8092774301099,49.1663573004659));
#22265=CARTESIAN_POINT('Ctrl Pts',(43.9280380549988,42.8083391875214,49.1775701757878));
#22266=CARTESIAN_POINT('Ctrl Pts',(43.924730136477,42.8079811332171,49.1818501720399));
#22267=CARTESIAN_POINT('Ctrl Pts',(43.9182959514685,42.8072909492012,49.190103154022));
#22268=CARTESIAN_POINT('Ctrl Pts',(43.9151720233292,42.8069586716358,49.1940778257007));
#22269=CARTESIAN_POINT('Ctrl Pts',(43.9082218307476,42.806225519278,49.2028495821503));
#22270=CARTESIAN_POINT('Ctrl Pts',(43.9043881942443,42.8058251638368,49.2076408288754));
#22271=CARTESIAN_POINT('Ctrl Pts',(43.8906761565823,42.8044071382266,49.2246113940858));
#22272=CARTESIAN_POINT('Ctrl Pts',(43.8806718698636,42.8033980268368,49.2366888542377));
#22273=CARTESIAN_POINT('Ctrl Pts',(43.7855089102804,42.7940198729723,49.3487617884767));
#22274=CARTESIAN_POINT('Ctrl Pts',(43.6904814708786,42.7862670300302,49.4399517428875));
#22275=CARTESIAN_POINT('Ctrl Pts',(43.4869373108206,42.770860259021,49.5988096809996));
#22276=CARTESIAN_POINT('Ctrl Pts',(43.3795280964244,42.7632423367256,49.6667765490118));
#22277=CARTESIAN_POINT('Ctrl Pts',(43.2474268579138,42.7538754904716,49.733162822768));
#22278=CARTESIAN_POINT('Ctrl Pts',(43.2284657035034,42.7525318353256,49.742305992699));
#22279=CARTESIAN_POINT('Ctrl Pts',(43.1994937941521,42.7504781336782,49.755696542629));
#22280=CARTESIAN_POINT('Ctrl Pts',(43.1895900903884,42.749775991563,49.7601727636372));
#22281=CARTESIAN_POINT('Ctrl Pts',(43.1715476200334,42.7484963849554,49.7681445859927));
#22282=CARTESIAN_POINT('Ctrl Pts',(43.1634215425631,42.7479199039048,49.7716682959576));
#22283=CARTESIAN_POINT('Ctrl Pts',(43.1458426097537,42.7466723225122,49.7791476494624));
#22284=CARTESIAN_POINT('Ctrl Pts',(43.1363819634245,42.7460005914546,49.7830841691193));
#22285=CARTESIAN_POINT('Ctrl Pts',(43.110582672471,42.7441677067713,49.7935787620019));
#22286=CARTESIAN_POINT('Ctrl Pts',(43.0941852223347,42.74300160408,49.7999887088273));
#22287=CARTESIAN_POINT('Ctrl Pts',(43.0054542591068,42.7366835283692,49.8332818741423));
#22288=CARTESIAN_POINT('Ctrl Pts',(42.931653717996,42.731396034906,49.856027715763));
#22289=CARTESIAN_POINT('Ctrl Pts',(42.7306077192985,42.716919944404,49.9050154024218));
#22290=CARTESIAN_POINT('Ctrl Pts',(42.6017426471223,42.7075466553483,49.9229354592763));
#22291=CARTESIAN_POINT('Ctrl Pts',(42.4078443894754,42.6938213012057,49.9301843965695));
#22292=CARTESIAN_POINT('Ctrl Pts',(42.3435307826269,42.6893366913106,49.9293746093143));
#22293=CARTESIAN_POINT('Ctrl Pts',(42.2685618543556,42.6842721158948,49.924677602452));
#22294=CARTESIAN_POINT('Ctrl Pts',(42.257758000344,42.6835462567445,49.9239093238542));
#22295=CARTESIAN_POINT('Ctrl Pts',(42.2411076775928,42.6824343604537,49.9225842670244));
#22296=CARTESIAN_POINT('Ctrl Pts',(42.2352565287868,42.6820449140683,49.9220917316563));
#22297=CARTESIAN_POINT('Ctrl Pts',(42.2244456072618,42.6813278468881,49.9211319652107));
#22298=CARTESIAN_POINT('Ctrl Pts',(42.2194854049952,42.6809998315774,49.9206722402568));
#22299=CARTESIAN_POINT('Ctrl Pts',(42.2081634422171,42.6802533209486,49.9195786420002));
#22300=CARTESIAN_POINT('Ctrl Pts',(42.2018030108196,42.6798355245672,49.9189323552678));
#22301=CARTESIAN_POINT('Ctrl Pts',(42.1851326314525,42.678744360844,49.9171546994656));
#22302=CARTESIAN_POINT('Ctrl Pts',(42.1748282278167,42.6780737596555,49.9159717670626));
#22303=CARTESIAN_POINT('Ctrl Pts',(42.0928645744725,42.6727669345001,49.9058920528224));
#22304=CARTESIAN_POINT('Ctrl Pts',(42.021737952952,42.6683272009993,49.8930602248049));
#22305=CARTESIAN_POINT('Ctrl Pts',(41.8984164307745,42.6606629043884,49.8635810507729));
#22306=CARTESIAN_POINT('Ctrl Pts',(41.845918938182,42.6574112284475,49.8486512139258));
#22307=CARTESIAN_POINT('Ctrl Pts',(41.7941387803776,42.6541583936299,49.831522519506));
#22308=CARTESIAN_POINT('Origin',(42.4,48.4493818343519,48.));
#22309=CARTESIAN_POINT('',(41.7941388322699,41.6906508784004,49.8315225366718));
#22310=CARTESIAN_POINT('',(41.7941388317731,41.8624153300426,49.8315225365075));
#22311=CARTESIAN_POINT('',(41.7941388317924,48.4493818343519,49.8315225365138));
#22312=CARTESIAN_POINT('Ctrl Pts',(41.7941388322699,41.6906508784004,49.8315225366718));
#22313=CARTESIAN_POINT('Ctrl Pts',(41.902301765201,41.6975401149299,49.8673024517636));
#22314=CARTESIAN_POINT('Ctrl Pts',(42.0134254443717,41.704230344215,49.8934319960916));
#22315=CARTESIAN_POINT('Ctrl Pts',(42.2104237760017,41.7162554282414,49.9216766110695));
#22316=CARTESIAN_POINT('Ctrl Pts',(42.2953332145075,41.7214877326998,49.9281655307091));
#22317=CARTESIAN_POINT('Ctrl Pts',(42.3980024058597,41.7280207752068,49.9292093980171));
#22318=CARTESIAN_POINT('Ctrl Pts',(42.4156189574747,41.7291488241351,49.9291471967907));
#22319=CARTESIAN_POINT('Ctrl Pts',(42.4433790754323,41.7309386364785,49.9286689223164));
#22320=CARTESIAN_POINT('Ctrl Pts',(42.4535247188529,41.7315953438571,49.928414025573));
#22321=CARTESIAN_POINT('Ctrl Pts',(42.4725316487446,41.7328306580704,49.9277863916251));
#22322=CARTESIAN_POINT('Ctrl Pts',(42.4813933261753,41.733408655195,49.927432575689));
#22323=CARTESIAN_POINT('Ctrl Pts',(42.5012469691224,41.7347083389644,49.9265027277153));
#22324=CARTESIAN_POINT('Ctrl Pts',(42.5122370050278,41.73543104391,49.9258937028818));
#22325=CARTESIAN_POINT('Ctrl Pts',(42.5402233859625,41.7372800051956,49.9241024460917));
#22326=CARTESIAN_POINT('Ctrl Pts',(42.5572100891708,41.7384103323653,49.9227890620355));
#22327=CARTESIAN_POINT('Ctrl Pts',(42.6982288167364,41.7478634839723,49.9100045898656));
#22328=CARTESIAN_POINT('Ctrl Pts',(42.8208768570923,41.7565618355221,49.8867723954869));
#22329=CARTESIAN_POINT('Ctrl Pts',(43.0318271865955,41.7722073235644,49.8252138952612));
#22330=CARTESIAN_POINT('Ctrl Pts',(43.1211447864983,41.7790559776539,49.7918041813452));
#22331=CARTESIAN_POINT('Ctrl Pts',(43.2384227365765,41.7881254672382,49.7377397642685));
#22332=CARTESIAN_POINT('Ctrl Pts',(43.26883669027,41.7904839659775,49.7227348174888));
#22333=CARTESIAN_POINT('Ctrl Pts',(43.3178977911307,41.7942820013022,49.6969001338608));
#22334=CARTESIAN_POINT('Ctrl Pts',(43.3367862114319,41.7957425890707,49.6865462072277));
#22335=CARTESIAN_POINT('Ctrl Pts',(43.3622027011903,41.7977017609218,49.6720550471824));
#22336=CARTESIAN_POINT('Ctrl Pts',(43.3688843342456,41.7982162052556,49.6681922163997));
#22337=CARTESIAN_POINT('Ctrl Pts',(43.3800233476619,41.7990726124423,49.6616629527363));
#22338=CARTESIAN_POINT('Ctrl Pts',(43.384493408753,41.7994159530059,49.6590184630073));
#22339=CARTESIAN_POINT('Ctrl Pts',(43.3929586098621,41.8000654414189,49.6539641842161));
#22340=CARTESIAN_POINT('Ctrl Pts',(43.3969557634222,41.8003718197589,49.6515579101284));
#22341=CARTESIAN_POINT('Ctrl Pts',(43.4064260216254,41.8010970873829,49.6458099344876));
#22342=CARTESIAN_POINT('Ctrl Pts',(43.4118913137847,41.8015151459244,49.6424553721232));
#22343=CARTESIAN_POINT('Ctrl Pts',(43.4311110535656,41.8029839575296,49.6305260676264));
#22344=CARTESIAN_POINT('Ctrl Pts',(43.4447745136464,41.8040256573163,49.6218050188767));
#22345=CARTESIAN_POINT('Ctrl Pts',(43.5537248026694,41.8123256765482,49.5503163099166));
#22346=CARTESIAN_POINT('Ctrl Pts',(43.6433946923034,41.8191258503394,49.4793709252952));
#22347=CARTESIAN_POINT('Ctrl Pts',(43.7984877666602,41.8318650744642,49.3325400174104));
#22348=CARTESIAN_POINT('Ctrl Pts',(43.8653027277568,41.8377842371834,49.2586965798393));
#22349=CARTESIAN_POINT('Ctrl Pts',(43.94777852791,41.8460834114385,49.1520318462068));
#22350=CARTESIAN_POINT('Ctrl Pts',(43.9686567313663,41.8482851215911,49.1234373955597));
#22351=CARTESIAN_POINT('Ctrl Pts',(44.0035385508157,41.8521593703719,49.072794337793));
#22352=CARTESIAN_POINT('Ctrl Pts',(44.0179032991913,41.853818482534,49.0510054165264));
#22353=CARTESIAN_POINT('Ctrl Pts',(44.0381333772114,41.8562539744058,49.0189218106444));
#22354=CARTESIAN_POINT('Ctrl Pts',(44.0443532482775,41.8570172244743,49.0088533106183));
#22355=CARTESIAN_POINT('Ctrl Pts',(44.0551207776517,41.8583646086331,48.9910590919031));
#22356=CARTESIAN_POINT('Ctrl Pts',(44.0597080036014,41.8589472710854,48.9833576411897));
#22357=CARTESIAN_POINT('Ctrl Pts',(44.06914117163,41.8601638001704,48.9672663413911));
#22358=CARTESIAN_POINT('Ctrl Pts',(44.0739779064899,41.8607979802326,48.9588714141048));
#22359=CARTESIAN_POINT('Ctrl Pts',(44.086388876947,41.8624529177927,48.9369500736254));
#22360=CARTESIAN_POINT('Ctrl Pts',(44.0938635393647,41.8634772124119,48.9233683830394));
#22361=CARTESIAN_POINT('Ctrl Pts',(44.124291827974,41.8677653012249,48.8664662294501));
#22362=CARTESIAN_POINT('Ctrl Pts',(44.1457518011165,41.8710809133144,48.8223721477913));
#22363=CARTESIAN_POINT('Ctrl Pts',(44.2214613400341,41.8839880979541,48.6504573694087));
#22364=CARTESIAN_POINT('Ctrl Pts',(44.2635300692004,41.8939493544161,48.5177471345995));
#22365=CARTESIAN_POINT('Ctrl Pts',(44.3066737159292,41.9094860842328,48.3040060300991));
#22366=CARTESIAN_POINT('Ctrl Pts',(44.3175545189683,41.9150857403102,48.2254142597761));
#22367=CARTESIAN_POINT('Ctrl Pts',(44.3248085884504,41.9215902287793,48.1300817375579));
#22368=CARTESIAN_POINT('Ctrl Pts',(44.3258410521265,41.9226923571831,48.1137789354332));
#22369=CARTESIAN_POINT('Ctrl Pts',(44.3270162125813,41.9242464773297,48.0905484675476));
#22370=CARTESIAN_POINT('Ctrl Pts',(44.3273288327098,41.9247072194103,48.0836306331353));
#22371=CARTESIAN_POINT('Ctrl Pts',(44.3278048813653,41.925500190321,48.0716684401934));
#22372=CARTESIAN_POINT('Ctrl Pts',(44.3279857758168,41.9258333746621,48.0666248949335));
#22373=CARTESIAN_POINT('Ctrl Pts',(44.3283245566772,41.9265316489924,48.0560173350611));
#22374=CARTESIAN_POINT('Ctrl Pts',(44.3284781575461,41.9268965004976,48.0504533004413));
#22375=CARTESIAN_POINT('Ctrl Pts',(44.3288268755569,41.9278753175095,48.0354708693569));
#22376=CARTESIAN_POINT('Ctrl Pts',(44.3289770942293,41.9284868386388,48.0260514337042));
#22377=CARTESIAN_POINT('Ctrl Pts',(44.3293485383783,41.9312678215677,47.9829670987715));
#22378=CARTESIAN_POINT('Ctrl Pts',(44.3287575336453,41.9333960796806,47.94929887603));
#22379=CARTESIAN_POINT('Ctrl Pts',(44.3220159834673,41.9429986843331,47.7952432363451));
#22380=CARTESIAN_POINT('Ctrl Pts',(44.3054719796454,41.950091208388,47.6755730656905));
#22381=CARTESIAN_POINT('Ctrl Pts',(44.2518821165112,41.9640796624603,47.4477794411589));
#22382=CARTESIAN_POINT('Ctrl Pts',(44.2162117644928,41.9709379025354,47.3398598828189));
#22383=CARTESIAN_POINT('Ctrl Pts',(44.1627972412724,41.9794763321761,47.2160702639712));
#22384=CARTESIAN_POINT('Ctrl Pts',(44.1539984997376,41.9808410967088,47.196576606338));
#22385=CARTESIAN_POINT('Ctrl Pts',(44.1402126263616,41.9829206450285,47.1673402744874));
#22386=CARTESIAN_POINT('Ctrl Pts',(44.1354635030115,41.9836272154368,47.1574867211703));
#22387=CARTESIAN_POINT('Ctrl Pts',(44.1267146682417,41.984911661889,47.1397223816314));
#22388=CARTESIAN_POINT('Ctrl Pts',(44.1227437142393,41.9854885201635,47.1317977097342));
#22389=CARTESIAN_POINT('Ctrl Pts',(44.1140865718742,41.9867332776627,47.1148142570634));
#22390=CARTESIAN_POINT('Ctrl Pts',(44.1093828934035,41.98740178081,47.1057647444193));
#22391=CARTESIAN_POINT('Ctrl Pts',(44.0964674395091,41.989216803376,47.0813906968972));
#22392=CARTESIAN_POINT('Ctrl Pts',(44.0881200586082,41.9903681100572,47.0661394863386));
#22393=CARTESIAN_POINT('Ctrl Pts',(44.0434765814393,41.9964164352621,46.9871278573033));
#22394=CARTESIAN_POINT('Ctrl Pts',(44.0037753157641,42.0014353123003,46.925370936773));
#22395=CARTESIAN_POINT('Ctrl Pts',(43.8830809660258,42.0157696292457,46.7592618070071));
#22396=CARTESIAN_POINT('Ctrl Pts',(43.7947538136503,42.0252994238503,46.6607400523754));
#22397=CARTESIAN_POINT('Ctrl Pts',(43.6639137946898,42.03781294897,46.5418945402952));
#22398=CARTESIAN_POINT('Ctrl Pts',(43.6297102446273,42.0409559573606,46.5129348183442));
#22399=CARTESIAN_POINT('Ctrl Pts',(43.5806774401909,42.0452557661766,46.4742692132599));
#22400=CARTESIAN_POINT('Ctrl Pts',(43.566677986607,42.0464611168152,46.4635377727867));
#22401=CARTESIAN_POINT('Ctrl Pts',(43.541957788275,42.0485482202678,46.4451209475018));
#22402=CARTESIAN_POINT('Ctrl Pts',(43.5313019226346,42.0494348106958,46.4373508258329));
#22403=CARTESIAN_POINT('Ctrl Pts',(43.5153953911154,42.050738032053,46.4259999869463));
#22404=CARTESIAN_POINT('Ctrl Pts',(43.5102056308366,42.0511600826889,46.4223351497442));
#22405=CARTESIAN_POINT('Ctrl Pts',(43.5013050926794,42.0518784170553,46.4161155521731));
#22406=CARTESIAN_POINT('Ctrl Pts',(43.4976033671385,42.0521755570466,46.4135480778687));
#22407=CARTESIAN_POINT('Ctrl Pts',(43.489187168632,42.0528474549226,46.4077542582658));
#22408=CARTESIAN_POINT('Ctrl Pts',(43.4844673352797,42.0532216732456,46.4045358696638));
#22409=CARTESIAN_POINT('Ctrl Pts',(43.4715888172863,42.0542359597282,46.3958377412963));
#22410=CARTESIAN_POINT('Ctrl Pts',(43.4634023091277,42.0548733326904,46.3903992158092));
#22411=CARTESIAN_POINT('Ctrl Pts',(43.4221460119354,42.0580505112439,46.3634436631518));
#22412=CARTESIAN_POINT('Ctrl Pts',(43.3884606940368,42.0605331228437,46.3428804893813));
#22413=CARTESIAN_POINT('Ctrl Pts',(43.3264174110082,42.0649523196356,46.3075719577956));
#22414=CARTESIAN_POINT('Ctrl Pts',(43.2982801390761,42.0669019562324,46.2924711253116));
#22415=CARTESIAN_POINT('Ctrl Pts',(43.1758613114292,42.0752072330507,46.2306348422674));
#22416=CARTESIAN_POINT('Ctrl Pts',(43.0782173102583,42.0813988720314,46.1909570717585));
#22417=CARTESIAN_POINT('Ctrl Pts',(42.9171319641701,42.0915557019867,46.1403862080576));
#22418=CARTESIAN_POINT('Ctrl Pts',(42.8555404200791,42.0954243164026,46.1243478742562));
#22419=CARTESIAN_POINT('Ctrl Pts',(42.7669448977293,42.1010518617757,46.1058993696022));
#22420=CARTESIAN_POINT('Ctrl Pts',(42.7405065386958,42.1027387539933,46.1009684183926));
#22421=CARTESIAN_POINT('Ctrl Pts',(42.6931748613807,42.1057779222193,46.0931608716059));
#22422=CARTESIAN_POINT('Ctrl Pts',(42.6723208948376,42.1071235273944,46.0900711439292));
#22423=CARTESIAN_POINT('Ctrl Pts',(42.6406373600095,42.1091797298192,46.0859063458874));
#22424=CARTESIAN_POINT('Ctrl Pts',(42.6298419925145,42.1098823952755,46.0845800705307));
#22425=CARTESIAN_POINT('Ctrl Pts',(42.6102333432009,42.111162713484,46.0823391853539));
#22426=CARTESIAN_POINT('Ctrl Pts',(42.6014238196071,42.1117393796737,46.0813938655603));
#22427=CARTESIAN_POINT('Ctrl Pts',(42.5824132868096,42.1129870884406,46.0794862841292));
#22428=CARTESIAN_POINT('Ctrl Pts',(42.5722105379181,42.113658760048,46.0785445454569));
#22429=CARTESIAN_POINT('Ctrl Pts',(42.5444693575738,42.1154908022985,46.0762066897057));
#22430=CARTESIAN_POINT('Ctrl Pts',(42.5269189042309,42.1166561124127,46.0749691813575));
#22431=CARTESIAN_POINT('Ctrl Pts',(42.4325784839858,42.1229554852961,46.0696127972839));
#22432=CARTESIAN_POINT('Ctrl Pts',(42.3556205371879,42.1282240791879,46.0698487447964));
#22433=CARTESIAN_POINT('Ctrl Pts',(42.1492547754344,42.1426873278712,46.0828298934952));
#22434=CARTESIAN_POINT('Ctrl Pts',(42.0207780564953,42.152068522268,46.1040567560623));
#22435=CARTESIAN_POINT('Ctrl Pts',(41.8332331090855,42.1658143695247,46.1548795119261));
#22436=CARTESIAN_POINT('Ctrl Pts',(41.7719181695772,42.1703107709796,46.1748399067633));
#22437=CARTESIAN_POINT('Ctrl Pts',(41.7015860372479,42.1753869644381,46.2017013676445));
#22438=CARTESIAN_POINT('Ctrl Pts',(41.6914931497129,42.1761133732053,46.2056538541874));
#22439=CARTESIAN_POINT('Ctrl Pts',(41.6759820780979,42.1772259990183,46.2118794461265));
#22440=CARTESIAN_POINT('Ctrl Pts',(41.6705402614033,42.177615630992,46.2140925112233));
#22441=CARTESIAN_POINT('Ctrl Pts',(41.6605013426352,42.1783329759775,46.2182286560142));
#22442=CARTESIAN_POINT('Ctrl Pts',(41.6559015905259,42.1786610842978,46.2201446844045));
#22443=CARTESIAN_POINT('Ctrl Pts',(41.6454165529065,42.1794077349973,46.2245599817978));
#22444=CARTESIAN_POINT('Ctrl Pts',(41.6395362303249,42.1798255786509,46.2270707022663));
#22445=CARTESIAN_POINT('Ctrl Pts',(41.6241509696908,42.1809167353337,46.2337303737719));
#22446=CARTESIAN_POINT('Ctrl Pts',(41.6146666665027,42.1815872832902,46.2379268808921));
#22447=CARTESIAN_POINT('Ctrl Pts',(41.5391454724107,42.1869134609174,46.2720735401987));
#22448=CARTESIAN_POINT('Ctrl Pts',(41.474803088873,42.1913709102639,46.3056524631706));
#22449=CARTESIAN_POINT('Ctrl Pts',(41.3149749064669,42.2026153057761,46.4008906360139));
#22450=CARTESIAN_POINT('Ctrl Pts',(41.2227715628433,42.2092828097478,46.4674973401075));
#22451=CARTESIAN_POINT('Ctrl Pts',(41.0731394476817,42.2212478096591,46.5971057254677));
#22452=CARTESIAN_POINT('Ctrl Pts',(41.0130251898619,42.2264422950811,46.6565084654121));
#22453=CARTESIAN_POINT('Ctrl Pts',(40.945328082262,42.2329327445638,46.7328057006051));
#22454=CARTESIAN_POINT('Ctrl Pts',(40.9338379386411,42.2340588076252,46.7461178055265));
#22455=CARTESIAN_POINT('Ctrl Pts',(40.9160104377474,42.2358461799329,46.7673522819909));
#22456=CARTESIAN_POINT('Ctrl Pts',(40.9095506574443,42.23650245671,46.7751709636296));
#22457=CARTESIAN_POINT('Ctrl Pts',(40.8975577628057,42.2377373921983,46.7899220898925));
#22458=CARTESIAN_POINT('Ctrl Pts',(40.8920102037896,42.2383154448917,46.7968424896431));
#22459=CARTESIAN_POINT('Ctrl Pts',(40.879679624264,42.2396158228637,46.8124437381098));
#22460=CARTESIAN_POINT('Ctrl Pts',(40.8729228903293,42.2403391712661,46.8211448720999));
#22461=CARTESIAN_POINT('Ctrl Pts',(40.8558882521919,42.2421908917947,46.8434738176695));
#22462=CARTESIAN_POINT('Ctrl Pts',(40.8457161927574,42.2433233556235,46.8571808040224));
#22463=CARTESIAN_POINT('Ctrl Pts',(40.76444525678,42.2525949042985,46.9697868261324));
#22464=CARTESIAN_POINT('Ctrl Pts',(40.702689985873,42.2610918800934,47.0750636232511));
#22465=CARTESIAN_POINT('Ctrl Pts',(40.6140074355371,42.27603628677,47.2654498846551));
#22466=CARTESIAN_POINT('Ctrl Pts',(40.5822731484203,42.2823799074249,47.3479243482902));
#22467=CARTESIAN_POINT('Ctrl Pts',(40.5388034807396,42.292804990859,47.4890951116254));
#22468=CARTESIAN_POINT('Ctrl Pts',(40.5239429427125,42.2969417156182,47.5466924834733));
#22469=CARTESIAN_POINT('Ctrl Pts',(40.5095847950574,42.3016666833414,47.6153101928554));
#22470=CARTESIAN_POINT('Ctrl Pts',(40.5074905880706,42.3023799760855,47.6257487030368));
#22471=CARTESIAN_POINT('Ctrl Pts',(40.5043828017806,42.3034768408688,47.6419329363921));
#22472=CARTESIAN_POINT('Ctrl Pts',(40.5033087288179,42.3038636815727,47.6476666233743));
#22473=CARTESIAN_POINT('Ctrl Pts',(40.5013645695192,42.3045785211562,47.6583116401143));
#22474=CARTESIAN_POINT('Ctrl Pts',(40.5004875242647,42.3049068920747,47.6632214547396));
#22475=CARTESIAN_POINT('Ctrl Pts',(40.4985197223067,42.3056575123142,47.6744897430042));
#22476=CARTESIAN_POINT('Ctrl Pts',(40.497441810224,42.30607903305,47.6808503308051));
#22477=CARTESIAN_POINT('Ctrl Pts',(40.4946829493129,42.3071862889506,47.6976407822273));
#22478=CARTESIAN_POINT('Ctrl Pts',(40.4930557040947,42.3078691252827,47.7080794207947));
#22479=CARTESIAN_POINT('Ctrl Pts',(40.4778536262782,42.3145619144477,47.8111563757288));
#22480=CARTESIAN_POINT('Ctrl Pts',(40.4709523081264,42.320239481112,47.9046666910671));
#22481=CARTESIAN_POINT('Ctrl Pts',(40.4707326658507,42.3353503593733,48.1568250863074));
#22482=CARTESIAN_POINT('Ctrl Pts',(40.4901284879639,42.3446521508147,48.3147276882422));
#22483=CARTESIAN_POINT('Ctrl Pts',(40.5355259498835,42.3563944593319,48.4960729318445));
#22484=CARTESIAN_POINT('Ctrl Pts',(40.5430435955585,42.3581988458114,48.5235118108636));
#22485=CARTESIAN_POINT('Ctrl Pts',(40.5544009834311,42.3607495104922,48.5616362721644));
#22486=CARTESIAN_POINT('Ctrl Pts',(40.5577326953223,42.3614793147686,48.5724702623754));
#22487=CARTESIAN_POINT('Ctrl Pts',(40.5636815291388,42.3627516018686,48.5912246631112));
#22488=CARTESIAN_POINT('Ctrl Pts',(40.5662549323146,42.3632926400475,48.599158703337));
#22489=CARTESIAN_POINT('Ctrl Pts',(40.5717318621456,42.3644251476594,48.6156787477004));
#22490=CARTESIAN_POINT('Ctrl Pts',(40.5746446015717,42.3650169101352,48.6242614588041));
#22491=CARTESIAN_POINT('Ctrl Pts',(40.581700850075,42.3664261751426,48.6445817986773));
#22492=CARTESIAN_POINT('Ctrl Pts',(40.5858976539058,42.3672454311106,48.6563003575406));
#22493=CARTESIAN_POINT('Ctrl Pts',(40.6004800506452,42.3700302379984,48.6958093563631));
#22494=CARTESIAN_POINT('Ctrl Pts',(40.6113927561166,42.3720132518584,48.7233993840596));
#22495=CARTESIAN_POINT('Ctrl Pts',(40.6579607594428,42.3800963704878,48.8336317904666));
#22496=CARTESIAN_POINT('Ctrl Pts',(40.6987387612596,42.3863641146625,48.9139742710991));
#22497=CARTESIAN_POINT('Ctrl Pts',(40.7891386014527,42.3988307694079,49.0649218736079));
#22498=CARTESIAN_POINT('Ctrl Pts',(40.8381884884264,42.4050056605702,49.135639605686));
#22499=CARTESIAN_POINT('Ctrl Pts',(40.9388159901847,42.4164724175829,49.2618130969654));
#22500=CARTESIAN_POINT('Ctrl Pts',(40.9892661233009,42.421768686245,49.3179770682951));
#22501=CARTESIAN_POINT('Ctrl Pts',(41.050287381502,42.4275654919543,49.3783783933363));
#22502=CARTESIAN_POINT('Ctrl Pts',(41.0577529283942,42.4282650383196,49.3856492912272));
#22503=CARTESIAN_POINT('Ctrl Pts',(41.0699043113111,42.429387651067,49.3972934858881));
#22504=CARTESIAN_POINT('Ctrl Pts',(41.0745535453387,42.4298134530209,49.4017044358679));
#22505=CARTESIAN_POINT('Ctrl Pts',(41.0828574677388,42.4305672475333,49.4095045040463));
#22506=CARTESIAN_POINT('Ctrl Pts',(41.0865033973776,42.4308959247206,49.4129027121736));
#22507=CARTESIAN_POINT('Ctrl Pts',(41.0944674049044,42.4316088995569,49.4202681373253));
#22508=CARTESIAN_POINT('Ctrl Pts',(41.0987904189152,42.4319927824082,49.4242298154117));
#22509=CARTESIAN_POINT('Ctrl Pts',(41.1111178473789,42.4330788263269,49.4354238845152));
#22510=CARTESIAN_POINT('Ctrl Pts',(41.1191651087773,42.4337775461156,49.442609069024));
#22511=CARTESIAN_POINT('Ctrl Pts',(41.1746484356022,42.4385289027755,49.4913183638746));
#22512=CARTESIAN_POINT('Ctrl Pts',(41.2240402379247,42.4424317002741,49.5305676509149));
#22513=CARTESIAN_POINT('Ctrl Pts',(41.3792013342771,42.4540417539977,49.641912464604));
#22514=CARTESIAN_POINT('Ctrl Pts',(41.4902937618086,42.4615218099984,49.7059728287113));
#22515=CARTESIAN_POINT('Ctrl Pts',(41.6680250795623,42.4733250684864,49.7861269607951));
#22516=CARTESIAN_POINT('Ctrl Pts',(41.7305183552398,42.4774429182762,49.8104771088016));
#22517=CARTESIAN_POINT('Ctrl Pts',(41.7941388473837,42.4816651137235,49.8315225416714));
#22518=CARTESIAN_POINT('Ctrl Pts',(41.7941387803776,42.6541583936299,49.831522519506));
#22519=CARTESIAN_POINT('Ctrl Pts',(41.7609009518026,42.652070389834,49.8205275624997));
#22520=CARTESIAN_POINT('Ctrl Pts',(41.7279586839609,42.6499820599924,49.8086265893831));
#22521=CARTESIAN_POINT('Ctrl Pts',(41.5956548730879,42.6414642847965,49.756713017299));
#22522=CARTESIAN_POINT('Ctrl Pts',(41.4994045378027,42.6349506160875,49.7093668430316));
#22523=CARTESIAN_POINT('Ctrl Pts',(41.3917602407269,42.6269721619504,49.6447904877291));
#22524=CARTESIAN_POINT('Ctrl Pts',(41.3760716721312,42.6257913447037,49.6350699991745));
#22525=CARTESIAN_POINT('Ctrl Pts',(41.3518254647877,42.6239368557057,49.6195614701564));
#22526=CARTESIAN_POINT('Ctrl Pts',(41.3431704957749,42.6232688847087,49.6139270751799));
#22527=CARTESIAN_POINT('Ctrl Pts',(41.3279215831576,42.6220811364806,49.6038247599118));
#22528=CARTESIAN_POINT('Ctrl Pts',(41.3213092349631,42.6215624262371,49.5993849513433));
#22529=CARTESIAN_POINT('Ctrl Pts',(41.3061330323522,42.6203633166099,49.589058088627));
#22530=CARTESIAN_POINT('Ctrl Pts',(41.2975889392358,42.6196818450353,49.5831425702874));
#22531=CARTESIAN_POINT('Ctrl Pts',(41.2741742783418,42.6177963749581,49.566649930126));
#22532=CARTESIAN_POINT('Ctrl Pts',(41.2594056709308,42.6165869435133,49.5559306207276));
#22533=CARTESIAN_POINT('Ctrl Pts',(41.1719468499182,42.6093006096093,49.4905371539673));
#22534=CARTESIAN_POINT('Ctrl Pts',(41.1030560339781,42.6030321492513,49.4309952944857));
#22535=CARTESIAN_POINT('Ctrl Pts',(40.9243428172365,42.5852678196432,49.2529952347166));
#22536=CARTESIAN_POINT('Ctrl Pts',(40.8247891827718,42.5735042162092,49.125287031941));
#22537=CARTESIAN_POINT('Ctrl Pts',(40.7342135112047,42.5613480654729,48.9731121728331));
#22538=CARTESIAN_POINT('Ctrl Pts',(40.7263033633215,42.5602717528433,48.9594433445829));
#22539=CARTESIAN_POINT('Ctrl Pts',(40.7126304185622,42.5583868133458,48.9351325300023));
#22540=CARTESIAN_POINT('Ctrl Pts',(40.7067983192092,42.5575744873042,48.9245307131735));
#22541=CARTESIAN_POINT('Ctrl Pts',(40.698159436616,42.5563592574608,48.9084706398389));
#22542=CARTESIAN_POINT('Ctrl Pts',(40.6952784460699,42.5559519130763,48.9030529512611));
#22543=CARTESIAN_POINT('Ctrl Pts',(40.6903375899028,42.5552498188499,48.8936537883733));
#22544=CARTESIAN_POINT('Ctrl Pts',(40.6882657150764,42.5549543223757,48.8896788123023));
#22545=CARTESIAN_POINT('Ctrl Pts',(40.6835125403024,42.5542738955873,48.8804815822695));
#22546=CARTESIAN_POINT('Ctrl Pts',(40.6808412092165,42.5538895931239,48.8752542889642));
#22547=CARTESIAN_POINT('Ctrl Pts',(40.6734469733955,42.5528202735524,48.8606206970058));
#22548=CARTESIAN_POINT('Ctrl Pts',(40.6687770405337,42.5521384591879,48.8511876494182));
#22549=CARTESIAN_POINT('Ctrl Pts',(40.6423176908154,42.5482347511193,48.7966223103786));
#22550=CARTESIAN_POINT('Ctrl Pts',(40.6222143640819,42.5451061107667,48.7506886160387));
#22551=CARTESIAN_POINT('Ctrl Pts',(40.5464705896604,42.5323775971079,48.5574529036845));
#22552=CARTESIAN_POINT('Ctrl Pts',(40.5071739215705,42.523264081888,48.4044011422224));
#22553=CARTESIAN_POINT('Ctrl Pts',(40.4783569354245,42.5095998207401,48.1823444814838));
#22554=CARTESIAN_POINT('Ctrl Pts',(40.4732158323177,42.5054724483302,48.1160297848249));
#22555=CARTESIAN_POINT('Ctrl Pts',(40.4710832469472,42.5001853991219,48.0330909520352));
#22556=CARTESIAN_POINT('Ctrl Pts',(40.4708707736736,42.4991275403952,48.0165907249398));
#22557=CARTESIAN_POINT('Ctrl Pts',(40.4708695389681,42.4974241211575,47.9901855699998));
#22558=CARTESIAN_POINT('Ctrl Pts',(40.470945355125,42.4967828133157,47.9802812344377));
#22559=CARTESIAN_POINT('Ctrl Pts',(40.4712341389415,42.4955605003437,47.9614763859268));
#22560=CARTESIAN_POINT('Ctrl Pts',(40.4714324580168,42.4949799707037,47.952575880103));
#22561=CARTESIAN_POINT('Ctrl Pts',(40.4720247824293,42.4936525711461,47.9322966418178));
#22562=CARTESIAN_POINT('Ctrl Pts',(40.472457926531,42.4929044917547,47.9209194726211));
#22563=CARTESIAN_POINT('Ctrl Pts',(40.4741019567423,42.4905908045723,47.8858950943901));
#22564=CARTESIAN_POINT('Ctrl Pts',(40.4756474802739,42.4890147993743,47.8622665721702));
#22565=CARTESIAN_POINT('Ctrl Pts',(40.4853499042818,42.481226002824,47.7466522358662));
#22566=CARTESIAN_POINT('Ctrl Pts',(40.4996684931085,42.4748238418407,47.6553177569385));
#22567=CARTESIAN_POINT('Ctrl Pts',(40.539991294348,42.4621705760943,47.4809439606581));
#22568=CARTESIAN_POINT('Ctrl Pts',(40.5651804567917,42.4559496928389,47.3979302582343));
#22569=CARTESIAN_POINT('Ctrl Pts',(40.624566617186,42.4440144985864,47.2410865388286));
#22570=CARTESIAN_POINT('Ctrl Pts',(40.6580232508475,42.4383062136994,47.1671534229146));
#22571=CARTESIAN_POINT('Ctrl Pts',(40.7009628580811,42.432121744993,47.0862572916244));
#22572=CARTESIAN_POINT('Ctrl Pts',(40.7059647171079,42.4314163326977,47.0770171079096));
#22573=CARTESIAN_POINT('Ctrl Pts',(40.7141505213841,42.4302862500226,47.0621857981093));
#22574=CARTESIAN_POINT('Ctrl Pts',(40.7172872978379,42.4298587858299,47.0565690768457));
#22575=CARTESIAN_POINT('Ctrl Pts',(40.7229043664715,42.4291032778905,47.04662827826));
#22576=CARTESIAN_POINT('Ctrl Pts',(40.7253733834617,42.4287745359542,47.0422980103479));
#22577=CARTESIAN_POINT('Ctrl Pts',(40.7307729155486,42.4280628452155,47.032912809011));
#22578=CARTESIAN_POINT('Ctrl Pts',(40.7337096233356,42.4276803002181,47.0278615955998));
#22579=CARTESIAN_POINT('Ctrl Pts',(40.7420866743934,42.4266015744032,47.013602339998));
#22580=CARTESIAN_POINT('Ctrl Pts',(40.7475808068098,42.4259087631971,47.0044259135753));
#22581=CARTESIAN_POINT('Ctrl Pts',(40.7847641284604,42.4213132502957,46.9434773406724));
#22582=CARTESIAN_POINT('Ctrl Pts',(40.8188087867542,42.4175493506,46.8931743555525));
#22583=CARTESIAN_POINT('Ctrl Pts',(40.9076216851214,42.4085210498048,46.7744316383732));
#22584=CARTESIAN_POINT('Ctrl Pts',(40.9647865687304,42.4033371474799,46.7079572147242));
#22585=CARTESIAN_POINT('Ctrl Pts',(41.1112991766687,42.3908706054489,46.5593544237548));
#22586=CARTESIAN_POINT('Ctrl Pts',(41.2042457298506,42.3835591401598,46.4813244026563));
#22587=CARTESIAN_POINT('Ctrl Pts',(41.3179479988541,42.3747828562728,46.4028155797908));
#22588=CARTESIAN_POINT('Ctrl Pts',(41.3321388572537,42.3736907149887,46.3932930711532));
#22589=CARTESIAN_POINT('Ctrl Pts',(41.3556863785254,42.371882624531,46.3779417147987));
#22590=CARTESIAN_POINT('Ctrl Pts',(41.3649700052253,42.3711708258873,46.3720021737815));
#22591=CARTESIAN_POINT('Ctrl Pts',(41.3818140566204,42.3698809555803,46.3614278858521));
#22592=CARTESIAN_POINT('Ctrl Pts',(41.3893565649688,42.369303944446,46.3567650711569));
#22593=CARTESIAN_POINT('Ctrl Pts',(41.4055867408465,42.3680633962687,46.3468855110679));
#22594=CARTESIAN_POINT('Ctrl Pts',(41.4142838715086,42.3673992892066,46.3416849060366));
#22595=CARTESIAN_POINT('Ctrl Pts',(41.4381575830003,42.3655778593715,46.3276633553057));
#22596=CARTESIAN_POINT('Ctrl Pts',(41.4534139192642,42.3644155741969,46.3189808313745));
#22597=CARTESIAN_POINT('Ctrl Pts',(41.5422434497142,42.3576559827849,46.2700197931112));
#22598=CARTESIAN_POINT('Ctrl Pts',(41.618252644225,42.3518965769761,46.2343711012668));
#22599=CARTESIAN_POINT('Ctrl Pts',(41.7998688851173,42.3382110845038,46.1632227855643));
#22600=CARTESIAN_POINT('Ctrl Pts',(41.9067166666116,42.3302089967473,46.1316914650072));
#22601=CARTESIAN_POINT('Ctrl Pts',(42.0895314665905,42.3169542758542,46.0945257791644));
#22602=CARTESIAN_POINT('Ctrl Pts',(42.1642129545515,42.3116620256094,46.0838502661021));
#22603=CARTESIAN_POINT('Ctrl Pts',(42.2497168103004,42.3058691639686,46.0767043780905));
#22604=CARTESIAN_POINT('Ctrl Pts',(42.2601055067152,42.3051698186053,46.0759208361231));
#22605=CARTESIAN_POINT('Ctrl Pts',(42.276892604627,42.3040475285068,46.0747913950961));
#22606=CARTESIAN_POINT('Ctrl Pts',(42.2832871085363,42.3036218496646,46.0743931587452));
#22607=CARTESIAN_POINT('Ctrl Pts',(42.2946579611768,42.3028682756267,46.0737418560076));
#22608=CARTESIAN_POINT('Ctrl Pts',(42.299633428302,42.3025396961623,46.0734762042283));
#22609=CARTESIAN_POINT('Ctrl Pts',(42.3104645530616,42.301826945031,46.0729399802209));
#22610=CARTESIAN_POINT('Ctrl Pts',(42.3163204405345,42.3014431878226,46.072676817534));
#22611=CARTESIAN_POINT('Ctrl Pts',(42.3329522985102,42.300357537789,46.0720053300256));
#22612=CARTESIAN_POINT('Ctrl Pts',(42.3437308243798,42.2996590834918,46.0716606536693));
#22613=CARTESIAN_POINT('Ctrl Pts',(42.4174842130787,42.294911352532,46.0699210979319));
#22614=CARTESIAN_POINT('Ctrl Pts',(42.4804987093173,42.2910116680776,46.0715208071771));
#22615=CARTESIAN_POINT('Ctrl Pts',(42.6708075327619,42.2794098195746,46.0856993526566));
#22616=CARTESIAN_POINT('Ctrl Pts',(42.7970290810384,42.2719348092528,46.1078441193079));
#22617=CARTESIAN_POINT('Ctrl Pts',(42.9526399110486,42.2621526387475,46.1514137792241));
#22618=CARTESIAN_POINT('Ctrl Pts',(42.9848982487448,42.2600942526379,46.1613657852326));
#22619=CARTESIAN_POINT('Ctrl Pts',(43.0649236823023,42.2548889816222,46.1883735540481));
#22620=CARTESIAN_POINT('Ctrl Pts',(43.1123078643337,42.2517164381873,46.2064753408143));
#22621=CARTESIAN_POINT('Ctrl Pts',(43.1733387324515,42.2474811853246,46.2325906841536));
#22622=CARTESIAN_POINT('Ctrl Pts',(43.1876802100688,42.2464749537834,46.2389354503562));
#22623=CARTESIAN_POINT('Ctrl Pts',(43.210788087629,42.2448349691112,46.2494972647144));
#22624=CARTESIAN_POINT('Ctrl Pts',(43.2196029295151,42.2442049142801,46.2536070941962));
#22625=CARTESIAN_POINT('Ctrl Pts',(43.236467552388,42.2429907151324,46.2616258561156));
#22626=CARTESIAN_POINT('Ctrl Pts',(43.2445219692226,42.2424069408119,46.2655244973582));
#22627=CARTESIAN_POINT('Ctrl Pts',(43.2630805255329,42.2410526852155,46.2746674524518));
#22628=CARTESIAN_POINT('Ctrl Pts',(43.2735644059398,42.2402808149916,46.2799518578051));
#22629=CARTESIAN_POINT('Ctrl Pts',(43.3067400483057,42.23781604646,46.2970555964997));
#22630=CARTESIAN_POINT('Ctrl Pts',(43.3292444192832,42.236110689375,46.3092303946116));
#22631=CARTESIAN_POINT('Ctrl Pts',(43.3815124347247,42.2320687610992,46.3388659641628));
#22632=CARTESIAN_POINT('Ctrl Pts',(43.4110621232873,42.2297200597884,46.3566844255384));
#22633=CARTESIAN_POINT('Ctrl Pts',(43.5201796878129,42.2208042032081,46.4265397405072));
#22634=CARTESIAN_POINT('Ctrl Pts',(43.5963361383991,42.2140736291461,46.4836372669162));
#22635=CARTESIAN_POINT('Ctrl Pts',(43.6770591482021,42.206428225723,46.5540373328247));
#22636=CARTESIAN_POINT('Ctrl Pts',(43.6860767837742,42.2055665345662,46.5620519453292));
#22637=CARTESIAN_POINT('Ctrl Pts',(43.7749316780139,42.197002525794,46.6425280732277));
#22638=CARTESIAN_POINT('Ctrl Pts',(43.8486441076355,42.189290989514,46.7214845249482));
#22639=CARTESIAN_POINT('Ctrl Pts',(43.9255149602306,42.1808349223287,46.8190618069945));
#22640=CARTESIAN_POINT('Ctrl Pts',(43.9354884323182,42.1797288973699,46.8320589794255));
#22641=CARTESIAN_POINT('Ctrl Pts',(43.9491508338691,42.1782029655587,46.8503410381966));
#22642=CARTESIAN_POINT('Ctrl Pts',(43.9529803510777,42.1777740331066,46.85551930264));
#22643=CARTESIAN_POINT('Ctrl Pts',(43.959542839346,42.1770370083119,46.8644866741722));
#22644=CARTESIAN_POINT('Ctrl Pts',(43.9622880816329,42.1767280855286,46.8682666692001));
#22645=CARTESIAN_POINT('Ctrl Pts',(43.9680503139702,42.1760784359588,46.8762617573903));
#22646=CARTESIAN_POINT('Ctrl Pts',(43.971064095289,42.1757379407688,46.8804791048579));
#22647=CARTESIAN_POINT('Ctrl Pts',(43.9784970661807,42.1748962507885,46.8909695906641));
#22648=CARTESIAN_POINT('Ctrl Pts',(43.9828959545468,42.1743964281027,46.8972571293659));
#22649=CARTESIAN_POINT('Ctrl Pts',(43.9993208984981,42.1725229850714,46.9210348744693));
#22650=CARTESIAN_POINT('Ctrl Pts',(44.0110960566988,42.1711652221737,46.9386976563516));
#22651=CARTESIAN_POINT('Ctrl Pts',(44.1016882124214,42.1605701136352,47.0795698752269));
#22652=CARTESIAN_POINT('Ctrl Pts',(44.166562512146,42.1520347784681,47.2112016237231));
#22653=CARTESIAN_POINT('Ctrl Pts',(44.2523591620418,42.1368059234787,47.4504973330234));
#22654=CARTESIAN_POINT('Ctrl Pts',(44.2801876586331,42.1302484117127,47.5549410539981));
#22655=CARTESIAN_POINT('Ctrl Pts',(44.3021296292297,42.1223131890977,47.6779201244869));
#22656=CARTESIAN_POINT('Ctrl Pts',(44.3048986555747,42.1212247858372,47.6947236416833));
#22657=CARTESIAN_POINT('Ctrl Pts',(44.3090899262524,42.119421615162,47.7224404999025));
#22658=CARTESIAN_POINT('Ctrl Pts',(44.3106419301598,42.1187109588467,47.7333334872246));
#22659=CARTESIAN_POINT('Ctrl Pts',(44.3132760897926,42.1174223132936,47.7530267858801));
#22660=CARTESIAN_POINT('Ctrl Pts',(44.3143909280882,42.1168453754762,47.7618224731361));
#22661=CARTESIAN_POINT('Ctrl Pts',(44.3166514757714,42.1156040463651,47.7806996946924));
#22662=CARTESIAN_POINT('Ctrl Pts',(44.3177783541332,42.1149390781362,47.7907831717692));
#22663=CARTESIAN_POINT('Ctrl Pts',(44.3206436294494,42.1131128394222,47.8183937738161));
#22664=CARTESIAN_POINT('Ctrl Pts',(44.3222215811193,42.1119465624861,47.8359361994197));
#22665=CARTESIAN_POINT('Ctrl Pts',(44.3300199215587,42.1051025662833,47.9383272623535));
#22666=CARTESIAN_POINT('Ctrl Pts',(44.3308613389443,42.099257844589,48.0234795864345));
#22667=CARTESIAN_POINT('Ctrl Pts',(44.319499291407,42.0850623748474,48.225364491383));
#22668=CARTESIAN_POINT('Ctrl Pts',(44.3022756720269,42.0766177001956,48.3414837930243));
#22669=CARTESIAN_POINT('Ctrl Pts',(44.2585218460129,42.0634782662563,48.52162854368));
#22670=CARTESIAN_POINT('Ctrl Pts',(44.2389054284624,42.0587033003943,48.5870508387798));
#22671=CARTESIAN_POINT('Ctrl Pts',(44.2123661714189,42.0533968537077,48.6610435092885));
#22672=CARTESIAN_POINT('Ctrl Pts',(44.2087937437583,42.0527021929845,48.6707569340298));
#22673=CARTESIAN_POINT('Ctrl Pts',(44.202890647127,42.0515859241476,48.6864172611924));
#22674=CARTESIAN_POINT('Ctrl Pts',(44.2006083686509,42.0511616276561,48.6923820098819));
#22675=CARTESIAN_POINT('Ctrl Pts',(44.1964933872782,42.0504095445521,48.7029785746101));
#22676=CARTESIAN_POINT('Ctrl Pts',(44.1946723249955,42.0500810844624,48.7076147360727));
#22677=CARTESIAN_POINT('Ctrl Pts',(44.1906635597271,42.0493674833538,48.7177054466541));
#22678=CARTESIAN_POINT('Ctrl Pts',(44.1884688806253,42.0489827651985,48.7231570767106));
#22679=CARTESIAN_POINT('Ctrl Pts',(44.1821499386006,42.0478916147088,48.7386487403222));
#22680=CARTESIAN_POINT('Ctrl Pts',(44.1779657295315,42.0471886761076,48.7486643060134));
#22681=CARTESIAN_POINT('Ctrl Pts',(44.1481655485945,42.0423126859851,48.8183366071522));
#22682=CARTESIAN_POINT('Ctrl Pts',(44.119633903019,42.0382986502641,48.8767090431292));
#22683=CARTESIAN_POINT('Ctrl Pts',(44.0251891504439,42.0264479031388,49.0475029895595));
#22684=CARTESIAN_POINT('Ctrl Pts',(43.950790536409,42.0188365505356,49.154795686159));
#22685=CARTESIAN_POINT('Ctrl Pts',(43.8166746619035,42.0063192085236,49.31162868257));
#22686=CARTESIAN_POINT('Ctrl Pts',(43.7638271258525,42.00161991698,49.3664956801145));
#22687=CARTESIAN_POINT('Ctrl Pts',(43.6949825788593,41.9956619456997,49.4299897075119));
#22688=CARTESIAN_POINT('Ctrl Pts',(43.6819227517177,41.9945385959975,49.4417088711395));
#22689=CARTESIAN_POINT('Ctrl Pts',(43.6609960437561,41.9927482405143,49.4599781716692));
#22690=CARTESIAN_POINT('Ctrl Pts',(43.6532335616526,41.9920861874737,49.4666468277555));
#22691=CARTESIAN_POINT('Ctrl Pts',(43.6386536138436,41.9908462753185,49.4789720245611));
#22692=CARTESIAN_POINT('Ctrl Pts',(43.6318495055318,41.9902690726206,49.4846440030623));
#22693=CARTESIAN_POINT('Ctrl Pts',(43.6165975935941,41.9889782647441,49.4971811328279));
#22694=CARTESIAN_POINT('Ctrl Pts',(43.6081303136521,41.9882637013066,49.5040220032294));
#22695=CARTESIAN_POINT('Ctrl Pts',(43.5830545021161,41.9861531993344,49.5239328266083));
#22696=CARTESIAN_POINT('Ctrl Pts',(43.5662890096734,41.9847493390159,49.5368015812861));
#22697=CARTESIAN_POINT('Ctrl Pts',(43.5276460181946,41.9815285913494,49.5654663822261));
#22698=CARTESIAN_POINT('Ctrl Pts',(43.505642122205,41.9797052513742,49.5810837773764));
#22699=CARTESIAN_POINT('Ctrl Pts',(43.4304131414429,41.9735054225005,49.6321395592134));
#22700=CARTESIAN_POINT('Ctrl Pts',(43.3757599899359,41.9690554288254,49.6653893990819));
#22701=CARTESIAN_POINT('Ctrl Pts',(43.2164183584837,41.9562666784319,49.7517905489689));
#22702=CARTESIAN_POINT('Ctrl Pts',(43.1083929651652,41.9477965963403,49.7981899265001));
#22703=CARTESIAN_POINT('Ctrl Pts',(42.942703813865,41.935510412296,49.8520945381106));
#22704=CARTESIAN_POINT('Ctrl Pts',(42.8878247836764,41.9315531232386,49.867300167906));
#22705=CARTESIAN_POINT('Ctrl Pts',(42.8226661425047,41.9270436084813,49.8822844083522));
#22706=CARTESIAN_POINT('Ctrl Pts',(42.8129665139945,41.9263771847094,49.8844362367873));
#22707=CARTESIAN_POINT('Ctrl Pts',(42.7971265585748,41.9252972850791,49.8878220967214));
#22708=CARTESIAN_POINT('Ctrl Pts',(42.790996226322,41.9248813895836,49.8891013011853));
#22709=CARTESIAN_POINT('Ctrl Pts',(42.779986111754,41.9241382353002,49.8913428689186));
#22710=CARTESIAN_POINT('Ctrl Pts',(42.775108752777,41.9238103689161,49.8923162310336));
#22711=CARTESIAN_POINT('Ctrl Pts',(42.7643635393785,41.9230910101079,49.8944174484557));
#22712=CARTESIAN_POINT('Ctrl Pts',(42.7584941849696,41.9226999948541,49.8955369106312));
#22713=CARTESIAN_POINT('Ctrl Pts',(42.7414907469936,41.9215725314157,49.8986981749699));
#22714=CARTESIAN_POINT('Ctrl Pts',(42.7303435468655,41.920839951727,49.9006693152455));
#22715=CARTESIAN_POINT('Ctrl Pts',(42.6386687406261,41.9148642360215,49.91604910605));
#22716=CARTESIAN_POINT('Ctrl Pts',(42.5573710276034,41.9098734741224,49.924433619399));
#22717=CARTESIAN_POINT('Ctrl Pts',(42.3504074242769,41.8974057694764,49.9325695346165));
#22718=CARTESIAN_POINT('Ctrl Pts',(42.2248590663551,41.8900454592222,49.925255854848));
#22719=CARTESIAN_POINT('Ctrl Pts',(42.0369512034123,41.8784335553712,49.8957662132446));
#22720=CARTESIAN_POINT('Ctrl Pts',(41.9735447531489,41.8744135933015,49.8825165486961));
#22721=CARTESIAN_POINT('Ctrl Pts',(41.894473350856,41.8692082285989,49.8617934204995));
#22722=CARTESIAN_POINT('Ctrl Pts',(41.8780762246925,41.86811827093,49.8572634375709));
#22723=CARTESIAN_POINT('Ctrl Pts',(41.8521236157303,41.8663753929775,49.8497227735046));
#22724=CARTESIAN_POINT('Ctrl Pts',(41.8425277329969,41.8657270858545,49.846853414999));
#22725=CARTESIAN_POINT('Ctrl Pts',(41.8253134753806,41.8645568828941,49.841559628887));
#22726=CARTESIAN_POINT('Ctrl Pts',(41.8176869532196,41.8640358880018,49.8391623040474));
#22727=CARTESIAN_POINT('Ctrl Pts',(41.8047558058709,41.8631480883241,49.83500902626));
#22728=CARTESIAN_POINT('Ctrl Pts',(41.7994434842431,41.8627820907004,49.8332772967566));
#22729=CARTESIAN_POINT('Ctrl Pts',(41.7941388317731,41.8624153300426,49.8315225365075));
#22730=CARTESIAN_POINT('Origin',(42.4,48.4493818343519,48.));
#22731=CARTESIAN_POINT('',(41.7941391176755,40.8966643233312,49.8315226310829));
#22732=CARTESIAN_POINT('',(41.7941388317924,41.0669118624314,49.8315225365138));
#22733=CARTESIAN_POINT('',(41.7941388317924,48.4493818343519,49.8315225365138));
#22734=CARTESIAN_POINT('',(40.4708703149926,41.5327745867846,48.0011024170354));
#22735=CARTESIAN_POINT('Ctrl Pts',(41.7941391176755,40.8966643233312,49.831522631083));
#22736=CARTESIAN_POINT('Ctrl Pts',(41.8581185305211,40.9014506186217,49.8526867831712));
#22737=CARTESIAN_POINT('Ctrl Pts',(41.923203389598,40.9061877965546,49.8704973808751));
#22738=CARTESIAN_POINT('Ctrl Pts',(42.0043953511471,40.9118383466694,49.88819586063));
#22739=CARTESIAN_POINT('Ctrl Pts',(42.0197007163529,40.912892311347,49.8913379230974));
#22740=CARTESIAN_POINT('Ctrl Pts',(42.0412423446147,40.9143584412164,49.8954881582493));
#22741=CARTESIAN_POINT('Ctrl Pts',(42.0474474720219,40.9147787593746,49.8966520848971));
#22742=CARTESIAN_POINT('Ctrl Pts',(42.0586772025161,40.9155356720216,49.8987014860313));
#22743=CARTESIAN_POINT('Ctrl Pts',(42.0636998085074,40.9158728519888,49.8995975280238));
#22744=CARTESIAN_POINT('Ctrl Pts',(42.0739835353635,40.9165603709582,49.9013900975472));
#22745=CARTESIAN_POINT('Ctrl Pts',(42.079244913191,40.9169106024865,49.9022847353325));
#22746=CARTESIAN_POINT('Ctrl Pts',(42.092780018769,40.9178078452656,49.9045284750944));
#22747=CARTESIAN_POINT('Ctrl Pts',(42.1010590553984,40.9183530743935,49.9058455203013));
#22748=CARTESIAN_POINT('Ctrl Pts',(42.1359511288381,40.9206368578791,49.9111632562143));
#22749=CARTESIAN_POINT('Ctrl Pts',(42.1626392193267,40.9223492231011,49.9146610232021));
#22750=CARTESIAN_POINT('Ctrl Pts',(42.2357217950739,40.9269659906813,49.9226875573822));
#22751=CARTESIAN_POINT('Ctrl Pts',(42.2822227046178,40.9298244628309,49.9260955001744));
#22752=CARTESIAN_POINT('Ctrl Pts',(42.4700533778608,40.9412117768441,49.9330322234343));
#22753=CARTESIAN_POINT('Ctrl Pts',(42.6114463742316,40.9494544976037,49.9227098379474));
#22754=CARTESIAN_POINT('Ctrl Pts',(42.8121119432309,40.9619279698461,49.8856401608799));
#22755=CARTESIAN_POINT('Ctrl Pts',(42.8731805425021,40.9658259841865,49.8712493211526));
#22756=CARTESIAN_POINT('Ctrl Pts',(42.9496175863159,40.9708922245715,49.8492556864682));
#22757=CARTESIAN_POINT('Ctrl Pts',(42.9657372610522,40.9719713043977,49.8443880848739));
#22758=CARTESIAN_POINT('Ctrl Pts',(42.9913060365639,40.9737009302023,49.8363004458457));
#22759=CARTESIAN_POINT('Ctrl Pts',(43.0007976710782,40.9743469874377,49.8332169289235));
#22760=CARTESIAN_POINT('Ctrl Pts',(43.0178563342052,40.9755154899954,49.8275284257964));
#22761=CARTESIAN_POINT('Ctrl Pts',(43.0254319380804,40.9760370549094,49.8249497210565));
#22762=CARTESIAN_POINT('Ctrl Pts',(43.0432203348745,40.9772680932921,49.8187708536315));
#22763=CARTESIAN_POINT('Ctrl Pts',(43.0534192064458,40.9779788494558,49.8151317169069));
#22764=CARTESIAN_POINT('Ctrl Pts',(43.0831602139729,40.9800662951778,49.804236463598));
#22765=CARTESIAN_POINT('Ctrl Pts',(43.1026155065284,40.9814506441943,49.7967494222345));
#22766=CARTESIAN_POINT('Ctrl Pts',(43.1465294381284,40.9846195150195,49.7790275937559));
#22767=CARTESIAN_POINT('Ctrl Pts',(43.1709056482116,40.986410195073,49.7686010704173));
#22768=CARTESIAN_POINT('Ctrl Pts',(43.2517696803878,40.9924585867652,49.7320234417323));
#22769=CARTESIAN_POINT('Ctrl Pts',(43.3072011634058,40.9967858856148,49.7036436128271));
#22770=CARTESIAN_POINT('Ctrl Pts',(43.4803451615369,41.0108606910713,49.6041485848714));
#22771=CARTESIAN_POINT('Ctrl Pts',(43.5918630127751,41.0208274688692,49.5231215463907));
#22772=CARTESIAN_POINT('Ctrl Pts',(43.7243233454903,41.0332954200884,49.4033535762986));
#22773=CARTESIAN_POINT('Ctrl Pts',(43.7539386987984,41.0361273786897,49.3748033143166));
#22774=CARTESIAN_POINT('Ctrl Pts',(43.7895630905453,41.0395664894806,49.3381913420326));
#22775=CARTESIAN_POINT('Ctrl Pts',(43.7964500152556,41.0402329148829,49.3310030112076));
#22776=CARTESIAN_POINT('Ctrl Pts',(43.8072210245297,41.0412772305618,49.3195849767576));
#22777=CARTESIAN_POINT('Ctrl Pts',(43.8111422805214,41.0416578542565,49.3153908122778));
#22778=CARTESIAN_POINT('Ctrl Pts',(43.8181033689359,41.0423342202955,49.307878297928));
#22779=CARTESIAN_POINT('Ctrl Pts',(43.8211503087269,41.0426304968696,49.3045668276438));
#22780=CARTESIAN_POINT('Ctrl Pts',(43.8284420233011,41.04334010751,49.2965861945416));
#22781=CARTESIAN_POINT('Ctrl Pts',(43.832675505979,41.0437525886897,49.2919068353246));
#22782=CARTESIAN_POINT('Ctrl Pts',(43.845537737919,41.0450076103139,49.2775489538392));
#22783=CARTESIAN_POINT('Ctrl Pts',(43.8540921455035,41.0458448219212,49.2678039026912));
#22784=CARTESIAN_POINT('Ctrl Pts',(43.873801695274,41.0477817810324,49.2448891337871));
#22785=CARTESIAN_POINT('Ctrl Pts',(43.884879813597,41.0488766397435,49.2316543250378));
#22786=CARTESIAN_POINT('Ctrl Pts',(43.9231571179139,41.0526888437998,49.1846579313957));
#22787=CARTESIAN_POINT('Ctrl Pts',(43.9493959824538,41.0553555861517,49.1501280838907));
#22788=CARTESIAN_POINT('Ctrl Pts',(44.0493472765207,41.0658638629027,49.0089577657068));
#22789=CARTESIAN_POINT('Ctrl Pts',(44.1133935866279,41.0734399193963,48.8958944141878));
#22790=CARTESIAN_POINT('Ctrl Pts',(44.1968236310758,41.0859918736241,48.7063750272404));
#22791=CARTESIAN_POINT('Ctrl Pts',(44.223727933227,41.0907699387044,48.6336837932964));
#22792=CARTESIAN_POINT('Ctrl Pts',(44.2513015484851,41.0968166850214,48.5427114806805));
#22793=CARTESIAN_POINT('Ctrl Pts',(44.256182282602,41.0979449192005,48.5257760696058));
#22794=CARTESIAN_POINT('Ctrl Pts',(44.2635342521272,41.0997414462192,48.498886533775));
#22795=CARTESIAN_POINT('Ctrl Pts',(44.2661593994532,41.100404729799,48.4889752258828));
#22796=CARTESIAN_POINT('Ctrl Pts',(44.2709054014978,41.1016459550314,48.4704615056965));
#22797=CARTESIAN_POINT('Ctrl Pts',(44.2730462525148,41.1022232311508,48.4618644619581));
#22798=CARTESIAN_POINT('Ctrl Pts',(44.2776811569261,41.1035129284537,48.4426896607373));
#22799=CARTESIAN_POINT('Ctrl Pts',(44.2801451807345,41.1042262978829,48.4321050265027));
#22800=CARTESIAN_POINT('Ctrl Pts',(44.2871160620178,41.1063291323712,48.4009714305734));
#22801=CARTESIAN_POINT('Ctrl Pts',(44.2913762546677,41.1077264298493,48.3803694560659));
#22802=CARTESIAN_POINT('Ctrl Pts',(44.3183048644127,41.1173929101452,48.2384807024407));
#22803=CARTESIAN_POINT('Ctrl Pts',(44.3296243489846,41.1260242166596,48.1153532461277));
#22804=CARTESIAN_POINT('Ctrl Pts',(44.3285528170195,41.144451865538,47.8566579616313));
#22805=CARTESIAN_POINT('Ctrl Pts',(44.3137490867992,41.154229566161,47.7217329695923));
#22806=CARTESIAN_POINT('Ctrl Pts',(44.2816824002445,41.1644655577599,47.5745022806212));
#22807=CARTESIAN_POINT('Ctrl Pts',(44.2782460980373,41.1654974604114,47.5595813400823));
#22808=CARTESIAN_POINT('Ctrl Pts',(44.2730570298807,41.1669656742092,47.5382159876295));
#22809=CARTESIAN_POINT('Ctrl Pts',(44.2714479892359,41.1674096107121,47.5317377464024));
#22810=CARTESIAN_POINT('Ctrl Pts',(44.2685682076344,41.1681845382193,47.5203952847873));
#22811=CARTESIAN_POINT('Ctrl Pts',(44.2673120298438,41.1685163476397,47.5155274878681));
#22812=CARTESIAN_POINT('Ctrl Pts',(44.2646088509248,41.1692173385357,47.5052191589439));
#22813=CARTESIAN_POINT('Ctrl Pts',(44.2631570554076,41.1695862419943,47.4997800118772));
#22814=CARTESIAN_POINT('Ctrl Pts',(44.2591368284411,41.170587677254,47.4849785865974));
#22815=CARTESIAN_POINT('Ctrl Pts',(44.2565214607171,41.1712175667514,47.4756290638882));
#22816=CARTESIAN_POINT('Ctrl Pts',(44.2422174246752,41.1745526281412,47.4259432795249));
#22817=CARTESIAN_POINT('Ctrl Pts',(44.2292836060134,41.177192140311,47.3859737400662));
#22818=CARTESIAN_POINT('Ctrl Pts',(44.1822462704462,41.1857721797249,47.2553395510333));
#22819=CARTESIAN_POINT('Ctrl Pts',(44.1426215129348,41.1915154249538,47.1668169402818));
#22820=CARTESIAN_POINT('Ctrl Pts',(44.0385611170396,41.2045567738288,46.974583264883));
#22821=CARTESIAN_POINT('Ctrl Pts',(43.9706136600271,41.2118576649052,46.8732658295929));
#22822=CARTESIAN_POINT('Ctrl Pts',(43.8773850802449,41.2211429881538,46.7592218104055));
#22823=CARTESIAN_POINT('Ctrl Pts',(43.8607996737614,41.2227702652929,46.7397375646306));
#22824=CARTESIAN_POINT('Ctrl Pts',(43.836128408382,41.2251593869539,46.7118957008343));
#22825=CARTESIAN_POINT('Ctrl Pts',(43.82834631145,41.2259086175819,46.7032716954816));
#22826=CARTESIAN_POINT('Ctrl Pts',(43.8144234679185,41.2272416987186,46.6881200062042));
#22827=CARTESIAN_POINT('Ctrl Pts',(43.8083141753005,41.2278242016569,46.6815637884909));
#22828=CARTESIAN_POINT('Ctrl Pts',(43.7954998634203,41.2290410956961,46.6680027366848));
#22829=CARTESIAN_POINT('Ctrl Pts',(43.7887872809272,41.2296758050924,46.6610054291406));
#22830=CARTESIAN_POINT('Ctrl Pts',(43.7711811586311,41.2313336740226,46.6429273286832));
#22831=CARTESIAN_POINT('Ctrl Pts',(43.7602061638159,41.2323603940855,46.6319272048614));
#22832=CARTESIAN_POINT('Ctrl Pts',(43.7100289143523,41.2370255737875,46.5828357503763));
#22833=CARTESIAN_POINT('Ctrl Pts',(43.669354814801,41.2407298862756,46.5462917728606));
#22834=CARTESIAN_POINT('Ctrl Pts',(43.4900258917407,41.2567547848277,46.3984421606042));
#22835=CARTESIAN_POINT('Ctrl Pts',(43.3379206332399,41.2697118963725,46.3048796378381));
#22836=CARTESIAN_POINT('Ctrl Pts',(43.1346935751145,41.2852412093358,46.2157011588096));
#22837=CARTESIAN_POINT('Ctrl Pts',(43.0936081709804,41.2882917906962,46.1993319572692));
#22838=CARTESIAN_POINT('Ctrl Pts',(43.0424234990391,41.2919547427511,46.1809513497059));
#22839=CARTESIAN_POINT('Ctrl Pts',(43.0328265866957,41.2926356826593,46.1775904778178));
#22840=CARTESIAN_POINT('Ctrl Pts',(43.0177234653792,41.2936976652191,46.1724350067101));
#22841=CARTESIAN_POINT('Ctrl Pts',(43.012235152103,41.294081590945,46.1705891098231));
#22842=CARTESIAN_POINT('Ctrl Pts',(43.0020434660126,41.2947907449261,46.1672123185203));
#22843=CARTESIAN_POINT('Ctrl Pts',(42.9973425390369,41.2951163419757,46.1656748074063));
#22844=CARTESIAN_POINT('Ctrl Pts',(42.9864618227649,41.295866556083,46.1621623644641));
#22845=CARTESIAN_POINT('Ctrl Pts',(42.9802779385651,41.2962904062305,46.1602005106044));
#22846=CARTESIAN_POINT('Ctrl Pts',(42.9608242969471,41.297616217463,46.1541366322295));
#22847=CARTESIAN_POINT('Ctrl Pts',(42.9475197156489,41.2985119382389,46.1501465862393));
#22848=CARTESIAN_POINT('Ctrl Pts',(42.8440925020433,41.3053983926774,46.1203424046129));
#22849=CARTESIAN_POINT('Ctrl Pts',(42.7522273592976,41.31106873742,46.1009814748822));
#22850=CARTESIAN_POINT('Ctrl Pts',(42.4968217993807,41.3264991902148,46.0663362243753));
#22851=CARTESIAN_POINT('Ctrl Pts',(42.332207857763,41.3361364094624,46.065102306466));
#22852=CARTESIAN_POINT('Ctrl Pts',(42.1465764946837,41.3479554843129,46.0874496862799));
#22853=CARTESIAN_POINT('Ctrl Pts',(42.1237798941795,41.3494220885553,46.0906088518849));
#22854=CARTESIAN_POINT('Ctrl Pts',(42.0899223361059,41.3516253703375,46.0959198598464));
#22855=CARTESIAN_POINT('Ctrl Pts',(42.0788143478763,41.3523522595083,46.0977620796102));
#22856=CARTESIAN_POINT('Ctrl Pts',(42.0589648606536,41.3536586949761,46.1012328614315));
#22857=CARTESIAN_POINT('Ctrl Pts',(42.0502172252744,41.3542370614802,46.1028248318007));
#22858=CARTESIAN_POINT('Ctrl Pts',(42.0316722542319,41.3554689142301,46.1063324255448));
#22859=CARTESIAN_POINT('Ctrl Pts',(42.0218781878226,41.3561228863688,46.1082637341229));
#22860=CARTESIAN_POINT('Ctrl Pts',(41.9955930169642,41.3578873778243,46.113659230078));
#22861=CARTESIAN_POINT('Ctrl Pts',(41.9791318959196,41.359002348794,46.117263556315));
#22862=CARTESIAN_POINT('Ctrl Pts',(41.8930448450856,41.3648872532325,46.137298554385));
#22863=CARTESIAN_POINT('Ctrl Pts',(41.8243335716497,41.3697732701749,46.1573751978238));
#22864=CARTESIAN_POINT('Ctrl Pts',(41.6699137041991,41.3811890255286,46.2119760490236));
#22865=CARTESIAN_POINT('Ctrl Pts',(41.5852498792528,41.387773256894,46.2489330625927));
#22866=CARTESIAN_POINT('Ctrl Pts',(41.415093985788,41.4015002727654,46.3382284333001));
#22867=CARTESIAN_POINT('Ctrl Pts',(41.3303572477324,41.4086237939684,46.3914624840049));
#22868=CARTESIAN_POINT('Ctrl Pts',(41.2368948554861,41.4165486229286,46.4608443045582));
#22869=CARTESIAN_POINT('Ctrl Pts',(41.2237958301023,41.4176607624129,46.4708310665137));
#22870=CARTESIAN_POINT('Ctrl Pts',(41.2057419707601,41.419193793046,46.4849646863879));
#22871=CARTESIAN_POINT('Ctrl Pts',(41.2006780681594,41.4196238140539,46.4889701695022));
#22872=CARTESIAN_POINT('Ctrl Pts',(41.1919810062191,41.4203622600533,46.495920700819));
#22873=CARTESIAN_POINT('Ctrl Pts',(41.1883383106288,41.4206715220936,46.4988536449626));
#22874=CARTESIAN_POINT('Ctrl Pts',(41.1807632224527,41.4213145134435,46.50499832273));
#22875=CARTESIAN_POINT('Ctrl Pts',(41.1768327823442,41.4216480613642,46.5082123832679));
#22876=CARTESIAN_POINT('Ctrl Pts',(41.1674556438012,41.4224437706635,46.51594237792));
#22877=CARTESIAN_POINT('Ctrl Pts',(41.1620209467042,41.4229048903603,46.5204728853126));
#22878=CARTESIAN_POINT('Ctrl Pts',(41.1501883291649,41.423909063726,46.5304477165828));
#22879=CARTESIAN_POINT('Ctrl Pts',(41.1438007628363,41.4244512776692,46.5359041668028));
#22880=CARTESIAN_POINT('Ctrl Pts',(41.1258977195987,41.4259720489525,46.551400904881));
#22881=CARTESIAN_POINT('Ctrl Pts',(41.1144653142055,41.426944420053,46.5615367356305));
#22882=CARTESIAN_POINT('Ctrl Pts',(41.0763782681241,41.4301929581844,46.5961210324591));
#22883=CARTESIAN_POINT('Ctrl Pts',(41.0502897676578,41.4324334434746,46.6211841124654));
#22884=CARTESIAN_POINT('Ctrl Pts',(40.9006183386253,41.4454902951244,46.7732944147));
#22885=CARTESIAN_POINT('Ctrl Pts',(40.7943164375551,41.4556954805726,46.9161463978581));
#22886=CARTESIAN_POINT('Ctrl Pts',(40.6868109816384,41.4695093578633,47.1119386162762));
#22887=CARTESIAN_POINT('Ctrl Pts',(40.666071766935,41.4724023354703,47.1531458276636));
#22888=CARTESIAN_POINT('Ctrl Pts',(40.6405024762728,41.4763149254304,47.2088356744813));
#22889=CARTESIAN_POINT('Ctrl Pts',(40.6343377382921,41.4772885326166,47.2226909995008));
#22890=CARTESIAN_POINT('Ctrl Pts',(40.6245322428981,41.4788886105219,47.2454476469767));
#22891=CARTESIAN_POINT('Ctrl Pts',(40.6207934893816,41.4795117182643,47.254306231116));
#22892=CARTESIAN_POINT('Ctrl Pts',(40.6136870707343,41.4807218870179,47.2715018748569));
#22893=CARTESIAN_POINT('Ctrl Pts',(40.6103111556473,41.4813086489769,47.2798352720588));
#22894=CARTESIAN_POINT('Ctrl Pts',(40.6025609293593,41.4826840591227,47.2993576739203));
#22895=CARTESIAN_POINT('Ctrl Pts',(40.5982326778415,41.4834742350113,47.3105644428771));
#22896=CARTESIAN_POINT('Ctrl Pts',(40.5844803926511,41.4860588425968,47.3471862190126));
#22897=CARTESIAN_POINT('Ctrl Pts',(40.5754876363461,41.4878675017102,47.3727585913714));
#22898=CARTESIAN_POINT('Ctrl Pts',(40.5554372704731,41.4922002267333,47.4338595767914));
#22899=CARTESIAN_POINT('Ctrl Pts',(40.5448632185349,41.4947389220043,47.4695343048505));
#22900=CARTESIAN_POINT('Ctrl Pts',(40.4924363865387,41.5088548081407,47.667222849361));
#22901=CARTESIAN_POINT('Ctrl Pts',(40.4707747286394,41.5210116021514,47.8338349804454));
#22902=CARTESIAN_POINT('Ctrl Pts',(40.4708703149926,41.5327745867846,48.0011024170354));
#22903=CARTESIAN_POINT('Ctrl Pts',(40.4708703166185,41.5327747866074,48.0011052584796));
#22904=CARTESIAN_POINT('Ctrl Pts',(40.4708910356162,41.5353179380368,48.0372684133744));
#22905=CARTESIAN_POINT('Ctrl Pts',(40.4719286180371,41.5378363427205,48.0734265716021));
#22906=CARTESIAN_POINT('Ctrl Pts',(40.4750553011039,41.5416089606166,48.1284040113603));
#22907=CARTESIAN_POINT('Ctrl Pts',(40.476405553459,41.5428923869818,48.1472554005316));
#22908=CARTESIAN_POINT('Ctrl Pts',(40.478611137742,41.5446135884969,48.1727788857062));
#22909=CARTESIAN_POINT('Ctrl Pts',(40.4792245864809,41.5450632790307,48.1794701016799));
#22910=CARTESIAN_POINT('Ctrl Pts',(40.4803556963078,41.5458445185021,48.1911369299981));
#22911=CARTESIAN_POINT('Ctrl Pts',(40.480857768946,41.5461768877265,48.1961139390409));
#22912=CARTESIAN_POINT('Ctrl Pts',(40.4818771242539,41.5468245464197,48.2058397630237));
#22913=CARTESIAN_POINT('Ctrl Pts',(40.4823926986165,41.5471399266619,48.2105887324994));
#22914=CARTESIAN_POINT('Ctrl Pts',(40.4835409100536,41.5478168761997,48.2208109325732));
#22915=CARTESIAN_POINT('Ctrl Pts',(40.4841793590307,41.5481781164396,48.2262834172197));
#22916=CARTESIAN_POINT('Ctrl Pts',(40.4859422200879,41.5491368194173,48.2408513244274));
#22917=CARTESIAN_POINT('Ctrl Pts',(40.4871080312627,41.5497320084403,48.2499417320189));
#22918=CARTESIAN_POINT('Ctrl Pts',(40.4925113790291,41.5523309932763,48.2898198245944));
#22919=CARTESIAN_POINT('Ctrl Pts',(40.4974279965344,41.5542998855106,48.3205127176437));
#22920=CARTESIAN_POINT('Ctrl Pts',(40.5108502723839,41.558905790742,48.3930353809672));
#22921=CARTESIAN_POINT('Ctrl Pts',(40.520006677116,41.5615169095456,48.4347286998954));
#22922=CARTESIAN_POINT('Ctrl Pts',(40.5590234336272,41.5710860523173,48.5879368617066));
#22923=CARTESIAN_POINT('Ctrl Pts',(40.5974884784632,41.5778605429286,48.6970064100749));
#22924=CARTESIAN_POINT('Ctrl Pts',(40.6809573254201,41.5899908299084,48.8796135899817));
#22925=CARTESIAN_POINT('Ctrl Pts',(40.7215493280278,41.5952395868679,48.9547923400153));
#22926=CARTESIAN_POINT('Ctrl Pts',(40.7763672505195,41.6017911588872,49.041954925123));
#22927=CARTESIAN_POINT('Ctrl Pts',(40.7859569548367,41.6029200635117,49.056748970379));
#22928=CARTESIAN_POINT('Ctrl Pts',(40.8013859716145,41.604710927223,49.0798512879276));
#22929=CARTESIAN_POINT('Ctrl Pts',(40.8070905800947,41.6053678201035,49.0882486798621));
#22930=CARTESIAN_POINT('Ctrl Pts',(40.8179023232201,41.6066032978008,49.1038968011063));
#22931=CARTESIAN_POINT('Ctrl Pts',(40.8229937142394,41.6071812713189,49.1111581240335));
#22932=CARTESIAN_POINT('Ctrl Pts',(40.8345136167881,41.608480657631,49.127349103891));
#22933=CARTESIAN_POINT('Ctrl Pts',(40.8409687788145,41.6092030866577,49.1362593281865));
#22934=CARTESIAN_POINT('Ctrl Pts',(40.8576047341472,41.6110508650984,49.1588137050245));
#22935=CARTESIAN_POINT('Ctrl Pts',(40.8678903846456,41.6121802764086,49.1723789719563));
#22936=CARTESIAN_POINT('Ctrl Pts',(40.9525487989169,41.6213748629403,49.2810140649258));
#22937=CARTESIAN_POINT('Ctrl Pts',(41.035501606412,41.6297911433942,49.3690312177839));
#22938=CARTESIAN_POINT('Ctrl Pts',(41.1910658328288,41.6445268695145,49.5058223536642));
#22939=CARTESIAN_POINT('Ctrl Pts',(41.2597825688829,41.6507416859,49.5585015669848));
#22940=CARTESIAN_POINT('Ctrl Pts',(41.3667885169207,41.65982324221,49.6296569783237));
#22941=CARTESIAN_POINT('Ctrl Pts',(41.4025277725476,41.662764962641,49.6517740303494));
#22942=CARTESIAN_POINT('Ctrl Pts',(41.4536177261703,41.6668173151942,49.6811272415018));
#22943=CARTESIAN_POINT('Ctrl Pts',(41.4683830515961,41.6679711354929,49.6893543485922));
#22944=CARTESIAN_POINT('Ctrl Pts',(41.4943892194213,41.669970843268,49.7034000704587));
#22945=CARTESIAN_POINT('Ctrl Pts',(41.5055825652418,41.6708211911854,49.7093039984893));
#22946=CARTESIAN_POINT('Ctrl Pts',(41.5223645603684,41.6720798508136,49.717945661478));
#22947=CARTESIAN_POINT('Ctrl Pts',(41.5279094069499,41.6724930975791,49.7207670559632));
#22948=CARTESIAN_POINT('Ctrl Pts',(41.5334875835222,41.6729061325938,49.7235715214273));
#22949=CARTESIAN_POINT('Ctrl Pts',(41.5335072653789,41.6729075898995,49.7235814161896));
#22950=CARTESIAN_POINT('Ctrl Pts',(41.5335468125291,41.6729105180257,49.7236012970858));
#22951=CARTESIAN_POINT('Ctrl Pts',(41.5335666780665,41.6729119888635,49.7236112833344));
#22952=CARTESIAN_POINT('Ctrl Pts',(41.5336065939171,41.6729149441512,49.7236313478524));
#22953=CARTESIAN_POINT('Ctrl Pts',(41.5336266451778,41.6729164286705,49.7236414265902));
#22954=CARTESIAN_POINT('Ctrl Pts',(41.5336669357823,41.672919411564,49.7236616777246));
#22955=CARTESIAN_POINT('Ctrl Pts',(41.5336871741521,41.6729209098655,49.7236718496235));
#22956=CARTESIAN_POINT('Ctrl Pts',(41.5337278412036,41.6729239204862,49.7236922881759));
#22957=CARTESIAN_POINT('Ctrl Pts',(41.533748269972,41.6729254328113,49.7237025548645));
#22958=CARTESIAN_POINT('Ctrl Pts',(41.5337893193495,41.6729284715906,49.7237231837391));
#22959=CARTESIAN_POINT('Ctrl Pts',(41.533809940713,41.6729299980999,49.7237335462957));
#22960=CARTESIAN_POINT('Ctrl Pts',(41.5338513778411,41.6729330654351,49.723754368167));
#22961=CARTESIAN_POINT('Ctrl Pts',(41.5338721937306,41.6729346062695,49.7237648275358));
#22962=CARTESIAN_POINT('Ctrl Pts',(41.5339140228206,41.6729377024681,49.7237858444674));
#22963=CARTESIAN_POINT('Ctrl Pts',(41.5339350356898,41.6729392578071,49.7237964018547));
#22964=CARTESIAN_POINT('Ctrl Pts',(41.5339772614457,41.672942383213,49.7238176161562));
#22965=CARTESIAN_POINT('Ctrl Pts',(41.5339984738186,41.6729439532413,49.723828272803));
#22966=CARTESIAN_POINT('Ctrl Pts',(41.5340411007461,41.6729471081837,49.7238496866831));
#22967=CARTESIAN_POINT('Ctrl Pts',(41.5340625153346,41.6729486930996,49.723860443924));
#22968=CARTESIAN_POINT('Ctrl Pts',(41.5341055489994,41.6729518779859,49.7238820601223));
#22969=CARTESIAN_POINT('Ctrl Pts',(41.5341271681326,41.6729534779596,49.7238929190989));
#22970=CARTESIAN_POINT('Ctrl Pts',(41.5341706132983,41.6729566931377,49.723914739951));
#22971=CARTESIAN_POINT('Ctrl Pts',(41.5341924395709,41.6729583083591,49.7239257019374));
#22972=CARTESIAN_POINT('Ctrl Pts',(41.5342363020941,41.6729615542578,49.7239477303261));
#22973=CARTESIAN_POINT('Ctrl Pts',(41.5342583377425,41.6729631848898,49.7239587964159));
#22974=CARTESIAN_POINT('Ctrl Pts',(41.5343026215585,41.6729664617954,49.7239810342574));
#22975=CARTESIAN_POINT('Ctrl Pts',(41.5343248696589,41.6729681080633,49.7239922059652));
#22976=CARTESIAN_POINT('Ctrl Pts',(41.5343695800479,41.6729714163618,49.7240146558499));
#22977=CARTESIAN_POINT('Ctrl Pts',(41.5343920434813,41.6729730784763,49.7240259345913));
#22978=CARTESIAN_POINT('Ctrl Pts',(41.5344371881827,41.6729764187352,49.7240486003426));
#22979=CARTESIAN_POINT('Ctrl Pts',(41.5344598685596,41.6729780968129,49.7240599868944));
#22980=CARTESIAN_POINT('Ctrl Pts',(41.5345054497366,41.6729814691872,49.7240828695341));
#22981=CARTESIAN_POINT('Ctrl Pts',(41.5345283508829,41.6729831635086,49.7240943657849));
#22982=CARTESIAN_POINT('Ctrl Pts',(41.5345743761216,41.6729865685544,49.724117469056));
#22983=CARTESIAN_POINT('Ctrl Pts',(41.5345975003172,41.6729882792855,49.724129076117));
#22984=CARTESIAN_POINT('Ctrl Pts',(41.5346439747086,41.672991717374,49.7241524025081));
#22985=CARTESIAN_POINT('Ctrl Pts',(41.5346673247705,41.6729934447205,49.7241641217595));
#22986=CARTESIAN_POINT('Ctrl Pts',(41.5347142538249,41.6729969162538,49.7241876739677));
#22987=CARTESIAN_POINT('Ctrl Pts',(41.5347378326906,41.6729986604303,49.7241995068492));
#22988=CARTESIAN_POINT('Ctrl Pts',(41.5347852222905,41.6730021658381,49.7242232877568));
#22989=CARTESIAN_POINT('Ctrl Pts',(41.5348090328349,41.6730039270543,49.7242352356757));
#22990=CARTESIAN_POINT('Ctrl Pts',(41.5348568884404,41.6730074667347,49.724259247951));
#22991=CARTESIAN_POINT('Ctrl Pts',(41.5348809337817,41.6730092452185,49.7242713124359));
#22992=CARTESIAN_POINT('Ctrl Pts',(41.5349292620101,41.673012819655,49.7242955593261));
#22993=CARTESIAN_POINT('Ctrl Pts',(41.5349535448745,41.673014615605,49.7243077417076));
#22994=CARTESIAN_POINT('Ctrl Pts',(41.5350023515116,41.6730182252196,49.7243322260406));
#22995=CARTESIAN_POINT('Ctrl Pts',(41.53502687491,41.6730200388554,49.7243445277916));
#22996=CARTESIAN_POINT('Ctrl Pts',(41.5350761650012,41.6730236840151,49.7243692520219));
#22997=CARTESIAN_POINT('Ctrl Pts',(41.5351009325253,41.6730255155994,49.7243816749053));
#22998=CARTESIAN_POINT('Ctrl Pts',(41.5351507143927,41.6730291969133,49.7244066431291));
#22999=CARTESIAN_POINT('Ctrl Pts',(41.5351757283507,41.6730310466135,49.7244191882629));
#23000=CARTESIAN_POINT('Ctrl Pts',(41.5352260064123,41.6730347644021,49.7244444026158));
#23001=CARTESIAN_POINT('Ctrl Pts',(41.5352512704939,41.6730366324878,49.7244570718102));
#23002=CARTESIAN_POINT('Ctrl Pts',(41.5353020520409,41.6730403872835,49.724482535867));
#23003=CARTESIAN_POINT('Ctrl Pts',(41.5353275692568,41.6730422739739,49.7244953305902));
#23004=CARTESIAN_POINT('Ctrl Pts',(41.5353788602599,41.6730460662116,49.7245210472609));
#23005=CARTESIAN_POINT('Ctrl Pts',(41.5354046340135,41.6730479717551,49.7245339691771));
#23006=CARTESIAN_POINT('Ctrl Pts',(41.535456440713,41.6730518018892,49.7245599415049));
#23007=CARTESIAN_POINT('Ctrl Pts',(41.5354824745391,41.6730537265436,49.7245729923431));
#23008=CARTESIAN_POINT('Ctrl Pts',(41.5355348054584,41.6730575951972,49.7245992245132));
#23009=CARTESIAN_POINT('Ctrl Pts',(41.5355611018867,41.6730595391461,49.7246124054969));
#23010=CARTESIAN_POINT('Ctrl Pts',(41.5356139616158,41.6730634466514,49.7246388997205));
#23011=CARTESIAN_POINT('Ctrl Pts',(41.5356405247149,41.6730654101917,49.724652212844));
#23012=CARTESIAN_POINT('Ctrl Pts',(41.5356939207531,41.6730693570957,49.7246789727882));
#23013=CARTESIAN_POINT('Ctrl Pts',(41.5357207539793,41.6730713404794,49.7246924197372));
#23014=CARTESIAN_POINT('Ctrl Pts',(41.5357746940368,41.6730753273444,49.724719449172));
#23015=CARTESIAN_POINT('Ctrl Pts',(41.5358018005083,41.673077330798,49.7247330314615));
#23016=CARTESIAN_POINT('Ctrl Pts',(41.5358562899825,41.6730813580154,49.7247603329956));
#23017=CARTESIAN_POINT('Ctrl Pts',(41.5358836738819,41.6730833818442,49.7247740526731));
#23018=CARTESIAN_POINT('Ctrl Pts',(41.5359387223972,41.6730874501173,49.7248016310303));
#23019=CARTESIAN_POINT('Ctrl Pts',(41.5359663863995,41.673089494515,49.724815489386));
#23020=CARTESIAN_POINT('Ctrl Pts',(41.5360219987301,41.6730936041886,49.7248433468575));
#23021=CARTESIAN_POINT('Ctrl Pts',(41.5360499472611,41.6730956694782,49.7248573460578));
#23022=CARTESIAN_POINT('Ctrl Pts',(41.5405326392237,41.6734269123859,49.7271025550605));
#23023=CARTESIAN_POINT('Ctrl Pts',(41.5449959295021,41.6737549844919,49.7293164604325));
#23024=CARTESIAN_POINT('Ctrl Pts',(41.5551987785285,41.6745010294112,49.7343281755207));
#23025=CARTESIAN_POINT('Ctrl Pts',(41.5609436864827,41.6749183080931,49.7371148004176));
#23026=CARTESIAN_POINT('Ctrl Pts',(41.5760290881034,41.6760069979231,49.7443398273652));
#23027=CARTESIAN_POINT('Ctrl Pts',(41.5853917653395,41.6766756642317,49.7487318068621));
#23028=CARTESIAN_POINT('Ctrl Pts',(41.6582624608841,41.6818291769998,49.7822027853363));
#23029=CARTESIAN_POINT('Ctrl Pts',(41.7232797262281,41.6861303680353,49.8078919529853));
#23030=CARTESIAN_POINT('Ctrl Pts',(41.7910819634347,41.690456096612,49.8305092118532));
#23031=CARTESIAN_POINT('Ctrl Pts',(41.7926101020481,41.6905535087766,49.8310168381293));
#23032=CARTESIAN_POINT('Ctrl Pts',(41.7941388322699,41.6906508784004,49.8315225366718));
#23033=CARTESIAN_POINT('',(40.4708708172652,41.7025068343519,47.9982242689299));
#23034=CARTESIAN_POINT('Ctrl Pts',(41.7941388317731,41.8624153300426,49.8315225365075));
#23035=CARTESIAN_POINT('Ctrl Pts',(41.7892186830212,41.8620751537533,49.8298949687264));
#23036=CARTESIAN_POINT('Ctrl Pts',(41.7843051319335,41.8617343210511,49.8282475879286));
#23037=CARTESIAN_POINT('Ctrl Pts',(41.7599237344004,41.8600374975222,49.8199637278008));
#23038=CARTESIAN_POINT('Ctrl Pts',(41.7405569098558,41.8586719070556,49.8130362244661));
#23039=CARTESIAN_POINT('Ctrl Pts',(41.6969070890574,41.855552516025,49.7966308099455));
#23040=CARTESIAN_POINT('Ctrl Pts',(41.6726984071991,41.8537928278026,49.786967876266));
#23041=CARTESIAN_POINT('Ctrl Pts',(41.5928156839767,41.8478857162481,49.7531904243072));
#23042=CARTESIAN_POINT('Ctrl Pts',(41.5380881659186,41.8436722457972,49.7269423780626));
#23043=CARTESIAN_POINT('Ctrl Pts',(41.3555549628571,41.8290720271415,49.6285571541991));
#23044=CARTESIAN_POINT('Ctrl Pts',(41.2347856430922,41.818412713764,49.5444537451597));
#23045=CARTESIAN_POINT('Ctrl Pts',(41.0982253084333,41.8057648919477,49.4241389510254));
#23046=CARTESIAN_POINT('Ctrl Pts',(41.072377611227,41.8033430665789,49.4000743799898));
#23047=CARTESIAN_POINT('Ctrl Pts',(41.0403811485847,41.8003246672332,49.3686017337567));
#23048=CARTESIAN_POINT('Ctrl Pts',(41.0336089283717,41.7996845996916,49.3618405102973));
#23049=CARTESIAN_POINT('Ctrl Pts',(41.0229551610083,41.7986761590713,49.3510445605028));
#23050=CARTESIAN_POINT('Ctrl Pts',(41.019040491923,41.7983052838696,49.3470429585196));
#23051=CARTESIAN_POINT('Ctrl Pts',(41.0116383365694,41.797603477322,49.3394102411973));
#23052=CARTESIAN_POINT('Ctrl Pts',(41.008147674562,41.7972723109,49.3357825449606));
#23053=CARTESIAN_POINT('Ctrl Pts',(40.9999402297618,41.7964930593378,49.3271857945718));
#23054=CARTESIAN_POINT('Ctrl Pts',(40.9952356605449,41.7960459109071,49.3222052214658));
#23055=CARTESIAN_POINT('Ctrl Pts',(40.9801341754675,41.794608617292,49.3060461876689));
#23056=CARTESIAN_POINT('Ctrl Pts',(40.9698430787115,41.7936261167636,49.2947690217377));
#23057=CARTESIAN_POINT('Ctrl Pts',(40.9055841622379,41.7874626740857,49.2226519016328));
#23058=CARTESIAN_POINT('Ctrl Pts',(40.8553686886246,41.7825146099197,49.1585653325076));
#23059=CARTESIAN_POINT('Ctrl Pts',(40.7633702271068,41.7727499424644,49.0244940229064));
#23060=CARTESIAN_POINT('Ctrl Pts',(40.7216750842606,41.767941930125,48.9546573638967));
#23061=CARTESIAN_POINT('Ctrl Pts',(40.6389408014605,41.7570796979552,48.7938117786158));
#23062=CARTESIAN_POINT('Ctrl Pts',(40.6003099179131,41.7510014937008,48.7018393035765));
#23063=CARTESIAN_POINT('Ctrl Pts',(40.5636316196754,41.7435992833381,48.5912526374627));
#23064=CARTESIAN_POINT('Ctrl Pts',(40.5585196052753,41.7425183919732,48.5751334074503));
#23065=CARTESIAN_POINT('Ctrl Pts',(40.5504427930779,41.7407251104298,48.5484532451553));
#23066=CARTESIAN_POINT('Ctrl Pts',(40.5473549196674,41.7400167526098,48.5379303132434));
#23067=CARTESIAN_POINT('Ctrl Pts',(40.5419339151009,41.7387305630651,48.5188559932604));
#23068=CARTESIAN_POINT('Ctrl Pts',(40.5395696648142,41.7381537644266,48.5103137085197));
#23069=CARTESIAN_POINT('Ctrl Pts',(40.5346185808692,41.7369108238037,48.4919331240307));
#23070=CARTESIAN_POINT('Ctrl Pts',(40.5320505412383,41.7362440907617,48.4820900850759));
#23071=CARTESIAN_POINT('Ctrl Pts',(40.526958307188,41.7348753964956,48.4619203181699));
#23072=CARTESIAN_POINT('Ctrl Pts',(40.5244413888776,41.734173225229,48.4515921299839));
#23073=CARTESIAN_POINT('Ctrl Pts',(40.5182996512163,41.7323925617641,48.4254521121162));
#23074=CARTESIAN_POINT('Ctrl Pts',(40.5147887323197,41.7313104746275,48.4096146373933));
#23075=CARTESIAN_POINT('Ctrl Pts',(40.4843509256643,41.7213041594941,48.2636219241579));
#23076=CARTESIAN_POINT('Ctrl Pts',(40.4707487026118,41.7119532339184,48.1310819386935));
#23077=CARTESIAN_POINT('Ctrl Pts',(40.4708708148797,41.7024705085611,47.9982268623347));
#23078=CARTESIAN_POINT('Ctrl Pts',(40.4708708172652,41.7025068343519,47.9982242689299));
#23079=CARTESIAN_POINT('Ctrl Pts',(40.4709547042422,41.6965367373028,47.9070906405182));
#23080=CARTESIAN_POINT('Ctrl Pts',(40.4775000933314,41.6905666402537,47.8162440648578));
#23081=CARTESIAN_POINT('Ctrl Pts',(40.4903640311629,41.6845965432046,47.7264437472407));
#23082=CARTESIAN_POINT('Ctrl Pts',(40.4984641755126,41.6808373017878,47.6698984230275));
#23083=CARTESIAN_POINT('Ctrl Pts',(40.5090686524231,41.677078060371,47.6137673003875));
#23084=CARTESIAN_POINT('Ctrl Pts',(40.5221325309265,41.6733188189542,47.5582349883756));
#23085=CARTESIAN_POINT('Ctrl Pts',(40.5376179791024,41.6688627504042,47.4924089980676));
#23086=CARTESIAN_POINT('Ctrl Pts',(40.5565997538975,41.6644066818542,47.4272665547092));
#23087=CARTESIAN_POINT('Ctrl Pts',(40.5790011947558,41.6599506133042,47.3632065419625));
#23088=CARTESIAN_POINT('Ctrl Pts',(40.6013686812249,41.6555012989218,47.2992436264797));
#23089=CARTESIAN_POINT('Ctrl Pts',(40.6271453858133,41.6510519845394,47.2363603479597));
#23090=CARTESIAN_POINT('Ctrl Pts',(40.6562040755905,41.646602670157,47.1749434377494));
#23091=CARTESIAN_POINT('Ctrl Pts',(40.6852283916312,41.6421586189011,47.113599178051));
#23092=CARTESIAN_POINT('Ctrl Pts',(40.7175267728883,41.6377145676452,47.0537182861443));
#23093=CARTESIAN_POINT('Ctrl Pts',(40.7529234645091,41.6332705163893,46.9956686586911));
#23094=CARTESIAN_POINT('Ctrl Pts',(40.7882978569756,41.6288292647901,46.9376556012545));
#23095=CARTESIAN_POINT('Ctrl Pts',(40.826766431711,41.6243880131909,46.8814719405339));
#23096=CARTESIAN_POINT('Ctrl Pts',(40.8681077126806,41.6199467615917,46.8274606288268));
#23097=CARTESIAN_POINT('Ctrl Pts',(40.9094372396547,41.6155067727123,46.7734646734101));
#23098=CARTESIAN_POINT('Ctrl Pts',(40.9536375515899,41.6110667838328,46.7216402328485));
#23099=CARTESIAN_POINT('Ctrl Pts',(41.0004451721161,41.6066267949533,46.6722994160403));
#23100=CARTESIAN_POINT('Ctrl Pts',(41.0472556636165,41.6021865337444,46.6229555728828));
#23101=CARTESIAN_POINT('Ctrl Pts',(41.0966734394862,41.5977462725355,46.5760960122977));
#23102=CARTESIAN_POINT('Ctrl Pts',(41.1483975187492,41.5933060113266,46.5319966669565));
#23103=CARTESIAN_POINT('Ctrl Pts',(41.2001770856412,41.588860986774,46.4878500135114));
#23104=CARTESIAN_POINT('Ctrl Pts',(41.25426751686,41.5844159622214,46.4464698053674));
#23105=CARTESIAN_POINT('Ctrl Pts',(41.3103348355896,41.5799709376688,46.4080915898299));
#23106=CARTESIAN_POINT('Ctrl Pts',(41.3664360672225,41.5755232244967,46.3696901608278));
#23107=CARTESIAN_POINT('Ctrl Pts',(41.4245161442928,41.5710755113246,46.3342945948905));
#23108=CARTESIAN_POINT('Ctrl Pts',(41.4842146373594,41.5666277981524,46.3020954895893));
#23109=CARTESIAN_POINT('Ctrl Pts',(41.5440166770513,41.5621723704524,46.2698405351615));
#23110=CARTESIAN_POINT('Ctrl Pts',(41.605442288967,41.5577169427524,46.2407933171338));
#23111=CARTESIAN_POINT('Ctrl Pts',(41.6681099803568,41.5532615150524,46.215096765635));
#23112=CARTESIAN_POINT('Ctrl Pts',(41.697030645708,41.5512053688844,46.2032380015718));
#23113=CARTESIAN_POINT('Ctrl Pts',(41.7262156185646,41.5491492227164,46.1920921510697));
#23114=CARTESIAN_POINT('Ctrl Pts',(41.7556264548729,41.5470930765484,46.1816696418856));
#23115=CARTESIAN_POINT('Ctrl Pts',(41.8193654558946,41.5426370079984,46.1590820378961));
#23116=CARTESIAN_POINT('Ctrl Pts',(41.8844210576915,41.5381809394484,46.139804735805));
#23117=CARTESIAN_POINT('Ctrl Pts',(41.9504163152003,41.5337248708983,46.1239890545997));
#23118=CARTESIAN_POINT('Ctrl Pts',(42.0163115421492,41.5292755565159,46.1081973455933));
#23119=CARTESIAN_POINT('Ctrl Pts',(42.0831431220984,41.5248262421335,46.0958569591184));
#23120=CARTESIAN_POINT('Ctrl Pts',(42.1505169711984,41.5203769277512,46.0870701070766));
#23121=CARTESIAN_POINT('Ctrl Pts',(42.2178111232798,41.5159328764953,46.0782936490663));
#23122=CARTESIAN_POINT('Ctrl Pts',(42.2856457833941,41.5114888252394,46.0730624413153));
#23123=CARTESIAN_POINT('Ctrl Pts',(42.3536164582438,41.5070447739835,46.0714276980227));
#23124=CARTESIAN_POINT('Ctrl Pts',(42.4215443130304,41.5026035223843,46.0697939845831));
#23125=CARTESIAN_POINT('Ctrl Pts',(42.4896075201079,41.4981622707851,46.0717522533283));
#23126=CARTESIAN_POINT('Ctrl Pts',(42.5573978303185,41.4937210191859,46.0773017709711));
#23127=CARTESIAN_POINT('Ctrl Pts',(42.6251688666464,41.4892810303064,46.0828497107962));
#23128=CARTESIAN_POINT('Ctrl Pts',(42.692666668266,41.484841041427,46.0919868324016));
#23129=CARTESIAN_POINT('Ctrl Pts',(42.7594862043598,41.4804010525475,46.1046603930232));
#23130=CARTESIAN_POINT('Ctrl Pts',(42.826309838871,41.4759607913386,46.1173347309854));
#23131=CARTESIAN_POINT('Ctrl Pts',(42.8924546406677,41.4715205301297,46.1335458440079));
#23132=CARTESIAN_POINT('Ctrl Pts',(42.9575257144821,41.4670802689208,46.1531898758694));
#23133=CARTESIAN_POINT('Ctrl Pts',(43.0226665940747,41.4626352443682,46.1728549811027));
#23134=CARTESIAN_POINT('Ctrl Pts',(43.0867309734581,41.4581902198155,46.1959602114558));
#23135=CARTESIAN_POINT('Ctrl Pts',(43.1493400721229,41.4537451952629,46.2223521121407));
#23136=CARTESIAN_POINT('Ctrl Pts',(43.2119870405549,41.4492974820908,46.2487599762423));
#23137=CARTESIAN_POINT('Ctrl Pts',(43.2731765323258,41.4448497689187,46.2784582512317));
#23138=CARTESIAN_POINT('Ctrl Pts',(43.3325532602683,41.4404020557466,46.3112469174971));
#23139=CARTESIAN_POINT('Ctrl Pts',(43.3920329767367,41.4359466280465,46.3440924554785));
#23140=CARTESIAN_POINT('Ctrl Pts',(43.4496932356182,41.4314912003465,46.3800388213601));
#23141=CARTESIAN_POINT('Ctrl Pts',(43.5052074443319,41.4270357726465,46.4188424930155));
#23142=CARTESIAN_POINT('Ctrl Pts',(43.5308268315607,41.4249796264785,46.4367500938456));
#23143=CARTESIAN_POINT('Ctrl Pts',(43.5559896265865,41.4229234803105,46.4552656648749));
#23144=CARTESIAN_POINT('Ctrl Pts',(43.5806662614674,41.4208673341425,46.4743625149032));
#23145=CARTESIAN_POINT('Ctrl Pts',(43.6341453274618,41.4164112655925,46.5157491021699));
#23146=CARTESIAN_POINT('Ctrl Pts',(43.6855526064654,41.4119551970425,46.5600338327948));
#23147=CARTESIAN_POINT('Ctrl Pts',(43.7345569108915,41.4074991284925,46.6069815476844));
#23148=CARTESIAN_POINT('Ctrl Pts',(43.7834869383439,41.4030498141101,46.6538581028213));
#23149=CARTESIAN_POINT('Ctrl Pts',(43.8300208656851,41.3986004997277,46.7033892932277));
#23150=CARTESIAN_POINT('Ctrl Pts',(43.8738595338283,41.3941511853453,46.7552989790944));
#23151=CARTESIAN_POINT('Ctrl Pts',(43.9176463448905,41.3897071340894,46.8071472606143));
#23152=CARTESIAN_POINT('Ctrl Pts',(43.9587439112277,41.3852630828335,46.8613680747775));
#23153=CARTESIAN_POINT('Ctrl Pts',(43.9968903328296,41.3808190315776,46.9176489378139));
#23154=CARTESIAN_POINT('Ctrl Pts',(44.0350127230065,41.3763777799784,46.9738943451172));
#23155=CARTESIAN_POINT('Ctrl Pts',(44.0701873797892,41.3719365283792,47.0321968192874));
#23156=CARTESIAN_POINT('Ctrl Pts',(44.102194060573,41.36749527678,47.0922126146227));
#23157=CARTESIAN_POINT('Ctrl Pts',(44.1341916413392,41.3630552879006,47.1522113464958));
#23158=CARTESIAN_POINT('Ctrl Pts',(44.1630228018407,41.3586152990211,47.2139219971069));
#23159=CARTESIAN_POINT('Ctrl Pts',(44.1885127819975,41.3541753101416,47.2769753907842));
#23160=CARTESIAN_POINT('Ctrl Pts',(44.2140043255979,41.3497350489327,47.3400326518802));
#23161=CARTESIAN_POINT('Ctrl Pts',(44.2361540993866,41.3452947877238,47.4044323608179));
#23162=CARTESIAN_POINT('Ctrl Pts',(44.2548358143818,41.3408545265149,47.4697862142619));
#23163=CARTESIAN_POINT('Ctrl Pts',(44.2735375704117,41.3364095019623,47.5352101768392));
#23164=CARTESIAN_POINT('Ctrl Pts',(44.2887637072124,41.3319644774097,47.601589850939));
#23165=CARTESIAN_POINT('Ctrl Pts',(44.3004383675356,41.3275194528571,47.6685236537871));
#23166=CARTESIAN_POINT('Ctrl Pts',(44.3121200893991,41.323071739685,47.735497942245));
#23167=CARTESIAN_POINT('Ctrl Pts',(44.3202460008862,41.3186240265128,47.8030265362109));
#23168=CARTESIAN_POINT('Ctrl Pts',(44.3247921167709,41.3141763133407,47.8707024202982));
#23169=CARTESIAN_POINT('Ctrl Pts',(44.3293461178622,41.3097208856407,47.9384956877405));
#23170=CARTESIAN_POINT('Ctrl Pts',(44.3303079245906,41.3052654579407,48.0064362617902));
#23171=CARTESIAN_POINT('Ctrl Pts',(44.3277056620925,41.3008100302407,48.0741177255224));
#23172=CARTESIAN_POINT('Ctrl Pts',(44.3265047376417,41.2987538840727,48.105352208869));
#23173=CARTESIAN_POINT('Ctrl Pts',(44.3245454806939,41.2966977379047,48.1365315920614));
#23174=CARTESIAN_POINT('Ctrl Pts',(44.3218343432927,41.2946415917367,48.1676165679185));
#23175=CARTESIAN_POINT('Ctrl Pts',(44.3159587813817,41.2901855231867,48.2349837548678));
#23176=CARTESIAN_POINT('Ctrl Pts',(44.3065249804363,41.2857294546367,48.3021763817014));
#23177=CARTESIAN_POINT('Ctrl Pts',(44.2935515461884,41.2812733860866,48.3687886912954));
#23178=CARTESIAN_POINT('Ctrl Pts',(44.2805977760792,41.2768240717042,48.4353000350494));
#23179=CARTESIAN_POINT('Ctrl Pts',(44.2641151134346,41.2723747573218,48.5012323264475));
#23180=CARTESIAN_POINT('Ctrl Pts',(44.2441739570645,41.2679254429394,48.566184575015));
#23181=CARTESIAN_POINT('Ctrl Pts',(44.2242563892341,41.2634813916835,48.631059991093));
#23182=CARTESIAN_POINT('Ctrl Pts',(44.2008885963532,41.2590373404276,48.6949571968475));
#23183=CARTESIAN_POINT('Ctrl Pts',(44.1741917003665,41.2545932891718,48.7574868759593));
#23184=CARTESIAN_POINT('Ctrl Pts',(44.14751162285,41.2501520375726,48.8199771627184));
#23185=CARTESIAN_POINT('Ctrl Pts',(44.1175067956851,41.2457107859734,48.8811011786283));
#23186=CARTESIAN_POINT('Ctrl Pts',(44.0843471692799,41.2412695343742,48.9404877299778));
#23187=CARTESIAN_POINT('Ctrl Pts',(44.0511969706933,41.2368295454947,48.9998573967694));
#23188=CARTESIAN_POINT('Ctrl Pts',(44.014893993986,41.2323895566152,49.0574901487156));
#23189=CARTESIAN_POINT('Ctrl Pts',(43.9756541825435,41.2279495677358,49.1130392867879));
#23190=CARTESIAN_POINT('Ctrl Pts',(43.9364119643029,41.2235093065269,49.1685918320008));
#23191=CARTESIAN_POINT('Ctrl Pts',(43.8942328407227,41.2190690453179,49.2220601078674));
#23192=CARTESIAN_POINT('Ctrl Pts',(43.8493750645417,41.214628784109,49.27312783301));
#23193=CARTESIAN_POINT('Ctrl Pts',(43.8044691666411,41.2101837595564,49.3242503416698));
#23194=CARTESIAN_POINT('Ctrl Pts',(43.7568792081038,41.2057387350038,49.3729667888091));
#23195=CARTESIAN_POINT('Ctrl Pts',(43.7069018931882,41.2012937104512,49.4189961234905));
#23196=CARTESIAN_POINT('Ctrl Pts',(43.6568943489718,41.1968459972791,49.4650532994956));
#23197=CARTESIAN_POINT('Ctrl Pts',(43.6044969551146,41.192398284107,49.5084198137376));
#23198=CARTESIAN_POINT('Ctrl Pts',(43.5500390471774,41.1879505709348,49.5488553021077));
#23199=CARTESIAN_POINT('Ctrl Pts',(43.4954866823738,41.1834951432348,49.5893609255541));
#23200=CARTESIAN_POINT('Ctrl Pts',(43.438867082001,41.1790397155348,49.6269251043419));
#23201=CARTESIAN_POINT('Ctrl Pts',(43.3805372695588,41.1745842878348,49.6613516244029));
#23202=CARTESIAN_POINT('Ctrl Pts',(43.3536185025159,41.1725281416668,49.6772392028953));
#23203=CARTESIAN_POINT('Ctrl Pts',(43.3263358248222,41.1704719954988,49.6924591937595));
#23204=CARTESIAN_POINT('Ctrl Pts',(43.2987257854211,41.1684158493308,49.7069957584948));
#23205=CARTESIAN_POINT('Ctrl Pts',(43.2389078604469,41.1639611509718,49.7384896338235));
#23206=CARTESIAN_POINT('Ctrl Pts',(43.1773128632059,41.1595064526128,49.7668983951178));
#23207=CARTESIAN_POINT('Ctrl Pts',(43.1142917840521,41.1550517542537,49.7920183604349));
#23208=CARTESIAN_POINT('Ctrl Pts',(43.0513574843709,41.1506031899752,49.8171037357803));
#23209=CARTESIAN_POINT('Ctrl Pts',(42.9870014511529,41.1461546256967,49.8389091144193));
#23210=CARTESIAN_POINT('Ctrl Pts',(42.9215988152741,41.1417060614182,49.8572768325709));
#23211=CARTESIAN_POINT('Ctrl Pts',(42.8562636241999,41.1372620846084,49.8756256094804));
#23212=CARTESIAN_POINT('Ctrl Pts',(42.7898844443704,41.1328181077987,49.8905436256558));
#23213=CARTESIAN_POINT('Ctrl Pts',(42.7228542004076,41.1283741309889,49.9019221125428));
#23214=CARTESIAN_POINT('Ctrl Pts',(42.6558699067754,41.1239332005981,49.9132927992906));
#23215=CARTESIAN_POINT('Ctrl Pts',(42.5882359204943,41.1194922702072,49.921128690664));
#23216=CARTESIAN_POINT('Ctrl Pts',(42.5203562755619,41.1150513398164,49.9253718923452));
#23217=CARTESIAN_POINT('Ctrl Pts',(42.4524776557753,41.1106104764943,49.9296150299438));
#23218=CARTESIAN_POINT('Ctrl Pts',(42.3843538763555,41.1061696131721,49.9302655382472));
#23219=CARTESIAN_POINT('Ctrl Pts',(42.3163935852902,41.10172874985,49.9273174425401));
#23220=CARTESIAN_POINT('Ctrl Pts',(42.248435826869,41.0972880520235,49.9243694566983));
#23221=CARTESIAN_POINT('Ctrl Pts',(42.1806420378965,41.0928473541969,49.9178231631969));
#23222=CARTESIAN_POINT('Ctrl Pts',(42.1134180541516,41.0884066563703,49.9077246513095));
#23223=CARTESIAN_POINT('Ctrl Pts',(42.0461359862326,41.0839621216057,49.8976174139093));
#23224=CARTESIAN_POINT('Ctrl Pts',(41.9794251940253,41.079517586841,49.8839519130002));
#23225=CARTESIAN_POINT('Ctrl Pts',(41.9136824370759,41.0750730520763,49.8668255903784));
#23226=CARTESIAN_POINT('Ctrl Pts',(41.8734428217844,41.072352655528,49.8563429658941));
#23227=CARTESIAN_POINT('Ctrl Pts',(41.8335656395969,41.0696322589797,49.844564784894));
#23228=CARTESIAN_POINT('Ctrl Pts',(41.7941388317924,41.0669118624314,49.8315225365138));
#23229=CARTESIAN_POINT('Origin',(42.4,48.4493818343519,48.));
#23230=CARTESIAN_POINT('',(41.7941388318207,40.1003056653051,49.8315225365232));
#23231=CARTESIAN_POINT('',(41.7933319732428,40.273017144546,49.8339081536803));
#23232=CARTESIAN_POINT('',(41.7941388317924,48.4493818343519,49.8315225365138));
#23233=CARTESIAN_POINT('Ctrl Pts',(41.7941388318207,40.1003056653051,49.8315225365232));
#23234=CARTESIAN_POINT('Ctrl Pts',(41.9417997033319,40.110751722448,49.8803682298326));
#23235=CARTESIAN_POINT('Ctrl Pts',(42.094800152278,40.1218028811348,49.9111691005024));
#23236=CARTESIAN_POINT('Ctrl Pts',(42.3518158958192,40.1402150999778,49.9312408979334));
#23237=CARTESIAN_POINT('Ctrl Pts',(42.454315125457,40.1474984258421,49.9310794105004));
#23238=CARTESIAN_POINT('Ctrl Pts',(42.5689914074891,40.1552819395496,49.9217559422526));
#23239=CARTESIAN_POINT('Ctrl Pts',(42.581645482915,40.1561356585347,49.920601191584));
#23240=CARTESIAN_POINT('Ctrl Pts',(42.6005145546417,40.1574000601793,49.9186911273435));
#23241=CARTESIAN_POINT('Ctrl Pts',(42.60673848085,40.1578157182278,49.9180304825638));
#23242=CARTESIAN_POINT('Ctrl Pts',(42.6174262346275,40.1585269504496,49.9168433921574));
#23243=CARTESIAN_POINT('Ctrl Pts',(42.6218915433195,40.1588233331116,49.9163316263134));
#23244=CARTESIAN_POINT('Ctrl Pts',(42.6320931728744,40.1594986906424,49.9151262883405));
#23245=CARTESIAN_POINT('Ctrl Pts',(42.6378281930103,40.1598770891584,49.9144225484361));
#23246=CARTESIAN_POINT('Ctrl Pts',(42.6535927438972,40.1609139722711,49.9124161582588));
#23247=CARTESIAN_POINT('Ctrl Pts',(42.6636154988476,40.1615695584285,49.9110603657899));
#23248=CARTESIAN_POINT('Ctrl Pts',(42.7165797682563,40.1650168705974,49.9034711956959));
#23249=CARTESIAN_POINT('Ctrl Pts',(42.7593160644031,40.1677390954992,49.8958686556973));
#23250=CARTESIAN_POINT('Ctrl Pts',(42.8190628227866,40.1715067945335,49.8831467703358));
#23251=CARTESIAN_POINT('Ctrl Pts',(42.8363115276671,40.1725899837901,49.8792252894721));
#23252=CARTESIAN_POINT('Ctrl Pts',(42.8655653586619,40.1744229785679,49.8721499494924));
#23253=CARTESIAN_POINT('Ctrl Pts',(42.8775981932023,40.175175745795,49.8691165053104));
#23254=CARTESIAN_POINT('Ctrl Pts',(43.0003577371279,40.1828506939619,49.8369062892878));
#23255=CARTESIAN_POINT('Ctrl Pts',(43.108307736997,40.1895737292688,49.7980420934161));
#23256=CARTESIAN_POINT('Ctrl Pts',(43.2889365399485,40.2016087955895,49.7142041968312));
#23257=CARTESIAN_POINT('Ctrl Pts',(43.3632612226724,40.20681475279,49.673567853177));
#23258=CARTESIAN_POINT('Ctrl Pts',(43.4495224805585,40.2133181221175,49.6187509635083));
#23259=CARTESIAN_POINT('Ctrl Pts',(43.4642419484988,40.2144447903505,49.6091119169191));
#23260=CARTESIAN_POINT('Ctrl Pts',(43.4872367266874,40.2162329062418,49.5936002509831));
#23261=CARTESIAN_POINT('Ctrl Pts',(43.4956013061423,40.2168893142542,49.5878612128394));
#23262=CARTESIAN_POINT('Ctrl Pts',(43.5111936786003,40.2181243650534,49.5769812393727));
#23263=CARTESIAN_POINT('Ctrl Pts',(43.5184320621103,40.2187024006963,49.5718558899296));
#23264=CARTESIAN_POINT('Ctrl Pts',(43.5345790544161,40.2200025665416,49.5602545384407));
#23265=CARTESIAN_POINT('Ctrl Pts',(43.5434680056432,40.2207257183945,49.5537518357014));
#23266=CARTESIAN_POINT('Ctrl Pts',(43.5659821423875,40.2225765959712,49.536983804038));
#23267=CARTESIAN_POINT('Ctrl Pts',(43.579527499039,40.2237084070158,49.5266133817451));
#23268=CARTESIAN_POINT('Ctrl Pts',(43.6798932593009,40.2322347925752,49.4476394271683));
#23269=CARTESIAN_POINT('Ctrl Pts',(43.7607898711524,40.2399209921067,49.3718709906854));
#23270=CARTESIAN_POINT('Ctrl Pts',(43.9307729139648,40.257960721092,49.1827574868696));
#23271=CARTESIAN_POINT('Ctrl Pts',(44.0145749331128,40.2683830478816,49.0655193927069));
#23272=CARTESIAN_POINT('Ctrl Pts',(44.0948608350144,40.2796624190017,48.9216474148817));
#23273=CARTESIAN_POINT('Ctrl Pts',(44.1048342876457,40.2810918586419,48.9030655287994));
#23274=CARTESIAN_POINT('Ctrl Pts',(44.1180108119841,40.2830163594297,48.8775192374203));
#23275=CARTESIAN_POINT('Ctrl Pts',(44.1214796324773,40.2835265866745,48.8706945744657));
#23276=CARTESIAN_POINT('Ctrl Pts',(44.1272277269227,40.2843779323347,48.8592169556688));
#23277=CARTESIAN_POINT('Ctrl Pts',(44.129529021435,40.2847203946612,48.8545751948618));
#23278=CARTESIAN_POINT('Ctrl Pts',(44.1338721102007,40.2853697304738,48.8457256853358));
#23279=CARTESIAN_POINT('Ctrl Pts',(44.1359173394209,40.2856768243729,48.8415197093557));
#23280=CARTESIAN_POINT('Ctrl Pts',(44.1407498964978,40.2864056833402,48.8314890555598));
#23281=CARTESIAN_POINT('Ctrl Pts',(44.1435233374075,40.2868265980652,48.8256576933044));
#23282=CARTESIAN_POINT('Ctrl Pts',(44.1532687309632,40.2883154000398,48.8048992079333));
#23283=CARTESIAN_POINT('Ctrl Pts',(44.160078922686,40.2893739097298,48.7898963270121));
#23284=CARTESIAN_POINT('Ctrl Pts',(44.2078613594484,40.2969483306882,48.6809440230193));
#23285=CARTESIAN_POINT('Ctrl Pts',(44.2414861357994,40.3030975850257,48.5839364046351));
#23286=CARTESIAN_POINT('Ctrl Pts',(44.2943161442119,40.3156524624026,48.3804177004246));
#23287=CARTESIAN_POINT('Ctrl Pts',(44.3126016608496,40.322038007028,48.2740520015252));
#23288=CARTESIAN_POINT('Ctrl Pts',(44.326735158817,40.332086908909,48.111123124695));
#23289=CARTESIAN_POINT('Ctrl Pts',(44.3291429028897,40.3355712281245,48.0553487415454));
#23290=CARTESIAN_POINT('Ctrl Pts',(44.3291263159966,40.3401293230084,47.9839090586368));
#23291=CARTESIAN_POINT('Ctrl Pts',(44.3289324137831,40.3411330932029,47.968267033101));
#23292=CARTESIAN_POINT('Ctrl Pts',(44.3283096522953,40.3427701760943,47.9429131821155));
#23293=CARTESIAN_POINT('Ctrl Pts',(44.3279975726937,40.3433998170171,47.9331989982244));
#23294=CARTESIAN_POINT('Ctrl Pts',(44.3272569746067,40.3446139818703,47.9145407372712));
#23295=CARTESIAN_POINT('Ctrl Pts',(44.3268395619174,40.3451981414213,47.9055964523037));
#23296=CARTESIAN_POINT('Ctrl Pts',(44.3257402812549,40.3465414232836,47.8851056602076));
#23297=CARTESIAN_POINT('Ctrl Pts',(44.3250168097472,40.3473018336337,47.8735618237272));
#23298=CARTESIAN_POINT('Ctrl Pts',(44.3223793737449,40.3497367056006,47.83678022075));
#23299=CARTESIAN_POINT('Ctrl Pts',(44.3200725934344,40.3514233884554,47.8115741924639));
#23300=CARTESIAN_POINT('Ctrl Pts',(44.3023435777907,40.3621926561487,47.6524225257492));
#23301=CARTESIAN_POINT('Ctrl Pts',(44.2734124885541,40.3717035878287,47.5203809366346));
#23302=CARTESIAN_POINT('Ctrl Pts',(44.2075958273054,40.3866276316793,47.3220277889969));
#23303=CARTESIAN_POINT('Ctrl Pts',(44.1801813062461,40.3919405292553,47.2530031806838));
#23304=CARTESIAN_POINT('Ctrl Pts',(44.134411331972,40.3995581310088,47.1547004869882));
#23305=CARTESIAN_POINT('Ctrl Pts',(44.1191409972667,40.4019395121946,47.124061391812));
#23306=CARTESIAN_POINT('Ctrl Pts',(44.0928774960435,40.4057700870818,47.074700856978));
#23307=CARTESIAN_POINT('Ctrl Pts',(44.0823698162676,40.4072407541839,47.0557306424382));
#23308=CARTESIAN_POINT('Ctrl Pts',(44.0676812519924,40.4092111259118,47.0302362822469));
#23309=CARTESIAN_POINT('Ctrl Pts',(44.0637781350985,40.409726918484,47.0235550457194));
#23310=CARTESIAN_POINT('Ctrl Pts',(44.0571860286228,40.4105849458717,47.0124251725123));
#23311=CARTESIAN_POINT('Ctrl Pts',(44.0545191026196,40.410928569234,47.007963652678));
#23312=CARTESIAN_POINT('Ctrl Pts',(44.0494259954213,40.4115781162381,46.9995210264337));
#23313=CARTESIAN_POINT('Ctrl Pts',(44.0470033694404,40.4118842735511,46.9955378587875));
#23314=CARTESIAN_POINT('Ctrl Pts',(44.0412214686857,40.4126084237112,46.9861086892509));
#23315=CARTESIAN_POINT('Ctrl Pts',(44.0378494652773,40.4130255919084,46.9806704991874));
#23316=CARTESIAN_POINT('Ctrl Pts',(44.0258847013086,40.4144881840771,46.9615870192747));
#23317=CARTESIAN_POINT('Ctrl Pts',(44.0171476943862,40.4155246545485,46.9480323407776));
#23318=CARTESIAN_POINT('Ctrl Pts',(43.9442392261779,40.4239343505241,46.8379768422594));
#23319=CARTESIAN_POINT('Ctrl Pts',(43.8716523813066,40.4308341587448,46.7473151739668));
#23320=CARTESIAN_POINT('Ctrl Pts',(43.6932765016396,40.4461933452028,46.5615888541548));
#23321=CARTESIAN_POINT('Ctrl Pts',(43.5842669151826,40.4546360512688,46.470589617404));
#23322=CARTESIAN_POINT('Ctrl Pts',(43.4489899111222,40.4649240456652,46.3808663920005));
#23323=CARTESIAN_POINT('Ctrl Pts',(43.4315070608787,40.4662494439422,46.3696728536568));
#23324=CARTESIAN_POINT('Ctrl Pts',(43.4046499532447,40.4682810015496,46.3530823018262));
#23325=CARTESIAN_POINT('Ctrl Pts',(43.3954049545883,40.4689795210464,46.3474781690943));
#23326=CARTESIAN_POINT('Ctrl Pts',(43.3785013684331,40.4702554961488,46.3374248680319));
#23327=CARTESIAN_POINT('Ctrl Pts',(43.3708582654323,40.4708319983841,46.3329501442662));
#23328=CARTESIAN_POINT('Ctrl Pts',(43.3542617006342,40.4720830327096,46.3233863823124));
#23329=CARTESIAN_POINT('Ctrl Pts',(43.3452977942177,40.4727582214937,46.3183161148528));
#23330=CARTESIAN_POINT('Ctrl Pts',(43.3207089595532,40.4746092016209,46.3046666098901));
#23331=CARTESIAN_POINT('Ctrl Pts',(43.3050053596735,40.4757901042452,46.2962319540647));
#23332=CARTESIAN_POINT('Ctrl Pts',(43.2172125876069,40.4823872207518,46.2506332463756));
#23333=CARTESIAN_POINT('Ctrl Pts',(43.1429616252921,40.4879538976458,46.2178312858369));
#23334=CARTESIAN_POINT('Ctrl Pts',(42.947601533405,40.5025486194758,46.1458607881171));
#23335=CARTESIAN_POINT('Ctrl Pts',(42.8242785740639,40.5117296819375,46.1138176641386));
#23336=CARTESIAN_POINT('Ctrl Pts',(42.6367763687192,40.5251454393547,46.0844295552565));
#23337=CARTESIAN_POINT('Ctrl Pts',(42.574394352051,40.5295162481237,46.0777457252237));
#23338=CARTESIAN_POINT('Ctrl Pts',(42.5010349178353,40.5344701898344,46.073487452713));
#23339=CARTESIAN_POINT('Ctrl Pts',(42.4902730477458,40.5351922360268,46.0729531818098));
#23340=CARTESIAN_POINT('Ctrl Pts',(42.4736511330289,40.5362996219209,46.0722675453735));
#23341=CARTESIAN_POINT('Ctrl Pts',(42.4677941333653,40.5366883276011,46.0720526812786));
#23342=CARTESIAN_POINT('Ctrl Pts',(42.4569543397704,40.5374048344325,46.071704482161));
#23343=CARTESIAN_POINT('Ctrl Pts',(42.4519720205151,40.537733023192,46.0715637653955));
#23344=CARTESIAN_POINT('Ctrl Pts',(42.440578507512,40.5384809611306,46.0712861640979));
#23345=CARTESIAN_POINT('Ctrl Pts',(42.434167134293,40.5389000018557,46.0711619337227));
#23346=CARTESIAN_POINT('Ctrl Pts',(42.4173225860087,40.539996391233,46.0709195595341));
#23347=CARTESIAN_POINT('Ctrl Pts',(42.4068886996906,40.5406709316627,46.0708540814113));
#23348=CARTESIAN_POINT('Ctrl Pts',(42.3202927448594,40.5462350177639,46.0710132333689));
#23349=CARTESIAN_POINT('Ctrl Pts',(42.2441962217715,40.5509056905943,46.0756634267802));
#23350=CARTESIAN_POINT('Ctrl Pts',(42.0778108905353,40.5610163586496,46.0957695946922));
#23351=CARTESIAN_POINT('Ctrl Pts',(41.9879493351605,40.5664135498373,46.1131735276365));
#23352=CARTESIAN_POINT('Ctrl Pts',(41.8102644416101,40.5774586906191,46.1608908987508));
#23353=CARTESIAN_POINT('Ctrl Pts',(41.7227235722522,40.5830956859637,46.1912977144555));
#23354=CARTESIAN_POINT('Ctrl Pts',(41.6159302159832,40.5904388173201,46.237235347621));
#23355=CARTESIAN_POINT('Ctrl Pts',(41.5943266028937,40.5919488731925,46.2470040090321));
#23356=CARTESIAN_POINT('Ctrl Pts',(41.5626162810388,40.5942047603212,46.2620526851427));
#23357=CARTESIAN_POINT('Ctrl Pts',(41.552366991471,40.5949400908624,46.2670283800173));
#23358=CARTESIAN_POINT('Ctrl Pts',(41.5341856274308,40.5962558744529,46.2760547154927));
#23359=CARTESIAN_POINT('Ctrl Pts',(41.5262363335693,40.5968350803296,46.2800700821029));
#23360=CARTESIAN_POINT('Ctrl Pts',(41.5095051351027,40.5980626020129,46.2886673133666));
#23361=CARTESIAN_POINT('Ctrl Pts',(41.5007301711631,40.5987113598786,46.2932620478017));
#23362=CARTESIAN_POINT('Ctrl Pts',(41.4774373787271,40.6004469554241,46.305688087215));
#23363=CARTESIAN_POINT('Ctrl Pts',(41.4629842193625,40.6015379954668,46.3136382221086));
#23364=CARTESIAN_POINT('Ctrl Pts',(41.3982778658854,40.6064878547876,46.3503193932303));
#23365=CARTESIAN_POINT('Ctrl Pts',(41.3492359528753,40.6104203718835,46.3811154877808));
#23366=CARTESIAN_POINT('Ctrl Pts',(41.1930143323616,40.6235615783891,46.4893073054275));
#23367=CARTESIAN_POINT('Ctrl Pts',(41.0924001713771,40.6330590924896,46.575506361972));
#23368=CARTESIAN_POINT('Ctrl Pts',(40.9623256012841,40.6465029188335,46.712423562647));
#23369=CARTESIAN_POINT('Ctrl Pts',(40.925083313537,40.6505128018396,46.7552581015143));
#23370=CARTESIAN_POINT('Ctrl Pts',(40.8707076216271,40.65655740037,46.823672212863));
#23371=CARTESIAN_POINT('Ctrl Pts',(40.8522075615836,40.6586517173107,46.8481228075257));
#23372=CARTESIAN_POINT('Ctrl Pts',(40.8291703805095,40.6612991634921,46.8801277436908));
#23373=CARTESIAN_POINT('Ctrl Pts',(40.8240923622885,40.661885327244,46.8872849921935));
#23374=CARTESIAN_POINT('Ctrl Pts',(40.8159552978936,40.6628285141119,46.8989212783622));
#23375=CARTESIAN_POINT('Ctrl Pts',(40.8128660616002,40.6631875274136,46.9033789018485));
#23376=CARTESIAN_POINT('Ctrl Pts',(40.8069364447978,40.6638783520808,46.9120126049537));
#23377=CARTESIAN_POINT('Ctrl Pts',(40.8040936222508,40.6642103196321,46.9161868718386));
#23378=CARTESIAN_POINT('Ctrl Pts',(40.7978470774428,40.6649415632018,46.9254368716389));
#23379=CARTESIAN_POINT('Ctrl Pts',(40.7944509842546,40.6653403307043,46.9305177586199));
#23380=CARTESIAN_POINT('Ctrl Pts',(40.7825172907873,40.6667462130417,46.9485566878378));
#23381=CARTESIAN_POINT('Ctrl Pts',(40.7741116813166,40.6677449623632,46.9616019234378));
#23382=CARTESIAN_POINT('Ctrl Pts',(40.6950451642346,40.6772371371896,47.0876249820522));
#23383=CARTESIAN_POINT('Ctrl Pts',(40.6361014036552,40.6850947264693,47.2075535069091));
#23384=CARTESIAN_POINT('Ctrl Pts',(40.5832793780464,40.6942070585453,47.3508121732161));
#23385=CARTESIAN_POINT('Ctrl Pts',(40.5768450938865,40.6953655303543,47.3691079078347));
#23386=CARTESIAN_POINT('Ctrl Pts',(40.5412818275329,40.7020732158501,47.4753218570515));
#23387=CARTESIAN_POINT('Ctrl Pts',(40.5182414996086,40.7076836396037,47.5651406787126));
#23388=CARTESIAN_POINT('Ctrl Pts',(40.4964455500316,40.7153620873896,47.6855061952501));
#23389=CARTESIAN_POINT('Ctrl Pts',(40.491826549795,40.7172467537808,47.7148687503005));
#23390=CARTESIAN_POINT('Ctrl Pts',(40.4862369811517,40.7199516243615,47.7566713726347));
#23391=CARTESIAN_POINT('Ctrl Pts',(40.4847057662242,40.7207541680439,47.7690331207121));
#23392=CARTESIAN_POINT('Ctrl Pts',(40.4822672299272,40.7221473156802,47.790415279881));
#23393=CARTESIAN_POINT('Ctrl Pts',(40.4813035713438,40.722736124833,47.7994289595217));
#23394=CARTESIAN_POINT('Ctrl Pts',(40.479464053374,40.7239436000353,47.8178633801338));
#23395=CARTESIAN_POINT('Ctrl Pts',(40.4785939011038,40.7245624290778,47.8272844294978));
#23396=CARTESIAN_POINT('Ctrl Pts',(40.476570168006,40.7261318402742,47.851107481023));
#23397=CARTESIAN_POINT('Ctrl Pts',(40.4755090332667,40.7270853008353,47.8655165423795));
#23398=CARTESIAN_POINT('Ctrl Pts',(40.4720939067683,40.7307260192037,47.9202826825161));
#23399=CARTESIAN_POINT('Ctrl Pts',(40.4708469418687,40.7334474714769,47.9606958459015));
#23400=CARTESIAN_POINT('Ctrl Pts',(40.4709085825278,40.740719875977,48.0672588147051));
#23401=CARTESIAN_POINT('Ctrl Pts',(40.4743484768184,40.7453296025145,48.1333497355389));
#23402=CARTESIAN_POINT('Ctrl Pts',(40.4957775446428,40.7599959601246,48.339843184221));
#23403=CARTESIAN_POINT('Ctrl Pts',(40.5258137430645,40.7702637749302,48.4785207838106));
#23404=CARTESIAN_POINT('Ctrl Pts',(40.5810551611003,40.7823215734393,48.6434567674931));
#23405=CARTESIAN_POINT('Ctrl Pts',(40.5921441131223,40.784544458076,48.6739839246788));
#23406=CARTESIAN_POINT('Ctrl Pts',(40.6073981370496,40.7873532077696,48.712886954693));
#23407=CARTESIAN_POINT('Ctrl Pts',(40.6108598177641,40.7879757256517,48.721530779779));
#23408=CARTESIAN_POINT('Ctrl Pts',(40.6164815524939,40.7889629834857,48.7352790059569));
#23409=CARTESIAN_POINT('Ctrl Pts',(40.6186012010772,40.7893300536813,48.7403996152913));
#23410=CARTESIAN_POINT('Ctrl Pts',(40.6226965602814,40.7900293842234,48.7501737110327));
#23411=CARTESIAN_POINT('Ctrl Pts',(40.6246685178124,40.7903618506289,48.7548286179249));
#23412=CARTESIAN_POINT('Ctrl Pts',(40.6294063280299,40.7911506642196,48.7658911882673));
#23413=CARTESIAN_POINT('Ctrl Pts',(40.6321887279894,40.7916060146594,48.7722917672449));
#23414=CARTESIAN_POINT('Ctrl Pts',(40.641729145953,40.7931413835098,48.7939166218842));
#23415=CARTESIAN_POINT('Ctrl Pts',(40.6486498011372,40.7942120281791,48.8090689246679));
#23416=CARTESIAN_POINT('Ctrl Pts',(40.6659910317275,40.7967972211464,48.8457708417275));
#23417=CARTESIAN_POINT('Ctrl Pts',(40.6766182819495,40.7983011482689,48.8672202611373));
#23418=CARTESIAN_POINT('Ctrl Pts',(40.7211294447461,40.8043100800076,48.9530073491391));
#23419=CARTESIAN_POINT('Ctrl Pts',(40.7582411803242,40.808682413978,49.0156076718594));
#23420=CARTESIAN_POINT('Ctrl Pts',(40.8855125480237,40.8223216435242,49.2050063163955));
#23421=CARTESIAN_POINT('Ctrl Pts',(40.9874925675597,40.8314953805544,49.3230758438179));
#23422=CARTESIAN_POINT('Ctrl Pts',(41.120282241947,40.8428259013328,49.4437591321584));
#23423=CARTESIAN_POINT('Ctrl Pts',(41.1383327932775,40.8443534167587,49.4595594369491));
#23424=CARTESIAN_POINT('Ctrl Pts',(41.1654244714394,40.8466304097556,49.4823956413424));
#23425=CARTESIAN_POINT('Ctrl Pts',(41.1742416201356,40.8473690935423,49.4896945855008));
#23426=CARTESIAN_POINT('Ctrl Pts',(41.1900384229289,40.8486886201596,49.5025361774477));
#23427=CARTESIAN_POINT('Ctrl Pts',(41.1969925729493,40.8492681890081,49.5081097799927));
#23428=CARTESIAN_POINT('Ctrl Pts',(41.2117339572474,40.8504941341118,49.5197578442459));
#23429=CARTESIAN_POINT('Ctrl Pts',(41.2195296974178,40.8511409357268,49.5258210747216));
#23430=CARTESIAN_POINT('Ctrl Pts',(41.2403637024477,40.8528657030654,49.5417697386173));
#23431=CARTESIAN_POINT('Ctrl Pts',(41.2534815264133,40.8539477792481,49.5515494291376));
#23432=CARTESIAN_POINT('Ctrl Pts',(41.3189507157316,40.8593305459919,49.5990748360092));
#23433=CARTESIAN_POINT('Ctrl Pts',(41.3730435103735,40.8637247399463,49.6343398102676));
#23434=CARTESIAN_POINT('Ctrl Pts',(41.4940758530742,40.8734467339797,49.7048613272617));
#23435=CARTESIAN_POINT('Ctrl Pts',(41.5615282696256,40.8787984580475,49.7390267930907));
#23436=CARTESIAN_POINT('Ctrl Pts',(41.6843087315625,40.8883492346791,49.792409657613));
#23437=CARTESIAN_POINT('Ctrl Pts',(41.738810557847,40.8925251977351,49.8132201490352));
#23438=CARTESIAN_POINT('Ctrl Pts',(41.7941391176755,40.8966643233312,49.831522631083));
#23439=CARTESIAN_POINT('',(40.4706609686455,40.9087567724484,48.0006653527742));
#23440=CARTESIAN_POINT('Ctrl Pts',(41.7941388317924,41.0669118624314,49.8315225365138));
#23441=CARTESIAN_POINT('Ctrl Pts',(41.7295757742925,41.0624570985652,49.8101653057618));
#23442=CARTESIAN_POINT('Ctrl Pts',(41.6662218155483,41.0580023346989,49.7854160650458));
#23443=CARTESIAN_POINT('Ctrl Pts',(41.604445100534,41.0535475708326,49.7574512678409));
#23444=CARTESIAN_POINT('Ctrl Pts',(41.5519449881319,41.0497617495301,49.7336857601377));
#23445=CARTESIAN_POINT('Ctrl Pts',(41.5005837656602,41.0459759282275,49.7075988058735));
#23446=CARTESIAN_POINT('Ctrl Pts',(41.4505716588481,41.042190106925,49.6793237870993));
#23447=CARTESIAN_POINT('Ctrl Pts',(41.3917053367279,41.037734038375,49.6460429183415));
#23448=CARTESIAN_POINT('Ctrl Pts',(41.3344733071312,41.033277969825,49.6095965126297));
#23449=CARTESIAN_POINT('Ctrl Pts',(41.279237085149,41.0288219012749,49.5701697505667));
#23450=CARTESIAN_POINT('Ctrl Pts',(41.2240845860042,41.0243725868925,49.5308027485718));
#23451=CARTESIAN_POINT('Ctrl Pts',(41.1709222897294,41.0199232725101,49.4884646395959));
#23452=CARTESIAN_POINT('Ctrl Pts',(41.1200858975378,41.0154739581277,49.4433857582845));
#23453=CARTESIAN_POINT('Ctrl Pts',(41.0693096400861,41.0110299068719,49.3983602011112));
#23454=CARTESIAN_POINT('Ctrl Pts',(41.0208541905169,41.006585855616,49.3506006360544));
#23455=CARTESIAN_POINT('Ctrl Pts',(40.9750235941449,41.0021418043601,49.3003787139353));
#23456=CARTESIAN_POINT('Ctrl Pts',(40.9292218700627,40.9977005527609,49.250188430547));
#23457=CARTESIAN_POINT('Ctrl Pts',(40.8860420512438,40.9932593011617,49.1975392309242));
#23458=CARTESIAN_POINT('Ctrl Pts',(40.8457514447914,40.9888180495625,49.1427396840628));
#23459=CARTESIAN_POINT('Ctrl Pts',(40.8054722936107,40.984378060683,49.0879557175998));
#23460=CARTESIAN_POINT('Ctrl Pts',(40.7680810164976,40.9799380718036,49.0310230151296));
#23461=CARTESIAN_POINT('Ctrl Pts',(40.7338035596483,40.9754980829241,48.9722818413708));
#23462=CARTESIAN_POINT('Ctrl Pts',(40.6995240003702,40.9710578217152,48.9135370646859));
#23463=CARTESIAN_POINT('Ctrl Pts',(40.6683588870979,40.9666175605063,48.8529840242597));
#23464=CARTESIAN_POINT('Ctrl Pts',(40.6404889427882,40.9621772992974,48.7909888725194));
#23465=CARTESIAN_POINT('Ctrl Pts',(40.6125891006601,40.9577322747448,48.7289272147334));
#23466=CARTESIAN_POINT('Ctrl Pts',(40.5879916846751,40.9532872501922,48.6654208095263));
#23467=CARTESIAN_POINT('Ctrl Pts',(40.5668294146933,40.9488422256396,48.6008561908363));
#23468=CARTESIAN_POINT('Ctrl Pts',(40.5456543444915,40.9443945124674,48.5362525195623));
#23469=CARTESIAN_POINT('Ctrl Pts',(40.5279186839299,40.9399467992953,48.4705898377334));
#23470=CARTESIAN_POINT('Ctrl Pts',(40.5137045979685,40.9354990861232,48.4042675020018));
#23471=CARTESIAN_POINT('Ctrl Pts',(40.4994658577728,40.9310436584232,48.3378301306353));
#23472=CARTESIAN_POINT('Ctrl Pts',(40.488760960153,40.9265882307232,48.2707313091753));
#23473=CARTESIAN_POINT('Ctrl Pts',(40.4816204135195,40.9221328030231,48.2033772825931));
#23474=CARTESIAN_POINT('Ctrl Pts',(40.4783251052828,40.9200766568551,48.1722939090133));
#23475=CARTESIAN_POINT('Ctrl Pts',(40.4757881850223,40.9180205106871,48.1411562042223));
#23476=CARTESIAN_POINT('Ctrl Pts',(40.4740089101723,40.9159643645191,48.1100039944922));
#23477=CARTESIAN_POINT('Ctrl Pts',(40.4719299112248,40.9135618544634,48.0736041031328));
#23478=CARTESIAN_POINT('Ctrl Pts',(40.4708827128295,40.9111593444076,48.0371447193032));
#23479=CARTESIAN_POINT('Ctrl Pts',(40.4708701150393,40.9087568343519,48.0006662218881));
#23480=CARTESIAN_POINT('Ctrl Pts',(40.4679315868973,40.9087559646023,48.0006540107483));
#23481=CARTESIAN_POINT('Ctrl Pts',(40.4706336067486,40.8690835171059,47.397369030549));
#23482=CARTESIAN_POINT('Ctrl Pts',(41.0996381208906,40.7873358221411,46.1494151750972));
#23483=CARTESIAN_POINT('Ctrl Pts',(43.2260810454985,40.6635128797074,45.8734020167473));
#23484=CARTESIAN_POINT('Ctrl Pts',(44.6354314050272,40.5372871373016,47.5442859344671));
#23485=CARTESIAN_POINT('Ctrl Pts',(43.992617684286,40.4110613948957,49.6335231212952));
#23486=CARTESIAN_POINT('Ctrl Pts',(42.5236823535331,40.3229713973105,50.0450157258572));
#23487=CARTESIAN_POINT('Ctrl Pts',(41.8501070242599,40.2769566471939,49.8531354571792));
#23488=CARTESIAN_POINT('Ctrl Pts',(41.7933319732428,40.273017144546,49.8339081536803));
#23489=CARTESIAN_POINT('Origin',(42.4,48.4493818343519,48.));
#23490=CARTESIAN_POINT('',(41.7943887027378,39.3084106968695,49.8307330830672));
#23491=CARTESIAN_POINT('',(41.7941386883808,39.4806729614233,49.8315224890738));
#23492=CARTESIAN_POINT('',(41.7941388317924,48.4493818343519,49.8315225365138));
#23493=CARTESIAN_POINT('',(40.4723183568643,39.943967372631,47.9983796934389));
#23494=CARTESIAN_POINT('Ctrl Pts',(40.4723183568643,39.943967372631,47.9983796934389));
#23495=CARTESIAN_POINT('Ctrl Pts',(40.4707394637107,39.9308026672141,47.7970115409001));
#23496=CARTESIAN_POINT('Ctrl Pts',(40.5925624326654,39.8755627143287,46.9539226443301));
#23497=CARTESIAN_POINT('Ctrl Pts',(41.8157413936134,39.7782475139746,45.7946723748715));
#23498=CARTESIAN_POINT('Ctrl Pts',(43.9386634949042,39.6520217715687,46.3155586377849));
#23499=CARTESIAN_POINT('Ctrl Pts',(44.6490663174714,39.5257960291628,48.3827907429751));
#23500=CARTESIAN_POINT('Ctrl Pts',(43.4201964457156,39.4112590042631,49.939726251279));
#23501=CARTESIAN_POINT('Ctrl Pts',(42.2366982772441,39.338797226832,49.9723701804534));
#23502=CARTESIAN_POINT('Ctrl Pts',(41.794388702738,39.3084106968696,49.8307330830672));
#23503=CARTESIAN_POINT('Ctrl Pts',(40.4708706300359,39.9431346927996,47.9984408842249));
#23504=CARTESIAN_POINT('Ctrl Pts',(40.4708198929901,39.9469209793088,48.0612189837307));
#23505=CARTESIAN_POINT('Ctrl Pts',(40.4738335460248,39.9507533765101,48.1239587143083));
#23506=CARTESIAN_POINT('Ctrl Pts',(40.4829575575197,39.9566479477974,48.2179258832443));
#23507=CARTESIAN_POINT('Ctrl Pts',(40.486788968357,39.9586440079182,48.2493326845192));
#23508=CARTESIAN_POINT('Ctrl Pts',(40.4930226546594,39.9613803307887,48.2917290150256));
#23509=CARTESIAN_POINT('Ctrl Pts',(40.4947513793214,39.9620996324809,48.3028136368557));
#23510=CARTESIAN_POINT('Ctrl Pts',(40.4979882649397,39.963380594018,48.3224425308214));
#23511=CARTESIAN_POINT('Ctrl Pts',(40.4994575820188,39.963941019675,48.3309929597083));
#23512=CARTESIAN_POINT('Ctrl Pts',(40.5025547379043,39.9650814816492,48.3483154166093));
#23513=CARTESIAN_POINT('Ctrl Pts',(40.5041858524087,39.9656616091957,48.3570866357031));
#23514=CARTESIAN_POINT('Ctrl Pts',(40.5077428997219,39.9668853856204,48.3755028016507));
#23515=CARTESIAN_POINT('Ctrl Pts',(40.5096818636515,39.9675294361126,48.3851449401285));
#23516=CARTESIAN_POINT('Ctrl Pts',(40.5150043720375,39.9692389829103,48.4106040159622));
#23517=CARTESIAN_POINT('Ctrl Pts',(40.518513197882,39.9703084618701,48.426393669733));
#23518=CARTESIAN_POINT('Ctrl Pts',(40.5348792070062,39.9750584023931,48.4959010127887));
#23519=CARTESIAN_POINT('Ctrl Pts',(40.549840314866,39.978805646307,48.5490915100576));
#23520=CARTESIAN_POINT('Ctrl Pts',(40.5873785567798,39.9871146086576,48.663469104035));
#23521=CARTESIAN_POINT('Ctrl Pts',(40.610817533297,39.9916969155441,48.7243014571535));
#23522=CARTESIAN_POINT('Ctrl Pts',(40.6913670948981,40.0057803290618,48.9054456747975));
#23523=CARTESIAN_POINT('Ctrl Pts',(40.7578893999033,40.0154128887556,49.0211432663966));
#23524=CARTESIAN_POINT('Ctrl Pts',(40.8459046548955,40.025761835615,49.1430785446304));
#23525=CARTESIAN_POINT('Ctrl Pts',(40.856201949067,40.0269416262726,49.1569479352129));
#23526=CARTESIAN_POINT('Ctrl Pts',(40.8745582195432,40.0289889028447,49.1809903803335));
#23527=CARTESIAN_POINT('Ctrl Pts',(40.882536022862,40.029860989169,49.1912237424591));
#23528=CARTESIAN_POINT('Ctrl Pts',(40.8945474054465,40.0311471005716,49.2063145860914));
#23529=CARTESIAN_POINT('Ctrl Pts',(40.8985023630385,40.0315663472175,49.2112337693731));
#23530=CARTESIAN_POINT('Ctrl Pts',(40.9053183806479,40.0322815531519,49.2196268548349));
#23531=CARTESIAN_POINT('Ctrl Pts',(40.9081675267248,40.0325783477594,49.2231102491008));
#23532=CARTESIAN_POINT('Ctrl Pts',(40.9146788241066,40.0332516981206,49.2310144247334));
#23533=CARTESIAN_POINT('Ctrl Pts',(40.9183485352365,40.0336276985401,49.2354288520781));
#23534=CARTESIAN_POINT('Ctrl Pts',(40.9284323800113,40.0346516044508,49.2474495138265));
#23535=CARTESIAN_POINT('Ctrl Pts',(40.9348858458118,40.0352967290142,49.2550227389352));
#23536=CARTESIAN_POINT('Ctrl Pts',(40.9682655366456,40.0385840068125,49.2935858449541));
#23537=CARTESIAN_POINT('Ctrl Pts',(40.9961195476466,40.0411641104287,49.3237628743878));
#23538=CARTESIAN_POINT('Ctrl Pts',(41.0402111799009,40.0450498620308,49.3685731225626));
#23539=CARTESIAN_POINT('Ctrl Pts',(41.0557675928957,40.0463854687096,49.3838559603307));
#23540=CARTESIAN_POINT('Ctrl Pts',(41.1468999684066,40.0540324283081,49.4703985701753));
#23541=CARTESIAN_POINT('Ctrl Pts',(41.2278759628396,40.06014924869,49.5357273945426));
#23542=CARTESIAN_POINT('Ctrl Pts',(41.3714815013165,40.0705709040585,49.6335781407554));
#23543=CARTESIAN_POINT('Ctrl Pts',(41.4313346834385,40.0748039198113,49.6697647122206));
#23544=CARTESIAN_POINT('Ctrl Pts',(41.5182463594611,40.0809141772239,49.7160624442938));
#23545=CARTESIAN_POINT('Ctrl Pts',(41.5437717730731,40.0827041644582,49.7289398179383));
#23546=CARTESIAN_POINT('Ctrl Pts',(41.5893784605062,40.0859014441967,49.7506903647484));
#23547=CARTESIAN_POINT('Ctrl Pts',(41.6093429998216,40.0873007461735,49.7597969993163));
#23548=CARTESIAN_POINT('Ctrl Pts',(41.6392824052511,40.0894008182492,49.7728412622097));
#23549=CARTESIAN_POINT('Ctrl Pts',(41.6491422435325,40.0900926830378,49.7770396793133));
#23550=CARTESIAN_POINT('Ctrl Pts',(41.6590906632278,40.0907911564754,49.7811782378637));
#23551=CARTESIAN_POINT('Ctrl Pts',(41.6591449388137,40.0907949671481,49.7812008136845));
#23552=CARTESIAN_POINT('Ctrl Pts',(41.6592566585854,40.090802810984,49.7812472773089));
#23553=CARTESIAN_POINT('Ctrl Pts',(41.659314102755,40.0908068441474,49.7812711647565));
#23554=CARTESIAN_POINT('Ctrl Pts',(41.6594323553904,40.0908151467091,49.7813203319432));
#23555=CARTESIAN_POINT('Ctrl Pts',(41.659493163925,40.0908194161136,49.7813456113183));
#23556=CARTESIAN_POINT('Ctrl Pts',(41.6596183543239,40.0908282058388,49.7813976480581));
#23557=CARTESIAN_POINT('Ctrl Pts',(41.6596827363164,40.0908327261702,49.7814244050346));
#23558=CARTESIAN_POINT('Ctrl Pts',(41.6598152965887,40.0908420334086,49.7814794882868));
#23559=CARTESIAN_POINT('Ctrl Pts',(41.6598834752016,40.0908468203409,49.7815078142043));
#23560=CARTESIAN_POINT('Ctrl Pts',(41.6600238676881,40.0908566775662,49.781566133104));
#23561=CARTESIAN_POINT('Ctrl Pts',(41.6600960816602,40.0908617478683,49.7815961255683));
#23562=CARTESIAN_POINT('Ctrl Pts',(41.6602448002229,40.0908721897694,49.7816578819079));
#23563=CARTESIAN_POINT('Ctrl Pts',(41.6603213048771,40.0908775613753,49.7816896451804));
#23564=CARTESIAN_POINT('Ctrl Pts',(41.6604788776197,40.0908886250471,49.7817550544779));
#23565=CARTESIAN_POINT('Ctrl Pts',(41.6605599460215,40.0908943171379,49.7817886999239));
#23566=CARTESIAN_POINT('Ctrl Pts',(41.6607269381773,40.0909060422848,49.7818579925507));
#23567=CARTESIAN_POINT('Ctrl Pts',(41.6608128624655,40.0909120753818,49.7818936391539));
#23568=CARTESIAN_POINT('Ctrl Pts',(41.660989880056,40.0909245045748,49.7819670617734));
#23569=CARTESIAN_POINT('Ctrl Pts',(41.6610809735456,40.0909309006878,49.7820048369655));
#23570=CARTESIAN_POINT('Ctrl Pts',(41.6612686646559,40.0909440794544,49.7820826529696));
#23571=CARTESIAN_POINT('Ctrl Pts',(41.6613652627393,40.0909508621447,49.7821226929553));
#23572=CARTESIAN_POINT('Ctrl Pts',(41.6615643231018,40.0909648393614,49.7822051846756));
#23573=CARTESIAN_POINT('Ctrl Pts',(41.661666785674,40.090972033913,49.7822476353817));
#23574=CARTESIAN_POINT('Ctrl Pts',(41.6618779607458,40.0909868619517,49.7823351048308));
#23575=CARTESIAN_POINT('Ctrl Pts',(41.6619866737438,40.0909944954791,49.7823801224804));
#23576=CARTESIAN_POINT('Ctrl Pts',(41.6622107635565,40.0910102305483,49.7824728932246));
#23577=CARTESIAN_POINT('Ctrl Pts',(41.6623261410521,40.091018332144,49.7825206451307));
#23578=CARTESIAN_POINT('Ctrl Pts',(41.6625640051157,40.0910350346339,49.7826190641635));
#23579=CARTESIAN_POINT('Ctrl Pts',(41.6626864920904,40.0910436355636,49.7826697297941));
#23580=CARTESIAN_POINT('Ctrl Pts',(41.6629390524401,40.0910613702606,49.7827741686183));
#23581=CARTESIAN_POINT('Ctrl Pts',(41.6630691265414,40.0910705040869,49.7828279402271));
#23582=CARTESIAN_POINT('Ctrl Pts',(41.6633373748465,40.0910893406741,49.7829387975903));
#23583=CARTESIAN_POINT('Ctrl Pts',(41.6634755496589,40.0910990434868,49.7829958814592));
#23584=CARTESIAN_POINT('Ctrl Pts',(41.6637605509215,40.0911190568044,49.7831135846472));
#23585=CARTESIAN_POINT('Ctrl Pts',(41.6639073782758,40.0911293673831,49.7831742019152));
#23586=CARTESIAN_POINT('Ctrl Pts',(41.6642102781484,40.0911506379438,49.7832992095053));
#23587=CARTESIAN_POINT('Ctrl Pts',(41.6643663515719,40.0911615980011,49.7833635974487));
#23588=CARTESIAN_POINT('Ctrl Pts',(41.6646883813852,40.0911842123444,49.7834964010764));
#23589=CARTESIAN_POINT('Ctrl Pts',(41.6648543389566,40.0911958667267,49.7835648141212));
#23590=CARTESIAN_POINT('Ctrl Pts',(41.6651968232844,40.091219917952,49.7837059412464));
#23591=CARTESIAN_POINT('Ctrl Pts',(41.665373351295,40.0912323148981,49.7837786522889));
#23592=CARTESIAN_POINT('Ctrl Pts',(41.6657377140861,40.0912579030969,49.7839286683168));
#23593=CARTESIAN_POINT('Ctrl Pts',(41.665925550341,40.0912710944704,49.7840059698655));
#23594=CARTESIAN_POINT('Ctrl Pts',(41.6662510195833,40.0912939517994,49.7841398523607));
#23595=CARTESIAN_POINT('Ctrl Pts',(41.6663886468353,40.0913036172827,49.7841964470181));
#23596=CARTESIAN_POINT('Ctrl Pts',(41.6667109039363,40.0913262494038,49.7843289210064));
#23597=CARTESIAN_POINT('Ctrl Pts',(41.6668955389595,40.0913392164695,49.7844047875828));
#23598=CARTESIAN_POINT('Ctrl Pts',(41.6673278852495,40.0913695808376,49.7845823603499));
#23599=CARTESIAN_POINT('Ctrl Pts',(41.6675756059249,40.0913869789176,49.7846840436247));
#23600=CARTESIAN_POINT('Ctrl Pts',(41.6681556685602,40.091427718874,49.7849220040277));
#23601=CARTESIAN_POINT('Ctrl Pts',(41.6684880273522,40.091451062144,49.7850582398889));
#23602=CARTESIAN_POINT('Ctrl Pts',(41.6770663736592,40.0920535759897,49.7885717573387));
#23603=CARTESIAN_POINT('Ctrl Pts',(41.6853355055779,40.0926346680125,49.7918919094512));
#23604=CARTESIAN_POINT('Ctrl Pts',(41.7042683260003,40.0939659451399,49.7993417573945));
#23605=CARTESIAN_POINT('Ctrl Pts',(41.7149462439636,40.094717363842,49.803434130722));
#23606=CARTESIAN_POINT('Ctrl Pts',(41.7480799877713,40.0970512031551,49.815796104629));
#23607=CARTESIAN_POINT('Ctrl Pts',(41.7706530473724,40.098644282232,49.8237427234191));
#23608=CARTESIAN_POINT('Ctrl Pts',(41.793624421975,40.1002692745907,49.8313523114559));
#23609=CARTESIAN_POINT('Ctrl Pts',(41.7938816187901,40.1002874691372,49.8314374513637));
#23610=CARTESIAN_POINT('Ctrl Pts',(41.7941388318207,40.1003056653051,49.8315225365232));
#23611=CARTESIAN_POINT('',(40.4728302759175,40.1150077701205,48.0014409743479));
#23612=CARTESIAN_POINT('Ctrl Pts',(41.7933319732428,40.273017144546,49.8339081536803));
#23613=CARTESIAN_POINT('Ctrl Pts',(41.2437298911391,40.2348813997253,49.6477812220981));
#23614=CARTESIAN_POINT('Ctrl Pts',(40.6001596419136,40.1822116082501,49.0283757153127));
#23615=CARTESIAN_POINT('Ctrl Pts',(40.471311607613,40.1295418167751,48.2239035093802));
#23616=CARTESIAN_POINT('Ctrl Pts',(40.4728302759175,40.1150077701205,48.0014409743479));
#23617=CARTESIAN_POINT('Ctrl Pts',(40.4708704789563,40.1161353185692,48.0013593887718));
#23618=CARTESIAN_POINT('Ctrl Pts',(40.4708380686763,40.1133347529338,47.9553654617617));
#23619=CARTESIAN_POINT('Ctrl Pts',(40.4724505230042,40.1105018024918,47.9093871381568));
#23620=CARTESIAN_POINT('Ctrl Pts',(40.4776042865313,40.1059406866609,47.8367260892297));
#23621=CARTESIAN_POINT('Ctrl Pts',(40.480063172739,40.1042439796843,47.8099838988324));
#23622=CARTESIAN_POINT('Ctrl Pts',(40.4843588666476,40.101803077152,47.7719838627056));
#23623=CARTESIAN_POINT('Ctrl Pts',(40.485738604911,40.1010729939168,47.7606767605226));
#23624=CARTESIAN_POINT('Ctrl Pts',(40.4883527066305,40.0997777399369,47.7407251993612));
#23625=CARTESIAN_POINT('Ctrl Pts',(40.4895457866756,40.0992138735614,47.7320755868885));
#23626=CARTESIAN_POINT('Ctrl Pts',(40.4920182108331,40.0980964698556,47.7150078105216));
#23627=CARTESIAN_POINT('Ctrl Pts',(40.4932946517388,40.0975430361036,47.7065894227091));
#23628=CARTESIAN_POINT('Ctrl Pts',(40.4961311359064,40.0963608234212,47.6886828600618));
#23629=CARTESIAN_POINT('Ctrl Pts',(40.4977064673102,40.0957315726104,47.6791973767437));
#23630=CARTESIAN_POINT('Ctrl Pts',(40.5019505023879,40.0941034184224,47.6547741086693));
#23631=CARTESIAN_POINT('Ctrl Pts',(40.5047246192555,40.093101187367,47.6398555566224));
#23632=CARTESIAN_POINT('Ctrl Pts',(40.516659863959,40.0890232439818,47.5796324594816));
#23633=CARTESIAN_POINT('Ctrl Pts',(40.5272711802967,40.0859018538545,47.5346344585295));
#23634=CARTESIAN_POINT('Ctrl Pts',(40.558779960203,40.0777290546985,47.4196739905426));
#23635=CARTESIAN_POINT('Ctrl Pts',(40.5820499012658,40.0726115679466,47.3504424002996));
#23636=CARTESIAN_POINT('Ctrl Pts',(40.662055976507,40.0573393182124,47.1506982591026));
#23637=CARTESIAN_POINT('Ctrl Pts',(40.7293622893511,40.0470279472954,47.0249433346778));
#23638=CARTESIAN_POINT('Ctrl Pts',(40.8217736054067,40.0358554383224,46.8904121543121));
#23639=CARTESIAN_POINT('Ctrl Pts',(40.8339488644304,40.0344316920863,46.8732934410902));
#23640=CARTESIAN_POINT('Ctrl Pts',(40.8509325406227,40.0325136301454,46.8502213378908));
#23641=CARTESIAN_POINT('Ctrl Pts',(40.8554998181267,40.032004272587,46.8440933607709));
#23642=CARTESIAN_POINT('Ctrl Pts',(40.8632219050962,40.0311540398518,46.8338600228404));
#23643=CARTESIAN_POINT('Ctrl Pts',(40.8663570053764,40.0308118272764,46.8297399748523));
#23644=CARTESIAN_POINT('Ctrl Pts',(40.8723560676635,40.0301627088197,46.8219217129795));
#23645=CARTESIAN_POINT('Ctrl Pts',(40.8752169423016,40.0298555843619,46.8182212294692));
#23646=CARTESIAN_POINT('Ctrl Pts',(40.882062693014,40.0291263360085,46.8094326328191));
#23647=CARTESIAN_POINT('Ctrl Pts',(40.8860597656042,40.0287050652564,46.8043540267516));
#23648=CARTESIAN_POINT('Ctrl Pts',(40.900360758893,40.0272133944104,46.7863701494729));
#23649=CARTESIAN_POINT('Ctrl Pts',(40.9108051222076,40.0261524203982,46.7735767747563));
#23650=CARTESIAN_POINT('Ctrl Pts',(40.9846375109812,40.0188343754772,46.6854731063218));
#23651=CARTESIAN_POINT('Ctrl Pts',(41.053552377494,40.0129146061821,46.614967268689));
#23652=CARTESIAN_POINT('Ctrl Pts',(41.1920313682759,40.0019065625327,46.4934434472128));
#23653=CARTESIAN_POINT('Ctrl Pts',(41.2602072208809,39.9968211917294,46.4412271586212));
#23654=CARTESIAN_POINT('Ctrl Pts',(41.3749780756536,39.9884664598837,46.3648905178379));
#23655=CARTESIAN_POINT('Ctrl Pts',(41.4194734034244,39.9852736659388,46.3378267373196));
#23656=CARTESIAN_POINT('Ctrl Pts',(41.4855843287958,39.9805518435421,46.3011945375382));
#23657=CARTESIAN_POINT('Ctrl Pts',(41.5063683849867,39.9790705496073,46.2901700425527));
#23658=CARTESIAN_POINT('Ctrl Pts',(41.5394708728636,39.9767129709179,46.2733799069669));
#23659=CARTESIAN_POINT('Ctrl Pts',(41.5516579478092,39.9758453559421,46.2673595087847));
#23660=CARTESIAN_POINT('Ctrl Pts',(41.5747992725415,39.9741979302012,46.2562304087504));
#23661=CARTESIAN_POINT('Ctrl Pts',(41.5857399356248,39.9734190831801,46.2510948668921));
#23662=CARTESIAN_POINT('Ctrl Pts',(41.6048147607361,39.9720608572839,46.2423589371548));
#23663=CARTESIAN_POINT('Ctrl Pts',(41.6129269920797,39.9714831252402,46.2387113393016));
#23664=CARTESIAN_POINT('Ctrl Pts',(41.6286764237479,39.9703611653448,46.2317602725213));
#23665=CARTESIAN_POINT('Ctrl Pts',(41.6363103561749,39.9698171913481,46.2284498546886));
#23666=CARTESIAN_POINT('Ctrl Pts',(41.6563075030613,39.9683917345989,46.2199314629391));
#23667=CARTESIAN_POINT('Ctrl Pts',(41.6687038713394,39.9675075731117,46.2148029567246));
#23668=CARTESIAN_POINT('Ctrl Pts',(41.7121333162006,39.9644076366284,46.1973639978971));
#23669=CARTESIAN_POINT('Ctrl Pts',(41.7434301193798,39.9621694017786,46.1857307570226));
#23670=CARTESIAN_POINT('Ctrl Pts',(41.9201550575998,39.9494995049822,46.1252124088615));
#23671=CARTESIAN_POINT('Ctrl Pts',(42.0706886883256,39.9385275372414,46.0930081611002));
#23672=CARTESIAN_POINT('Ctrl Pts',(42.2369739080843,39.9266172723342,46.0777225612502));
#23673=CARTESIAN_POINT('Ctrl Pts',(42.2505495367126,39.9256469141815,46.0766194805214));
#23674=CARTESIAN_POINT('Ctrl Pts',(42.3428892935131,39.9190639442161,46.0701000149224));
#23675=CARTESIAN_POINT('Ctrl Pts',(42.4219196440293,39.9135122025576,46.0693788444267));
#23676=CARTESIAN_POINT('Ctrl Pts',(42.5120246297948,39.9074238000866,46.0740924661395));
#23677=CARTESIAN_POINT('Ctrl Pts',(42.5232643190722,39.906668692889,46.0747791635083));
#23678=CARTESIAN_POINT('Ctrl Pts',(42.5404457227236,39.9055217293803,46.075979961664));
#23679=CARTESIAN_POINT('Ctrl Pts',(42.5463919084768,39.9051261281493,46.0764232480964));
#23680=CARTESIAN_POINT('Ctrl Pts',(42.55729477516,39.904403339198,46.0772869028557));
#23681=CARTESIAN_POINT('Ctrl Pts',(42.5622518960863,39.9040757063069,46.0776988728193));
#23682=CARTESIAN_POINT('Ctrl Pts',(42.5734610277722,39.9033370679969,46.0786740956611));
#23683=CARTESIAN_POINT('Ctrl Pts',(42.5797119171643,39.9029267009378,46.0792486916809));
#23684=CARTESIAN_POINT('Ctrl Pts',(42.5958978742643,39.9018678407538,46.0808162496946));
#23685=CARTESIAN_POINT('Ctrl Pts',(42.6058283833303,39.9012218542597,46.081855862707));
#23686=CARTESIAN_POINT('Ctrl Pts',(42.6735305633519,39.8968399712864,46.0894753612223));
#23687=CARTESIAN_POINT('Ctrl Pts',(42.7309932505305,39.8932308825393,46.0985878257651));
#23688=CARTESIAN_POINT('Ctrl Pts',(42.8329844938905,39.886883859484,46.1195268028226));
#23689=CARTESIAN_POINT('Ctrl Pts',(42.8776639593492,39.8841240645453,46.1303763837589));
#23690=CARTESIAN_POINT('Ctrl Pts',(43.0308717896726,39.874609742797,46.1734314810836));
#23691=CARTESIAN_POINT('Ctrl Pts',(43.1369170989435,39.8679205080747,46.2135780262212));
#23692=CARTESIAN_POINT('Ctrl Pts',(43.2904295826289,39.857456421598,46.287702987494));
#23693=CARTESIAN_POINT('Ctrl Pts',(43.3408895045421,39.853881560762,46.3149030070584));
#23694=CARTESIAN_POINT('Ctrl Pts',(43.4035980647876,39.8492206594647,46.3524010616639));
#23695=CARTESIAN_POINT('Ctrl Pts',(43.4170350706918,39.8482087111747,46.360661420472));
#23696=CARTESIAN_POINT('Ctrl Pts',(43.4386080599026,39.8465617064191,46.3742906680056));
#23697=CARTESIAN_POINT('Ctrl Pts',(43.4468074672948,39.8459304081136,46.3795581914682));
#23698=CARTESIAN_POINT('Ctrl Pts',(43.4624532356056,39.8447153774266,46.389777765402));
#23699=CARTESIAN_POINT('Ctrl Pts',(43.4699057826619,39.8441320270595,46.3947199202883));
#23700=CARTESIAN_POINT('Ctrl Pts',(43.4868641682392,39.8427939044853,46.4061364201039));
#23701=CARTESIAN_POINT('Ctrl Pts',(43.4963469330379,39.8420378757616,46.4126442666584));
#23702=CARTESIAN_POINT('Ctrl Pts',(43.5262238119617,39.8396307198262,46.4335436467429));
#23703=CARTESIAN_POINT('Ctrl Pts',(43.5463963894135,39.8379677574257,46.4482458957952));
#23704=CARTESIAN_POINT('Ctrl Pts',(43.6801558865336,39.8266790944768,46.5497648616212));
#23705=CARTESIAN_POINT('Ctrl Pts',(43.7840536772881,39.816565033277,46.6485704291856));
#23706=CARTESIAN_POINT('Ctrl Pts',(43.8985986243681,39.8038559302602,46.7846937843164));
#23707=CARTESIAN_POINT('Ctrl Pts',(43.9203963046694,39.8013554931575,46.8120765354504));
#23708=CARTESIAN_POINT('Ctrl Pts',(43.9900313651473,39.7931155584811,46.9046123326988));
#23709=CARTESIAN_POINT('Ctrl Pts',(44.0345256058119,39.7874271401505,46.9721853214095));
#23710=CARTESIAN_POINT('Ctrl Pts',(44.0802638157801,39.7812094070985,47.052168896266));
#23711=CARTESIAN_POINT('Ctrl Pts',(44.0857880920703,39.7804514458512,47.0620294164645));
#23712=CARTESIAN_POINT('Ctrl Pts',(44.094098229957,39.7793010665626,47.0771731467608));
#23713=CARTESIAN_POINT('Ctrl Pts',(44.0969466365806,39.7789048701243,47.0824214863061));
#23714=CARTESIAN_POINT('Ctrl Pts',(44.1021228515544,39.7781815145435,47.0920654795095));
#23715=CARTESIAN_POINT('Ctrl Pts',(44.1044580368625,39.777853905374,47.0964569202328));
#23716=CARTESIAN_POINT('Ctrl Pts',(44.1096970795922,39.7771159690502,47.1064018111144));
#23717=CARTESIAN_POINT('Ctrl Pts',(44.1125908776776,39.7767062747462,47.1119604087828));
#23718=CARTESIAN_POINT('Ctrl Pts',(44.1200089315979,39.7756503254396,47.1263806175873));
#23719=CARTESIAN_POINT('Ctrl Pts',(44.124491876757,39.7750065542618,47.1352634347741));
#23720=CARTESIAN_POINT('Ctrl Pts',(44.1543135600822,39.770682706301,47.1955085021706));
#23721=CARTESIAN_POINT('Ctrl Pts',(44.1774255081934,39.7671256235491,47.2479477623848));
#23722=CARTESIAN_POINT('Ctrl Pts',(44.2146037969928,39.7608639049724,47.3436355463144));
#23723=CARTESIAN_POINT('Ctrl Pts',(44.2295394843348,39.758137845114,47.386496279672));
#23724=CARTESIAN_POINT('Ctrl Pts',(44.2767446232207,39.7485859166721,47.5390806858801));
#23725=CARTESIAN_POINT('Ctrl Pts',(44.3007586060393,39.7418317044264,47.6510984688772));
#23726=CARTESIAN_POINT('Ctrl Pts',(44.3217420361472,39.7312792228694,47.8217611548666));
#23727=CARTESIAN_POINT('Ctrl Pts',(44.326206988774,39.7276856069946,47.8792225341522));
#23728=CARTESIAN_POINT('Ctrl Pts',(44.3286119373994,39.7230033882651,47.9525849827165));
#23729=CARTESIAN_POINT('Ctrl Pts',(44.3289355724879,39.721989739491,47.9683816175594));
#23730=CARTESIAN_POINT('Ctrl Pts',(44.3291451006418,39.7203406462953,47.993931260495));
#23731=CARTESIAN_POINT('Ctrl Pts',(44.3291511294837,39.7197089779125,48.0036827604339));
#23732=CARTESIAN_POINT('Ctrl Pts',(44.3290209665491,39.7184936963109,48.0223741400859));
#23733=CARTESIAN_POINT('Ctrl Pts',(44.3288965572465,39.7179104686639,48.0313138695423));
#23734=CARTESIAN_POINT('Ctrl Pts',(44.3284702899616,39.7165732777726,48.051738696733));
#23735=CARTESIAN_POINT('Ctrl Pts',(44.3281279665236,39.7158180640398,48.0632225195437));
#23736=CARTESIAN_POINT('Ctrl Pts',(44.3267191239553,39.7134161752024,48.0995774735461));
#23737=CARTESIAN_POINT('Ctrl Pts',(44.3252737995631,39.7117577381274,48.1244305173558));
#23738=CARTESIAN_POINT('Ctrl Pts',(44.3121934537165,39.7003925155832,48.2929963390269));
#23739=CARTESIAN_POINT('Ctrl Pts',(44.2849607637538,39.6901879564356,48.4350156825309));
#23740=CARTESIAN_POINT('Ctrl Pts',(44.2090952952734,39.6719299524125,48.6790706088753));
#23741=CARTESIAN_POINT('Ctrl Pts',(44.1668501527213,39.6639626757688,48.7824374944683));
#23742=CARTESIAN_POINT('Ctrl Pts',(44.1098094001838,39.6555095117496,48.8934610254329));
#23743=CARTESIAN_POINT('Ctrl Pts',(44.1035851536705,39.654611768955,48.9052725763823));
#23744=CARTESIAN_POINT('Ctrl Pts',(44.0942040922014,39.6532954859621,48.9226352484668));
#23745=CARTESIAN_POINT('Ctrl Pts',(44.0911416936151,39.6528713708583,48.9282365446162));
#23746=CARTESIAN_POINT('Ctrl Pts',(44.0856404833439,39.6521194829628,48.9381809664632));
#23747=CARTESIAN_POINT('Ctrl Pts',(44.083212600403,39.6517910381102,48.9425299510779));
#23748=CARTESIAN_POINT('Ctrl Pts',(44.0778823967139,39.6510773235496,48.9519914802742));
#23749=CARTESIAN_POINT('Ctrl Pts',(44.0749735385761,39.6506924778185,48.9571001844423));
#23750=CARTESIAN_POINT('Ctrl Pts',(44.0667728298719,39.6496201861095,48.9713508460675));
#23751=CARTESIAN_POINT('Ctrl Pts',(44.061429084704,39.6489359713391,48.9804629219373));
#23752=CARTESIAN_POINT('Ctrl Pts',(44.0299491234931,39.6449856312155,49.033145612655));
#23753=CARTESIAN_POINT('Ctrl Pts',(44.0021721767424,39.6418153969879,49.0757180458397));
#23754=CARTESIAN_POINT('Ctrl Pts',(43.8735284995272,39.6281992354596,49.2568253026773));
#23755=CARTESIAN_POINT('Ctrl Pts',(43.7561479631914,39.6183225634696,49.3826660682542));
#23756=CARTESIAN_POINT('Ctrl Pts',(43.5960456342671,39.6055800605953,49.5140328656471));
#23757=CARTESIAN_POINT('Ctrl Pts',(43.5677840085502,39.6033572793829,49.5359365082439));
#23758=CARTESIAN_POINT('Ctrl Pts',(43.5177101487212,39.5994493960218,49.5725641084382));
#23759=CARTESIAN_POINT('Ctrl Pts',(43.4961746749687,39.5977780538879,49.5876507258598));
#23760=CARTESIAN_POINT('Ctrl Pts',(43.4644813066983,39.5953280154655,49.6089011618202));
#23761=CARTESIAN_POINT('Ctrl Pts',(43.4545636135286,39.5945626785039,49.615419133067));
#23762=CARTESIAN_POINT('Ctrl Pts',(43.4370480333845,39.5932130366146,49.6267004450533));
#23763=CARTESIAN_POINT('Ctrl Pts',(43.429475823536,39.5926302211794,49.6315031368898));
#23764=CARTESIAN_POINT('Ctrl Pts',(43.4136684988975,39.5914147710388,49.6413751071379));
#23765=CARTESIAN_POINT('Ctrl Pts',(43.4054282165221,39.5907818328079,49.646435593526));
#23766=CARTESIAN_POINT('Ctrl Pts',(43.3839448822949,39.5891332265844,49.6594074208124));
#23767=CARTESIAN_POINT('Ctrl Pts',(43.3706445780308,39.588114069993,49.6672221205236));
#23768=CARTESIAN_POINT('Ctrl Pts',(43.3152532414906,39.5838747655288,49.6988802705821));
#23769=CARTESIAN_POINT('Ctrl Pts',(43.2723696561869,39.5806042569261,49.7212940326191));
#23770=CARTESIAN_POINT('Ctrl Pts',(43.0876736738055,39.5665578581451,49.8091527426551));
#23771=CARTESIAN_POINT('Ctrl Pts',(42.9390435451542,39.5552871755764,49.8588565344614));
#23772=CARTESIAN_POINT('Ctrl Pts',(42.7388802085037,39.540796999496,49.899743108681));
#23773=CARTESIAN_POINT('Ctrl Pts',(42.691329001164,39.5374092627518,49.9076141402746));
#23774=CARTESIAN_POINT('Ctrl Pts',(42.6251777098498,39.5328111103733,49.9160323115752));
#23775=CARTESIAN_POINT('Ctrl Pts',(42.60679195547,39.5315453356662,49.9181037413716));
#23776=CARTESIAN_POINT('Ctrl Pts',(42.5747613362871,39.5293645275621,49.9212465342048));
#23777=CARTESIAN_POINT('Ctrl Pts',(42.5611298369547,39.5284440724283,49.9224377679704));
#23778=CARTESIAN_POINT('Ctrl Pts',(42.5410579681312,39.527101091732,49.923976812116));
#23779=CARTESIAN_POINT('Ctrl Pts',(42.5346270411319,39.526672670391,49.9244374987805));
#23780=CARTESIAN_POINT('Ctrl Pts',(42.5232639473802,39.5259191056261,49.9251942674772));
#23781=CARTESIAN_POINT('Ctrl Pts',(42.5183328193101,39.5255932366131,49.9255036520611));
#23782=CARTESIAN_POINT('Ctrl Pts',(42.507596149151,39.5248862349984,49.9261358808473));
#23783=CARTESIAN_POINT('Ctrl Pts',(42.5017903092753,39.5245055109469,49.926451426312));
#23784=CARTESIAN_POINT('Ctrl Pts',(42.4857177506217,39.5234557047476,49.9272521012426));
#23785=CARTESIAN_POINT('Ctrl Pts',(42.4754482663264,39.5227896413108,49.9276814479935));
#23786=CARTESIAN_POINT('Ctrl Pts',(42.4193470767905,39.519174289965,49.9295779067254));
#23787=CARTESIAN_POINT('Ctrl Pts',(42.3734737023976,39.5163027972602,49.9294927621431));
#23788=CARTESIAN_POINT('Ctrl Pts',(42.2160620065461,39.5066081559006,49.9235844778319));
#23789=CARTESIAN_POINT('Ctrl Pts',(42.1050481183819,39.5000351013078,49.9097165252285));
#23790=CARTESIAN_POINT('Ctrl Pts',(41.9276400629401,39.4891781157111,49.871706447512));
#23791=CARTESIAN_POINT('Ctrl Pts',(41.8603051399067,39.4849734388322,49.8534101226387));
#23792=CARTESIAN_POINT('Ctrl Pts',(41.7941386883808,39.4806729614233,49.8315224890738));
#23793=CARTESIAN_POINT('Origin',(42.4,48.4493818343519,48.));
#23794=CARTESIAN_POINT('',(41.7941388317924,38.5145390814761,49.8315225365138));
#23795=CARTESIAN_POINT('',(41.7941383335288,38.6866921868075,49.8315223716899));
#23796=CARTESIAN_POINT('',(41.7941388317924,48.4493818343519,49.8315225365138));
#23797=CARTESIAN_POINT('',(40.4705489998756,39.1502182104393,47.9997072692622));
#23798=CARTESIAN_POINT('Ctrl Pts',(40.4708700223059,39.1502181656481,47.9997066371674));
#23799=CARTESIAN_POINT('Ctrl Pts',(40.4708724067228,39.1491850444138,47.9840269063358));
#23800=CARTESIAN_POINT('Ctrl Pts',(40.4710659517807,39.1481519231795,47.9683488185713));
#23801=CARTESIAN_POINT('Ctrl Pts',(40.4714505599335,39.1471188019453,47.9526754385228));
#23802=CARTESIAN_POINT('Ctrl Pts',(40.4731094555565,39.1426627333953,47.885072863346));
#23803=CARTESIAN_POINT('Ctrl Pts',(40.4783305474797,39.1382066648452,47.8174223947577));
#23804=CARTESIAN_POINT('Ctrl Pts',(40.4871205945074,39.1337505962952,47.7501301599985));
#23805=CARTESIAN_POINT('Ctrl Pts',(40.4958973182547,39.1293012819128,47.6829399216579));
#23806=CARTESIAN_POINT('Ctrl Pts',(40.5082321983288,39.1248519675304,47.6161073251916));
#23807=CARTESIAN_POINT('Ctrl Pts',(40.5240800039167,39.120402653148,47.5500369735246));
#23808=CARTESIAN_POINT('Ctrl Pts',(40.5399090630196,39.1159586018922,47.4840447769595));
#23809=CARTESIAN_POINT('Ctrl Pts',(40.5592426806972,39.1115145506363,47.4188135124089));
#23810=CARTESIAN_POINT('Ctrl Pts',(40.581984273194,39.1070704993804,47.3547392976586));
#23811=CARTESIAN_POINT('Ctrl Pts',(40.6047115389767,39.1026292477812,47.2907054482854));
#23812=CARTESIAN_POINT('Ctrl Pts',(40.6308423562216,39.098187996182,47.2278276671201));
#23813=CARTESIAN_POINT('Ctrl Pts',(40.6602302766802,39.0937467445828,47.1664870326626));
#23814=CARTESIAN_POINT('Ctrl Pts',(40.6896098416771,39.0893067557033,47.1051638383406));
#23815=CARTESIAN_POINT('Ctrl Pts',(40.7222444583952,39.0848667668239,47.045377368246));
#23816=CARTESIAN_POINT('Ctrl Pts',(40.7579402462904,39.0804267779444,46.9874871249474));
#23817=CARTESIAN_POINT('Ctrl Pts',(40.7936382236088,39.0759865167355,46.9295933309152));
#23818=CARTESIAN_POINT('Ctrl Pts',(40.832397483487,39.0715462555265,46.8735964134657));
#23819=CARTESIAN_POINT('Ctrl Pts',(40.8739800198014,39.0671059943176,46.8198281578793));
#23820=CARTESIAN_POINT('Ctrl Pts',(40.9156071642824,39.062660969765,46.7660022217491));
#23821=CARTESIAN_POINT('Ctrl Pts',(40.9600633266848,39.0582159452124,46.7144101099497));
#23822=CARTESIAN_POINT('Ctrl Pts',(41.0070699251909,39.0537709206598,46.665350846255));
#23823=CARTESIAN_POINT('Ctrl Pts',(41.054104956129,39.0493232074877,46.6162619085522));
#23824=CARTESIAN_POINT('Ctrl Pts',(41.1036931331262,39.0448754943155,46.5697092057024));
#23825=CARTESIAN_POINT('Ctrl Pts',(41.1555207669375,39.0404277811434,46.5259531909141));
#23826=CARTESIAN_POINT('Ctrl Pts',(41.207438295423,39.0359723534434,46.4821212816194));
#23827=CARTESIAN_POINT('Ctrl Pts',(41.2616026394671,39.0315169257434,46.4410960392844));
#23828=CARTESIAN_POINT('Ctrl Pts',(41.3176697199394,39.0270614980434,46.4030955815191));
#23829=CARTESIAN_POINT('Ctrl Pts',(41.3435442533007,39.0250053518754,46.3855586578214));
#23830=CARTESIAN_POINT('Ctrl Pts',(41.3698236599141,39.0229492057074,46.3686653037414));
#23831=CARTESIAN_POINT('Ctrl Pts',(41.3964724507869,39.0208930595394,46.3524336083573));
#23832=CARTESIAN_POINT('Ctrl Pts',(41.4542255622892,39.0164369909894,46.3172563683145));
#23833=CARTESIAN_POINT('Ctrl Pts',(41.5139460713761,39.0119809224394,46.2850491254104));
#23834=CARTESIAN_POINT('Ctrl Pts',(41.5752960700954,39.0075248538894,46.2560372753697));
#23835=CARTESIAN_POINT('Ctrl Pts',(41.6365530791826,39.003075539507,46.2270693992707));
#23836=CARTESIAN_POINT('Ctrl Pts',(41.6994342337059,38.9986262251246,46.2012875137176));
#23837=CARTESIAN_POINT('Ctrl Pts',(41.7635747817648,38.9941769107422,46.1788724650661));
#23838=CARTESIAN_POINT('Ctrl Pts',(41.8276394575007,38.9897328594863,46.1564839313395));
#23839=CARTESIAN_POINT('Ctrl Pts',(41.892960104418,38.9852888082304,46.1374544874787));
#23840=CARTESIAN_POINT('Ctrl Pts',(41.9591513253518,38.9808447569745,46.121917200185));
#23841=CARTESIAN_POINT('Ctrl Pts',(42.0253008472402,38.9764035053753,46.1063897010481));
#23842=CARTESIAN_POINT('Ctrl Pts',(42.0923193756932,38.9719622537761,46.0943501072782));
#23843=CARTESIAN_POINT('Ctrl Pts',(42.1598071857408,38.9675210021769,46.0858814120128));
#23844=CARTESIAN_POINT('Ctrl Pts',(42.2272758079114,38.9630810132975,46.0774151245345));
#23845=CARTESIAN_POINT('Ctrl Pts',(42.2952129571544,38.958641024418,46.0725177816399));
#23846=CARTESIAN_POINT('Ctrl Pts',(42.3632113939956,38.9542010355385,46.0712208121798));
#23847=CARTESIAN_POINT('Ctrl Pts',(42.4312140015627,38.9497607743296,46.0699237631693));
#23848=CARTESIAN_POINT('Ctrl Pts',(42.4992774104961,38.9453205131207,46.0722275327985));
#23849=CARTESIAN_POINT('Ctrl Pts',(42.5669938207757,38.9408802519118,46.07811144425));
#23850=CARTESIAN_POINT('Ctrl Pts',(42.6347828746501,38.9364352273592,46.0840016677385));
#23851=CARTESIAN_POINT('Ctrl Pts',(42.7022236941851,38.9319902028066,46.0934796546508));
#23852=CARTESIAN_POINT('Ctrl Pts',(42.768914081602,38.927545178254,46.1064728791761));
#23853=CARTESIAN_POINT('Ctrl Pts',(42.8356448073962,38.9230974650819,46.1194739627889));
#23854=CARTESIAN_POINT('Ctrl Pts',(42.9016237187846,38.9186497519098,46.1359943953654));
#23855=CARTESIAN_POINT('Ctrl Pts',(42.9664620640971,38.9142020387376,46.1559112584155));
#23856=CARTESIAN_POINT('Ctrl Pts',(43.0314128710733,38.9097466110376,46.1758626671275));
#23857=CARTESIAN_POINT('Ctrl Pts',(43.0952187004583,38.9052911833376,46.1992220937228));
#23858=CARTESIAN_POINT('Ctrl Pts',(43.1575099653391,38.9008357556376,46.2258181577663));
#23859=CARTESIAN_POINT('Ctrl Pts',(43.1862569127051,38.8987796094696,46.238092040062));
#23860=CARTESIAN_POINT('Ctrl Pts',(43.2146816329436,38.8967234633016,46.251054597812));
#23861=CARTESIAN_POINT('Ctrl Pts',(43.2427497133888,38.8946673171336,46.2646857698149));
#23862=CARTESIAN_POINT('Ctrl Pts',(43.3035787013652,38.8902112485836,46.2942271700357));
#23863=CARTESIAN_POINT('Ctrl Pts',(43.3629741837397,38.8857551800335,46.3270299500181));
#23864=CARTESIAN_POINT('Ctrl Pts',(43.4205637910556,38.8812991114835,46.3629318568593));
#23865=CARTESIAN_POINT('Ctrl Pts',(43.4780661084529,38.8768497971011,46.3987793463382));
#23866=CARTESIAN_POINT('Ctrl Pts',(43.5337675672398,38.8724004827187,46.437716381483));
#23867=CARTESIAN_POINT('Ctrl Pts',(43.5873187428817,38.8679511683363,46.4795340320475));
#23868=CARTESIAN_POINT('Ctrl Pts',(43.6408065724465,38.8635071170805,46.5213022162074));
#23869=CARTESIAN_POINT('Ctrl Pts',(43.6921487828764,38.8590630658246,46.5659439464106));
#23870=CARTESIAN_POINT('Ctrl Pts',(43.7410249647544,38.8546190145687,46.6132070807775));
#23871=CARTESIAN_POINT('Ctrl Pts',(43.7898703556891,38.8501777629695,46.6604404403864));
#23872=CARTESIAN_POINT('Ctrl Pts',(43.8362524454727,38.8457365113703,46.7102915860248));
#23873=CARTESIAN_POINT('Ctrl Pts',(43.8798851867402,38.8412952597711,46.7624692363553));
#23874=CARTESIAN_POINT('Ctrl Pts',(43.9235055225129,38.8368552708916,46.814632051735));
#23875=CARTESIAN_POINT('Ctrl Pts',(43.9643777448819,38.8324152820121,46.8691196801779));
#23876=CARTESIAN_POINT('Ctrl Pts',(44.0022551082116,38.8279752931327,46.925606624597));
#23877=CARTESIAN_POINT('Ctrl Pts',(44.0401347947727,38.8235350319238,46.9820970336777));
#23878=CARTESIAN_POINT('Ctrl Pts',(44.0750189848174,38.8190947707148,47.0405865906522));
#23879=CARTESIAN_POINT('Ctrl Pts',(44.106704451789,38.8146545095059,47.1007211382761));
#23880=CARTESIAN_POINT('Ctrl Pts',(44.138423909727,38.8102094849533,47.1609201959602));
#23881=CARTESIAN_POINT('Ctrl Pts',(44.1669375661157,38.8057644604007,47.2227673282688));
#23882=CARTESIAN_POINT('Ctrl Pts',(44.1920888316226,38.8013194358481,47.2858850397355));
#23883=CARTESIAN_POINT('Ctrl Pts',(44.217255310135,38.796871722676,47.349040928609));
#23884=CARTESIAN_POINT('Ctrl Pts',(44.2390551921984,38.7924240095039,47.4134684583036));
#23885=CARTESIAN_POINT('Ctrl Pts',(44.2573815443677,38.7879762963317,47.4787741798967));
#23886=CARTESIAN_POINT('Ctrl Pts',(44.2757396834686,38.7835208686317,47.5441931738144));
#23887=CARTESIAN_POINT('Ctrl Pts',(44.2906121607465,38.7790654409317,47.6104929181125));
#23888=CARTESIAN_POINT('Ctrl Pts',(44.3019431685829,38.7746100132317,47.6772698644672));
#23889=CARTESIAN_POINT('Ctrl Pts',(44.3071723429542,38.7725538670637,47.7080869198887));
#23890=CARTESIAN_POINT('Ctrl Pts',(44.3116479998062,38.7704977208957,47.7390055408118));
#23891=CARTESIAN_POINT('Ctrl Pts',(44.3153683942132,38.7684415747277,47.7699859322796));
#23892=CARTESIAN_POINT('Ctrl Pts',(44.323431212299,38.7639855061777,47.8371264645216));
#23893=CARTESIAN_POINT('Ctrl Pts',(44.3279756041396,38.7595294376277,47.9048257570133));
#23894=CARTESIAN_POINT('Ctrl Pts',(44.3289365802731,38.7550733690777,47.9726828591508));
#23895=CARTESIAN_POINT('Ctrl Pts',(44.3298960998326,38.7506240546953,48.040437108687));
#23896=CARTESIAN_POINT('Ctrl Pts',(44.3272829755928,38.7461747403129,48.108348203499));
#23897=CARTESIAN_POINT('Ctrl Pts',(44.3210838880556,38.7417254259305,48.1760092382609));
#23898=CARTESIAN_POINT('Ctrl Pts',(44.3148921334643,38.7372813746746,48.2435902362903));
#23899=CARTESIAN_POINT('Ctrl Pts',(44.3051228843093,38.7328373234187,48.3109212723607));
#23900=CARTESIAN_POINT('Ctrl Pts',(44.2918148602202,38.7283932721628,48.3775964665486));
#23901=CARTESIAN_POINT('Ctrl Pts',(44.2785152199001,38.7239520205636,48.4442296567984));
#23902=CARTESIAN_POINT('Ctrl Pts',(44.2616813230989,38.7195107689644,48.5102073416065));
#23903=CARTESIAN_POINT('Ctrl Pts',(44.2414033964069,38.7150695173652,48.5751313663862));
#23904=CARTESIAN_POINT('Ctrl Pts',(44.2211312350577,38.7106295284858,48.6400369322145));
#23905=CARTESIAN_POINT('Ctrl Pts',(44.1974171347102,38.7061895396063,48.7038889616217));
#23906=CARTESIAN_POINT('Ctrl Pts',(44.1704013602613,38.7017495507268,48.7663038434492));
#23907=CARTESIAN_POINT('Ctrl Pts',(44.1433839287832,38.6973092895179,48.8287225535319));
#23908=CARTESIAN_POINT('Ctrl Pts',(44.113064619696,38.692869028309,48.8897034889676));
#23909=CARTESIAN_POINT('Ctrl Pts',(44.0796313453446,38.6884287671001,48.9488841344632));
#23910=CARTESIAN_POINT('Ctrl Pts',(44.0461622050455,38.6839837425475,49.0081282667091));
#23911=CARTESIAN_POINT('Ctrl Pts',(44.0095726763772,38.6795387179949,49.0655678242221));
#23912=CARTESIAN_POINT('Ctrl Pts',(43.9700955301258,38.6750936934423,49.1208668891439));
#23913=CARTESIAN_POINT('Ctrl Pts',(43.9305945057102,38.6706459802702,49.1761994022826));
#23914=CARTESIAN_POINT('Ctrl Pts',(43.8882026956471,38.6661982670981,49.2293884601807));
#23915=CARTESIAN_POINT('Ctrl Pts',(43.8431931514392,38.6617505539259,49.2801312762912));
#23916=CARTESIAN_POINT('Ctrl Pts',(43.7981055384867,38.6572951262259,49.330962105467));
#23917=CARTESIAN_POINT('Ctrl Pts',(43.7503914763641,38.6528396985259,49.3793378736793));
#23918=CARTESIAN_POINT('Ctrl Pts',(43.7003601690913,38.6483842708259,49.4249933289461));
#23919=CARTESIAN_POINT('Ctrl Pts',(43.6772710993866,38.6463281246579,49.4460629760634));
#23920=CARTESIAN_POINT('Ctrl Pts',(43.6536889636795,38.6442719784899,49.4665538398702));
#23921=CARTESIAN_POINT('Ctrl Pts',(43.6296462866558,38.6422158323219,49.4864429241022));
#23922=CARTESIAN_POINT('Ctrl Pts',(43.5775411306069,38.6377597637719,49.5295464369329));
#23923=CARTESIAN_POINT('Ctrl Pts',(43.5230626028515,38.6333036952218,49.5699931390812));
#23924=CARTESIAN_POINT('Ctrl Pts',(43.4665127553548,38.6288476266718,49.6075114617214));
#23925=CARTESIAN_POINT('Ctrl Pts',(43.4100486217883,38.6243983122894,49.6449729169599));
#23926=CARTESIAN_POINT('Ctrl Pts',(43.3515198070534,38.619948997907,49.6795145304511));
#23927=CARTESIAN_POINT('Ctrl Pts',(43.2912613242142,38.6154996835246,49.7109049678051));
#23928=CARTESIAN_POINT('Ctrl Pts',(43.2310741215748,38.6110556322688,49.7422582731812));
#23929=CARTESIAN_POINT('Ctrl Pts',(43.1691617498466,38.6066115810129,49.7704675779291));
#23930=CARTESIAN_POINT('Ctrl Pts',(43.1058865124272,38.602167529757,49.7953458687599));
#23931=CARTESIAN_POINT('Ctrl Pts',(43.0426511370463,38.5977262781578,49.8202084868027));
#23932=CARTESIAN_POINT('Ctrl Pts',(42.9780550574625,38.5932850265586,49.8417440730858));
#23933=CARTESIAN_POINT('Ctrl Pts',(42.9124819446754,38.5888437749594,49.859813112461));
#23934=CARTESIAN_POINT('Ctrl Pts',(42.846927475386,38.5844037860799,49.8778770145157));
#23935=CARTESIAN_POINT('Ctrl Pts',(42.7803970000913,38.5799637972005,49.8924761950324));
#23936=CARTESIAN_POINT('Ctrl Pts',(42.7132890286575,38.575523808321,49.9035210903541));
#23937=CARTESIAN_POINT('Ctrl Pts',(42.646176941115,38.5710835471121,49.9145666631213));
#23938=CARTESIAN_POINT('Ctrl Pts',(42.5784877747189,38.5666432859032,49.9220574402996));
#23939=CARTESIAN_POINT('Ctrl Pts',(42.5106280739844,38.5622030246943,49.9259553437571));
#23940=CARTESIAN_POINT('Ctrl Pts',(42.4426955759387,38.5577580001417,49.9298574287375));
#23941=CARTESIAN_POINT('Ctrl Pts',(42.3745926723404,38.553312975589,49.930158919949));
#23942=CARTESIAN_POINT('Ctrl Pts',(42.3067278065509,38.5488679510364,49.9268738554532));
#23943=CARTESIAN_POINT('Ctrl Pts',(42.2388218919885,38.5444202378643,49.9235868039519));
#23944=CARTESIAN_POINT('Ctrl Pts',(42.1711547930101,38.5399725246922,49.9167089295442));
#23945=CARTESIAN_POINT('Ctrl Pts',(42.1041288801391,38.5355248115201,49.9063060712625));
#23946=CARTESIAN_POINT('Ctrl Pts',(42.0369867112835,38.5310693838201,49.8958851692947));
#23947=CARTESIAN_POINT('Ctrl Pts',(41.9704884309552,38.52661395612,49.8819271827729));
#23948=CARTESIAN_POINT('Ctrl Pts',(41.9050244002588,38.52215852842,49.8645486618914));
#23949=CARTESIAN_POINT('Ctrl Pts',(41.8748132454782,38.520102382252,49.8565286060129));
#23950=CARTESIAN_POINT('Ctrl Pts',(41.8448221191952,38.518046236084,49.8477807509429));
#23951=CARTESIAN_POINT('Ctrl Pts',(41.8150879574917,38.515990089916,49.8383200100714));
#23952=CARTESIAN_POINT('Ctrl Pts',(41.8080935585759,38.5155064204361,49.8360945497959));
#23953=CARTESIAN_POINT('Ctrl Pts',(41.8011103478743,38.5150227509561,49.8338286893421));
#23954=CARTESIAN_POINT('Ctrl Pts',(41.7941388317924,38.5145390814761,49.8315225365138));
#23955=CARTESIAN_POINT('Ctrl Pts',(41.794388702738,39.3084106968696,49.8307330830672));
#23956=CARTESIAN_POINT('Ctrl Pts',(41.6242464827134,39.2967219793634,49.7762498623184));
#23957=CARTESIAN_POINT('Ctrl Pts',(40.8927293640396,39.243991282706,49.4267783126541));
#23958=CARTESIAN_POINT('Ctrl Pts',(40.4690312818219,39.1912605860486,48.6236303199305));
#23959=CARTESIAN_POINT('Ctrl Pts',(40.4677075517586,39.1502186068972,47.9997128640878));
#23960=CARTESIAN_POINT('Ctrl Pts',(41.7941386883808,39.4806729614233,49.8315224890738));
#23961=CARTESIAN_POINT('Ctrl Pts',(41.7572007799993,39.4782721882691,49.8193035565988));
#23962=CARTESIAN_POINT('Ctrl Pts',(41.720626997409,39.4758420980136,49.8059653724231));
#23963=CARTESIAN_POINT('Ctrl Pts',(41.6648128553858,39.4720348275255,49.7836732792336));
#23964=CARTESIAN_POINT('Ctrl Pts',(41.6452889524772,39.4706839644207,49.775500403506));
#23965=CARTESIAN_POINT('Ctrl Pts',(41.6159277838943,39.4686214767054,49.7626377800555));
#23966=CARTESIAN_POINT('Ctrl Pts',(41.6059888700241,39.4679178616983,49.7581830112859));
#23967=CARTESIAN_POINT('Ctrl Pts',(41.5880356441581,39.466636703225,49.7499528324736));
#23968=CARTESIAN_POINT('Ctrl Pts',(41.5800085491572,39.4660601549749,49.7462059005683));
#23969=CARTESIAN_POINT('Ctrl Pts',(41.5627688755735,39.4648137120119,49.7380135876415));
#23970=CARTESIAN_POINT('Ctrl Pts',(41.5535653133043,39.4641431961828,49.7335499706784));
#23971=CARTESIAN_POINT('Ctrl Pts',(41.5286901639997,39.4623168446785,49.7212405049893));
#23972=CARTESIAN_POINT('Ctrl Pts',(41.5130896082403,39.4611561186577,49.7132541051122));
#23973=CARTESIAN_POINT('Ctrl Pts',(41.4306461857406,39.4549382696789,49.6696210011786));
#23974=CARTESIAN_POINT('Ctrl Pts',(41.3658458138884,39.4497507967578,49.6302771643636));
#23975=CARTESIAN_POINT('Ctrl Pts',(41.1963341554496,39.4353488207674,49.5131775915762));
#23976=CARTESIAN_POINT('Ctrl Pts',(41.0969173575093,39.4259401962981,49.4284568581312));
#23977=CARTESIAN_POINT('Ctrl Pts',(40.9762616586075,39.413595948292,49.3024830002245));
#23978=CARTESIAN_POINT('Ctrl Pts',(40.9468170149334,39.4104991199501,49.2695481691971));
#23979=CARTESIAN_POINT('Ctrl Pts',(40.9073374957543,39.4062560106887,49.2222137290788));
#23980=CARTESIAN_POINT('Ctrl Pts',(40.896330196568,39.4050624252255,49.2086459038197));
#23981=CARTESIAN_POINT('Ctrl Pts',(40.8774008566907,39.4029936908133,49.1846542640887));
#23982=CARTESIAN_POINT('Ctrl Pts',(40.8693979126598,39.4021138133726,49.1742960231302));
#23983=CARTESIAN_POINT('Ctrl Pts',(40.857680046825,39.400818581186,49.1588062068697));
#23984=CARTESIAN_POINT('Ctrl Pts',(40.8538841673837,39.4003978982557,49.153736754207));
#23985=CARTESIAN_POINT('Ctrl Pts',(40.8474329986074,39.399681165666,49.1450321069591));
#23986=CARTESIAN_POINT('Ctrl Pts',(40.8447653943652,39.3993842695105,49.141406212859));
#23987=CARTESIAN_POINT('Ctrl Pts',(40.838735123276,39.3987119483314,49.1331492812333));
#23988=CARTESIAN_POINT('Ctrl Pts',(40.8353803549895,39.398337069403,49.1285125951464));
#23989=CARTESIAN_POINT('Ctrl Pts',(40.8262918142114,39.3973189247411,49.1158327243912));
#23990=CARTESIAN_POINT('Ctrl Pts',(40.8205990075511,39.3966783895212,49.1077601897435));
#23991=CARTESIAN_POINT('Ctrl Pts',(40.7921010249354,39.3934556013828,49.0666830753785));
#23992=CARTESIAN_POINT('Ctrl Pts',(40.7702655459503,39.3909325345241,49.0330140525441));
#23993=CARTESIAN_POINT('Ctrl Pts',(40.7373861659563,39.3870033112992,48.9786750416741));
#23994=CARTESIAN_POINT('Ctrl Pts',(40.7256425512353,39.3855705623336,48.9584449915192));
#23995=CARTESIAN_POINT('Ctrl Pts',(40.6632895401385,39.3777703119716,48.8463877054721));
#23996=CARTESIAN_POINT('Ctrl Pts',(40.6198618690059,39.3715981013804,48.7507631724698));
#23997=CARTESIAN_POINT('Ctrl Pts',(40.5525759702005,39.359654748008,48.5634196189072));
#23998=CARTESIAN_POINT('Ctrl Pts',(40.5272734114907,39.353922997071,48.4725560589942));
#23999=CARTESIAN_POINT('Ctrl Pts',(40.5039970048509,39.346464967583,48.3567729292254));
#24000=CARTESIAN_POINT('Ctrl Pts',(40.4997208135259,39.3449422661323,48.3332464754407));
#24001=CARTESIAN_POINT('Ctrl Pts',(40.4940485475633,39.3426712186698,48.2983659743585));
#24002=CARTESIAN_POINT('Ctrl Pts',(40.4923142882815,39.3419335863272,48.2870686498577));
#24003=CARTESIAN_POINT('Ctrl Pts',(40.4894072254195,39.3406153820887,48.2669403625762));
#24004=CARTESIAN_POINT('Ctrl Pts',(40.488194998409,39.3400360767431,48.2581153596175));
#24005=CARTESIAN_POINT('Ctrl Pts',(40.4857672255838,39.3388101134469,48.2394849921932));
#24006=CARTESIAN_POINT('Ctrl Pts',(40.4845658063796,39.338163026284,48.2296780787845));
#24007=CARTESIAN_POINT('Ctrl Pts',(40.4815718759133,39.3364361325577,48.2035797335713));
#24008=CARTESIAN_POINT('Ctrl Pts',(40.4799115898022,39.3353521956303,48.1872742478333));
#24009=CARTESIAN_POINT('Ctrl Pts',(40.4733613752745,39.3304338430108,48.11364743718));
#24010=CARTESIAN_POINT('Ctrl Pts',(40.4708297108102,39.3265266190048,48.056151172904));
#24011=CARTESIAN_POINT('Ctrl Pts',(40.4709432424599,39.315454698046,47.895994494694));
#24012=CARTESIAN_POINT('Ctrl Pts',(40.4792070365146,39.308147369249,47.7935357747464));
#24013=CARTESIAN_POINT('Ctrl Pts',(40.5122448140058,39.2933532485622,47.5891031991035));
#24014=CARTESIAN_POINT('Ctrl Pts',(40.5372622012714,39.2858911459844,47.4874885874659));
#24015=CARTESIAN_POINT('Ctrl Pts',(40.5756031817763,39.277657876097,47.3727924232959));
#24016=CARTESIAN_POINT('Ctrl Pts',(40.5810173459183,39.2765472774639,47.3572595834893));
#24017=CARTESIAN_POINT('Ctrl Pts',(40.5888309240076,39.2750160935208,47.3357329176423));
#24018=CARTESIAN_POINT('Ctrl Pts',(40.5910625614552,39.2745864041359,47.3296795356606));
#24019=CARTESIAN_POINT('Ctrl Pts',(40.5949634532207,39.2738484320678,47.3192596146288));
#24020=CARTESIAN_POINT('Ctrl Pts',(40.5966182707184,39.2735393141178,47.3148877849963));
#24021=CARTESIAN_POINT('Ctrl Pts',(40.6001404397498,39.2728896713182,47.3056838215192));
#24022=CARTESIAN_POINT('Ctrl Pts',(40.6020113929379,39.2725493757342,47.3008531182257));
#24023=CARTESIAN_POINT('Ctrl Pts',(40.6066962963271,39.2717088804307,47.2889001287027));
#24024=CARTESIAN_POINT('Ctrl Pts',(40.6095332778297,39.271210044207,47.2817868546033));
#24025=CARTESIAN_POINT('Ctrl Pts',(40.6203511862378,39.2693447142586,47.2551251919791));
#24026=CARTESIAN_POINT('Ctrl Pts',(40.6286108505886,39.2679939012571,47.2356905404024));
#24027=CARTESIAN_POINT('Ctrl Pts',(40.6957596493483,39.2575348292537,47.0846315185017));
#24028=CARTESIAN_POINT('Ctrl Pts',(40.7689270280666,39.2491101547511,46.9598332643251));
#24029=CARTESIAN_POINT('Ctrl Pts',(40.9212756821805,39.2338835330702,46.7562014504121));
#24030=CARTESIAN_POINT('Ctrl Pts',(40.994634592764,39.227201349917,46.6738764092354));
#24031=CARTESIAN_POINT('Ctrl Pts',(41.0869948728352,39.2191273242738,46.5865464982635));
#24032=CARTESIAN_POINT('Ctrl Pts',(41.0995382544105,39.2180376452817,46.5749973740234));
#24033=CARTESIAN_POINT('Ctrl Pts',(41.1204299091927,39.2162327954686,46.5562672888958));
#24034=CARTESIAN_POINT('Ctrl Pts',(41.1286896755948,39.2155217491854,46.5489886943392));
#24035=CARTESIAN_POINT('Ctrl Pts',(41.1437133203832,39.2142326858313,46.5359764513183));
#24036=CARTESIAN_POINT('Ctrl Pts',(41.1504553349946,39.2136557232901,46.5302179419323));
#24037=CARTESIAN_POINT('Ctrl Pts',(41.1649937129591,39.2124146622441,46.5179727110113));
#24038=CARTESIAN_POINT('Ctrl Pts',(41.1728019845625,39.2117499891727,46.5115006084769));
#24039=CARTESIAN_POINT('Ctrl Pts',(41.1942935696943,39.2099253990083,46.4939707634743));
#24040=CARTESIAN_POINT('Ctrl Pts',(41.2080774072111,39.208760490584,46.4830383804725));
#24041=CARTESIAN_POINT('Ctrl Pts',(41.2890526385286,39.2019456662222,46.4205994790996));
#24042=CARTESIAN_POINT('Ctrl Pts',(41.3594176076335,39.1961304518185,46.3733793444299));
#24043=CARTESIAN_POINT('Ctrl Pts',(41.5319026431404,39.1821374384727,46.2734107427961));
#24044=CARTESIAN_POINT('Ctrl Pts',(41.6360890500218,39.1738734558777,46.2248547046026));
#24045=CARTESIAN_POINT('Ctrl Pts',(41.7775097994723,39.1632037352662,46.1737138321046));
#24046=CARTESIAN_POINT('Ctrl Pts',(41.8113895807534,39.1606883272452,46.162514431062));
#24047=CARTESIAN_POINT('Ctrl Pts',(41.8822463478663,39.15553467628,46.1412529397935));
#24048=CARTESIAN_POINT('Ctrl Pts',(41.9192535767295,39.1529020568492,46.131339296387));
#24049=CARTESIAN_POINT('Ctrl Pts',(41.9661011507873,39.14966293581,46.1202736961043));
#24050=CARTESIAN_POINT('Ctrl Pts',(41.9756854348441,39.1490051351641,46.1180870506836));
#24051=CARTESIAN_POINT('Ctrl Pts',(41.9908092716992,39.1479752467331,46.1147579767026));
#24052=CARTESIAN_POINT('Ctrl Pts',(41.9963376890241,39.147600478758,46.1135665187244));
#24053=CARTESIAN_POINT('Ctrl Pts',(42.0067818552093,39.1468957856102,46.1113636577592));
#24054=CARTESIAN_POINT('Ctrl Pts',(42.011696271132,39.1465655909001,46.1103471331056));
#24055=CARTESIAN_POINT('Ctrl Pts',(42.0232183998512,39.1457946110378,46.1080106808329));
#24056=CARTESIAN_POINT('Ctrl Pts',(42.029829128553,39.1453547038684,46.1067061803977));
#24057=CARTESIAN_POINT('Ctrl Pts',(42.0514382506145,39.1439242805252,46.1025595432674));
#24058=CARTESIAN_POINT('Ctrl Pts',(42.0664640089414,39.1429414883017,46.0998607003952));
#24059=CARTESIAN_POINT('Ctrl Pts',(42.149402338378,39.1375739015709,46.0859779573723));
#24060=CARTESIAN_POINT('Ctrl Pts',(42.2178510210939,39.1333537973385,46.0782551227953));
#24061=CARTESIAN_POINT('Ctrl Pts',(42.4066888467311,39.1219332133013,46.067132769227));
#24062=CARTESIAN_POINT('Ctrl Pts',(42.5272025950652,39.1148755555931,46.0713111293193));
#24063=CARTESIAN_POINT('Ctrl Pts',(42.721195806884,39.1030056823874,46.0963084994355));
#24064=CARTESIAN_POINT('Ctrl Pts',(42.7952133723485,39.0983569312193,46.1102877210163));
#24065=CARTESIAN_POINT('Ctrl Pts',(42.8851943505182,39.0924557974302,46.1328001780605));
#24066=CARTESIAN_POINT('Ctrl Pts',(42.9021099918791,39.0913355171407,46.1372777296383));
#24067=CARTESIAN_POINT('Ctrl Pts',(42.9288076673937,39.0895489658275,46.1447346528061));
#24068=CARTESIAN_POINT('Ctrl Pts',(42.938631210012,39.0888876116105,46.1475628295367));
#24069=CARTESIAN_POINT('Ctrl Pts',(42.9569251776393,39.0876483347286,46.1529874428265));
#24070=CARTESIAN_POINT('Ctrl Pts',(42.9654011277285,39.0870710625808,46.1555644223251));
#24071=CARTESIAN_POINT('Ctrl Pts',(42.9842652903852,39.0857792280311,46.1614420234705));
#24072=CARTESIAN_POINT('Ctrl Pts',(42.994643818116,39.0850637001294,46.1647724708143));
#24073=CARTESIAN_POINT('Ctrl Pts',(43.0251290005625,39.082947493201,46.1748408404315));
#24074=CARTESIAN_POINT('Ctrl Pts',(43.0451528755385,39.0815388274328,46.1818223598861));
#24075=CARTESIAN_POINT('Ctrl Pts',(43.0904926017613,39.0783053079238,46.1984737693127));
#24076=CARTESIAN_POINT('Ctrl Pts',(43.1157274847944,39.0764739283183,46.2083496892094));
#24077=CARTESIAN_POINT('Ctrl Pts',(43.200170055643,39.0702366648794,46.2434657756511));
#24078=CARTESIAN_POINT('Ctrl Pts',(43.2583157339956,39.0657562925065,46.2711340994453));
#24079=CARTESIAN_POINT('Ctrl Pts',(43.4186632612192,39.0529023988584,46.3575195785736));
#24080=CARTESIAN_POINT('Ctrl Pts',(43.5170217130359,39.0443979853303,46.4227625782621));
#24081=CARTESIAN_POINT('Ctrl Pts',(43.6166302380897,39.0353902583729,46.5028513719334));
#24082=CARTESIAN_POINT('Ctrl Pts',(43.6243976426928,39.0346851569305,46.5091970054033));
#24083=CARTESIAN_POINT('Ctrl Pts',(43.6680935891876,39.0307047187082,46.5454665780805));
#24084=CARTESIAN_POINT('Ctrl Pts',(43.7029776770778,39.0274731622907,46.5766311789618));
#24085=CARTESIAN_POINT('Ctrl Pts',(43.7441440353361,39.0236265394354,46.6161914774334));
#24086=CARTESIAN_POINT('Ctrl Pts',(43.7515331385909,39.0229347412754,46.6234073217633));
#24087=CARTESIAN_POINT('Ctrl Pts',(43.7629991483236,39.0218596255801,46.6347857987943));
#24088=CARTESIAN_POINT('Ctrl Pts',(43.767115621351,39.0214733103927,46.6389080216273));
#24089=CARTESIAN_POINT('Ctrl Pts',(43.7747211942386,39.0207590478848,46.6465935333712));
#24090=CARTESIAN_POINT('Ctrl Pts',(43.778215138132,39.0204307321622,46.6501516901234));
#24091=CARTESIAN_POINT('Ctrl Pts',(43.7862019958432,39.019679742385,46.658348672111));
#24092=CARTESIAN_POINT('Ctrl Pts',(43.7906854469215,39.0192578009104,46.6629965409169));
#24093=CARTESIAN_POINT('Ctrl Pts',(43.8046333246866,39.0179436475635,46.6776019874962));
#24094=CARTESIAN_POINT('Ctrl Pts',(43.814015029175,39.0170575224528,46.6876384630627));
#24095=CARTESIAN_POINT('Ctrl Pts',(43.8358425391412,39.0149881731168,46.7114952061302));
#24096=CARTESIAN_POINT('Ctrl Pts',(43.8481974861094,39.0138108110424,46.7253971217567));
#24097=CARTESIAN_POINT('Ctrl Pts',(43.8920818162645,39.0095972988479,46.7762382662281));
#24098=CARTESIAN_POINT('Ctrl Pts',(43.9224164973262,39.0066239413646,46.8141882136135));
#24099=CARTESIAN_POINT('Ctrl Pts',(44.0486865858999,38.99377438918,46.9850018057142));
#24100=CARTESIAN_POINT('Ctrl Pts',(44.1288993006195,38.9842572057103,47.1286235283099));
#24101=CARTESIAN_POINT('Ctrl Pts',(44.2055763545409,38.9714957029341,47.3194250648631));
#24102=CARTESIAN_POINT('Ctrl Pts',(44.2198913317623,38.9688682491835,47.3586862269963));
#24103=CARTESIAN_POINT('Ctrl Pts',(44.2374793407569,38.9652644095579,47.4122704776094));
#24104=CARTESIAN_POINT('Ctrl Pts',(44.24188076888,38.9643251348417,47.4262129896059));
#24105=CARTESIAN_POINT('Ctrl Pts',(44.2488787914039,38.9627672067203,47.449291412655));
#24106=CARTESIAN_POINT('Ctrl Pts',(44.2515672060382,38.962151578104,47.4583990310013));
#24107=CARTESIAN_POINT('Ctrl Pts',(44.2566839328357,38.9609454518536,47.4762165666444));
#24108=CARTESIAN_POINT('Ctrl Pts',(44.2591184700721,38.9603551754785,47.4849244511377));
#24109=CARTESIAN_POINT('Ctrl Pts',(44.2647290631648,38.9589549320483,47.5055506025358));
#24110=CARTESIAN_POINT('Ctrl Pts',(44.2678521781921,38.9581432701149,47.517482731882));
#24111=CARTESIAN_POINT('Ctrl Pts',(44.2779331130477,38.9554109810469,47.5575630072758));
#24112=CARTESIAN_POINT('Ctrl Pts',(44.2843704287005,38.9534737696925,47.5858367456617));
#24113=CARTESIAN_POINT('Ctrl Pts',(44.309146871886,38.9451098020085,47.7072388296506));
#24114=CARTESIAN_POINT('Ctrl Pts',(44.3212345010496,38.9384922981646,47.8014947948279));
#24115=CARTESIAN_POINT('Ctrl Pts',(44.3321439783103,38.9241022856435,48.0040437749043));
#24116=CARTESIAN_POINT('Ctrl Pts',(44.3288913655582,38.9163190100983,48.1121376370611));
#24117=CARTESIAN_POINT('Ctrl Pts',(44.3108184602381,38.9051505583447,48.2700231215503));
#24118=CARTESIAN_POINT('Ctrl Pts',(44.3030181609168,38.9016194268671,48.3204099815791));
#24119=CARTESIAN_POINT('Ctrl Pts',(44.2912006234036,38.8974710449596,48.3808077071793));
#24120=CARTESIAN_POINT('Ctrl Pts',(44.2890854288227,38.8967626597076,48.3911656463099));
#24121=CARTESIAN_POINT('Ctrl Pts',(44.2856612322629,38.895667405426,48.4072577252834));
#24122=CARTESIAN_POINT('Ctrl Pts',(44.2844110135683,38.8952773609034,48.4130039611114));
#24123=CARTESIAN_POINT('Ctrl Pts',(44.2820533998654,38.8945597493575,48.423606378354));
#24124=CARTESIAN_POINT('Ctrl Pts',(44.2809534768241,38.8942317828576,48.428463980641));
#24125=CARTESIAN_POINT('Ctrl Pts',(44.2784013938672,38.8934860894097,48.4395355267987));
#24126=CARTESIAN_POINT('Ctrl Pts',(44.2769372068717,38.8930690552023,48.4457465649162));
#24127=CARTESIAN_POINT('Ctrl Pts',(44.2723175624508,38.8917855812395,48.4649165388688));
#24128=CARTESIAN_POINT('Ctrl Pts',(44.2690584350834,38.8909248294404,48.477850429498));
#24129=CARTESIAN_POINT('Ctrl Pts',(44.261112014321,38.8889243433001,48.5080600359224));
#24130=CARTESIAN_POINT('Ctrl Pts',(44.256317841084,38.8877899530337,48.5253066269653));
#24131=CARTESIAN_POINT('Ctrl Pts',(44.2384012239809,38.8837875737641,48.5864489084932));
#24132=CARTESIAN_POINT('Ctrl Pts',(44.2239553937596,38.8809758064384,48.6299433905435));
#24133=CARTESIAN_POINT('Ctrl Pts',(44.1601953046972,38.8698940029453,48.801260277132));
#24134=CARTESIAN_POINT('Ctrl Pts',(44.0988807443618,38.8618992627093,48.9241815550249));
#24135=CARTESIAN_POINT('Ctrl Pts',(43.9886465595339,38.8494320888307,49.0964995169153));
#24136=CARTESIAN_POINT('Ctrl Pts',(43.9492686837471,38.8452421134808,49.1514660817397));
#24137=CARTESIAN_POINT('Ctrl Pts',(43.8963544494236,38.8398456097511,49.2176870545653));
#24138=CARTESIAN_POINT('Ctrl Pts',(43.8854384194936,38.8387437517679,49.2309797204837));
#24139=CARTESIAN_POINT('Ctrl Pts',(43.8678606077272,38.8369862460035,49.2518102621233));
#24140=CARTESIAN_POINT('Ctrl Pts',(43.8613149330871,38.8363353481609,49.2594452572637));
#24141=CARTESIAN_POINT('Ctrl Pts',(43.8494628323335,38.8351629311323,49.2730529761167));
#24142=CARTESIAN_POINT('Ctrl Pts',(43.8441783986887,38.8346423350809,49.2790446168286));
#24143=CARTESIAN_POINT('Ctrl Pts',(43.8317206122763,38.8334199275515,49.2929939774011));
#24144=CARTESIAN_POINT('Ctrl Pts',(43.824517941207,38.8327168884227,49.3009250418483));
#24145=CARTESIAN_POINT('Ctrl Pts',(43.8034818287595,38.8306739669742,49.3237043244996));
#24146=CARTESIAN_POINT('Ctrl Pts',(43.7894800324291,38.8293269126964,49.3383943993127));
#24147=CARTESIAN_POINT('Ctrl Pts',(43.6823586979531,38.8191119260573,49.4472885374793));
#24148=CARTESIAN_POINT('Ctrl Pts',(43.5800071337812,38.809820019025,49.5318807818622));
#24149=CARTESIAN_POINT('Ctrl Pts',(43.3644824381448,38.7913458446355,49.6755120273465));
#24150=CARTESIAN_POINT('Ctrl Pts',(43.2524819043023,38.7822289632951,49.7351791451136));
#24151=CARTESIAN_POINT('Ctrl Pts',(43.1210208775772,38.7725601031495,49.7893894383931));
#24152=CARTESIAN_POINT('Ctrl Pts',(43.1065342315239,38.7715082902099,49.7951587912484));
#24153=CARTESIAN_POINT('Ctrl Pts',(43.0860916350656,38.7700447144953,49.8030143094472));
#24154=CARTESIAN_POINT('Ctrl Pts',(43.0801934360561,38.7696248332792,49.8052476905077));
#24155=CARTESIAN_POINT('Ctrl Pts',(43.0695068487902,38.7688685392684,49.8092344062377));
#24156=CARTESIAN_POINT('Ctrl Pts',(43.0647222675997,38.7685315432248,49.8109977543844));
#24157=CARTESIAN_POINT('Ctrl Pts',(43.0549157284213,38.7678442026703,49.8145678350829));
#24158=CARTESIAN_POINT('Ctrl Pts',(43.0498931782063,38.7674939668654,49.8163727310496));
#24159=CARTESIAN_POINT('Ctrl Pts',(43.036957588152,38.7665963845983,49.8209607209855));
#24160=CARTESIAN_POINT('Ctrl Pts',(43.0290336689952,38.7660508238317,49.8237131260307));
#24161=CARTESIAN_POINT('Ctrl Pts',(42.9955560913265,38.7637628443871,49.8350975402084));
#24162=CARTESIAN_POINT('Ctrl Pts',(42.9698394374398,38.762046738982,49.843245299016));
#24163=CARTESIAN_POINT('Ctrl Pts',(42.8990915829143,38.7574166132156,49.8640378480051));
#24164=CARTESIAN_POINT('Ctrl Pts',(42.8537564966018,38.7545488542413,49.8755892804064));
#24165=CARTESIAN_POINT('Ctrl Pts',(42.6689347399941,38.7430938071423,49.9155871716998));
#24166=CARTESIAN_POINT('Ctrl Pts',(42.5269234233933,38.7347952420668,49.9302052107738));
#24167=CARTESIAN_POINT('Ctrl Pts',(42.3229421139634,38.7223179472847,49.9285760942051));
#24168=CARTESIAN_POINT('Ctrl Pts',(42.2613555020867,38.7184835111987,49.9251286201491));
#24169=CARTESIAN_POINT('Ctrl Pts',(42.1833784088071,38.7134892501052,49.9170024507489));
#24170=CARTESIAN_POINT('Ctrl Pts',(42.1667367471954,38.7124153726899,49.9150487033754));
#24171=CARTESIAN_POINT('Ctrl Pts',(42.1402468676717,38.7106922619895,49.9115883632989));
#24172=CARTESIAN_POINT('Ctrl Pts',(42.1303809732373,38.7100474597499,49.9102218024807));
#24173=CARTESIAN_POINT('Ctrl Pts',(42.1126079135513,38.7088801838101,49.9076195610772));
#24174=CARTESIAN_POINT('Ctrl Pts',(42.1046969653766,38.7083585807557,49.9064109514066));
#24175=CARTESIAN_POINT('Ctrl Pts',(42.0860784172047,38.7071260625944,49.9034477996196));
#24176=CARTESIAN_POINT('Ctrl Pts',(42.0753777381585,38.7064138534964,49.901652088303));
#24177=CARTESIAN_POINT('Ctrl Pts',(42.0440507928679,38.7043172451695,49.8961229104975));
#24178=CARTESIAN_POINT('Ctrl Pts',(42.0234701061044,38.7029250812669,49.8921435224594));
#24179=CARTESIAN_POINT('Ctrl Pts',(41.932298749733,38.696689819279,49.8729687183958));
#24180=CARTESIAN_POINT('Ctrl Pts',(41.8625838747428,38.6917365813973,49.8541639349618));
#24181=CARTESIAN_POINT('Ctrl Pts',(41.7941383335288,38.6866921868075,49.8315223716899));
#24182=CARTESIAN_POINT('Origin',(42.4,48.4493818343519,48.));
#24183=CARTESIAN_POINT('',(41.7941388718785,37.7199737694749,49.8315225497742));
#24184=CARTESIAN_POINT('',(41.7941388317907,37.8901046061668,49.8315225365133));
#24185=CARTESIAN_POINT('',(41.7941388317924,48.4493818343519,49.8315225365138));
#24186=CARTESIAN_POINT('',(40.4708708049845,38.3564681656839,48.001762339035));
#24187=CARTESIAN_POINT('Ctrl Pts',(41.7941388718785,37.7199737694749,49.8315225497742));
#24188=CARTESIAN_POINT('Ctrl Pts',(41.8877523316507,37.7269321000002,49.8624895484344));
#24189=CARTESIAN_POINT('Ctrl Pts',(41.9836178395209,37.7340242380728,49.8862387901888));
#24190=CARTESIAN_POINT('Ctrl Pts',(42.1540699352791,37.746299514361,49.9148281177976));
#24191=CARTESIAN_POINT('Ctrl Pts',(42.2279046256527,37.7515068157566,49.9228712970221));
#24192=CARTESIAN_POINT('Ctrl Pts',(42.3124126332644,37.7572194796111,49.9271686893187));
#24193=CARTESIAN_POINT('Ctrl Pts',(42.3228029724612,37.7579175714046,49.9276128590917));
#24194=CARTESIAN_POINT('Ctrl Pts',(42.339595075755,37.7590383149552,49.9281946973126));
#24195=CARTESIAN_POINT('Ctrl Pts',(42.3459946577612,37.7594636880468,49.9283845497075));
#24196=CARTESIAN_POINT('Ctrl Pts',(42.3573771748442,37.7602170194124,49.928665519751));
#24197=CARTESIAN_POINT('Ctrl Pts',(42.3623596385389,37.7605456589677,49.9287691923685));
#24198=CARTESIAN_POINT('Ctrl Pts',(42.3732100202436,37.7612588948147,49.9289528998913));
#24199=CARTESIAN_POINT('Ctrl Pts',(42.3790779275809,37.7616430737147,49.929025469547));
#24200=CARTESIAN_POINT('Ctrl Pts',(42.3957552273418,37.7627308111796,49.9291556136361));
#24201=CARTESIAN_POINT('Ctrl Pts',(42.4065651051185,37.7634309115056,49.9291491161159));
#24202=CARTESIAN_POINT('Ctrl Pts',(42.480999192376,37.7682210699932,49.9284787002925));
#24203=CARTESIAN_POINT('Ctrl Pts',(42.5445638419713,37.7721584675607,49.9247581881385));
#24204=CARTESIAN_POINT('Ctrl Pts',(42.7360603000483,37.7838638319947,49.904006532693));
#24205=CARTESIAN_POINT('Ctrl Pts',(42.8625708468446,37.7914036571621,49.8772873612571));
#24206=CARTESIAN_POINT('Ctrl Pts',(43.0117068161834,37.8008862719049,49.8297856211282));
#24207=CARTESIAN_POINT('Ctrl Pts',(43.0377590121689,37.8025646746312,49.8208690260277));
#24208=CARTESIAN_POINT('Ctrl Pts',(43.1146177880199,37.807596104434,49.7927115990767));
#24209=CARTESIAN_POINT('Ctrl Pts',(43.1648086639362,37.8109878777721,49.7718804527781));
#24210=CARTESIAN_POINT('Ctrl Pts',(43.2286321984564,37.8154766773523,49.7421739071562));
#24211=CARTESIAN_POINT('Ctrl Pts',(43.243127981925,37.8165082251169,49.7352050091779));
#24212=CARTESIAN_POINT('Ctrl Pts',(43.266326865696,37.818179427095,49.7236927392929));
#24213=CARTESIAN_POINT('Ctrl Pts',(43.2750855789402,37.8188151159209,49.7192626679247));
#24214=CARTESIAN_POINT('Ctrl Pts',(43.2917446232535,37.820033445157,49.7106764064012));
#24215=CARTESIAN_POINT('Ctrl Pts',(43.2996506794741,37.820615663391,49.7065318312051));
#24216=CARTESIAN_POINT('Ctrl Pts',(43.3177309421539,37.8219565460912,49.6968930937317));
#24217=CARTESIAN_POINT('Ctrl Pts',(43.3278850035971,37.8227165084903,49.6913620735717));
#24218=CARTESIAN_POINT('Ctrl Pts',(43.3594923298819,37.8251041828696,49.6737749567397));
#24219=CARTESIAN_POINT('Ctrl Pts',(43.380764302695,37.8267432748955,49.6613998386583));
#24220=CARTESIAN_POINT('Ctrl Pts',(43.4871957334718,37.8351124619477,49.5967262655778));
#24221=CARTESIAN_POINT('Ctrl Pts',(43.5684239762704,37.8420659007577,49.5382812788406));
#24222=CARTESIAN_POINT('Ctrl Pts',(43.6652471040792,37.8510528295861,49.4565068112768));
#24223=CARTESIAN_POINT('Ctrl Pts',(43.685379886816,37.8529629506852,49.438770595866));
#24224=CARTESIAN_POINT('Ctrl Pts',(43.7973844590631,37.8638137483778,49.3358710652742));
#24225=CARTESIAN_POINT('Ctrl Pts',(43.8811659973364,37.8728313751821,49.2423313698739));
#24226=CARTESIAN_POINT('Ctrl Pts',(43.9645473189848,37.8824151078907,49.128706812523));
#24227=CARTESIAN_POINT('Ctrl Pts',(43.9736509592223,37.8834706873842,49.1159794258304));
#24228=CARTESIAN_POINT('Ctrl Pts',(43.9862115013965,37.8849386802412,49.0979597157393));
#24229=CARTESIAN_POINT('Ctrl Pts',(43.9897985049483,37.8853592729924,49.092759434178));
#24230=CARTESIAN_POINT('Ctrl Pts',(43.9962366873083,37.8861165328041,49.0833268362994));
#24231=CARTESIAN_POINT('Ctrl Pts',(43.9990967362183,37.8864537870104,49.079100656333));
#24232=CARTESIAN_POINT('Ctrl Pts',(44.004912696669,37.8871412792135,49.070432743143));
#24233=CARTESIAN_POINT('Ctrl Pts',(44.0078670040356,37.8874914109149,49.0659900189884));
#24234=CARTESIAN_POINT('Ctrl Pts',(44.0154117599794,37.8883880923588,49.0545413956931));
#24235=CARTESIAN_POINT('Ctrl Pts',(44.0199751409865,37.8889328642698,49.0475176649484));
#24236=CARTESIAN_POINT('Ctrl Pts',(44.0389729966439,37.8912120978329,49.0178560234238));
#24237=CARTESIAN_POINT('Ctrl Pts',(44.052980603543,37.8929205001628,48.9949465648968));
#24238=CARTESIAN_POINT('Ctrl Pts',(44.0899013469995,37.8975233984548,48.9316292528973));
#24239=CARTESIAN_POINT('Ctrl Pts',(44.11184159907,37.900372300004,48.8906730922922));
#24240=CARTESIAN_POINT('Ctrl Pts',(44.1940642782995,37.9116931909724,48.7229000486566));
#24241=CARTESIAN_POINT('Ctrl Pts',(44.2418999831702,37.9198815061603,48.590472046673));
#24242=CARTESIAN_POINT('Ctrl Pts',(44.2899369788385,37.9323497506817,48.3920973784401));
#24243=CARTESIAN_POINT('Ctrl Pts',(44.3018539193616,37.9363080522644,48.3294731137162));
#24244=CARTESIAN_POINT('Ctrl Pts',(44.3129896610024,37.9414441089459,48.2495998958885));
#24245=CARTESIAN_POINT('Ctrl Pts',(44.3151077191802,37.9425296492652,48.2327916355552));
#24246=CARTESIAN_POINT('Ctrl Pts',(44.3181238003864,37.9442672168932,48.2060186620459));
#24247=CARTESIAN_POINT('Ctrl Pts',(44.3191661784829,37.9449146822668,48.1960708438832));
#24248=CARTESIAN_POINT('Ctrl Pts',(44.3209028636329,37.9460843610345,48.1781536751628));
#24249=CARTESIAN_POINT('Ctrl Pts',(44.3216250556844,37.9466056818446,48.1701872075138));
#24250=CARTESIAN_POINT('Ctrl Pts',(44.3232055213664,37.9478343292878,48.15145838507));
#24251=CARTESIAN_POINT('Ctrl Pts',(44.3240230262112,37.9485429229655,48.1406929506482));
#24252=CARTESIAN_POINT('Ctrl Pts',(44.3261433628525,37.9506176764822,48.1092807426832));
#24253=CARTESIAN_POINT('Ctrl Pts',(44.3272044579299,37.9519913545403,48.0886197235859));
#24254=CARTESIAN_POINT('Ctrl Pts',(44.3288578067952,37.9551319912494,48.0417070029651));
#24255=CARTESIAN_POINT('Ctrl Pts',(44.3292467477289,37.9569049520084,48.015452700315));
#24256=CARTESIAN_POINT('Ctrl Pts',(44.328756371073,37.9628721387924,47.9278640447596));
#24257=CARTESIAN_POINT('Ctrl Pts',(44.3254879901965,37.9671339013594,47.8665852240479));
#24258=CARTESIAN_POINT('Ctrl Pts',(44.3105578752507,37.977568794074,47.719202543636));
#24259=CARTESIAN_POINT('Ctrl Pts',(44.2959890040791,37.9837918243251,47.6335261818599));
#24260=CARTESIAN_POINT('Ctrl Pts',(44.2545927368263,37.996421702991,47.4613113027187));
#24261=CARTESIAN_POINT('Ctrl Pts',(44.2273403937788,38.0028100714955,47.3750754619958));
#24262=CARTESIAN_POINT('Ctrl Pts',(44.1902624491323,38.0096237644902,47.2812411071322));
#24263=CARTESIAN_POINT('Ctrl Pts',(44.1863026300751,38.0103325340234,47.2714556232835));
#24264=CARTESIAN_POINT('Ctrl Pts',(44.1797946231788,38.0114669908775,47.2557451772789));
#24265=CARTESIAN_POINT('Ctrl Pts',(44.1772967636231,38.0118955047755,47.2497997874969));
#24266=CARTESIAN_POINT('Ctrl Pts',(44.1728142871328,38.0126522403754,47.2392786754813));
#24267=CARTESIAN_POINT('Ctrl Pts',(44.1708416881168,38.0129811678504,47.2346980021741));
#24268=CARTESIAN_POINT('Ctrl Pts',(44.166522637338,38.0136925477032,47.2247746287503));
#24269=CARTESIAN_POINT('Ctrl Pts',(44.16416970015,38.0140746013856,47.2194348997332));
#24270=CARTESIAN_POINT('Ctrl Pts',(44.1574522305179,38.0151502026677,47.2043758899221));
#24271=CARTESIAN_POINT('Ctrl Pts',(44.1530312781341,38.0158404127178,47.1946817911306));
#24272=CARTESIAN_POINT('Ctrl Pts',(44.1233344374674,38.0203654980837,47.1309672089294));
#24273=CARTESIAN_POINT('Ctrl Pts',(44.0956426382716,38.0240664333629,47.0781013312181));
#24274=CARTESIAN_POINT('Ctrl Pts',(44.0210057536534,38.0330790372086,46.9503935876734));
#24275=CARTESIAN_POINT('Ctrl Pts',(43.9712895797699,38.0383040940369,46.8773318789603));
#24276=CARTESIAN_POINT('Ctrl Pts',(43.8415901525552,38.0508420181915,46.7123075731327));
#24277=CARTESIAN_POINT('Ctrl Pts',(43.7575744225633,38.0581829111807,46.6240203666063));
#24278=CARTESIAN_POINT('Ctrl Pts',(43.6529491420653,38.0669897024222,46.5330468034921));
#24279=CARTESIAN_POINT('Ctrl Pts',(43.6399359993038,38.0680793221632,46.5220311501145));
#24280=CARTESIAN_POINT('Ctrl Pts',(43.6182814563195,38.0698842033573,46.5041878183656));
#24281=CARTESIAN_POINT('Ctrl Pts',(43.609724385289,38.0705953417871,46.497258940181));
#24282=CARTESIAN_POINT('Ctrl Pts',(43.5941683541407,38.0718846607242,46.484881800432));
#24283=CARTESIAN_POINT('Ctrl Pts',(43.5871901963442,38.0724617870051,46.4794077962919));
#24284=CARTESIAN_POINT('Ctrl Pts',(43.5721485664578,38.0737033004324,46.4677750683705));
#24285=CARTESIAN_POINT('Ctrl Pts',(43.5640737850582,38.0743682632118,46.4616314748382));
#24286=CARTESIAN_POINT('Ctrl Pts',(43.5418572226091,38.0761939164913,46.4450033604784));
#24287=CARTESIAN_POINT('Ctrl Pts',(43.5276200845685,38.0773596060269,46.4346484818016));
#24288=CARTESIAN_POINT('Ctrl Pts',(43.4439644705572,38.0841864833071,46.3755380417219));
#24289=CARTESIAN_POINT('Ctrl Pts',(43.3715418859448,38.0900136533926,46.3312156399125));
#24290=CARTESIAN_POINT('Ctrl Pts',(43.1940433649751,38.1040847206503,46.2380657598986));
#24291=CARTESIAN_POINT('Ctrl Pts',(43.0870172085324,38.1124176925237,46.1936440701145));
#24292=CARTESIAN_POINT('Ctrl Pts',(42.9424480925474,38.1231621886984,46.1483578843879));
#24293=CARTESIAN_POINT('Ctrl Pts',(42.9079344253046,38.1256891277892,46.1385942649481));
#24294=CARTESIAN_POINT('Ctrl Pts',(42.8371291768762,38.1307725634051,46.1206803062474));
#24295=CARTESIAN_POINT('Ctrl Pts',(42.8008322182366,38.1333257715061,46.1126053948789));
#24296=CARTESIAN_POINT('Ctrl Pts',(42.754760839883,38.1364821090489,46.1037452445277));
#24297=CARTESIAN_POINT('Ctrl Pts',(42.7451857724544,38.1371335256212,46.1019788875023));
#24298=CARTESIAN_POINT('Ctrl Pts',(42.7300477835494,38.1381557639955,46.0993046593495));
#24299=CARTESIAN_POINT('Ctrl Pts',(42.724493711424,38.1385292008528,46.0983485727744));
#24300=CARTESIAN_POINT('Ctrl Pts',(42.7139789917127,38.1392330126092,46.0965859603361));
#24301=CARTESIAN_POINT('Ctrl Pts',(42.7090194236735,38.1395636444851,46.0957744855223));
#24302=CARTESIAN_POINT('Ctrl Pts',(42.6973604419017,38.1403378307104,46.0939136155589));
#24303=CARTESIAN_POINT('Ctrl Pts',(42.6906585945456,38.1407804853452,46.0928801500175));
#24304=CARTESIAN_POINT('Ctrl Pts',(42.6686191159204,38.142228834074,46.0896004058019));
#24305=CARTESIAN_POINT('Ctrl Pts',(42.6532593865179,38.1432265357254,46.0875035793695));
#24306=CARTESIAN_POINT('Ctrl Pts',(42.5673918001028,38.1487474431376,46.0768340706416));
#24307=CARTESIAN_POINT('Ctrl Pts',(42.4964701280656,38.1530954842667,46.0719743407672));
#24308=CARTESIAN_POINT('Ctrl Pts',(42.3243555401359,38.1634752807328,46.0697048672239));
#24309=CARTESIAN_POINT('Ctrl Pts',(42.2233272886737,38.1694308425207,46.0763189574079));
#24310=CARTESIAN_POINT('Ctrl Pts',(42.0336143009998,38.1809812381941,46.103816153472));
#24311=CARTESIAN_POINT('Ctrl Pts',(41.9449849794371,38.1865343154721,46.1231116464965));
#24312=CARTESIAN_POINT('Ctrl Pts',(41.8405433320331,38.1934510545008,46.153683832365));
#24313=CARTESIAN_POINT('Ctrl Pts',(41.8231145709406,38.1946178177491,46.1590550471593));
#24314=CARTESIAN_POINT('Ctrl Pts',(41.7958789029824,38.1964620700816,46.16787330171));
#24315=CARTESIAN_POINT('Ctrl Pts',(41.7860189488402,38.1971340868875,46.1711539703255));
#24316=CARTESIAN_POINT('Ctrl Pts',(41.7678896458641,38.198377981206,46.1773492032833));
#24317=CARTESIAN_POINT('Ctrl Pts',(41.7596126952469,38.1989490842556,46.1802408065321));
#24318=CARTESIAN_POINT('Ctrl Pts',(41.7413123925342,38.2002190427889,46.1867744427497));
#24319=CARTESIAN_POINT('Ctrl Pts',(41.7312990100742,38.2009187799918,46.1904433515382));
#24320=CARTESIAN_POINT('Ctrl Pts',(41.703037334668,38.2029077637198,46.2010650557742));
#24321=CARTESIAN_POINT('Ctrl Pts',(41.6848639053973,38.2042034705136,46.2082120078709));
#24322=CARTESIAN_POINT('Ctrl Pts',(41.6439215836784,38.2071615655797,46.225035233195));
#24323=CARTESIAN_POINT('Ctrl Pts',(41.6212244090851,38.2088292727656,46.2348759310476));
#24324=CARTESIAN_POINT('Ctrl Pts',(41.5477058314402,38.2143239514411,46.2684450117237));
#24325=CARTESIAN_POINT('Ctrl Pts',(41.4977325345518,38.2182071570383,46.2939517951274));
#24326=CARTESIAN_POINT('Ctrl Pts',(41.3308746376221,38.2316680505038,46.3885006426163));
#24327=CARTESIAN_POINT('Ctrl Pts',(41.2202028421741,38.241495192672,46.4676702495838));
#24328=CARTESIAN_POINT('Ctrl Pts',(41.0802584481814,38.2546550837173,46.5919954585786));
#24329=CARTESIAN_POINT('Ctrl Pts',(41.0431402466294,38.2582244728711,46.6277291840621));
#24330=CARTESIAN_POINT('Ctrl Pts',(41.0001563111384,38.2624112774179,46.6725616392385));
#24331=CARTESIAN_POINT('Ctrl Pts',(40.9928821435564,38.2631217430239,46.6802749129147));
#24332=CARTESIAN_POINT('Ctrl Pts',(40.9816671563294,38.2642195890141,46.6923650451294));
#24333=CARTESIAN_POINT('Ctrl Pts',(40.9776822986068,38.2646101670077,46.6967004990273));
#24334=CARTESIAN_POINT('Ctrl Pts',(40.9703630478456,38.2653283746357,46.7047372630213));
#24335=CARTESIAN_POINT('Ctrl Pts',(40.9670231437181,38.2656564074203,46.7084332370719));
#24336=CARTESIAN_POINT('Ctrl Pts',(40.9594416016885,38.2664017731188,46.7168886646609));
#24337=CARTESIAN_POINT('Ctrl Pts',(40.9552092121771,38.2668184170653,46.7216562355496));
#24338=CARTESIAN_POINT('Ctrl Pts',(40.9426280734039,38.2680588762959,46.7359705456478));
#24339=CARTESIAN_POINT('Ctrl Pts',(40.9343495551088,38.2688777066575,46.7455789431137));
#24340=CARTESIAN_POINT('Ctrl Pts',(40.8593661970961,38.2763259522985,46.8343635689892));
#24341=CARTESIAN_POINT('Ctrl Pts',(40.7990318110347,38.2825566281651,46.9187194066031));
#24342=CARTESIAN_POINT('Ctrl Pts',(40.7056194365599,38.2934067504237,47.0744175103242));
#24343=CARTESIAN_POINT('Ctrl Pts',(40.6695797137903,38.2980338761474,47.1436859391152));
#24344=CARTESIAN_POINT('Ctrl Pts',(40.6030423303135,38.3079070958165,47.2930383394611));
#24345=CARTESIAN_POINT('Ctrl Pts',(40.5734847052241,38.3131603611238,47.3733495127022));
#24346=CARTESIAN_POINT('Ctrl Pts',(40.5442665095039,38.3197399817398,47.4726289650197));
#24347=CARTESIAN_POINT('Ctrl Pts',(40.5394235313273,38.320892600617,47.4899782698166));
#24348=CARTESIAN_POINT('Ctrl Pts',(40.5321837910426,38.3227193378752,47.5173903257529));
#24349=CARTESIAN_POINT('Ctrl Pts',(40.5296237308704,38.3233881560484,47.5274091694835));
#24350=CARTESIAN_POINT('Ctrl Pts',(40.5250416628631,38.3246290190652,47.5459617882296));
#24351=CARTESIAN_POINT('Ctrl Pts',(40.5229970510513,38.3252003159665,47.5544897429874));
#24352=CARTESIAN_POINT('Ctrl Pts',(40.5185819939146,38.326474316769,47.57347472695));
#24353=CARTESIAN_POINT('Ctrl Pts',(40.5162404560886,38.3271779315351,47.5839381115833));
#24354=CARTESIAN_POINT('Ctrl Pts',(40.5115883779812,38.3286358591826,47.6055710555313));
#24355=CARTESIAN_POINT('Ctrl Pts',(40.5092894344784,38.3293905140956,47.6167426526673));
#24356=CARTESIAN_POINT('Ctrl Pts',(40.5035983753021,38.3313511438125,47.6456962735304));
#24357=CARTESIAN_POINT('Ctrl Pts',(40.5003573131292,38.332561836806,47.663506497741));
#24358=CARTESIAN_POINT('Ctrl Pts',(40.4796312963282,38.3410083164143,47.7872633835643));
#24359=CARTESIAN_POINT('Ctrl Pts',(40.4707714790782,38.3485105546629,47.8944436334601));
#24360=CARTESIAN_POINT('Ctrl Pts',(40.4708708262362,38.3561431341929,48.0017854504995));
#24361=CARTESIAN_POINT('Ctrl Pts',(41.7941388317924,38.5145390814761,49.8315225365138));
#24362=CARTESIAN_POINT('Ctrl Pts',(41.7299216957678,38.5100838283546,49.8102797353606));
#24363=CARTESIAN_POINT('Ctrl Pts',(41.6666977242728,38.5056285752331,49.7856139649871));
#24364=CARTESIAN_POINT('Ctrl Pts',(41.604857307503,38.5011733221117,49.7576378055414));
#24365=CARTESIAN_POINT('Ctrl Pts',(41.5404242173827,38.4965312815033,49.728488739333));
#24366=CARTESIAN_POINT('Ctrl Pts',(41.4774937984495,38.4918892408949,49.695745643155));
#24367=CARTESIAN_POINT('Ctrl Pts',(41.4164901120889,38.4872472002865,49.6595935819595));
#24368=CARTESIAN_POINT('Ctrl Pts',(41.3580952101157,38.4828036736333,49.6249875409874));
#24369=CARTESIAN_POINT('Ctrl Pts',(41.3014660882663,38.4783601469802,49.58725843197));
#24370=CARTESIAN_POINT('Ctrl Pts',(41.2469521014508,38.473916620327,49.5466166624446));
#24371=CARTESIAN_POINT('Ctrl Pts',(41.1924695936992,38.4694756595853,49.5059983614809));
#24372=CARTESIAN_POINT('Ctrl Pts',(41.1401001932213,38.4650346988435,49.4624710309536));
#24373=CARTESIAN_POINT('Ctrl Pts',(41.0901639809884,38.4605937381018,49.4162881628397));
#24374=CARTESIAN_POINT('Ctrl Pts',(41.040239343403,38.4561538067243,49.3701159993908));
#24375=CARTESIAN_POINT('Ctrl Pts',(40.9927471365817,38.4517138753469,49.3212898556712));
#24376=CARTESIAN_POINT('Ctrl Pts',(40.9479726604171,38.4472739439695,49.2701020281866));
#24377=CARTESIAN_POINT('Ctrl Pts',(40.9031930861608,38.4428335070545,49.2189083723763));
#24378=CARTESIAN_POINT('Ctrl Pts',(40.861132179701,38.4383930701396,49.1653528725191));
#24379=CARTESIAN_POINT('Ctrl Pts',(40.8220355921919,38.4339526332247,49.1097616341318));
#24380=CARTESIAN_POINT('Ctrl Pts',(40.7828957995435,38.4295072892396,49.0541089625772));
#24381=CARTESIAN_POINT('Ctrl Pts',(40.746727145482,38.4250619452546,48.9964164690217));
#24382=CARTESIAN_POINT('Ctrl Pts',(40.7137318736977,38.4206166012696,48.9370391470568));
#24383=CARTESIAN_POINT('Ctrl Pts',(40.6807150902982,38.4161683590957,48.8776231134209));
#24384=CARTESIAN_POINT('Ctrl Pts',(40.6508760217607,38.4117201169218,48.8165205094757));
#24385=CARTESIAN_POINT('Ctrl Pts',(40.6243696140539,38.4072718747479,48.7541082743247));
#24386=CARTESIAN_POINT('Ctrl Pts',(40.5978184275985,38.4028161179112,48.6915906027141));
#24387=CARTESIAN_POINT('Ctrl Pts',(40.5746113015034,38.3983603610744,48.627759349526));
#24388=CARTESIAN_POINT('Ctrl Pts',(40.5548536832294,38.3939046042376,48.5630076612336));
#24389=CARTESIAN_POINT('Ctrl Pts',(40.5487341383369,38.3925245186618,48.5429520625337));
#24390=CARTESIAN_POINT('Ctrl Pts',(40.5429451459992,38.391144433086,48.522808238269));
#24391=CARTESIAN_POINT('Ctrl Pts',(40.5374888394459,38.3897643475102,48.5025880357822));
#24392=CARTESIAN_POINT('Ctrl Pts',(40.5151350420091,38.3841103115601,48.4197484251217));
#24393=CARTESIAN_POINT('Ctrl Pts',(40.4982971116051,38.3784562756099,48.3353614403265));
#24394=CARTESIAN_POINT('Ctrl Pts',(40.4871470116547,38.3728022396598,48.2500719933908));
#24395=CARTESIAN_POINT('Ctrl Pts',(40.4764097519324,38.3673575483345,48.167940447719));
#24396=CARTESIAN_POINT('Ctrl Pts',(40.4709468203384,38.3619128570092,48.0849718892169));
#24397=CARTESIAN_POINT('Ctrl Pts',(40.4708708049845,38.3564681656839,48.001762339035));
#24398=CARTESIAN_POINT('',(40.470870157182,38.525946964697,47.9992212516664));
#24399=CARTESIAN_POINT('Ctrl Pts',(41.7941383335288,38.6866921868075,49.8315223716899));
#24400=CARTESIAN_POINT('Ctrl Pts',(41.7345131632266,38.6822978481676,49.811798558538));
#24401=CARTESIAN_POINT('Ctrl Pts',(41.6758511936192,38.6778350035951,49.7891631561228));
#24402=CARTESIAN_POINT('Ctrl Pts',(41.5063613798738,38.6646047384149,49.7140482245953));
#24403=CARTESIAN_POINT('Ctrl Pts',(41.3993318161974,38.6557943233053,49.6538499110831));
#24404=CARTESIAN_POINT('Ctrl Pts',(41.2857470068709,38.6463847195162,49.5748754919079));
#24405=CARTESIAN_POINT('Ctrl Pts',(41.2728763285008,38.6453178685796,49.5656898851235));
#24406=CARTESIAN_POINT('Ctrl Pts',(41.2550011804056,38.6438369540284,49.5525979874554));
#24407=CARTESIAN_POINT('Ctrl Pts',(41.2499012506518,38.6434145248567,49.5488239658133));
#24408=CARTESIAN_POINT('Ctrl Pts',(41.2410977614784,38.6426856145579,49.5422417962612));
#24409=CARTESIAN_POINT('Ctrl Pts',(41.2373855982471,38.6423783442543,49.5394453256201));
#24410=CARTESIAN_POINT('Ctrl Pts',(41.2296150603196,38.6417353974066,49.5335474358518));
#24411=CARTESIAN_POINT('Ctrl Pts',(41.2255588228935,38.6413999249021,49.530443258614));
#24412=CARTESIAN_POINT('Ctrl Pts',(41.2157684695609,38.6405904374971,49.5228890047723));
#24413=CARTESIAN_POINT('Ctrl Pts',(41.2100469840157,38.6401175626914,49.5184225572714));
#24414=CARTESIAN_POINT('Ctrl Pts',(41.1975741273322,38.6390867725923,49.5085718886914));
#24415=CARTESIAN_POINT('Ctrl Pts',(41.1908333869482,38.6385297507721,49.5031743847474));
#24416=CARTESIAN_POINT('Ctrl Pts',(41.1717853435303,38.6369551185881,49.4877110247934));
#24417=CARTESIAN_POINT('Ctrl Pts',(41.1595656274798,38.6359442446782,49.4775377960907));
#24418=CARTESIAN_POINT('Ctrl Pts',(41.024671210722,38.6247590070962,49.3623815129185));
#24419=CARTESIAN_POINT('Ctrl Pts',(40.9155015210314,38.6154184177973,49.2425340352882));
#24420=CARTESIAN_POINT('Ctrl Pts',(40.770390204396,38.6002288398038,49.0363976472431));
#24421=CARTESIAN_POINT('Ctrl Pts',(40.7235347387086,38.5946768683313,48.9587540343476));
#24422=CARTESIAN_POINT('Ctrl Pts',(40.6740101399462,38.5877615818485,48.8618781845855));
#24423=CARTESIAN_POINT('Ctrl Pts',(40.6659415151775,38.5865950808534,48.845527135437));
#24424=CARTESIAN_POINT('Ctrl Pts',(40.6536414510752,38.5847512718634,48.8196842680601));
#24425=CARTESIAN_POINT('Ctrl Pts',(40.6492527394026,38.584079433847,48.8102681674697));
#24426=CARTESIAN_POINT('Ctrl Pts',(40.641301886416,38.5828358894247,48.7928431912967));
#24427=CARTESIAN_POINT('Ctrl Pts',(40.6377178461755,38.5822649571779,48.784844562157));
#24428=CARTESIAN_POINT('Ctrl Pts',(40.6298955906118,38.580995403973,48.7670636152126));
#24429=CARTESIAN_POINT('Ctrl Pts',(40.6256837324284,38.5802959020097,48.7572700870777));
#24430=CARTESIAN_POINT('Ctrl Pts',(40.6137894100295,38.57827351474,48.7289690161755));
#24431=CARTESIAN_POINT('Ctrl Pts',(40.6063140495642,38.5769436781771,48.7103764901403));
#24432=CARTESIAN_POINT('Ctrl Pts',(40.5543563741725,38.5672557408761,48.5750969136374));
#24433=CARTESIAN_POINT('Ctrl Pts',(40.5210158307069,38.558523920786,48.4544720155103));
#24434=CARTESIAN_POINT('Ctrl Pts',(40.4804260210494,38.5416985024399,48.2217730010995));
#24435=CARTESIAN_POINT('Ctrl Pts',(40.4708251956828,38.5336760400102,48.11060071288));
#24436=CARTESIAN_POINT('Ctrl Pts',(40.470870157182,38.525946964697,47.9992212516664));
#24437=CARTESIAN_POINT('Ctrl Pts',(40.4708701582568,38.525946780244,47.999218593614));
#24438=CARTESIAN_POINT('Ctrl Pts',(40.4708828771651,38.5237677840215,47.9678182544532));
#24439=CARTESIAN_POINT('Ctrl Pts',(40.4716622495162,38.521614512766,47.9364204037251));
#24440=CARTESIAN_POINT('Ctrl Pts',(40.4735867665144,38.5189788945381,47.8973654208977));
#24441=CARTESIAN_POINT('Ctrl Pts',(40.4740116154422,38.5184622999845,47.8896797830328));
#24442=CARTESIAN_POINT('Ctrl Pts',(40.4748112955889,38.5175889646993,47.876631006523));
#24443=CARTESIAN_POINT('Ctrl Pts',(40.4751625608978,38.5172310083412,47.87126658988));
#24444=CARTESIAN_POINT('Ctrl Pts',(40.4758591479525,38.5165660252818,47.8612696260183));
#24445=CARTESIAN_POINT('Ctrl Pts',(40.4761987858263,38.5162586913329,47.8566367387658));
#24446=CARTESIAN_POINT('Ctrl Pts',(40.4769427946358,38.5156190460474,47.8469670843212));
#24447=CARTESIAN_POINT('Ctrl Pts',(40.4773502233187,38.5152869238488,47.8419306315224));
#24448=CARTESIAN_POINT('Ctrl Pts',(40.4782953772045,38.5145545771141,47.8307917642694));
#24449=CARTESIAN_POINT('Ctrl Pts',(40.4788423962425,38.5141548677088,47.8246901361843));
#24450=CARTESIAN_POINT('Ctrl Pts',(40.4808871023558,38.5127416111478,47.8030427687767));
#24451=CARTESIAN_POINT('Ctrl Pts',(40.4825445378641,38.5117365472453,47.787512228136));
#24452=CARTESIAN_POINT('Ctrl Pts',(40.4890904066313,38.5082033222473,47.7325144643651));
#24453=CARTESIAN_POINT('Ctrl Pts',(40.4950106074898,38.5057236959999,47.6931777964464));
#24454=CARTESIAN_POINT('Ctrl Pts',(40.5228658095184,38.496179636794,47.5403663602293));
#24455=CARTESIAN_POINT('Ctrl Pts',(40.5537622609088,38.4893899605038,47.4287684341477));
#24456=CARTESIAN_POINT('Ctrl Pts',(40.6322377188398,38.4760360474054,47.2202159453531));
#24457=CARTESIAN_POINT('Ctrl Pts',(40.6783120434001,38.4695130050146,47.1231689427268));
#24458=CARTESIAN_POINT('Ctrl Pts',(40.7414842708779,38.461523942277,47.0145006803006));
#24459=CARTESIAN_POINT('Ctrl Pts',(40.750990264355,38.460342831877,46.9986757834234));
#24460=CARTESIAN_POINT('Ctrl Pts',(40.7661666121303,38.4584879831545,46.9742136220707));
#24461=CARTESIAN_POINT('Ctrl Pts',(40.7716818955155,38.457819949258,46.9654810894983));
#24462=CARTESIAN_POINT('Ctrl Pts',(40.7815739647561,38.4566321366866,46.9500937369045));
#24463=CARTESIAN_POINT('Ctrl Pts',(40.7859223751219,38.4561134254891,46.9434208924532));
#24464=CARTESIAN_POINT('Ctrl Pts',(40.7960388770744,38.4549143821289,46.928104833901));
#24465=CARTESIAN_POINT('Ctrl Pts',(40.8018356882228,38.4542329782975,46.9194809782624));
#24466=CARTESIAN_POINT('Ctrl Pts',(40.8180014092799,38.4523478753954,46.8958460912822));
#24467=CARTESIAN_POINT('Ctrl Pts',(40.8285138053603,38.4511387468309,46.8809349901932));
#24468=CARTESIAN_POINT('Ctrl Pts',(40.8926322914025,38.4438597767395,46.792672784679));
#24469=CARTESIAN_POINT('Ctrl Pts',(40.9511462556602,38.4375988435618,46.7230446786938));
#24470=CARTESIAN_POINT('Ctrl Pts',(41.1266021784099,38.4198390688107,46.5419067131972));
#24471=CARTESIAN_POINT('Ctrl Pts',(41.2529561922209,38.4080714894062,46.4405554325174));
#24472=CARTESIAN_POINT('Ctrl Pts',(41.403932690626,38.3959089596003,46.3478369256697));
#24473=CARTESIAN_POINT('Ctrl Pts',(41.4175174961777,38.394830480361,46.3397225910146));
#24474=CARTESIAN_POINT('Ctrl Pts',(41.4386434202174,38.393179452719,46.3274539910938));
#24475=CARTESIAN_POINT('Ctrl Pts',(41.4461147666631,38.3926005254017,46.3231817052689));
#24476=CARTESIAN_POINT('Ctrl Pts',(41.4600581359444,38.3915296629823,46.3153319237529));
#24477=CARTESIAN_POINT('Ctrl Pts',(41.4665225897587,38.391036968115,46.3117413812084));
#24478=CARTESIAN_POINT('Ctrl Pts',(41.4774598976384,38.3902099309013,46.3057485162845));
#24479=CARTESIAN_POINT('Ctrl Pts',(41.4819218320276,38.3898743645437,46.3033265458544));
#24480=CARTESIAN_POINT('Ctrl Pts',(41.4905098397954,38.3892320688824,46.2987087109564));
#24481=CARTESIAN_POINT('Ctrl Pts',(41.4946344018336,38.3889251652736,46.2965101889044));
#24482=CARTESIAN_POINT('Ctrl Pts',(41.5044690072693,38.3881970192153,46.2913138415089));
#24483=CARTESIAN_POINT('Ctrl Pts',(41.5101862179994,38.3877766238892,46.2883295926389));
#24484=CARTESIAN_POINT('Ctrl Pts',(41.5305250086771,38.3862909671198,46.2778426695003));
#24485=CARTESIAN_POINT('Ctrl Pts',(41.5452278595765,38.3852350339145,46.2704979725989));
#24486=CARTESIAN_POINT('Ctrl Pts',(41.6534745254211,38.377578991168,46.2181418615298));
#24487=CARTESIAN_POINT('Ctrl Pts',(41.7504344936811,38.3713554792503,46.1805525576345));
#24488=CARTESIAN_POINT('Ctrl Pts',(41.9523371384044,38.3587799056597,46.1204923208798));
#24489=CARTESIAN_POINT('Ctrl Pts',(42.0570606023698,38.3524465994496,46.0985947214382));
#24490=CARTESIAN_POINT('Ctrl Pts',(42.2181705055776,38.342469653369,46.0786554619686));
#24491=CARTESIAN_POINT('Ctrl Pts',(42.2735502556596,38.3390016023127,46.0742179836061));
#24492=CARTESIAN_POINT('Ctrl Pts',(42.3446459739966,38.3344622059646,46.0716010929313));
#24493=CARTESIAN_POINT('Ctrl Pts',(42.3602573121018,38.3334601480009,46.0712162100114));
#24494=CARTESIAN_POINT('Ctrl Pts',(42.3855819168024,38.3318252874659,46.0708994355424));
#24495=CARTESIAN_POINT('Ctrl Pts',(42.3952932218594,38.3311961397296,46.0708512993016));
#24496=CARTESIAN_POINT('Ctrl Pts',(42.4139572395595,38.3299825356453,46.0708997155454));
#24497=CARTESIAN_POINT('Ctrl Pts',(42.4229097481966,38.3293984404601,46.0709852642114));
#24498=CARTESIAN_POINT('Ctrl Pts',(42.4434331495145,38.3280547528015,46.071324271756));
#24499=CARTESIAN_POINT('Ctrl Pts',(42.4550029126305,38.3272938678415,46.0716195466551));
#24500=CARTESIAN_POINT('Ctrl Pts',(42.4919142552796,38.3248551697899,46.0728940172018));
#24501=CARTESIAN_POINT('Ctrl Pts',(42.5172385930815,38.3231650781469,46.0742687864083));
#24502=CARTESIAN_POINT('Ctrl Pts',(42.6753525891751,38.3125021041073,46.0859825370008));
#24503=CARTESIAN_POINT('Ctrl Pts',(42.8067781968864,38.3031123722117,46.1095499431242));
#24504=CARTESIAN_POINT('Ctrl Pts',(43.0071000741235,38.2882257143609,46.167338233671));
#24505=CARTESIAN_POINT('Ctrl Pts',(43.0782109842461,38.2828293234543,46.1924463375233));
#24506=CARTESIAN_POINT('Ctrl Pts',(43.1794685955045,38.2751110808578,46.2350181493611));
#24507=CARTESIAN_POINT('Ctrl Pts',(43.2109020358738,38.2727106318649,46.2492371957595));
#24508=CARTESIAN_POINT('Ctrl Pts',(43.2615560057805,38.2688530675511,46.2738078965972));
#24509=CARTESIAN_POINT('Ctrl Pts',(43.281011290616,38.2673741215825,46.283655881264));
#24510=CARTESIAN_POINT('Ctrl Pts',(43.3071528421466,38.2653946509521,46.2974500365546));
#24511=CARTESIAN_POINT('Ctrl Pts',(43.3139875466697,38.2648778490537,46.3011093541202));
#24512=CARTESIAN_POINT('Ctrl Pts',(43.3253693624177,38.2640186777861,46.3072917742108));
#24513=CARTESIAN_POINT('Ctrl Pts',(43.3299286046148,38.2636749113159,46.3097922060175));
#24514=CARTESIAN_POINT('Ctrl Pts',(43.3385524028167,38.2630255060592,46.3145672256351));
#24515=CARTESIAN_POINT('Ctrl Pts',(43.3426189114209,38.2627196309846,46.3168381424467));
#24516=CARTESIAN_POINT('Ctrl Pts',(43.3522401940965,38.2619966677628,46.3222568931005));
#24517=CARTESIAN_POINT('Ctrl Pts',(43.3577876869971,38.2615803984777,46.3254176432707));
#24518=CARTESIAN_POINT('Ctrl Pts',(43.3772237379715,38.2601236447576,46.336619745097));
#24519=CARTESIAN_POINT('Ctrl Pts',(43.3910280009102,38.2590920224127,46.34480706613));
#24520=CARTESIAN_POINT('Ctrl Pts',(43.5053947930275,38.2505566087909,46.4145819410158));
#24521=CARTESIAN_POINT('Ctrl Pts',(43.6002319135202,38.2435437827632,46.4851075451388));
#24522=CARTESIAN_POINT('Ctrl Pts',(43.7920307615505,38.2281776174326,46.6571281789475));
#24523=CARTESIAN_POINT('Ctrl Pts',(43.885567937651,38.2198400748564,46.7613976280763));
#24524=CARTESIAN_POINT('Ctrl Pts',(43.979126806952,38.209673417496,46.8916987706547));
#24525=CARTESIAN_POINT('Ctrl Pts',(43.9909555891399,38.2083486029498,46.9087468912238));
#24526=CARTESIAN_POINT('Ctrl Pts',(44.008523455373,38.2063178806684,46.934959322801));
#24527=CARTESIAN_POINT('Ctrl Pts',(44.0144645268454,38.2056196053928,46.9439869156749));
#24528=CARTESIAN_POINT('Ctrl Pts',(44.0251343926841,38.204344047837,46.9605005261727));
#24529=CARTESIAN_POINT('Ctrl Pts',(44.0298881275316,38.2037677180478,46.9679701372034));
#24530=CARTESIAN_POINT('Ctrl Pts',(44.0400581925859,38.2025170270191,46.9841960387369));
#24531=CARTESIAN_POINT('Ctrl Pts',(44.0454561568118,38.2018420092287,46.9929634605411));
#24532=CARTESIAN_POINT('Ctrl Pts',(44.0600054373806,38.199991425817,47.0170238460025));
#24533=CARTESIAN_POINT('Ctrl Pts',(44.0690152352166,38.1988107505105,47.0324007649544));
#24534=CARTESIAN_POINT('Ctrl Pts',(44.1176546217441,38.1922387343321,47.1181140934827));
#24535=CARTESIAN_POINT('Ctrl Pts',(44.1530466289284,38.1866984006722,47.190750619225));
#24536=CARTESIAN_POINT('Ctrl Pts',(44.2322888929989,38.1721134479023,47.3831647708215));
#24537=CARTESIAN_POINT('Ctrl Pts',(44.2690091596579,38.1629128345966,47.505460373763));
#24538=CARTESIAN_POINT('Ctrl Pts',(44.3054362809851,38.149469917971,47.6921054779624));
#24539=CARTESIAN_POINT('Ctrl Pts',(44.3144503266707,38.145091486024,47.7543007512472));
#24540=CARTESIAN_POINT('Ctrl Pts',(44.321437675373,38.140130268204,47.8275588564956));
#24541=CARTESIAN_POINT('Ctrl Pts',(44.3223710070259,38.1394080991493,47.8382952912293));
#24542=CARTESIAN_POINT('Ctrl Pts',(44.3236729216371,38.1383006350748,47.854881466209));
#24543=CARTESIAN_POINT('Ctrl Pts',(44.3241048825643,38.1379119722042,47.860725804802));
#24544=CARTESIAN_POINT('Ctrl Pts',(44.3248548435972,38.1371956140276,47.8715429416073));
#24545=CARTESIAN_POINT('Ctrl Pts',(44.325180209317,38.1368675307165,47.8765149914305));
#24546=CARTESIAN_POINT('Ctrl Pts',(44.3258800302165,38.1361199314396,47.8878851518256));
#24547=CARTESIAN_POINT('Ctrl Pts',(44.3262418698489,38.1357011226355,47.8942839098425));
#24548=CARTESIAN_POINT('Ctrl Pts',(44.3271085100355,38.1346055335085,47.9110954244415));
#24549=CARTESIAN_POINT('Ctrl Pts',(44.3275608152474,38.1339315558168,47.9215108407627));
#24550=CARTESIAN_POINT('Ctrl Pts',(44.330602046884,38.1283935028826,48.007646448082));
#24551=CARTESIAN_POINT('Ctrl Pts',(44.3288129001901,38.1237460055738,48.0834647323864));
#24552=CARTESIAN_POINT('Ctrl Pts',(44.3134294778128,38.1124832129306,48.2694874058114));
#24553=CARTESIAN_POINT('Ctrl Pts',(44.2947827881961,38.1059655818114,48.3789917164589));
#24554=CARTESIAN_POINT('Ctrl Pts',(44.245711657485,38.0941960435457,48.5673725662768));
#24555=CARTESIAN_POINT('Ctrl Pts',(44.2193328286842,38.0890394078023,48.646984246574));
#24556=CARTESIAN_POINT('Ctrl Pts',(44.1812737444074,38.0825917940524,48.740887565833));
#24557=CARTESIAN_POINT('Ctrl Pts',(44.1744603679558,38.0814679571615,48.7570607027052));
#24558=CARTESIAN_POINT('Ctrl Pts',(44.1633666564329,38.0796834401741,48.7824214080142));
#24559=CARTESIAN_POINT('Ctrl Pts',(44.1592328354569,38.0790277670848,48.7916723115531));
#24560=CARTESIAN_POINT('Ctrl Pts',(44.1513449762753,38.0777935572384,48.8089573316478));
#24561=CARTESIAN_POINT('Ctrl Pts',(44.1476080317465,38.0772156226168,48.816998992225));
#24562=CARTESIAN_POINT('Ctrl Pts',(44.1391019866668,38.0759149699601,48.8349780413386));
#24563=CARTESIAN_POINT('Ctrl Pts',(44.1343029238249,38.0751912248091,48.8449008281262));
#24564=CARTESIAN_POINT('Ctrl Pts',(44.1218450636452,38.073337437284,48.870105930736));
#24565=CARTESIAN_POINT('Ctrl Pts',(44.1140678263621,38.0722032857657,48.885328305437));
#24566=CARTESIAN_POINT('Ctrl Pts',(44.0533122374122,38.0635127370108,49.0004430373963));
#24567=CARTESIAN_POINT('Ctrl Pts',(43.9918550135485,38.0556510387715,49.0955898828234));
#24568=CARTESIAN_POINT('Ctrl Pts',(43.8356244396221,38.0375910909269,49.2963423551251));
#24569=CARTESIAN_POINT('Ctrl Pts',(43.7368179572382,38.0273443997952,49.3980135428803));
#24570=CARTESIAN_POINT('Ctrl Pts',(43.6116223334799,38.0162341301515,49.5013171136203));
#24571=CARTESIAN_POINT('Ctrl Pts',(43.5952406139366,38.0148136520421,49.5143915339451));
#24572=CARTESIAN_POINT('Ctrl Pts',(43.5726032867357,38.0128992348627,49.5318623947231));
#24573=CARTESIAN_POINT('Ctrl Pts',(43.5665305189835,38.0123903256665,49.5364919191376));
#24574=CARTESIAN_POINT('Ctrl Pts',(43.5562956461419,38.0115406303185,49.5441987320435));
#24575=CARTESIAN_POINT('Ctrl Pts',(43.552148403139,38.0111985103501,49.5472955130144));
#24576=CARTESIAN_POINT('Ctrl Pts',(43.5442286455974,38.0105494044313,49.5531597640408));
#24577=CARTESIAN_POINT('Ctrl Pts',(43.540458462733,38.010242200991,49.5559302497188));
#24578=CARTESIAN_POINT('Ctrl Pts',(43.5314525312783,38.0095125592745,49.5624978580046));
#24579=CARTESIAN_POINT('Ctrl Pts',(43.5262076516921,38.0090909762904,49.5662824505859));
#24580=CARTESIAN_POINT('Ctrl Pts',(43.5074800908337,38.0075971290453,49.5796531503095));
#24581=CARTESIAN_POINT('Ctrl Pts',(43.4938928023392,38.0065343265305,49.5890924479047));
#24582=CARTESIAN_POINT('Ctrl Pts',(43.3990021682629,37.9992434871589,49.6532204960091));
#24583=CARTESIAN_POINT('Ctrl Pts',(43.3137462156888,37.993349422584,49.7018272747386));
#24584=CARTESIAN_POINT('Ctrl Pts',(43.1281716410722,37.9810819937308,49.7896426472311));
#24585=CARTESIAN_POINT('Ctrl Pts',(43.0275328132674,37.9747321865891,49.8273631148328));
#24586=CARTESIAN_POINT('Ctrl Pts',(42.8860712856132,37.9657252336868,49.8673119171781));
#24587=CARTESIAN_POINT('Ctrl Pts',(42.8475381334365,37.9632653987664,49.876919925449));
#24588=CARTESIAN_POINT('Ctrl Pts',(42.7809075769987,37.9589804295541,49.8913653523718));
#24589=CARTESIAN_POINT('Ctrl Pts',(42.7529484643632,37.9571730984245,49.8967816758628));
#24590=CARTESIAN_POINT('Ctrl Pts',(42.7128086705744,37.9545604135965,49.9036394835358));
#24591=CARTESIAN_POINT('Ctrl Pts',(42.7007173875253,37.9537710925186,49.9055869408502));
#24592=CARTESIAN_POINT('Ctrl Pts',(42.6796831166216,37.9523936127224,49.9087696035394));
#24593=CARTESIAN_POINT('Ctrl Pts',(42.6707483877105,37.9518071397987,49.9100574208714));
#24594=CARTESIAN_POINT('Ctrl Pts',(42.6534980129453,37.9506720690815,49.9124203555728));
#24595=CARTESIAN_POINT('Ctrl Pts',(42.645183734059,37.9501237575855,49.9135040610787));
#24596=CARTESIAN_POINT('Ctrl Pts',(42.6254354936514,37.9488183520545,49.9159472791148));
#24597=CARTESIAN_POINT('Ctrl Pts',(42.6139960114156,37.9480597561804,49.9172586772337));
#24598=CARTESIAN_POINT('Ctrl Pts',(42.573154955329,37.9453424262621,49.9215705455976));
#24599=CARTESIAN_POINT('Ctrl Pts',(42.5436982817441,37.9433658527993,49.9239975673861));
#24600=CARTESIAN_POINT('Ctrl Pts',(42.3571382620817,37.9307356183577,49.9350607728096));
#24601=CARTESIAN_POINT('Ctrl Pts',(42.1995527190802,37.9194952146165,49.925123481119));
#24602=CARTESIAN_POINT('Ctrl Pts',(41.9814009092743,37.9036617675993,49.884276695539));
#24603=CARTESIAN_POINT('Ctrl Pts',(41.9184766450361,37.8990719270222,49.8691870468411));
#24604=CARTESIAN_POINT('Ctrl Pts',(41.8355561037461,37.8930797482899,49.8448356947448));
#24605=CARTESIAN_POINT('Ctrl Pts',(41.8147908688387,37.8915841490299,49.8383541572236));
#24606=CARTESIAN_POINT('Ctrl Pts',(41.7941388317907,37.8901046061668,49.8315225365133));
#24607=CARTESIAN_POINT('Origin',(42.4,48.4493818343519,48.));
#24608=CARTESIAN_POINT('',(41.7941388333426,36.925511940895,49.8315225370267));
#24609=CARTESIAN_POINT('',(41.794138668834,37.0981147778663,49.8315224826078));
#24610=CARTESIAN_POINT('',(41.7941388317924,48.4493818343519,49.8315225365138));
#24611=CARTESIAN_POINT('Ctrl Pts',(41.7941388333426,36.925511940895,49.8315225370267));
#24612=CARTESIAN_POINT('Ctrl Pts',(41.8060345762917,36.926294977607,49.8354576066508));
#24613=CARTESIAN_POINT('Ctrl Pts',(41.817968681362,36.9270813457443,49.839276790227));
#24614=CARTESIAN_POINT('Ctrl Pts',(41.8543274298654,36.9294805522131,49.8505230830555));
#24615=CARTESIAN_POINT('Ctrl Pts',(41.8788617517728,36.9311042214315,49.8575815092058));
#24616=CARTESIAN_POINT('Ctrl Pts',(41.9148648790757,36.933497124824,49.867170081126));
#24617=CARTESIAN_POINT('Ctrl Pts',(41.9262288312078,36.9342538806049,49.8700858448245));
#24618=CARTESIAN_POINT('Ctrl Pts',(41.9463069684267,36.9355938327101,49.87504274115));
#24619=CARTESIAN_POINT('Ctrl Pts',(41.9550101639066,36.9361756099049,49.8771272437635));
#24620=CARTESIAN_POINT('Ctrl Pts',(41.9732093993492,36.9373942948904,49.8813524640453));
#24621=CARTESIAN_POINT('Ctrl Pts',(41.9827077469165,36.9380315440896,49.8834820095747));
#24622=CARTESIAN_POINT('Ctrl Pts',(42.0075782914191,36.9397034710488,49.8888606659938));
#24623=CARTESIAN_POINT('Ctrl Pts',(42.0229745216687,36.9407418223874,49.8919939684465));
#24624=CARTESIAN_POINT('Ctrl Pts',(42.088457553686,36.9451733056218,49.9044894701625));
#24625=CARTESIAN_POINT('Ctrl Pts',(42.1388625314101,36.9486227073296,49.9120526243647));
#24626=CARTESIAN_POINT('Ctrl Pts',(42.3414500871881,36.9626463664976,49.9342906382361));
#24627=CARTESIAN_POINT('Ctrl Pts',(42.4948275987231,36.9736778486032,49.9328487185738));
#24628=CARTESIAN_POINT('Ctrl Pts',(42.6942737474017,36.9879415379767,49.9071643443188));
#24629=CARTESIAN_POINT('Ctrl Pts',(42.7419067904804,36.9913362025543,49.8992033183142));
#24630=CARTESIAN_POINT('Ctrl Pts',(42.8073385398224,36.9959428616924,49.8857256079213));
#24631=CARTESIAN_POINT('Ctrl Pts',(42.8254291772253,36.9972104077715,49.8817268200415));
#24632=CARTESIAN_POINT('Ctrl Pts',(42.8567910341496,36.9993940081145,49.8743191126987));
#24633=CARTESIAN_POINT('Ctrl Pts',(42.8700885109143,37.0003155008391,49.8710283277702));
#24634=CARTESIAN_POINT('Ctrl Pts',(42.8895957424663,37.0016597745725,49.8659796849242));
#24635=CARTESIAN_POINT('Ctrl Pts',(42.8958331854637,37.002088465589,49.8643319529452));
#24636=CARTESIAN_POINT('Ctrl Pts',(42.9068344948969,37.0028424102396,49.8613666429615));
#24637=CARTESIAN_POINT('Ctrl Pts',(42.9116016937555,37.0031683909764,49.8600620133947));
#24638=CARTESIAN_POINT('Ctrl Pts',(42.9219665441837,37.0038755334002,49.8571826228401));
#24639=CARTESIAN_POINT('Ctrl Pts',(42.9275621161994,37.0042562870459,49.8556008686084));
#24640=CARTESIAN_POINT('Ctrl Pts',(42.9430257522519,37.0053059552818,49.8511540112982));
#24641=CARTESIAN_POINT('Ctrl Pts',(42.9528783804659,37.0059718535566,49.8482352796313));
#24642=CARTESIAN_POINT('Ctrl Pts',(43.0064975001434,37.009582307764,49.8318840655602));
#24643=CARTESIAN_POINT('Ctrl Pts',(43.0498023112808,37.0124493275329,49.8169744512251));
#24644=CARTESIAN_POINT('Ctrl Pts',(43.256970262587,37.0261108048817,49.7372915811473));
#24645=CARTESIAN_POINT('Ctrl Pts',(43.4119677859631,37.0362407854834,49.6518202102932));
#24646=CARTESIAN_POINT('Ctrl Pts',(43.5968909569512,37.0504280829964,49.5139228794145));
#24647=CARTESIAN_POINT('Ctrl Pts',(43.6391609562452,37.0538320189597,49.4795234811528));
#24648=CARTESIAN_POINT('Ctrl Pts',(43.6915296575464,37.0582985695638,49.4330857017385));
#24649=CARTESIAN_POINT('Ctrl Pts',(43.7030181820937,37.0592946991623,49.422647911177));
#24650=CARTESIAN_POINT('Ctrl Pts',(43.7214741274392,37.0609224030172,49.4054688321503));
#24651=CARTESIAN_POINT('Ctrl Pts',(43.728519034571,37.0615503847009,49.3988115229383));
#24652=CARTESIAN_POINT('Ctrl Pts',(43.7419810344977,37.0627634809693,49.3858967456898));
#24653=CARTESIAN_POINT('Ctrl Pts',(43.7484052881546,37.0633482474514,49.3796470784079));
#24654=CARTESIAN_POINT('Ctrl Pts',(43.7630609656262,37.0646959769885,49.3651895409924));
#24655=CARTESIAN_POINT('Ctrl Pts',(43.7712621512257,37.0654602568066,49.3569516503467));
#24656=CARTESIAN_POINT('Ctrl Pts',(43.7966406006525,37.0678575088682,49.3309945921986));
#24657=CARTESIAN_POINT('Ctrl Pts',(43.8135520596582,37.0695019057727,49.3130202017218));
#24658=CARTESIAN_POINT('Ctrl Pts',(43.9256237062896,37.0807280782194,49.1892295018467));
#24659=CARTESIAN_POINT('Ctrl Pts',(44.0091501720827,37.0907935804863,49.0735063237269));
#24660=CARTESIAN_POINT('Ctrl Pts',(44.1192965609647,37.1067772291639,48.878750262007));
#24661=CARTESIAN_POINT('Ctrl Pts',(44.154879051092,37.1126032493256,48.8053469019537));
#24662=CARTESIAN_POINT('Ctrl Pts',(44.1953884290047,37.1200577004435,48.7062412737482));
#24663=CARTESIAN_POINT('Ctrl Pts',(44.2045918771911,37.1218219853662,48.6823815916965));
#24664=CARTESIAN_POINT('Ctrl Pts',(44.2192922108447,37.1247573763274,48.6418915803677));
#24665=CARTESIAN_POINT('Ctrl Pts',(44.2250417918035,37.1259398830866,48.6253570665403));
#24666=CARTESIAN_POINT('Ctrl Pts',(44.2328119474277,37.1275860577485,48.6019913548318));
#24667=CARTESIAN_POINT('Ctrl Pts',(44.2350207761071,37.1280599014165,48.5952243116268));
#24668=CARTESIAN_POINT('Ctrl Pts',(44.2387412432922,37.1288680940063,48.5836085917102));
#24669=CARTESIAN_POINT('Ctrl Pts',(44.2402712714225,37.1292035001485,48.5787659269039));
#24670=CARTESIAN_POINT('Ctrl Pts',(44.2432109231775,37.1298538446012,48.5693321638626));
#24671=CARTESIAN_POINT('Ctrl Pts',(44.2446225388257,37.1301689069782,48.5647418088313));
#24672=CARTESIAN_POINT('Ctrl Pts',(44.2484449432028,37.1310298430793,48.5521446976991));
#24673=CARTESIAN_POINT('Ctrl Pts',(44.2508208749326,37.1315737198112,48.5441273476092));
#24674=CARTESIAN_POINT('Ctrl Pts',(44.2599107675537,37.1336903457472,48.5127058686927));
#24675=CARTESIAN_POINT('Ctrl Pts',(44.2662338646827,37.1352421570881,48.4891898049213));
#24676=CARTESIAN_POINT('Ctrl Pts',(44.3090381727509,37.1464090212368,48.3170647232475));
#24677=CARTESIAN_POINT('Ctrl Pts',(44.328171925458,37.1552965366678,48.1646866814955));
#24678=CARTESIAN_POINT('Ctrl Pts',(44.3296338122186,37.1698679015916,47.9222736510853));
#24679=CARTESIAN_POINT('Ctrl Pts',(44.3239631914961,37.1753198616714,47.8329943418672));
#24680=CARTESIAN_POINT('Ctrl Pts',(44.3090400614135,37.1824383753172,47.7213396978242));
#24681=CARTESIAN_POINT('Ctrl Pts',(44.3055350598471,37.1839229979152,47.6983021695107));
#24682=CARTESIAN_POINT('Ctrl Pts',(44.2997094343599,37.1861481075846,47.664180616244));
#24683=CARTESIAN_POINT('Ctrl Pts',(44.2977070429041,37.186878513836,47.6530438589525));
#24684=CARTESIAN_POINT('Ctrl Pts',(44.2939553795354,37.1881888307152,47.6331829647005));
#24685=CARTESIAN_POINT('Ctrl Pts',(44.292243492506,37.1887675334921,47.6244520301376));
#24686=CARTESIAN_POINT('Ctrl Pts',(44.2884894182793,37.1899975163054,47.6059831623475));
#24687=CARTESIAN_POINT('Ctrl Pts',(44.286432173291,37.1906492636461,47.5962485906201));
#24688=CARTESIAN_POINT('Ctrl Pts',(44.2807206618891,37.1924014188702,47.5702195847155));
#24689=CARTESIAN_POINT('Ctrl Pts',(44.2769300381581,37.1935061712577,47.5539562630075));
#24690=CARTESIAN_POINT('Ctrl Pts',(44.2583395928054,37.1986706530152,47.4786330029873));
#24691=CARTESIAN_POINT('Ctrl Pts',(44.2409616301131,37.2028124663578,47.4202513614452));
#24692=CARTESIAN_POINT('Ctrl Pts',(44.1736034541804,37.2169419470818,47.2277713336924));
#24693=CARTESIAN_POINT('Ctrl Pts',(44.1114826442367,37.2272698071009,47.0984318150873));
#24694=CARTESIAN_POINT('Ctrl Pts',(44.0107973237218,37.2407295459482,46.9374220286937));
#24695=CARTESIAN_POINT('Ctrl Pts',(43.9845010624469,37.244022918802,46.8985932038399));
#24696=CARTESIAN_POINT('Ctrl Pts',(43.9408598025008,37.2491159395384,46.8389558381092));
#24697=CARTESIAN_POINT('Ctrl Pts',(43.9244477134863,37.2509566001855,46.8174891852747));
#24698=CARTESIAN_POINT('Ctrl Pts',(43.9023515033295,37.2533321242968,46.7898128297121));
#24699=CARTESIAN_POINT('Ctrl Pts',(43.8970710243374,37.2538924591732,46.7832866479017));
#24700=CARTESIAN_POINT('Ctrl Pts',(43.888362451477,37.2548043296976,46.7726661909366));
#24701=CARTESIAN_POINT('Ctrl Pts',(43.8849597304916,37.2551576260458,46.7685513951476));
#24702=CARTESIAN_POINT('Ctrl Pts',(43.8782734686682,37.2558459163128,46.7605339377026));
#24703=CARTESIAN_POINT('Ctrl Pts',(43.8749914751714,37.256181009304,46.7566300965399));
#24704=CARTESIAN_POINT('Ctrl Pts',(43.8676165605556,37.2569279671385,46.7479281327418));
#24705=CARTESIAN_POINT('Ctrl Pts',(43.8635154762454,37.2573392412833,46.7431369274583));
#24706=CARTESIAN_POINT('Ctrl Pts',(43.8491985152274,37.2587612140411,46.7265758329303));
#24707=CARTESIAN_POINT('Ctrl Pts',(43.8388632413289,37.259763596078,46.7149093200139));
#24708=CARTESIAN_POINT('Ctrl Pts',(43.7431381137568,37.2688441759801,46.609457153374));
#24709=CARTESIAN_POINT('Ctrl Pts',(43.6488223123056,37.2763497065289,46.5241675166809));
#24710=CARTESIAN_POINT('Ctrl Pts',(43.4865640938745,37.2883866339599,46.4042139931791));
#24711=CARTESIAN_POINT('Ctrl Pts',(43.423784525815,37.2928638526135,46.3632291252425));
#24712=CARTESIAN_POINT('Ctrl Pts',(43.3030395794736,37.3013667031375,46.2940724315528));
#24713=CARTESIAN_POINT('Ctrl Pts',(43.2457405536162,37.3053598864243,46.2649521753635));
#24714=CARTESIAN_POINT('Ctrl Pts',(43.1721824553614,37.310495361995,46.2320792465237));
#24715=CARTESIAN_POINT('Ctrl Pts',(43.1571811669382,37.3115430235403,46.2256025842955));
#24716=CARTESIAN_POINT('Ctrl Pts',(43.1329882111123,37.3132340284976,46.2155201656794));
#24717=CARTESIAN_POINT('Ctrl Pts',(43.1238477732688,37.3138732320851,46.2117929672905));
#24718=CARTESIAN_POINT('Ctrl Pts',(43.1064002885805,37.3150941544965,46.2048340928264));
#24719=CARTESIAN_POINT('Ctrl Pts',(43.098098639228,37.3156754185127,46.2015895108764));
#24720=CARTESIAN_POINT('Ctrl Pts',(43.0790768763525,37.3170082034382,46.1943066767072));
#24721=CARTESIAN_POINT('Ctrl Pts',(43.0683427643728,37.3177609680659,46.1903061801944));
#24722=CARTESIAN_POINT('Ctrl Pts',(43.0349772913259,37.320103237105,46.1782085390536));
#24723=CARTESIAN_POINT('Ctrl Pts',(43.0122304994892,37.3217035113785,46.1704388465869));
#24724=CARTESIAN_POINT('Ctrl Pts',(42.841747099017,37.333727869541,46.1157415837748));
#24725=CARTESIAN_POINT('Ctrl Pts',(42.6890058690732,37.3447388992426,46.0863575198811));
#24726=CARTESIAN_POINT('Ctrl Pts',(42.4616007185982,37.3610206129566,46.0704719933373));
#24727=CARTESIAN_POINT('Ctrl Pts',(42.3885338187064,37.3662228527457,46.0695226495647));
#24728=CARTESIAN_POINT('Ctrl Pts',(42.2916156436767,37.3729641635258,46.0737676599795));
#24729=CARTESIAN_POINT('Ctrl Pts',(42.2676666149053,37.3746167797358,46.0752646458915));
#24730=CARTESIAN_POINT('Ctrl Pts',(42.2271184787695,37.3773858671642,46.078559656993));
#24731=CARTESIAN_POINT('Ctrl Pts',(42.2105038604399,37.3785122235328,46.0801270168205));
#24732=CARTESIAN_POINT('Ctrl Pts',(42.1869668740035,37.3800941725693,46.0826559459354));
#24733=CARTESIAN_POINT('Ctrl Pts',(42.1800267192449,37.380558934833,46.0834397755508));
#24734=CARTESIAN_POINT('Ctrl Pts',(42.1680698577809,37.3813565530821,46.0848560028054));
#24735=CARTESIAN_POINT('Ctrl Pts',(42.1630511434674,37.3816903957373,46.0854704591711));
#24736=CARTESIAN_POINT('Ctrl Pts',(42.152538837011,37.3823876265515,46.0867994831837));
#24737=CARTESIAN_POINT('Ctrl Pts',(42.1470458569659,37.3827507931034,46.0875179874896));
#24738=CARTESIAN_POINT('Ctrl Pts',(42.1323389165952,37.3837202220535,46.0895061874315));
#24739=CARTESIAN_POINT('Ctrl Pts',(42.1231307760607,37.3843241203496,46.0908188915755));
#24740=CARTESIAN_POINT('Ctrl Pts',(42.0819255196667,37.387014183275,46.096997465374));
#24741=CARTESIAN_POINT('Ctrl Pts',(42.0500423607073,37.3890623831829,46.1026017908161));
#24742=CARTESIAN_POINT('Ctrl Pts',(41.879595587157,37.3999057214379,46.1370055445229));
#24743=CARTESIAN_POINT('Ctrl Pts',(41.7443670970048,37.4081552299275,46.18018606003));
#24744=CARTESIAN_POINT('Ctrl Pts',(41.5322156671077,37.4221077569098,46.2746827502607));
#24745=CARTESIAN_POINT('Ctrl Pts',(41.4520770664198,37.4276372464387,46.3173804648249));
#24746=CARTESIAN_POINT('Ctrl Pts',(41.3553568345844,37.4348498628924,46.3780215173));
#24747=CARTESIAN_POINT('Ctrl Pts',(41.3356993450523,37.4363452071428,46.3908519083714));
#24748=CARTESIAN_POINT('Ctrl Pts',(41.3068931453071,37.4385832960766,46.4104123981866));
#24749=CARTESIAN_POINT('Ctrl Pts',(41.2975613844119,37.4393157839426,46.4168700529033));
#24750=CARTESIAN_POINT('Ctrl Pts',(41.2810130791843,37.4406284072515,46.4285388798066));
#24751=CARTESIAN_POINT('Ctrl Pts',(41.2737745456599,37.4412073182274,46.4337184152365));
#24752=CARTESIAN_POINT('Ctrl Pts',(41.2585364198354,37.4424362388853,46.4447823085724));
#24753=CARTESIAN_POINT('Ctrl Pts',(41.250545925606,37.4430867050916,46.4506786978925));
#24754=CARTESIAN_POINT('Ctrl Pts',(41.229311625625,37.4448317615975,46.4666027151973));
#24755=CARTESIAN_POINT('Ctrl Pts',(41.2161514654952,37.4459306352323,46.4767399694097));
#24756=CARTESIAN_POINT('Ctrl Pts',(41.1566781457875,37.4509779809276,46.5237884324047));
#24757=CARTESIAN_POINT('Ctrl Pts',(41.1119533659701,37.455003807069,46.5626467307444));
#24758=CARTESIAN_POINT('Ctrl Pts',(40.9512944671883,37.4703651482437,46.7157595434215));
#24759=CARTESIAN_POINT('Ctrl Pts',(40.8481814416517,37.4821848649888,46.8424728567648));
#24760=CARTESIAN_POINT('Ctrl Pts',(40.7435926760575,37.4961011672469,47.0105057331523));
#24761=CARTESIAN_POINT('Ctrl Pts',(40.7257949091819,37.498554993609,47.0409266241879));
#24762=CARTESIAN_POINT('Ctrl Pts',(40.6981867638974,37.5024882830913,47.0912291418198));
#24763=CARTESIAN_POINT('Ctrl Pts',(40.6878684074296,37.5039905798036,47.1108215721562));
#24764=CARTESIAN_POINT('Ctrl Pts',(40.6743742013247,37.5059960368236,47.1375505882188));
#24765=CARTESIAN_POINT('Ctrl Pts',(40.6709014564426,37.5065160093268,47.1445342690819));
#24766=CARTESIAN_POINT('Ctrl Pts',(40.6651793750562,37.5073790655705,47.1562185669369));
#24767=CARTESIAN_POINT('Ctrl Pts',(40.6629065911517,37.5077235715462,47.1609075150205));
#24768=CARTESIAN_POINT('Ctrl Pts',(40.6586409192041,37.5083733290271,47.1697995754708));
#24769=CARTESIAN_POINT('Ctrl Pts',(40.6566441926893,37.5086788239434,47.1740007727454));
#24770=CARTESIAN_POINT('Ctrl Pts',(40.6519548226461,37.5093996002311,47.18396015989));
#24771=CARTESIAN_POINT('Ctrl Pts',(40.6492753847375,37.5098140753305,47.1897245610128));
#24772=CARTESIAN_POINT('Ctrl Pts',(40.6400035175406,37.5112579908241,47.209932279821));
#24773=CARTESIAN_POINT('Ctrl Pts',(40.6335607236798,37.5122787737353,47.2244441070733));
#24774=CARTESIAN_POINT('Ctrl Pts',(40.5793011709017,37.5210448826691,47.3508440891409));
#24775=CARTESIAN_POINT('Ctrl Pts',(40.5419836366834,37.5282657885556,47.4669604383437));
#24776=CARTESIAN_POINT('Ctrl Pts',(40.4859803649962,37.5438238508871,47.721732834052));
#24777=CARTESIAN_POINT('Ctrl Pts',(40.4709013140451,37.5521462336006,47.8604462285944));
#24778=CARTESIAN_POINT('Ctrl Pts',(40.470866204085,37.562069016386,48.0166737762658));
#24779=CARTESIAN_POINT('Ctrl Pts',(40.4710899182901,37.563162280457,48.0337799347538));
#24780=CARTESIAN_POINT('Ctrl Pts',(40.4718319635774,37.5649719579374,48.0619047739402));
#24781=CARTESIAN_POINT('Ctrl Pts',(40.4722173529074,37.5656842098326,48.0729262294255));
#24782=CARTESIAN_POINT('Ctrl Pts',(40.4730831965717,37.5669747231676,48.092805566662));
#24783=CARTESIAN_POINT('Ctrl Pts',(40.4735302922043,37.5675519215008,48.1016646500113));
#24784=CARTESIAN_POINT('Ctrl Pts',(40.4746190292379,37.5687926765634,48.120637339368));
#24785=CARTESIAN_POINT('Ctrl Pts',(40.4752792944777,37.5694568021974,48.1307495670864));
#24786=CARTESIAN_POINT('Ctrl Pts',(40.4773003618044,37.5712777813411,48.1583557450754));
#24787=CARTESIAN_POINT('Ctrl Pts',(40.4788201922457,37.572439591095,48.1758367203876));
#24788=CARTESIAN_POINT('Ctrl Pts',(40.4889616628486,37.5791848325426,48.2765421453077));
#24789=CARTESIAN_POINT('Ctrl Pts',(40.5027507964943,37.584929520007,48.3591449415101));
#24790=CARTESIAN_POINT('Ctrl Pts',(40.5470819389444,37.5985471708437,48.5481226780583));
#24791=CARTESIAN_POINT('Ctrl Pts',(40.581498171747,37.606494200744,48.653293396967));
#24792=CARTESIAN_POINT('Ctrl Pts',(40.6545761214094,37.619765989015,48.8251416705001));
#24793=CARTESIAN_POINT('Ctrl Pts',(40.688574760283,37.6251258515477,48.8935265141757));
#24794=CARTESIAN_POINT('Ctrl Pts',(40.7317306331961,37.6309827355547,48.9687769510339));
#24795=CARTESIAN_POINT('Ctrl Pts',(40.7369958179616,37.6316833069803,48.9777875860359));
#24796=CARTESIAN_POINT('Ctrl Pts',(40.7456142923333,37.6328072367718,48.9922658989641));
#24797=CARTESIAN_POINT('Ctrl Pts',(40.7489220967485,37.6332333407615,48.9977602138346));
#24798=CARTESIAN_POINT('Ctrl Pts',(40.7548493973254,37.6339874617808,49.0074953574341));
#24799=CARTESIAN_POINT('Ctrl Pts',(40.7574579936243,37.6343161657963,49.0117426352487));
#24800=CARTESIAN_POINT('Ctrl Pts',(40.7631694910493,37.6350289582747,49.0209616965136));
#24801=CARTESIAN_POINT('Ctrl Pts',(40.7662785985618,37.6354126337587,49.025929473948));
#24802=CARTESIAN_POINT('Ctrl Pts',(40.7751669443698,37.6364974920067,49.0399885315531));
#24803=CARTESIAN_POINT('Ctrl Pts',(40.7809998711022,37.6371952453438,49.0490458522051));
#24804=CARTESIAN_POINT('Ctrl Pts',(40.8212636661896,37.6419198081871,49.1104313573072));
#24805=CARTESIAN_POINT('Ctrl Pts',(40.8581534444709,37.645798710245,49.161110312538));
#24806=CARTESIAN_POINT('Ctrl Pts',(40.9771058465114,37.6573317871873,49.3088339244236));
#24807=CARTESIAN_POINT('Ctrl Pts',(41.0663394920247,37.6647602575618,49.3996520877434));
#24808=CARTESIAN_POINT('Ctrl Pts',(41.2262347611737,37.6773613220463,49.533107857091));
#24809=CARTESIAN_POINT('Ctrl Pts',(41.2918344186456,37.6823645119123,49.5811739932347));
#24810=CARTESIAN_POINT('Ctrl Pts',(41.3752779205529,37.6886642557149,49.6345656772653));
#24811=CARTESIAN_POINT('Ctrl Pts',(41.3904245530283,37.6898051166411,49.6439640130144));
#24812=CARTESIAN_POINT('Ctrl Pts',(41.4145240807677,37.6916172890748,49.6584588717224));
#24813=CARTESIAN_POINT('Ctrl Pts',(41.4233915308754,37.692283441564,49.66369603828));
#24814=CARTESIAN_POINT('Ctrl Pts',(41.4399621205037,37.693527314986,49.6733045949206));
#24815=CARTESIAN_POINT('Ctrl Pts',(41.447654286415,37.6941043463257,49.6776944402528));
#24816=CARTESIAN_POINT('Ctrl Pts',(41.4648024645625,37.6953900229255,49.6873248064568));
#24817=CARTESIAN_POINT('Ctrl Pts',(41.474272793011,37.6960995878142,49.6925390875579));
#24818=CARTESIAN_POINT('Ctrl Pts',(41.5020541806685,37.6981800369615,49.7075323649935));
#24819=CARTESIAN_POINT('Ctrl Pts',(41.5204793775371,37.6995585026626,49.7170954804915));
#24820=CARTESIAN_POINT('Ctrl Pts',(41.6093901956069,37.7062063178128,49.7614358209183));
#24821=CARTESIAN_POINT('Ctrl Pts',(41.6817944141776,37.7116125554173,49.7921768662197));
#24822=CARTESIAN_POINT('Ctrl Pts',(41.768578352681,37.7180730212865,49.8229183237142));
#24823=CARTESIAN_POINT('Ctrl Pts',(41.7813375499239,37.7190222414624,49.8272879181221));
#24824=CARTESIAN_POINT('Ctrl Pts',(41.7941388718785,37.7199737694749,49.8315225497742));
#24825=CARTESIAN_POINT('Ctrl Pts',(41.7941388317907,37.8901046061668,49.8315225365133));
#24826=CARTESIAN_POINT('Ctrl Pts',(41.7936175134844,37.8900672581426,49.831350086264));
#24827=CARTESIAN_POINT('Ctrl Pts',(41.7930962673079,37.8900299203585,49.8311774129395));
#24828=CARTESIAN_POINT('Ctrl Pts',(41.7775906461537,37.8889193776992,49.8260335149338));
#24829=CARTESIAN_POINT('Ctrl Pts',(41.7626671831116,37.8878547612407,49.8208785575848));
#24830=CARTESIAN_POINT('Ctrl Pts',(41.741380515005,37.8863439509835,49.8132318043135));
#24831=CARTESIAN_POINT('Ctrl Pts',(41.7349651065048,37.8858896374652,49.8108886758016));
#24832=CARTESIAN_POINT('Ctrl Pts',(41.7238455115517,37.8851041279316,49.8067603542927));
#24833=CARTESIAN_POINT('Ctrl Pts',(41.7191356651461,37.8847720256459,49.8049907562126));
#24834=CARTESIAN_POINT('Ctrl Pts',(41.7091904720039,37.8840721107104,49.8012096506244));
#24835=CARTESIAN_POINT('Ctrl Pts',(41.7039569347537,37.8837045639093,49.7991937257514));
#24836=CARTESIAN_POINT('Ctrl Pts',(41.6897736712279,37.8827103990024,49.7936592746756));
#24837=CARTESIAN_POINT('Ctrl Pts',(41.6808411984499,37.8820863599445,49.7900965502503));
#24838=CARTESIAN_POINT('Ctrl Pts',(41.6387554072491,37.8791543059777,49.7729447258289));
#24839=CARTESIAN_POINT('Ctrl Pts',(41.6059559311538,37.8768931595464,49.7584995689046));
#24840=CARTESIAN_POINT('Ctrl Pts',(41.5409849409625,37.8724257336572,49.7276968973652));
#24841=CARTESIAN_POINT('Ctrl Pts',(41.508832473336,37.8702208021449,49.7113340211458));
#24842=CARTESIAN_POINT('Ctrl Pts',(41.3745965089642,37.8609637208791,49.6382094170411));
#24843=CARTESIAN_POINT('Ctrl Pts',(41.2773210319681,37.8541116161374,49.5731419845162));
#24844=CARTESIAN_POINT('Ctrl Pts',(41.1204299356666,37.8419166407192,49.4461922574094));
#24845=CARTESIAN_POINT('Ctrl Pts',(41.0579494871242,37.8366872741337,49.3884053180214));
#24846=CARTESIAN_POINT('Ctrl Pts',(40.9873772697403,37.8301577496872,49.3139062785321));
#24847=CARTESIAN_POINT('Ctrl Pts',(40.9754422334157,37.8290300671449,49.3009565032879));
#24848=CARTESIAN_POINT('Ctrl Pts',(40.9569133932338,37.8272408249234,49.2802915832768));
#24849=CARTESIAN_POINT('Ctrl Pts',(40.9502001268667,37.8265843178307,49.27268449121));
#24850=CARTESIAN_POINT('Ctrl Pts',(40.9377333252335,37.8253493754633,49.258331171475));
#24851=CARTESIAN_POINT('Ctrl Pts',(40.9319656657561,37.8247715494766,49.2515975208875));
#24852=CARTESIAN_POINT('Ctrl Pts',(40.9191442527848,37.8234722462379,49.2364181714709));
#24853=CARTESIAN_POINT('Ctrl Pts',(40.9121159791754,37.822749751237,49.2279514529624));
#24854=CARTESIAN_POINT('Ctrl Pts',(40.8943943429978,37.8209013255124,49.2062272842276));
#24855=CARTESIAN_POINT('Ctrl Pts',(40.8838036056596,37.819771326238,49.1928877221357));
#24856=CARTESIAN_POINT('Ctrl Pts',(40.8072578045933,37.8114126496384,49.0938081038673));
#24857=CARTESIAN_POINT('Ctrl Pts',(40.7484527297161,37.8039060341859,49.0028102373976));
#24858=CARTESIAN_POINT('Ctrl Pts',(40.6289008794188,37.7858878480136,48.778508882103));
#24859=CARTESIAN_POINT('Ctrl Pts',(40.5750673597407,37.7752855007878,48.642255024258));
#24860=CARTESIAN_POINT('Ctrl Pts',(40.5316112131668,37.7638334714754,48.4807451187842));
#24861=CARTESIAN_POINT('Ctrl Pts',(40.5264376966115,37.762395343422,48.4601705282495));
#24862=CARTESIAN_POINT('Ctrl Pts',(40.5198565498977,37.7604612543522,48.4320439980544));
#24863=CARTESIAN_POINT('Ctrl Pts',(40.5181532817463,37.7599499339563,48.424563709172));
#24864=CARTESIAN_POINT('Ctrl Pts',(40.5153740867943,37.7590973473114,48.4120128493432));
#24865=CARTESIAN_POINT('Ctrl Pts',(40.5142739044657,37.7587547279642,48.406947804326));
#24866=CARTESIAN_POINT('Ctrl Pts',(40.5122208635655,37.7581055481189,48.3973088421006));
#24867=CARTESIAN_POINT('Ctrl Pts',(40.5112641889311,37.7577987643148,48.3927358159358));
#24868=CARTESIAN_POINT('Ctrl Pts',(40.5090280110873,37.7570712177177,48.381849431554));
#24869=CARTESIAN_POINT('Ctrl Pts',(40.507763487663,37.7566512987757,48.3755330018968));
#24870=CARTESIAN_POINT('Ctrl Pts',(40.5033939069377,37.7551689868781,48.3531239072154));
#24871=CARTESIAN_POINT('Ctrl Pts',(40.5004622076336,37.7541158676232,48.336997602995));
#24872=CARTESIAN_POINT('Ctrl Pts',(40.4799570430327,37.746265020802,48.2154204695495));
#24873=CARTESIAN_POINT('Ctrl Pts',(40.4709685654758,37.7398674548764,48.1086955161729));
#24874=CARTESIAN_POINT('Ctrl Pts',(40.4707395022945,37.7249146031399,47.8581397620656));
#24875=CARTESIAN_POINT('Ctrl Pts',(40.4866464982344,37.7163916848305,47.7149681425424));
#24876=CARTESIAN_POINT('Ctrl Pts',(40.5237838102496,37.7057607332682,47.5505819330389));
#24877=CARTESIAN_POINT('Ctrl Pts',(40.5297466586376,37.70417471704,47.5263797537508));
#24878=CARTESIAN_POINT('Ctrl Pts',(40.5391420010776,37.7018352851868,47.4911953330941));
#24879=CARTESIAN_POINT('Ctrl Pts',(40.5422066360675,37.7010937434822,47.480116850894));
#24880=CARTESIAN_POINT('Ctrl Pts',(40.5478308879236,37.6997696252662,47.460470495555));
#24881=CARTESIAN_POINT('Ctrl Pts',(40.5503514359761,37.6991883366205,47.4518917160081));
#24882=CARTESIAN_POINT('Ctrl Pts',(40.5557446033393,37.6979691608629,47.4339967953654));
#24883=CARTESIAN_POINT('Ctrl Pts',(40.5586283793337,37.6973309219276,47.4246843088805));
#24884=CARTESIAN_POINT('Ctrl Pts',(40.5663667595188,37.6956529728556,47.4003493235536));
#24885=CARTESIAN_POINT('Ctrl Pts',(40.5713353238868,37.6946095384393,47.3853641147973));
#24886=CARTESIAN_POINT('Ctrl Pts',(40.5952411834719,37.6897395073416,47.3161208694104));
#24887=CARTESIAN_POINT('Ctrl Pts',(40.6164112624952,37.6858396957832,47.2626702934077));
#24888=CARTESIAN_POINT('Ctrl Pts',(40.6865238166123,37.6740083304901,47.1064150892322));
#24889=CARTESIAN_POINT('Ctrl Pts',(40.7422069308834,37.665881784329,47.0069182001163));
#24890=CARTESIAN_POINT('Ctrl Pts',(40.8326518509076,37.6544198064664,46.8743246238609));
#24891=CARTESIAN_POINT('Ctrl Pts',(40.8603728648284,37.6510899440287,46.8366970210532));
#24892=CARTESIAN_POINT('Ctrl Pts',(40.924688540041,37.6437993726581,46.7557285390511));
#24893=CARTESIAN_POINT('Ctrl Pts',(40.961886439201,37.6398586607133,46.7129156694088));
#24894=CARTESIAN_POINT('Ctrl Pts',(41.00775342733,37.6353654466197,46.6646009745871));
#24895=CARTESIAN_POINT('Ctrl Pts',(41.0146428686088,37.6346996604662,46.6574551385845));
#24896=CARTESIAN_POINT('Ctrl Pts',(41.0259664720512,37.6336205835688,46.645890107438));
#24897=CARTESIAN_POINT('Ctrl Pts',(41.0303674296514,37.6332048791198,46.6414388633405));
#24898=CARTESIAN_POINT('Ctrl Pts',(41.0383039207166,37.6324619250366,46.6334894514279));
#24899=CARTESIAN_POINT('Ctrl Pts',(41.0418313758721,37.6321340693116,46.6299834738834));
#24900=CARTESIAN_POINT('Ctrl Pts',(41.0496283056739,37.6314145668222,46.6222937273982));
#24901=CARTESIAN_POINT('Ctrl Pts',(41.0539036840771,37.6310233985328,46.6181161419839));
#24902=CARTESIAN_POINT('Ctrl Pts',(41.0663395786764,37.6298950464938,46.6060771796823));
#24903=CARTESIAN_POINT('Ctrl Pts',(41.074550192666,37.6291617406367,46.5982675820099));
#24904=CARTESIAN_POINT('Ctrl Pts',(41.1428721001029,37.6231504363752,46.5344197209621));
#24905=CARTESIAN_POINT('Ctrl Pts',(41.206447132777,37.6181282114454,46.4821952781277));
#24906=CARTESIAN_POINT('Ctrl Pts',(41.2800162989781,37.6126734931055,46.4292516873316));
#24907=CARTESIAN_POINT('Ctrl Pts',(41.2868972695629,37.6121665814886,46.4243680425329));
#24908=CARTESIAN_POINT('Ctrl Pts',(41.4153981859246,37.6027565893435,46.3344287290135));
#24909=CARTESIAN_POINT('Ctrl Pts',(41.5463907047871,37.5940538132914,46.263648288005));
#24910=CARTESIAN_POINT('Ctrl Pts',(41.719954421196,37.5824224106004,46.1942970769385));
#24911=CARTESIAN_POINT('Ctrl Pts',(41.7561263990339,37.5799963032222,46.1810850749619));
#24912=CARTESIAN_POINT('Ctrl Pts',(41.8061235608414,37.5766279050356,46.1645016169033));
#24913=CARTESIAN_POINT('Ctrl Pts',(41.8196279948348,37.5757166446797,46.1601870047517));
#24914=CARTESIAN_POINT('Ctrl Pts',(41.8412670820739,37.5742536320947,46.1535353534401));
#24915=CARTESIAN_POINT('Ctrl Pts',(41.8493718578679,37.5737050407088,46.151102271662));
#24916=CARTESIAN_POINT('Ctrl Pts',(41.8661105023714,37.5725706213813,46.1461970942401));
#24917=CARTESIAN_POINT('Ctrl Pts',(41.8747461367017,37.5719845865806,46.1437318125979));
#24918=CARTESIAN_POINT('Ctrl Pts',(41.8949206400934,37.5706135382331,46.1381244908785));
#24919=CARTESIAN_POINT('Ctrl Pts',(41.9064720342812,37.5698270241417,46.1350293012116));
#24920=CARTESIAN_POINT('Ctrl Pts',(41.9440074348758,37.5672660839849,46.1253448556922));
#24921=CARTESIAN_POINT('Ctrl Pts',(41.970099211458,37.5654777867601,46.1191899834915));
#24922=CARTESIAN_POINT('Ctrl Pts',(42.0321655376173,37.5612026386333,46.1059078997389));
#24923=CARTESIAN_POINT('Ctrl Pts',(42.0682307381263,37.5587016719349,46.0992591088863));
#24924=CARTESIAN_POINT('Ctrl Pts',(42.2091978696957,37.5488617276344,46.0774052850129));
#24925=CARTESIAN_POINT('Ctrl Pts',(42.3150834827794,37.5413194780256,46.0698288971812));
#24926=CARTESIAN_POINT('Ctrl Pts',(42.525959346993,37.5262536441428,46.0721292676597));
#24927=CARTESIAN_POINT('Ctrl Pts',(42.6306178711824,37.5187576441944,46.081831348923));
#24928=CARTESIAN_POINT('Ctrl Pts',(42.7501625820139,37.5104944031991,46.10284454583));
#24929=CARTESIAN_POINT('Ctrl Pts',(42.7663126206386,37.5093847316243,46.1058965816952));
#24930=CARTESIAN_POINT('Ctrl Pts',(42.7887434953279,37.5078546165903,46.1104332127845));
#24931=CARTESIAN_POINT('Ctrl Pts',(42.7950583252172,37.5074250849347,46.1117433778411));
#24932=CARTESIAN_POINT('Ctrl Pts',(42.8059381656325,37.506687310305,46.1140576340681));
#24933=CARTESIAN_POINT('Ctrl Pts',(42.8105062667067,37.50637823307,46.1150466827802));
#24934=CARTESIAN_POINT('Ctrl Pts',(42.8201303920262,37.505728589119,46.1171670672088));
#24935=CARTESIAN_POINT('Ctrl Pts',(42.8251855330876,37.5053882521536,46.1183021861466));
#24936=CARTESIAN_POINT('Ctrl Pts',(42.8377042526321,37.5045475089004,46.121166256214));
#24937=CARTESIAN_POINT('Ctrl Pts',(42.8451623214394,37.5040484678945,46.1229193512287));
#24938=CARTESIAN_POINT('Ctrl Pts',(42.8731574200033,37.5021814562977,46.1296761222987));
#24939=CARTESIAN_POINT('Ctrl Pts',(42.8936230707684,37.5008292029739,46.1349730016387));
#24940=CARTESIAN_POINT('Ctrl Pts',(43.0533899702802,37.4903421419444,46.1791378891239));
#24941=CARTESIAN_POINT('Ctrl Pts',(43.1880250547904,37.4818946920488,46.2332274868453));
#24942=CARTESIAN_POINT('Ctrl Pts',(43.4118692999527,37.4666676403285,46.353888520676));
#24943=CARTESIAN_POINT('Ctrl Pts',(43.5037536390697,37.4600110566575,46.4140347763983));
#24944=CARTESIAN_POINT('Ctrl Pts',(43.6034428752972,37.4519655766891,46.4921676617587));
#24945=CARTESIAN_POINT('Ctrl Pts',(43.616718643532,37.4508761759025,46.5028597837532));
#24946=CARTESIAN_POINT('Ctrl Pts',(43.6383314795768,37.4490716922599,46.5207438100603));
#24947=CARTESIAN_POINT('Ctrl Pts',(43.6467519383969,37.4483607310096,46.5278337985858));
#24948=CARTESIAN_POINT('Ctrl Pts',(43.6618443988954,37.4470717587842,46.5407639383377));
#24949=CARTESIAN_POINT('Ctrl Pts',(43.6685377356452,37.4464948016611,46.5465788017551));
#24950=CARTESIAN_POINT('Ctrl Pts',(43.682801521875,37.4452536822939,46.5591441122663));
#24951=CARTESIAN_POINT('Ctrl Pts',(43.69035926602,37.4445889449673,46.5659085134983));
#24952=CARTESIAN_POINT('Ctrl Pts',(43.7108823808683,37.4427639959479,46.5845708790155));
#24953=CARTESIAN_POINT('Ctrl Pts',(43.7237385882742,37.4415987896344,46.5965869004962));
#24954=CARTESIAN_POINT('Ctrl Pts',(43.7975477872308,37.4347776365027,46.6674890377287));
#24955=CARTESIAN_POINT('Ctrl Pts',(43.8547232309565,37.4289560223963,46.7301566948169));
#24956=CARTESIAN_POINT('Ctrl Pts',(43.9794718063388,37.4149215863325,46.8864088297881));
#24957=CARTESIAN_POINT('Ctrl Pts',(44.0431429491775,37.4066210530261,46.9827021105529));
#24958=CARTESIAN_POINT('Ctrl Pts',(44.1148208351882,37.3959118100115,47.1155727297766));
#24959=CARTESIAN_POINT('Ctrl Pts',(44.1309258246779,37.3933904116179,47.1475223686525));
#24960=CARTESIAN_POINT('Ctrl Pts',(44.1621634790723,37.3882738203714,47.2140329172255));
#24961=CARTESIAN_POINT('Ctrl Pts',(44.1771904329341,37.3856830271622,47.2486285882515));
#24962=CARTESIAN_POINT('Ctrl Pts',(44.1948263426804,37.3824875404477,47.2927259324309));
#24963=CARTESIAN_POINT('Ctrl Pts',(44.1983890263743,37.3818331429623,47.301834456016));
#24964=CARTESIAN_POINT('Ctrl Pts',(44.203898339984,37.3808073683962,47.3162418604289));
#24965=CARTESIAN_POINT('Ctrl Pts',(44.2058911893622,37.3804333456778,47.3215227132426));
#24966=CARTESIAN_POINT('Ctrl Pts',(44.2096131108994,37.3797292204236,47.3315180183997));
#24967=CARTESIAN_POINT('Ctrl Pts',(44.2113469400763,37.3793988548974,47.3362304359815));
#24968=CARTESIAN_POINT('Ctrl Pts',(44.2153714338275,37.3786263606993,47.3473019105476));
#24969=CARTESIAN_POINT('Ctrl Pts',(44.217647103664,37.378185120806,47.3536663023927));
#24970=CARTESIAN_POINT('Ctrl Pts',(44.2249922240706,37.3767458088115,47.3745541099661));
#24971=CARTESIAN_POINT('Ctrl Pts',(44.2299215731768,37.3757555941091,47.3891266486942));
#24972=CARTESIAN_POINT('Ctrl Pts',(44.2562877589714,37.3703115103879,47.4702570380722));
#24973=CARTESIAN_POINT('Ctrl Pts',(44.2742701688066,37.3660275235868,47.5378903571943));
#24974=CARTESIAN_POINT('Ctrl Pts',(44.2953692404926,37.3597885861315,47.639115402867));
#24975=CARTESIAN_POINT('Ctrl Pts',(44.3013438573136,37.357785516413,47.6720459313911));
#24976=CARTESIAN_POINT('Ctrl Pts',(44.3293467788555,37.3468450213011,47.8530878921842));
#24977=CARTESIAN_POINT('Ctrl Pts',(44.334927978243,37.3379856866592,48.003203323262));
#24978=CARTESIAN_POINT('Ctrl Pts',(44.3211599374976,37.3269905122201,48.176883887801));
#24979=CARTESIAN_POINT('Ctrl Pts',(44.3187573750752,37.3254302265982,48.2012795669041));
#24980=CARTESIAN_POINT('Ctrl Pts',(44.314555210387,37.323121750736,48.2369626495734));
#24981=CARTESIAN_POINT('Ctrl Pts',(44.3131190536956,37.3223849834513,48.2482910148551));
#24982=CARTESIAN_POINT('Ctrl Pts',(44.3103806003394,37.3210663081327,48.2684553564751));
#24983=CARTESIAN_POINT('Ctrl Pts',(44.3091173448619,37.32048565043,48.2772963678373));
#24984=CARTESIAN_POINT('Ctrl Pts',(44.3063412809526,37.3192646107851,48.2958060962498));
#24985=CARTESIAN_POINT('Ctrl Pts',(44.3048162004491,37.3186238546289,48.3054726870846));
#24986=CARTESIAN_POINT('Ctrl Pts',(44.3006107914344,37.3169319824356,48.3308713549115));
#24987=CARTESIAN_POINT('Ctrl Pts',(44.2978087273593,37.3158770282695,48.3465822301078));
#24988=CARTESIAN_POINT('Ctrl Pts',(44.2836428882995,37.3108605820911,48.4206778793085));
#24989=CARTESIAN_POINT('Ctrl Pts',(44.2697788671548,37.3068203569583,48.4785458213757));
#24990=CARTESIAN_POINT('Ctrl Pts',(44.2239113359991,37.2953936279628,48.6372326013979));
#24991=CARTESIAN_POINT('Ctrl Pts',(44.186261663696,37.2878570981544,48.7361949094014));
#24992=CARTESIAN_POINT('Ctrl Pts',(44.0974802087398,37.273144194891,48.9220397609233));
#24993=CARTESIAN_POINT('Ctrl Pts',(44.0472662095272,37.2659941472145,49.0090165512006));
#24994=CARTESIAN_POINT('Ctrl Pts',(43.9812032349665,37.2580465122039,49.1052644473512));
#24995=CARTESIAN_POINT('Ctrl Pts',(43.9717204712065,37.2569357584839,49.1187081717325));
#24996=CARTESIAN_POINT('Ctrl Pts',(43.9582805050011,37.2554043957846,49.1372537321468));
#24997=CARTESIAN_POINT('Ctrl Pts',(43.9544682413488,37.2549746800725,49.1424590465889));
#24998=CARTESIAN_POINT('Ctrl Pts',(43.947848957908,37.2542366750473,49.1514026280646));
#24999=CARTESIAN_POINT('Ctrl Pts',(43.9450543629053,37.253927550299,49.1551499579051));
#25000=CARTESIAN_POINT('Ctrl Pts',(43.9391342436043,37.2532779076783,49.1630284482156));
#25001=CARTESIAN_POINT('Ctrl Pts',(43.936005652029,37.2529376189908,49.1671572427157));
#25002=CARTESIAN_POINT('Ctrl Pts',(43.9282112460747,37.2520971650225,49.1773578809224));
#25003=CARTESIAN_POINT('Ctrl Pts',(43.9235257761273,37.2515983629403,49.1834147230486));
#25004=CARTESIAN_POINT('Ctrl Pts',(43.9057880512276,37.2497333132278,49.2060640791116));
#25005=CARTESIAN_POINT('Ctrl Pts',(43.8924992399637,37.2483827402351,49.2224705826886));
#25006=CARTESIAN_POINT('Ctrl Pts',(43.7864039689174,37.2379283220036,49.3491472525141));
#25007=CARTESIAN_POINT('Ctrl Pts',(43.6817620436271,37.2295074347663,49.4489346340064));
#25008=CARTESIAN_POINT('Ctrl Pts',(43.4792516554998,37.2142808846742,49.6027765346566));
#25009=CARTESIAN_POINT('Ctrl Pts',(43.3860023521216,37.2075944492648,49.661767546029));
#25010=CARTESIAN_POINT('Ctrl Pts',(43.2731012140215,37.1995156788889,49.7203277483209));
#25011=CARTESIAN_POINT('Ctrl Pts',(43.2578621779031,37.1984259519915,49.7279773567782));
#25012=CARTESIAN_POINT('Ctrl Pts',(43.2326202035982,37.1966210391263,49.7402319845528));
#25013=CARTESIAN_POINT('Ctrl Pts',(43.2226754777222,37.1959099782016,49.7449552468613));
#25014=CARTESIAN_POINT('Ctrl Pts',(43.2046496533096,37.1946208991545,49.7533282944777));
#25015=CARTESIAN_POINT('Ctrl Pts',(43.196582730267,37.1940439356789,49.7570080028878));
#25016=CARTESIAN_POINT('Ctrl Pts',(43.1792349555457,37.1928028846678,49.7647771233372));
#25017=CARTESIAN_POINT('Ctrl Pts',(43.1699466819887,37.1921382226546,49.768849205335));
#25018=CARTESIAN_POINT('Ctrl Pts',(43.1444601646397,37.1903136942465,49.7797840020163));
#25019=CARTESIAN_POINT('Ctrl Pts',(43.1281998036609,37.1891488370865,49.7864985422583));
#25020=CARTESIAN_POINT('Ctrl Pts',(43.0331782900985,37.182335100671,49.8242238571027));
#25021=CARTESIAN_POINT('Ctrl Pts',(42.9525470534217,37.1765209863044,49.8502420410682));
#25022=CARTESIAN_POINT('Ctrl Pts',(42.7593007523353,37.162534957377,49.8988384664183));
#25023=CARTESIAN_POINT('Ctrl Pts',(42.6458559570098,37.1542771136271,49.9168298509069));
#25024=CARTESIAN_POINT('Ctrl Pts',(42.4959203772501,37.1436140163687,49.9270737825472));
#25025=CARTESIAN_POINT('Ctrl Pts',(42.4602826792262,37.1410995972006,49.9285176444353));
#25026=CARTESIAN_POINT('Ctrl Pts',(42.3862269337409,37.1359396937168,49.9294629909972));
#25027=CARTESIAN_POINT('Ctrl Pts',(42.347820607805,37.1333000374757,49.9288066040749));
#25028=CARTESIAN_POINT('Ctrl Pts',(42.2996288349812,37.1300535770805,49.9265422351811));
#25029=CARTESIAN_POINT('Ctrl Pts',(42.2898045073605,37.1293952034604,49.9260052747159));
#25030=CARTESIAN_POINT('Ctrl Pts',(42.2743383435585,37.1283646225048,49.9250412222961));
#25031=CARTESIAN_POINT('Ctrl Pts',(42.2686937076775,37.1279897291444,49.924664443243));
#25032=CARTESIAN_POINT('Ctrl Pts',(42.258045306268,37.1272849397764,49.9239065993204));
#25033=CARTESIAN_POINT('Ctrl Pts',(42.2530414107192,37.1269547731323,49.9235308449851));
#25034=CARTESIAN_POINT('Ctrl Pts',(42.241325219988,37.126184044992,49.922605062305));
#25035=CARTESIAN_POINT('Ctrl Pts',(42.2346142704908,37.1257443596817,49.922039405226));
#25036=CARTESIAN_POINT('Ctrl Pts',(42.2127214800651,37.124315412343,49.9200785768345));
#25037=CARTESIAN_POINT('Ctrl Pts',(42.1975527434189,37.1233338522199,49.9185385397944));
#25038=CARTESIAN_POINT('Ctrl Pts',(42.1141964382157,37.1179788914244,49.9090759563455));
#25039=CARTESIAN_POINT('Ctrl Pts',(42.0464437575831,37.1137693319594,49.8976972121558));
#25040=CARTESIAN_POINT('Ctrl Pts',(41.9168262889714,37.1057501864126,49.8687432203114));
#25041=CARTESIAN_POINT('Ctrl Pts',(41.8549849134989,37.1019392963471,49.8516502108444));
#25042=CARTESIAN_POINT('Ctrl Pts',(41.794138668834,37.0981147778663,49.8315224826078));
#25043=CARTESIAN_POINT('Origin',(42.4,48.4493818343519,48.));
#25044=CARTESIAN_POINT('',(41.7941388330275,36.1345714126848,49.8315225369224));
#25045=CARTESIAN_POINT('',(41.7941388317569,36.3061495715672,49.8315225365021));
#25046=CARTESIAN_POINT('',(41.7941388317924,48.4493818343519,49.8315225365138));
#25047=CARTESIAN_POINT('',(40.4708706606089,36.7697993578986,47.9984035036532));
#25048=CARTESIAN_POINT('Ctrl Pts',(41.7941388330275,36.1345714126848,49.8315225369224));
#25049=CARTESIAN_POINT('Ctrl Pts',(41.8009572806551,36.1350086104464,49.833778055243));
#25050=CARTESIAN_POINT('Ctrl Pts',(41.8077888007653,36.1354448604187,49.8359956555078));
#25051=CARTESIAN_POINT('Ctrl Pts',(41.9455836056583,36.1442111378064,49.8798764128082));
#25052=CARTESIAN_POINT('Ctrl Pts',(42.0806146586887,36.1522315503165,49.9074654288939));
#25053=CARTESIAN_POINT('Ctrl Pts',(42.2841799109813,36.1646978117889,49.9268169322791));
#25054=CARTESIAN_POINT('Ctrl Pts',(42.3512044109253,36.1688560477862,49.929677515734));
#25055=CARTESIAN_POINT('Ctrl Pts',(42.4354047530644,36.1742170632708,49.9288814942915));
#25056=CARTESIAN_POINT('Ctrl Pts',(42.4525691265035,36.1753169335038,49.9284900237877));
#25057=CARTESIAN_POINT('Ctrl Pts',(42.4797707775054,36.1770721158391,49.9275062174923));
#25058=CARTESIAN_POINT('Ctrl Pts',(42.4898128466723,36.177722701858,49.9270644103481));
#25059=CARTESIAN_POINT('Ctrl Pts',(42.5078325914792,36.1788950326237,49.9261304650688));
#25060=CARTESIAN_POINT('Ctrl Pts',(42.5158115829642,36.1794158579891,49.9256671857462));
#25061=CARTESIAN_POINT('Ctrl Pts',(42.5344928357372,36.180639426134,49.9244659817669));
#25062=CARTESIAN_POINT('Ctrl Pts',(42.5451921896351,36.1813434025495,49.9236883474193));
#25063=CARTESIAN_POINT('Ctrl Pts',(42.5761700197746,36.1833911804766,49.9211769557397));
#25064=CARTESIAN_POINT('Ctrl Pts',(42.5964277291924,36.1847422042499,49.9192115214702));
#25065=CARTESIAN_POINT('Ctrl Pts',(42.6422030676289,36.1878230626574,49.9140380182859));
#25066=CARTESIAN_POINT('Ctrl Pts',(42.6676948359833,36.1895585761448,49.9106394818276));
#25067=CARTESIAN_POINT('Ctrl Pts',(42.7518620571181,36.1953557499667,49.8977009816661));
#25068=CARTESIAN_POINT('Ctrl Pts',(42.8101600314783,36.1994807566417,49.8859595800851));
#25069=CARTESIAN_POINT('Ctrl Pts',(43.0033079610357,36.2134873853851,49.837679631603));
#25070=CARTESIAN_POINT('Ctrl Pts',(43.1347104660036,36.2236161020049,49.7892023279416));
#25071=CARTESIAN_POINT('Ctrl Pts',(43.2983030526839,36.2363931871989,49.7077620660429));
#25072=CARTESIAN_POINT('Ctrl Pts',(43.3362301453234,36.2393647182202,49.6872680312452));
#25073=CARTESIAN_POINT('Ctrl Pts',(43.3821561796756,36.242946989608,49.6604257511065));
#25074=CARTESIAN_POINT('Ctrl Pts',(43.3908305787249,36.2436228661545,49.6552640911219));
#25075=CARTESIAN_POINT('Ctrl Pts',(43.4044023747732,36.2446786882718,49.6470433381782));
#25076=CARTESIAN_POINT('Ctrl Pts',(43.4093270843368,36.2450614643382,49.6440300262716));
#25077=CARTESIAN_POINT('Ctrl Pts',(43.4180620812676,36.2457396818177,49.6386312466677));
#25078=CARTESIAN_POINT('Ctrl Pts',(43.4218775540147,36.2460356752885,49.6362545734473));
#25079=CARTESIAN_POINT('Ctrl Pts',(43.4309909645052,36.2467420965395,49.6305334829408));
#25080=CARTESIAN_POINT('Ctrl Pts',(43.4362809518388,36.2471516939045,49.6271765729215));
#25081=CARTESIAN_POINT('Ctrl Pts',(43.4522763039183,36.2483891178528,49.6169166302427));
#25082=CARTESIAN_POINT('Ctrl Pts',(43.46292999451,36.2492118309391,49.6099331218116));
#25083=CARTESIAN_POINT('Ctrl Pts',(43.5595209897823,36.2566650191664,49.5452407572224));
#25084=CARTESIAN_POINT('Ctrl Pts',(43.6407648190996,36.2628959960399,49.4807993335028));
#25085=CARTESIAN_POINT('Ctrl Pts',(43.8292169004898,36.278302792853,49.3048676443737));
#25086=CARTESIAN_POINT('Ctrl Pts',(43.9289341128406,36.2874108156162,49.186463417218));
#25087=CARTESIAN_POINT('Ctrl Pts',(44.0266999911801,36.298671602816,49.0372901679564));
#25088=CARTESIAN_POINT('Ctrl Pts',(44.0395351919021,36.3002066290058,49.0168815199937));
#25089=CARTESIAN_POINT('Ctrl Pts',(44.0579069099156,36.3024926957422,48.9864171387052));
#25090=CARTESIAN_POINT('Ctrl Pts',(44.0637418732611,36.3032328152226,48.9765434262065));
#25091=CARTESIAN_POINT('Ctrl Pts',(44.0739552557175,36.3045539492513,48.9589034534954));
#25092=CARTESIAN_POINT('Ctrl Pts',(44.0783685685713,36.305133678329,48.9511577023916));
#25093=CARTESIAN_POINT('Ctrl Pts',(44.0875516082019,36.3063589719796,48.9347777398681));
#25094=CARTESIAN_POINT('Ctrl Pts',(44.092309103392,36.3070049548786,48.926137001601));
#25095=CARTESIAN_POINT('Ctrl Pts',(44.1047549801387,36.3087251919349,48.9031162195246));
#25096=CARTESIAN_POINT('Ctrl Pts',(44.1123275208251,36.3098035183433,48.8886747896752));
#25097=CARTESIAN_POINT('Ctrl Pts',(44.1486263152331,36.3151331092247,48.8172632866138));
#25098=CARTESIAN_POINT('Ctrl Pts',(44.1746942181496,36.3194756439799,48.7589941478702));
#25099=CARTESIAN_POINT('Ctrl Pts',(44.2465816683818,36.3332280347396,48.5742442184276));
#25100=CARTESIAN_POINT('Ctrl Pts',(44.2821006647031,36.3429146200307,48.4441963964617));
#25101=CARTESIAN_POINT('Ctrl Pts',(44.3158528097258,36.3577608374964,48.237933784063));
#25102=CARTESIAN_POINT('Ctrl Pts',(44.3236197499801,36.3629956320636,48.1636889931486));
#25103=CARTESIAN_POINT('Ctrl Pts',(44.3275489082023,36.3687343087476,48.0787784743352));
#25104=CARTESIAN_POINT('Ctrl Pts',(44.3279458195893,36.3694328518889,48.0683796020343));
#25105=CARTESIAN_POINT('Ctrl Pts',(44.3284510474268,36.3705541754809,48.0515764333418));
#25106=CARTESIAN_POINT('Ctrl Pts',(44.3286116446584,36.3709796816807,48.0451740834075));
#25107=CARTESIAN_POINT('Ctrl Pts',(44.3288405185264,36.3717331567373,48.0337882806378));
#25108=CARTESIAN_POINT('Ctrl Pts',(44.3289213705609,36.3720618079144,48.0288052417905));
#25109=CARTESIAN_POINT('Ctrl Pts',(44.3290553592587,36.3727749624879,48.0179554183574));
#25110=CARTESIAN_POINT('Ctrl Pts',(44.3291010451083,36.3731590492992,48.0120886787781));
#25111=CARTESIAN_POINT('Ctrl Pts',(44.3291548070831,36.3742462598663,47.9954191406808));
#25112=CARTESIAN_POINT('Ctrl Pts',(44.3290989099084,36.3749459306643,47.9846161504112));
#25113=CARTESIAN_POINT('Ctrl Pts',(44.3280910718764,36.3797239490435,47.9103755652056));
#25114=CARTESIAN_POINT('Ctrl Pts',(44.3241007971104,36.3836505217062,47.8470109472369));
#25115=CARTESIAN_POINT('Ctrl Pts',(44.3025826947547,36.3953281363148,47.656081049615));
#25116=CARTESIAN_POINT('Ctrl Pts',(44.2754136488311,36.4028511752207,47.5299712337034));
#25117=CARTESIAN_POINT('Ctrl Pts',(44.2116427354186,36.4154277965226,47.3323733059094));
#25118=CARTESIAN_POINT('Ctrl Pts',(44.182810293558,36.4202944950793,47.2588117373764));
#25119=CARTESIAN_POINT('Ctrl Pts',(44.1420959732181,36.4264408876067,47.1711709034922));
#25120=CARTESIAN_POINT('Ctrl Pts',(44.1344157607817,36.427574241417,47.155217195752));
#25121=CARTESIAN_POINT('Ctrl Pts',(44.1219348894102,36.4293771125267,47.1301791577639));
#25122=CARTESIAN_POINT('Ctrl Pts',(44.1172792651016,36.4300415600776,47.1210233337375));
#25123=CARTESIAN_POINT('Ctrl Pts',(44.1084727881656,36.4312838549264,47.1040414299086));
#25124=CARTESIAN_POINT('Ctrl Pts',(44.1043406993559,36.4318610269098,47.0962058844363));
#25125=CARTESIAN_POINT('Ctrl Pts',(44.095030401762,36.4331490697278,47.078841982025));
#25126=CARTESIAN_POINT('Ctrl Pts',(44.0898255502881,36.4338608770641,47.0693283294348));
#25127=CARTESIAN_POINT('Ctrl Pts',(44.0743444780676,36.4359545060972,47.0415893999121));
#25128=CARTESIAN_POINT('Ctrl Pts',(44.063851917181,36.4373440565229,47.0234873024757));
#25129=CARTESIAN_POINT('Ctrl Pts',(44.0393371339341,36.4405267074739,46.9827361368184));
#25130=CARTESIAN_POINT('Ctrl Pts',(44.0251362931791,36.4423260432584,46.9602000594332));
#25131=CARTESIAN_POINT('Ctrl Pts',(43.9759623109439,36.4484142832456,46.8856323631042));
#25132=CARTESIAN_POINT('Ctrl Pts',(43.9389233599734,36.4527737926352,46.8350167285073));
#25133=CARTESIAN_POINT('Ctrl Pts',(43.8520976515911,36.4625033669065,46.7277464059677));
#25134=CARTESIAN_POINT('Ctrl Pts',(43.8013186451659,36.4678927262991,46.6720233519219));
#25135=CARTESIAN_POINT('Ctrl Pts',(43.7228114364217,36.4757249590862,46.5954024267692));
#25136=CARTESIAN_POINT('Ctrl Pts',(43.6975704097303,36.4781751260998,46.5720519737054));
#25137=CARTESIAN_POINT('Ctrl Pts',(43.6222225686771,36.4852702805575,46.5059962378081));
#25138=CARTESIAN_POINT('Ctrl Pts',(43.5705325842715,36.4898697908531,46.4651610442292));
#25139=CARTESIAN_POINT('Ctrl Pts',(43.5084877348528,36.4950055596224,46.4211071304611));
#25140=CARTESIAN_POINT('Ctrl Pts',(43.5000774800546,36.4956939013415,46.4152358847721));
#25141=CARTESIAN_POINT('Ctrl Pts',(43.4863770367598,36.4968021065985,46.4058331529704));
#25142=CARTESIAN_POINT('Ctrl Pts',(43.4811156393179,36.4972245968493,46.4022603530433));
#25143=CARTESIAN_POINT('Ctrl Pts',(43.4717025469631,36.4979748293884,46.3959360946856));
#25144=CARTESIAN_POINT('Ctrl Pts',(43.4675577744175,36.4983032304236,46.3931746324963));
#25145=CARTESIAN_POINT('Ctrl Pts',(43.4584794484624,36.4990182858207,46.3871768152563));
#25146=CARTESIAN_POINT('Ctrl Pts',(43.4535417216059,36.4994045050021,46.3839470271071));
#25147=CARTESIAN_POINT('Ctrl Pts',(43.4393903201526,36.500503940726,46.3747829612085));
#25148=CARTESIAN_POINT('Ctrl Pts',(43.4301406117594,36.5012135808167,46.3689043576677));
#25149=CARTESIAN_POINT('Ctrl Pts',(43.3631742485993,36.5062907868552,46.3271411406001));
#25150=CARTESIAN_POINT('Ctrl Pts',(43.3036402425044,36.5104839565738,46.2942456597732));
#25151=CARTESIAN_POINT('Ctrl Pts',(43.1180360963973,36.5229890073882,46.2041422765265));
#25152=CARTESIAN_POINT('Ctrl Pts',(42.9874479961017,36.5310611392555,46.157288033414));
#25153=CARTESIAN_POINT('Ctrl Pts',(42.7888060176593,36.5435272366493,46.1093044985585));
#25154=CARTESIAN_POINT('Ctrl Pts',(42.7238964608718,36.5476232114347,46.0971102814945));
#25155=CARTESIAN_POINT('Ctrl Pts',(42.6415484750845,36.5529142552284,46.0859756261338));
#25156=CARTESIAN_POINT('Ctrl Pts',(42.6245733460683,36.5540098162237,46.0839097746938));
#25157=CARTESIAN_POINT('Ctrl Pts',(42.5975947827078,36.5557597017254,46.0809899431215));
#25158=CARTESIAN_POINT('Ctrl Pts',(42.5876080233734,36.5564093497652,46.0799878855096));
#25159=CARTESIAN_POINT('Ctrl Pts',(42.5696536332314,36.5575808770428,46.0783277824564));
#25160=CARTESIAN_POINT('Ctrl Pts',(42.5616888172968,36.5581018449284,46.0776412431434));
#25161=CARTESIAN_POINT('Ctrl Pts',(42.5430063339167,36.5593269089645,46.076147806392));
#25162=CARTESIAN_POINT('Ctrl Pts',(42.5322858227665,36.5600322486143,46.0753809396336));
#25163=CARTESIAN_POINT('Ctrl Pts',(42.5011492706283,36.5620879736502,46.0734150353505));
#25164=CARTESIAN_POINT('Ctrl Pts',(42.4807203970856,36.5634456678922,46.0724510477104));
#25165=CARTESIAN_POINT('Ctrl Pts',(42.4344188785877,36.5665441049198,46.0710035288296));
#25166=CARTESIAN_POINT('Ctrl Pts',(42.4085445063989,36.5682906205869,46.0707154362865));
#25167=CARTESIAN_POINT('Ctrl Pts',(42.3226799045727,36.5741375221424,46.0714866753528));
#25168=CARTESIAN_POINT('Ctrl Pts',(42.2627497625028,36.5783024655663,46.0748238390646));
#25169=CARTESIAN_POINT('Ctrl Pts',(42.1257891429925,36.5879922453757,46.0888780023973));
#25170=CARTESIAN_POINT('Ctrl Pts',(42.0490540534555,36.5935485658404,46.1014703664577));
#25171=CARTESIAN_POINT('Ctrl Pts',(41.8817581829358,36.6057983577597,46.1394147961711));
#25172=CARTESIAN_POINT('Ctrl Pts',(41.791852492104,36.6124734034057,46.1668300494897));
#25173=CARTESIAN_POINT('Ctrl Pts',(41.6889784090794,36.6199820789853,46.2066064457459));
#25174=CARTESIAN_POINT('Ctrl Pts',(41.6737397850468,36.6210906892824,46.2127232202605));
#25175=CARTESIAN_POINT('Ctrl Pts',(41.6526280758012,36.6226196577722,46.2215120647586));
#25176=CARTESIAN_POINT('Ctrl Pts',(41.646687998176,36.623049085284,46.2240199438821));
#25177=CARTESIAN_POINT('Ctrl Pts',(41.6364633661507,36.6237867883855,46.2283972749394));
#25178=CARTESIAN_POINT('Ctrl Pts',(41.6321728735536,36.6240958972375,46.2302525853289));
#25179=CARTESIAN_POINT('Ctrl Pts',(41.6231388719413,36.6247457400443,46.2341981386607));
#25180=CARTESIAN_POINT('Ctrl Pts',(41.6183969685774,36.6250862433636,46.2362919379391));
#25181=CARTESIAN_POINT('Ctrl Pts',(41.6069257491492,36.6259086484721,46.2414124325074));
#25182=CARTESIAN_POINT('Ctrl Pts',(41.6002051635955,36.6263893682201,46.24445870914));
#25183=CARTESIAN_POINT('Ctrl Pts',(41.5754567372873,36.6281561432442,46.2558481812904));
#25184=CARTESIAN_POINT('Ctrl Pts',(41.5575398783452,36.6294283966347,46.2644314543195));
#25185=CARTESIAN_POINT('Ctrl Pts',(41.5124210643545,36.6326228291553,46.2869095242789));
#25186=CARTESIAN_POINT('Ctrl Pts',(41.4854098995034,36.6345264331339,46.3011767309174));
#25187=CARTESIAN_POINT('Ctrl Pts',(41.3588961211328,36.6434539001505,46.3718935219641));
#25188=CARTESIAN_POINT('Ctrl Pts',(41.2642004126601,36.6501819496267,46.4364812258942));
#25189=CARTESIAN_POINT('Ctrl Pts',(41.0901678247078,36.6636621416798,46.5793826026087));
#25190=CARTESIAN_POINT('Ctrl Pts',(41.0107800366663,36.6703842196541,46.656915037007));
#25191=CARTESIAN_POINT('Ctrl Pts',(40.9273521396177,36.6785029912698,46.7537488581037));
#25192=CARTESIAN_POINT('Ctrl Pts',(40.9163884808457,36.6795933394521,46.7668209944236));
#25193=CARTESIAN_POINT('Ctrl Pts',(40.8986347094142,36.6813991794055,46.7885685610281));
#25194=CARTESIAN_POINT('Ctrl Pts',(40.8917428217386,36.6821105404719,46.7971599678215));
#25195=CARTESIAN_POINT('Ctrl Pts',(40.8794346298839,36.6834000980226,46.8127754312641));
#25196=CARTESIAN_POINT('Ctrl Pts',(40.8739924438112,36.6839772385048,46.8197787684332));
#25197=CARTESIAN_POINT('Ctrl Pts',(40.8624300144788,36.6852185993072,46.8348716844132));
#25198=CARTESIAN_POINT('Ctrl Pts',(40.8563249186648,36.6858833939101,46.8429724771036));
#25199=CARTESIAN_POINT('Ctrl Pts',(40.8398069183229,36.6877081079555,46.8652535057699));
#25200=CARTESIAN_POINT('Ctrl Pts',(40.8295238662872,36.6888730178222,46.8795283418628));
#25201=CARTESIAN_POINT('Ctrl Pts',(40.7709365156526,36.6956833330119,46.9632499057979));
#25202=CARTESIAN_POINT('Ctrl Pts',(40.7270533897486,36.7014937554484,47.0356636124512));
#25203=CARTESIAN_POINT('Ctrl Pts',(40.661535844037,36.7114692725471,47.1617890949728));
#25204=CARTESIAN_POINT('Ctrl Pts',(40.6373044749432,36.715560480507,47.2140235135481));
#25205=CARTESIAN_POINT('Ctrl Pts',(40.5907323562836,36.7243121413339,47.3274478437722));
#25206=CARTESIAN_POINT('Ctrl Pts',(40.5690796922284,36.7289721003683,47.3888478644616));
#25207=CARTESIAN_POINT('Ctrl Pts',(40.5324931790245,36.7380700826651,47.5121483578574));
#25208=CARTESIAN_POINT('Ctrl Pts',(40.5174350806266,36.7425051278411,47.5739342508564));
#25209=CARTESIAN_POINT('Ctrl Pts',(40.5035350550902,36.7474811980011,47.6463520758601));
#25210=CARTESIAN_POINT('Ctrl Pts',(40.5016956336781,36.7481641647341,47.6563625670655));
#25211=CARTESIAN_POINT('Ctrl Pts',(40.4988397481347,36.7492654512868,47.6726280407071));
#25212=CARTESIAN_POINT('Ctrl Pts',(40.4977747530299,36.7496863462597,47.6788741436277));
#25213=CARTESIAN_POINT('Ctrl Pts',(40.4959278740491,36.7504348752451,47.6900376065054));
#25214=CARTESIAN_POINT('Ctrl Pts',(40.4951342347208,36.7507631555098,47.6949528490451));
#25215=CARTESIAN_POINT('Ctrl Pts',(40.4936236219974,36.7514012208612,47.7045443494784));
#25216=CARTESIAN_POINT('Ctrl Pts',(40.4929048209998,36.7517111136964,47.7092201598197));
#25217=CARTESIAN_POINT('Ctrl Pts',(40.4913332108834,36.7524031734755,47.7197000562021));
#25218=CARTESIAN_POINT('Ctrl Pts',(40.4904896572616,36.7527848304333,47.7255055127927));
#25219=CARTESIAN_POINT('Ctrl Pts',(40.4884319193051,36.7537425276665,47.7401358440947));
#25220=CARTESIAN_POINT('Ctrl Pts',(40.4872523373952,36.7543167518144,47.7489655543143));
#25221=CARTESIAN_POINT('Ctrl Pts',(40.4760359757809,36.7600459676455,47.837598533665));
#25222=CARTESIAN_POINT('Ctrl Pts',(40.4709372370669,36.7649585678963,47.9179557164651));
#25223=CARTESIAN_POINT('Ctrl Pts',(40.4708706606089,36.7697993578986,47.9984035036532));
#25224=CARTESIAN_POINT('Ctrl Pts',(40.4708706624223,36.7697992261421,47.9984013140282));
#25225=CARTESIAN_POINT('Ctrl Pts',(40.4707569252598,36.7780577578374,48.1356475905335));
#25226=CARTESIAN_POINT('Ctrl Pts',(40.4852891210741,36.7860953737044,48.2725153539239));
#25227=CARTESIAN_POINT('Ctrl Pts',(40.5257982606741,36.7979099669867,48.460352132471));
#25228=CARTESIAN_POINT('Ctrl Pts',(40.5396557529755,36.8013392905584,48.513492618657));
#25229=CARTESIAN_POINT('Ctrl Pts',(40.5603242358317,36.8058347654552,48.5808422919918));
#25230=CARTESIAN_POINT('Ctrl Pts',(40.565069059847,36.8068333305538,48.5956619068988));
#25231=CARTESIAN_POINT('Ctrl Pts',(40.5730622252872,36.808464023713,48.6196249172202));
#25232=CARTESIAN_POINT('Ctrl Pts',(40.5762012489584,36.8090925340274,48.6288042467116));
#25233=CARTESIAN_POINT('Ctrl Pts',(40.5823723405563,36.8103059670176,48.6464151358981));
#25234=CARTESIAN_POINT('Ctrl Pts',(40.5853941839218,36.8108905363832,48.654850031664));
#25235=CARTESIAN_POINT('Ctrl Pts',(40.5924648089623,36.8122368309938,48.6741615383886));
#25236=CARTESIAN_POINT('Ctrl Pts',(40.5965531697579,36.8129998637378,48.6850231872972));
#25237=CARTESIAN_POINT('Ctrl Pts',(40.6099470246769,36.815451861123,48.7196558507389));
#25238=CARTESIAN_POINT('Ctrl Pts',(40.6196261066162,36.8171532906534,48.7432784747977));
#25239=CARTESIAN_POINT('Ctrl Pts',(40.6761888861681,36.8267266070038,48.8738757613358));
#25240=CARTESIAN_POINT('Ctrl Pts',(40.7322362040158,36.8349105836414,48.976595710591));
#25241=CARTESIAN_POINT('Ctrl Pts',(40.8516279067285,36.8501935261282,49.1548358867709));
#25242=CARTESIAN_POINT('Ctrl Pts',(40.9121384244596,36.857224964475,49.2318161402958));
#25243=CARTESIAN_POINT('Ctrl Pts',(40.9988947501641,36.8662112869134,49.3264169120343));
#25244=CARTESIAN_POINT('Ctrl Pts',(41.0200982243359,36.8683320553846,49.3484617329203));
#25245=CARTESIAN_POINT('Ctrl Pts',(41.055872782144,36.8717760531038,49.3839278378523));
#25246=CARTESIAN_POINT('Ctrl Pts',(41.0701418204504,36.8731164110648,49.3976449962793));
#25247=CARTESIAN_POINT('Ctrl Pts',(41.089975502176,36.8749314146436,49.4161327523362));
#25248=CARTESIAN_POINT('Ctrl Pts',(41.0953593875194,36.8754193679366,49.4210943085137));
#25249=CARTESIAN_POINT('Ctrl Pts',(41.1046229880529,36.8762506886312,49.4295342252387));
#25250=CARTESIAN_POINT('Ctrl Pts',(41.1084887483931,36.8765951729143,49.4330277014369));
#25251=CARTESIAN_POINT('Ctrl Pts',(41.1158325428134,36.8772449247393,49.4396104116713));
#25252=CARTESIAN_POINT('Ctrl Pts',(41.1193076673501,36.8775504354563,49.4427027918916));
#25253=CARTESIAN_POINT('Ctrl Pts',(41.1275586557853,36.8782712926793,49.4499917244929));
#25254=CARTESIAN_POINT('Ctrl Pts',(41.132344182394,36.8786858324727,49.4541773297817));
#25255=CARTESIAN_POINT('Ctrl Pts',(41.1491568500165,36.8801301942742,49.4687362675003));
#25256=CARTESIAN_POINT('Ctrl Pts',(41.1612917120652,36.8811513517883,49.4789849985772));
#25257=CARTESIAN_POINT('Ctrl Pts',(41.267190321235,36.8898943984561,49.5662058622677));
#25258=CARTESIAN_POINT('Ctrl Pts',(41.367908044144,36.8970950927505,49.6343356640115));
#25259=CARTESIAN_POINT('Ctrl Pts',(41.5573348998316,36.9099720537676,49.7379296876064));
#25260=CARTESIAN_POINT('Ctrl Pts',(41.6435181852034,36.9156155288907,49.7771374697818));
#25261=CARTESIAN_POINT('Ctrl Pts',(41.7527389599502,36.9227892690317,49.8174360782789));
#25262=CARTESIAN_POINT('Ctrl Pts',(41.7733804888912,36.924145523862,49.8246557502234));
#25263=CARTESIAN_POINT('Ctrl Pts',(41.7941388333426,36.925511940895,49.8315225370267));
#25264=CARTESIAN_POINT('',(40.4708700028765,36.9418246930855,47.9998946523509));
#25265=CARTESIAN_POINT('Ctrl Pts',(41.794138668834,37.0981147778663,49.8315224826078));
#25266=CARTESIAN_POINT('Ctrl Pts',(41.7454310361826,37.0950532373841,49.815410165431));
#25267=CARTESIAN_POINT('Ctrl Pts',(41.6973610717923,37.091983196828,49.7973531909593));
#25268=CARTESIAN_POINT('Ctrl Pts',(41.5766700783443,37.0840521298605,49.7464285821558));
#25269=CARTESIAN_POINT('Ctrl Pts',(41.5052907762867,37.0791449949644,49.710958237956));
#25270=CARTESIAN_POINT('Ctrl Pts',(41.4209724660933,37.0729555239317,49.6623360721082));
#25271=CARTESIAN_POINT('Ctrl Pts',(41.4057552262409,37.0718222576782,49.6532795967791));
#25272=CARTESIAN_POINT('Ctrl Pts',(41.3820247275679,37.0700281489059,49.63871037718));
#25273=CARTESIAN_POINT('Ctrl Pts',(41.3734263389798,37.0693724405478,49.6333376465228));
#25274=CARTESIAN_POINT('Ctrl Pts',(41.3580770133011,37.0681915414317,49.6235774896652));
#25275=CARTESIAN_POINT('Ctrl Pts',(41.3513103884722,37.0676672896392,49.6192150785249));
#25276=CARTESIAN_POINT('Ctrl Pts',(41.3375614442115,37.0665944740949,49.6102288664108));
#25277=CARTESIAN_POINT('Ctrl Pts',(41.3305815375667,37.0660457917976,49.6056017051235));
#25278=CARTESIAN_POINT('Ctrl Pts',(41.3102370988762,37.0644344994713,49.5919233364144));
#25279=CARTESIAN_POINT('Ctrl Pts',(41.2969560432276,37.0633672790527,49.5827498513841));
#25280=CARTESIAN_POINT('Ctrl Pts',(41.2334528888738,37.0581884089966,49.5376994940218));
#25281=CARTESIAN_POINT('Ctrl Pts',(41.1848619101246,37.0539916450362,49.4995965720038));
#25282=CARTESIAN_POINT('Ctrl Pts',(41.038747219693,37.0406094233033,49.3732496309346));
#25283=CARTESIAN_POINT('Ctrl Pts',(40.9483668961227,37.0311543843263,49.2773324207762));
#25284=CARTESIAN_POINT('Ctrl Pts',(40.8199206676892,37.0161258388123,49.1096225847369));
#25285=CARTESIAN_POINT('Ctrl Pts',(40.7753633117638,37.0105087196857,49.0432984151213));
#25286=CARTESIAN_POINT('Ctrl Pts',(40.7297413294677,37.004409723654,48.9653437547797));
#25287=CARTESIAN_POINT('Ctrl Pts',(40.7245167852918,37.0037054663072,48.9562471441007));
#25288=CARTESIAN_POINT('Ctrl Pts',(40.7162106812862,37.0025768666194,48.9415080496272));
#25289=CARTESIAN_POINT('Ctrl Pts',(40.7130827545468,37.0021497418739,48.9358921344244));
#25290=CARTESIAN_POINT('Ctrl Pts',(40.7075794086608,37.0013946023317,48.9258941309088));
#25291=CARTESIAN_POINT('Ctrl Pts',(40.7051928389852,37.0010658919909,48.9215183604213));
#25292=CARTESIAN_POINT('Ctrl Pts',(40.7000437638187,37.0003540028192,48.9119898744771));
#25293=CARTESIAN_POINT('Ctrl Pts',(40.6972877088918,36.9999712298017,48.9068338282324));
#25294=CARTESIAN_POINT('Ctrl Pts',(40.6895485471102,36.9988912027357,48.8921956750119));
#25295=CARTESIAN_POINT('Ctrl Pts',(40.6846208209799,36.9981973312007,48.882684303784));
#25296=CARTESIAN_POINT('Ctrl Pts',(40.6521097475877,36.9935739404767,48.8186316325582));
#25297=CARTESIAN_POINT('Ctrl Pts',(40.627049591588,36.9897851675397,48.7628411188254));
#25298=CARTESIAN_POINT('Ctrl Pts',(40.5727654199779,36.9807557946529,48.6247893259087));
#25299=CARTESIAN_POINT('Ctrl Pts',(40.5463909450823,36.975593039245,48.5415557795884));
#25300=CARTESIAN_POINT('Ctrl Pts',(40.4971987142562,36.9631828912664,48.3397278068748));
#25301=CARTESIAN_POINT('Ctrl Pts',(40.4796982803696,36.9559069732899,48.2202350126324));
#25302=CARTESIAN_POINT('Ctrl Pts',(40.4724802446671,36.947056890077,48.0810365037881));
#25303=CARTESIAN_POINT('Ctrl Pts',(40.4717792364017,36.9458494637154,48.0621608277055));
#25304=CARTESIAN_POINT('Ctrl Pts',(40.4711555394033,36.9440594710842,48.0343666126744));
#25305=CARTESIAN_POINT('Ctrl Pts',(40.4710173343154,36.9434836384135,48.0254536503816));
#25306=CARTESIAN_POINT('Ctrl Pts',(40.4708933347106,36.9425462252616,48.010991735587));
#25307=CARTESIAN_POINT('Ctrl Pts',(40.4708696998777,36.9421858346456,48.0054431776609));
#25308=CARTESIAN_POINT('Ctrl Pts',(40.4708700028765,36.9418246930855,47.9998946523509));
#25309=CARTESIAN_POINT('Ctrl Pts',(40.4708700028783,36.9418246909392,47.9998946193751));
#25310=CARTESIAN_POINT('Ctrl Pts',(40.4708703171738,36.9414502021496,47.994141029262));
#25311=CARTESIAN_POINT('Ctrl Pts',(40.4708963714056,36.9410749081892,47.9883875098055));
#25312=CARTESIAN_POINT('Ctrl Pts',(40.4710383629421,36.9400437949537,47.9726145800584));
#25313=CARTESIAN_POINT('Ctrl Pts',(40.4712066235956,36.9393863442948,47.9625959473324));
#25314=CARTESIAN_POINT('Ctrl Pts',(40.4719114878001,36.9374977927137,47.933929941959));
#25315=CARTESIAN_POINT('Ctrl Pts',(40.472640525301,36.9362607098083,47.915288861529));
#25316=CARTESIAN_POINT('Ctrl Pts',(40.4796010678418,36.9275846167825,47.7855351380816));
#25317=CARTESIAN_POINT('Ctrl Pts',(40.4951657822964,36.9198518695679,47.6751521228974));
#25318=CARTESIAN_POINT('Ctrl Pts',(40.5522539584392,36.9018142395651,47.4274540122385));
#25319=CARTESIAN_POINT('Ctrl Pts',(40.5997378559718,36.8914466171965,47.2921628362161));
#25320=CARTESIAN_POINT('Ctrl Pts',(40.6708608603666,36.8802200109951,47.1443930266558));
#25321=CARTESIAN_POINT('Ctrl Pts',(40.6802981116673,36.8787934437358,47.125579642263));
#25322=CARTESIAN_POINT('Ctrl Pts',(40.6935825187309,36.8768722364856,47.1001442158016));
#25323=CARTESIAN_POINT('Ctrl Pts',(40.6971635819629,36.8763624925994,47.0933858643113));
#25324=CARTESIAN_POINT('Ctrl Pts',(40.7032364820796,36.8755117967366,47.0820877298892));
#25325=CARTESIAN_POINT('Ctrl Pts',(40.7057065471878,36.8751695042738,47.0775364130618));
#25326=CARTESIAN_POINT('Ctrl Pts',(40.7104420437151,36.8745203745675,47.0688940249943));
#25327=CARTESIAN_POINT('Ctrl Pts',(40.7127040626889,36.8742133178133,47.0648011733126));
#25328=CARTESIAN_POINT('Ctrl Pts',(40.7181256018287,36.873484407005,47.0550752525117));
#25329=CARTESIAN_POINT('Ctrl Pts',(40.7212985967575,36.8730634042505,47.0494497007954));
#25330=CARTESIAN_POINT('Ctrl Pts',(40.7326726248818,36.8715735878042,47.0295187396789));
#25331=CARTESIAN_POINT('Ctrl Pts',(40.7410290216617,36.8705141699155,47.0153021838153));
#25332=CARTESIAN_POINT('Ctrl Pts',(40.8007555556011,36.8631698525741,46.9166097071062));
#25333=CARTESIAN_POINT('Ctrl Pts',(40.8583776778178,36.8572254473591,46.8360743456382));
#25334=CARTESIAN_POINT('Ctrl Pts',(40.9929134129562,36.8447176937851,46.67566926447));
#25335=CARTESIAN_POINT('Ctrl Pts',(41.0710326544027,36.8381800291895,46.5972923459725));
#25336=CARTESIAN_POINT('Ctrl Pts',(41.1986442560613,36.8279227753285,46.4895410397143));
#25337=CARTESIAN_POINT('Ctrl Pts',(41.2434417872356,36.8243925523091,46.4549711773303));
#25338=CARTESIAN_POINT('Ctrl Pts',(41.3025355347381,36.8197824086446,46.4133806246838));
#25339=CARTESIAN_POINT('Ctrl Pts',(41.3154905477751,36.8187745507199,46.4044974086333));
#25340=CARTESIAN_POINT('Ctrl Pts',(41.3354943708255,36.8172218648858,46.3911370436227));
#25341=CARTESIAN_POINT('Ctrl Pts',(41.3424663801117,36.8166813516314,46.3865456665564));
#25342=CARTESIAN_POINT('Ctrl Pts',(41.3563078658337,36.8156094332521,46.3775586931019));
#25343=CARTESIAN_POINT('Ctrl Pts',(41.3631758536137,36.8150781168087,46.3731611169891));
#25344=CARTESIAN_POINT('Ctrl Pts',(41.378808142928,36.8138699264588,46.3632909519611));
#25345=CARTESIAN_POINT('Ctrl Pts',(41.3875888843045,36.8131920855955,46.3578450004252));
#25346=CARTESIAN_POINT('Ctrl Pts',(41.4122654394281,36.8112891451264,46.3428133629127));
#25347=CARTESIAN_POINT('Ctrl Pts',(41.4282561261429,36.8100583033561,46.3333863930788));
#25348=CARTESIAN_POINT('Ctrl Pts',(41.5498200343681,36.8007155297687,46.2640652601025));
#25349=CARTESIAN_POINT('Ctrl Pts',(41.6606798664753,36.7922496489529,46.2140349069197));
#25350=CARTESIAN_POINT('Ctrl Pts',(41.8587370595397,36.7773564422047,46.1462687793514));
#25351=CARTESIAN_POINT('Ctrl Pts',(41.9438412272781,36.7710326115839,46.1235127492855));
#25352=CARTESIAN_POINT('Ctrl Pts',(42.0892086906285,36.7605756588918,46.0951204906196));
#25353=CARTESIAN_POINT('Ctrl Pts',(42.1487286345174,36.7563902633524,46.0863591179395));
#25354=CARTESIAN_POINT('Ctrl Pts',(42.2191853672955,36.7516177176654,46.0793327957863));
#25355=CARTESIAN_POINT('Ctrl Pts',(42.2298132372096,36.7509026816564,46.0783619177059));
#25356=CARTESIAN_POINT('Ctrl Pts',(42.2462666527663,36.7498037900726,46.0769964394007));
#25357=CARTESIAN_POINT('Ctrl Pts',(42.2520866519703,36.7494166460545,46.0765400238514));
#25358=CARTESIAN_POINT('Ctrl Pts',(42.262880528788,36.7487016487293,46.0757428287392));
#25359=CARTESIAN_POINT('Ctrl Pts',(42.2678536390572,36.7483734200831,46.0753949104563));
#25360=CARTESIAN_POINT('Ctrl Pts',(42.2792543960875,36.7476236498434,46.0746417133527));
#25361=CARTESIAN_POINT('Ctrl Pts',(42.285682767818,36.7472028317202,46.0742493395556));
#25362=CARTESIAN_POINT('Ctrl Pts',(42.3026271525625,36.7460984425102,46.0733002367636));
#25363=CARTESIAN_POINT('Ctrl Pts',(42.3131461361322,36.7454177472603,46.0727973984728));
#25364=CARTESIAN_POINT('Ctrl Pts',(42.4067927897772,36.7393971853489,46.0690891228776));
#25365=CARTESIAN_POINT('Ctrl Pts',(42.4900538123251,36.7343189004283,46.0711773376252));
#25366=CARTESIAN_POINT('Ctrl Pts',(42.5945455641111,36.7280091183409,46.0805819565372));
#25367=CARTESIAN_POINT('Ctrl Pts',(42.6161276451181,36.72670944365,46.0828921614466));
#25368=CARTESIAN_POINT('Ctrl Pts',(42.7188888398743,36.7205209147854,46.0956493950066));
#25369=CARTESIAN_POINT('Ctrl Pts',(42.799386582122,36.7156685448763,46.1108913979855));
#25370=CARTESIAN_POINT('Ctrl Pts',(42.9595498656809,36.7056711001515,46.1519152932779));
#25371=CARTESIAN_POINT('Ctrl Pts',(43.0389894577895,36.7005320899267,46.1778575697527));
#25372=CARTESIAN_POINT('Ctrl Pts',(43.1327732108063,36.6941043262898,46.215373027404));
#25373=CARTESIAN_POINT('Ctrl Pts',(43.1489633193507,36.6929814361813,46.222106886383));
#25374=CARTESIAN_POINT('Ctrl Pts',(43.1743576194729,36.6911980825739,46.2330774108851));
#25375=CARTESIAN_POINT('Ctrl Pts',(43.1836243354947,36.6905426148878,46.2371676049385));
#25376=CARTESIAN_POINT('Ctrl Pts',(43.2009425939524,36.6893085848252,46.2449751688662));
#25377=CARTESIAN_POINT('Ctrl Pts',(43.2090015791004,36.6887306228197,46.2486754620328));
#25378=CARTESIAN_POINT('Ctrl Pts',(43.2270238403651,36.6874296347854,46.2571013457235));
#25379=CARTESIAN_POINT('Ctrl Pts',(43.2369726199378,36.6867055793159,46.261857032208));
#25380=CARTESIAN_POINT('Ctrl Pts',(43.262252197299,36.6848504602083,46.2742084643575));
#25381=CARTESIAN_POINT('Ctrl Pts',(43.2775234489809,36.6837152773168,46.2819232146027));
#25382=CARTESIAN_POINT('Ctrl Pts',(43.396286603507,36.674770443648,46.3439166134479));
#25383=CARTESIAN_POINT('Ctrl Pts',(43.4947369566645,36.6666332820997,46.4072849135489));
#25384=CARTESIAN_POINT('Ctrl Pts',(43.6722368003156,36.6506318504383,46.5458022813326));
#25385=CARTESIAN_POINT('Ctrl Pts',(43.7518728604917,36.6428232846468,46.6195225679128));
#25386=CARTESIAN_POINT('Ctrl Pts',(43.8454498597295,36.6331059731979,46.7220538090091));
#25387=CARTESIAN_POINT('Ctrl Pts',(43.8654635755177,36.6309921989567,46.7450543911489));
#25388=CARTESIAN_POINT('Ctrl Pts',(43.897650542614,36.6275452610939,46.7838656263321));
#25389=CARTESIAN_POINT('Ctrl Pts',(43.9101382799499,36.626195331275,46.7994074733848));
#25390=CARTESIAN_POINT('Ctrl Pts',(43.9269836714137,36.6243598470176,46.821051518329));
#25391=CARTESIAN_POINT('Ctrl Pts',(43.9315495404351,36.6238608320935,46.8269890601568));
#25392=CARTESIAN_POINT('Ctrl Pts',(43.939194213498,36.6230229642824,46.8370510689767));
#25393=CARTESIAN_POINT('Ctrl Pts',(43.9422912736149,36.622682856252,46.8411614984653));
#25394=CARTESIAN_POINT('Ctrl Pts',(43.9481899563555,36.6220338777575,46.8490557872351));
#25395=CARTESIAN_POINT('Ctrl Pts',(43.9509942176807,36.6217248144004,46.8528375617343));
#25396=CARTESIAN_POINT('Ctrl Pts',(43.9576849073498,36.6209860270682,46.8619298829991));
#25397=CARTESIAN_POINT('Ctrl Pts',(43.9615580943989,36.6205572084981,46.8672501676447));
#25398=CARTESIAN_POINT('Ctrl Pts',(43.9733571173195,36.619247005931,46.8836330652246));
#25399=CARTESIAN_POINT('Ctrl Pts',(43.9811933807205,36.6183713976806,46.8947600851909));
#25400=CARTESIAN_POINT('Ctrl Pts',(44.0668265734546,36.6087302944878,47.0191291596374));
#25401=CARTESIAN_POINT('Ctrl Pts',(44.1324423102089,36.6006465526967,47.1403061533718));
#25402=CARTESIAN_POINT('Ctrl Pts',(44.2256530564769,36.5859913907075,47.3673829199694));
#25403=CARTESIAN_POINT('Ctrl Pts',(44.2582048357959,36.5794939006893,47.4705808835711));
#25404=CARTESIAN_POINT('Ctrl Pts',(44.2885606998226,36.5708282070692,47.6053025247742));
#25405=CARTESIAN_POINT('Ctrl Pts',(44.2944858313437,36.568920987599,47.6348002030437));
#25406=CARTESIAN_POINT('Ctrl Pts',(44.3018952892932,36.5661894706214,47.6767455411945));
#25407=CARTESIAN_POINT('Ctrl Pts',(44.3039519999358,36.5653833249849,47.6890885875231));
#25408=CARTESIAN_POINT('Ctrl Pts',(44.3072925900086,36.5639860587674,47.7104143400978));
#25409=CARTESIAN_POINT('Ctrl Pts',(44.3086334566281,36.5633967640545,47.7193878088022));
#25410=CARTESIAN_POINT('Ctrl Pts',(44.3110829109165,36.5622629949858,47.73661066461));
#25411=CARTESIAN_POINT('Ctrl Pts',(44.3122015101052,36.561718852178,47.744858440342));
#25412=CARTESIAN_POINT('Ctrl Pts',(44.3147090216696,36.5604338947866,47.7642905694446));
#25413=CARTESIAN_POINT('Ctrl Pts',(44.3160533535948,36.5596916883663,47.7754802674773));
#25414=CARTESIAN_POINT('Ctrl Pts',(44.3204036438068,36.5570898788824,47.8145804208853));
#25415=CARTESIAN_POINT('Ctrl Pts',(44.3228982653626,36.5552143506592,47.8425430372192));
#25416=CARTESIAN_POINT('Ctrl Pts',(44.3367613252612,36.5412730738972,48.0486700571453));
#25417=CARTESIAN_POINT('Ctrl Pts',(44.3239545659027,36.5284201795127,48.2275668539296));
#25418=CARTESIAN_POINT('Ctrl Pts',(44.2724220942797,36.510858713565,48.4693708413194));
#25419=CARTESIAN_POINT('Ctrl Pts',(44.254496451837,36.5060264124634,48.5358342369383));
#25420=CARTESIAN_POINT('Ctrl Pts',(44.2283007855537,36.5003168344293,48.6157042070648));
#25421=CARTESIAN_POINT('Ctrl Pts',(44.2233729200037,36.4992883665514,48.6301481282379));
#25422=CARTESIAN_POINT('Ctrl Pts',(44.2160230574539,36.4978193823372,48.6508826325433));
#25423=CARTESIAN_POINT('Ctrl Pts',(44.213738836856,36.4973713342049,48.6572209534226));
#25424=CARTESIAN_POINT('Ctrl Pts',(44.2096953084201,36.4965929570195,48.6682594039745));
#25425=CARTESIAN_POINT('Ctrl Pts',(44.2079507998602,36.4962617701558,48.6729648192413));
#25426=CARTESIAN_POINT('Ctrl Pts',(44.2042011645192,36.4955597100276,48.6829587847218));
#25427=CARTESIAN_POINT('Ctrl Pts',(44.2021911305572,36.4951891316179,48.6882453593436));
#25428=CARTESIAN_POINT('Ctrl Pts',(44.1966231514421,36.4941780102849,48.7026980015945));
#25429=CARTESIAN_POINT('Ctrl Pts',(44.193018276199,36.4935401974951,48.7118459811861));
#25430=CARTESIAN_POINT('Ctrl Pts',(44.1750204674084,36.4904347231155,48.7565141793475));
#25431=CARTESIAN_POINT('Ctrl Pts',(44.1596401187362,36.4880208939262,48.7916302674852));
#25432=CARTESIAN_POINT('Ctrl Pts',(44.1279568928906,36.4834364418977,48.8584741371831));
#25433=CARTESIAN_POINT('Ctrl Pts',(44.1118009444526,36.4812615443856,48.8902531256488));
#25434=CARTESIAN_POINT('Ctrl Pts',(44.0399735493278,36.4721678416991,49.0223445057281));
#25435=CARTESIAN_POINT('Ctrl Pts',(43.9762943400279,36.4654331111313,49.118033451548));
#25436=CARTESIAN_POINT('Ctrl Pts',(43.8514954980191,36.45338344161,49.2735271518019));
#25437=CARTESIAN_POINT('Ctrl Pts',(43.7942187906395,36.448175242888,49.3359872341358));
#25438=CARTESIAN_POINT('Ctrl Pts',(43.7203131965847,36.441669558159,49.4066361040174));
#25439=CARTESIAN_POINT('Ctrl Pts',(43.7074307665747,36.4405429847606,49.4186179273792));
#25440=CARTESIAN_POINT('Ctrl Pts',(43.6868665142056,36.4387551053353,49.4372264922803));
#25441=CARTESIAN_POINT('Ctrl Pts',(43.6792930037712,36.4380988387308,49.4439718901251));
#25442=CARTESIAN_POINT('Ctrl Pts',(43.6649993634062,36.4368641080045,49.4565018993982));
#25443=CARTESIAN_POINT('Ctrl Pts',(43.658291831643,36.4362862511102,49.4623005280588));
#25444=CARTESIAN_POINT('Ctrl Pts',(43.6431668386492,36.4349865607776,49.4751948915058));
#25445=CARTESIAN_POINT('Ctrl Pts',(43.6347281860772,36.4342637069014,49.4822651768796));
#25446=CARTESIAN_POINT('Ctrl Pts',(43.6130673077097,36.4324137424148,49.5001003179589));
#25447=CARTESIAN_POINT('Ctrl Pts',(43.5997622665717,36.4312825516223,49.5107626315234));
#25448=CARTESIAN_POINT('Ctrl Pts',(43.4995172303082,36.4227955398117,49.5889369836959));
#25449=CARTESIAN_POINT('Ctrl Pts',(43.4070974827407,36.4151513156321,49.6490621791765));
#25450=CARTESIAN_POINT('Ctrl Pts',(43.1829061684697,36.3971160210018,49.7690111933048));
#25451=CARTESIAN_POINT('Ctrl Pts',(43.0485107674243,36.3866510859355,49.8225748784175));
#25452=CARTESIAN_POINT('Ctrl Pts',(42.8890322850437,36.3753309627018,49.8662357383775));
#25453=CARTESIAN_POINT('Ctrl Pts',(42.8685753319509,36.3738995615024,49.8714768649011));
#25454=CARTESIAN_POINT('Ctrl Pts',(42.8405868291907,36.3719729664018,49.8781598568549));
#25455=CARTESIAN_POINT('Ctrl Pts',(42.8331275368688,36.3714625620198,49.8798940777791));
#25456=CARTESIAN_POINT('Ctrl Pts',(42.820605372883,36.3706110741624,49.8827268820315));
#25457=CARTESIAN_POINT('Ctrl Pts',(42.8155481055648,36.3702686449195,49.8838495603618));
#25458=CARTESIAN_POINT('Ctrl Pts',(42.8059188798285,36.3696194950306,49.8859465184157));
#25459=CARTESIAN_POINT('Ctrl Pts',(42.801347822297,36.3693125532805,49.8869245703072));
#25460=CARTESIAN_POINT('Ctrl Pts',(42.7904597057428,36.3685842165975,49.8892129037964));
#25461=CARTESIAN_POINT('Ctrl Pts',(42.7841394904624,36.3681636698291,49.8905081413376));
#25462=CARTESIAN_POINT('Ctrl Pts',(42.7616836474814,36.366676981367,49.8949928816099));
#25463=CARTESIAN_POINT('Ctrl Pts',(42.7455133236641,36.3656201846239,49.8980078157847));
#25464=CARTESIAN_POINT('Ctrl Pts',(42.6299433809009,36.3581522688903,49.9180296674882));
#25465=CARTESIAN_POINT('Ctrl Pts',(42.5293706754951,36.3520959837909,49.9274284002903));
#25466=CARTESIAN_POINT('Ctrl Pts',(42.3232388480361,36.3397833729224,49.9304754319349));
#25467=CARTESIAN_POINT('Ctrl Pts',(42.2180195067605,36.3335462658379,49.9234108632692));
#25468=CARTESIAN_POINT('Ctrl Pts',(42.0750336026653,36.3246833716208,49.9019685403077));
#25469=CARTESIAN_POINT('Ctrl Pts',(42.036351914111,36.3222474545379,49.8949531028532));
#25470=CARTESIAN_POINT('Ctrl Pts',(41.9702743615923,36.3180003441819,49.880871349407));
#25471=CARTESIAN_POINT('Ctrl Pts',(41.9427694664882,36.3162065200763,49.8743748999336));
#25472=CARTESIAN_POINT('Ctrl Pts',(41.9035994731228,36.313609944394,49.8642097963953));
#25473=CARTESIAN_POINT('Ctrl Pts',(41.8918102943711,36.312822949022,49.8610305907989));
#25474=CARTESIAN_POINT('Ctrl Pts',(41.8713651988944,36.3114481890472,49.8553083790504));
#25475=CARTESIAN_POINT('Ctrl Pts',(41.8626953763152,36.3108620910395,49.8528161460451));
#25476=CARTESIAN_POINT('Ctrl Pts',(41.8448952240478,36.3096521723843,49.847563861332));
#25477=CARTESIAN_POINT('Ctrl Pts',(41.8357672619247,36.309028133631,49.8447967220602));
#25478=CARTESIAN_POINT('Ctrl Pts',(41.8157889717394,36.3076542533022,49.8385781649168));
#25479=CARTESIAN_POINT('Ctrl Pts',(41.8049480515291,36.3069034943769,49.835098188119));
#25480=CARTESIAN_POINT('Ctrl Pts',(41.7941388317569,36.3061495715672,49.8315225365021));
#25481=CARTESIAN_POINT('Origin',(42.4,48.4493818343519,48.));
#25482=CARTESIAN_POINT('',(41.7941388318214,35.3402141276758,49.8315225365235));
#25483=CARTESIAN_POINT('',(41.7941383590443,35.5100558711261,49.8315223801304));
#25484=CARTESIAN_POINT('',(41.7941388317924,48.4493818343519,49.8315225365138));
#25485=CARTESIAN_POINT('Ctrl Pts',(41.7941388318214,35.3402141276758,49.8315225365234));
#25486=CARTESIAN_POINT('Ctrl Pts',(41.8033302780717,35.3409038661738,49.8345630343887));
#25487=CARTESIAN_POINT('Ctrl Pts',(41.812544588084,35.3415928991055,49.8375343336986));
#25488=CARTESIAN_POINT('Ctrl Pts',(41.8888872174798,35.3472800816834,49.8615192786733));
#25489=CARTESIAN_POINT('Ctrl Pts',(41.9571036059003,35.3522261553391,49.8789186026669));
#25490=CARTESIAN_POINT('Ctrl Pts',(42.0412603432048,35.3580545162817,49.8955438416919));
#25491=CARTESIAN_POINT('Ctrl Pts',(42.056432293349,35.3590945200303,49.8983524080361));
#25492=CARTESIAN_POINT('Ctrl Pts',(42.0783062494708,35.3605769491042,49.9021307776737));
#25493=CARTESIAN_POINT('Ctrl Pts',(42.084981757483,35.3610270909399,49.9032477176702));
#25494=CARTESIAN_POINT('Ctrl Pts',(42.0966222704121,35.3618079237036,49.9051324751577));
#25495=CARTESIAN_POINT('Ctrl Pts',(42.101584594612,35.3621394880998,49.9059160639689));
#25496=CARTESIAN_POINT('Ctrl Pts',(42.1121266725425,35.3628410595028,49.907538555089));
#25497=CARTESIAN_POINT('Ctrl Pts',(42.1177070830929,35.3632107806761,49.9083723700837));
#25498=CARTESIAN_POINT('Ctrl Pts',(42.1329564517591,35.3642167901322,49.9105825500303));
#25499=CARTESIAN_POINT('Ctrl Pts',(42.1426324898158,35.3648503952973,49.9119100166115));
#25500=CARTESIAN_POINT('Ctrl Pts',(42.1895318375846,35.367900406053,49.9179816883714));
#25501=CARTESIAN_POINT('Ctrl Pts',(42.2268808268281,35.3702652685993,49.9217129844686));
#25502=CARTESIAN_POINT('Ctrl Pts',(42.300000531919,35.3748117286257,49.9268685110003));
#25503=CARTESIAN_POINT('Ctrl Pts',(42.3357481680346,35.3769958187494,49.928391581943));
#25504=CARTESIAN_POINT('Ctrl Pts',(42.4868752137132,35.3861408098428,49.9306230087209));
#25505=CARTESIAN_POINT('Ctrl Pts',(42.6021524449234,35.392912627826,49.921975047383));
#25506=CARTESIAN_POINT('Ctrl Pts',(42.7996080457485,35.4050085530928,49.8891914717841));
#25507=CARTESIAN_POINT('Ctrl Pts',(42.8822316284253,35.4102238279034,49.869807742403));
#25508=CARTESIAN_POINT('Ctrl Pts',(42.9801412610197,35.4167376910143,49.8399153541119));
#25509=CARTESIAN_POINT('Ctrl Pts',(42.9969046888878,35.4178648489885,49.8345454893335));
#25510=CARTESIAN_POINT('Ctrl Pts',(43.0232107565205,35.4196535666268,49.8257200899659));
#25511=CARTESIAN_POINT('Ctrl Pts',(43.0328038950717,35.4203100808338,49.822417273238));
#25512=CARTESIAN_POINT('Ctrl Pts',(43.0507333286609,35.4215452250147,49.8160857227827));
#25513=CARTESIAN_POINT('Ctrl Pts',(43.0590756871328,35.4221232469345,49.8130748610368));
#25514=CARTESIAN_POINT('Ctrl Pts',(43.0777281259963,35.4234232414845,49.8061972180578));
#25515=CARTESIAN_POINT('Ctrl Pts',(43.0880263890052,35.4241462345755,49.8022994986282));
#25516=CARTESIAN_POINT('Ctrl Pts',(43.1141855822169,35.4259964313371,49.7921418074748));
#25517=CARTESIAN_POINT('Ctrl Pts',(43.1299976406923,35.4271277151774,49.7857594229469));
#25518=CARTESIAN_POINT('Ctrl Pts',(43.2470824220886,35.435603420777,49.736684380505));
#25519=CARTESIAN_POINT('Ctrl Pts',(43.3446088698674,35.4432352910934,49.6856238950551));
#25520=CARTESIAN_POINT('Ctrl Pts',(43.5589761464888,35.461268422096,49.5489225952098));
#25521=CARTESIAN_POINT('Ctrl Pts',(43.6716094957436,35.4717449957763,49.4578747941354));
#25522=CARTESIAN_POINT('Ctrl Pts',(43.7878719216008,35.48307648185,49.3400747652066));
#25523=CARTESIAN_POINT('Ctrl Pts',(43.8024642967664,35.4845086051447,49.3247953932939));
#25524=CARTESIAN_POINT('Ctrl Pts',(43.8220027532965,35.4864360967266,49.3036523365457));
#25525=CARTESIAN_POINT('Ctrl Pts',(43.8271686096639,35.4869466903525,49.2979949959321));
#25526=CARTESIAN_POINT('Ctrl Pts',(43.835772045806,35.4877984753721,49.2884595614572));
#25527=CARTESIAN_POINT('Ctrl Pts',(43.8392279069567,35.4881410136081,49.2845981640024));
#25528=CARTESIAN_POINT('Ctrl Pts',(43.8457724308015,35.4887903607895,49.2772260952095));
#25529=CARTESIAN_POINT('Ctrl Pts',(43.8488639442129,35.4890973910311,49.273718058393));
#25530=CARTESIAN_POINT('Ctrl Pts',(43.8561917023474,35.4898259320701,49.2653418221002));
#25531=CARTESIAN_POINT('Ctrl Pts',(43.860416368106,35.4902465942611,49.2604635002365));
#25532=CARTESIAN_POINT('Ctrl Pts',(43.8753241716578,35.4917336682518,49.2430735336266));
#25533=CARTESIAN_POINT('Ctrl Pts',(43.8858720069806,35.4927907305562,49.2304461157585));
#25534=CARTESIAN_POINT('Ctrl Pts',(43.9595323284834,35.5002207476962,49.1399343489077));
#25535=CARTESIAN_POINT('Ctrl Pts',(44.0166592637935,35.5062431981322,49.0573596350628));
#25536=CARTESIAN_POINT('Ctrl Pts',(44.1203081332262,35.5185469002135,48.8793511025263));
#25537=CARTESIAN_POINT('Ctrl Pts',(44.1659006178351,35.5248081372512,48.7837806045677));
#25538=CARTESIAN_POINT('Ctrl Pts',(44.2174211053208,35.5337019972348,48.6481318962427));
#25539=CARTESIAN_POINT('Ctrl Pts',(44.2302762596672,35.5361431828442,48.6108870151002));
#25540=CARTESIAN_POINT('Ctrl Pts',(44.25039427698,35.5403987310147,48.5462462604069));
#25541=CARTESIAN_POINT('Ctrl Pts',(44.2582104534106,35.5421956313585,48.5190353903268));
#25542=CARTESIAN_POINT('Ctrl Pts',(44.2685394077921,35.5447960126869,48.4798462116819));
#25543=CARTESIAN_POINT('Ctrl Pts',(44.2715416178398,35.545583675958,48.4679998576269));
#25544=CARTESIAN_POINT('Ctrl Pts',(44.2765648423415,35.5469593518779,48.4473571233139));
#25545=CARTESIAN_POINT('Ctrl Pts',(44.2786370790861,35.5475456933324,48.4385735100676));
#25546=CARTESIAN_POINT('Ctrl Pts',(44.282517747946,35.5486812991517,48.4215921666877));
#25547=CARTESIAN_POINT('Ctrl Pts',(44.2843344549966,35.5492302823014,48.413396521851));
#25548=CARTESIAN_POINT('Ctrl Pts',(44.2885229323607,35.5505385452273,48.3938997697985));
#25549=CARTESIAN_POINT('Ctrl Pts',(44.2908468160997,35.5512993411058,48.3825888169371));
#25550=CARTESIAN_POINT('Ctrl Pts',(44.298795008162,35.5540322159728,48.3420604505009));
#25551=CARTESIAN_POINT('Ctrl Pts',(44.3038445068806,35.5560223998313,48.3127359274706));
#25552=CARTESIAN_POINT('Ctrl Pts',(44.3341200523289,35.5699575131201,48.1088155663776));
#25553=CARTESIAN_POINT('Ctrl Pts',(44.3359651641253,35.5826613566377,47.9316181871203));
#25554=CARTESIAN_POINT('Ctrl Pts',(44.3050852516379,35.6000507892934,47.6887364079094));
#25555=CARTESIAN_POINT('Ctrl Pts',(44.2928315150079,35.6048625665033,47.6212842600879));
#25556=CARTESIAN_POINT('Ctrl Pts',(44.2734970491747,35.6105508409513,47.5398007282598));
#25557=CARTESIAN_POINT('Ctrl Pts',(44.2698049527442,35.6115773539234,47.5250220664612));
#25558=CARTESIAN_POINT('Ctrl Pts',(44.2642288070903,35.6130441499113,47.5037754048378));
#25559=CARTESIAN_POINT('Ctrl Pts',(44.2624854373206,35.6134919328008,47.4972715512534));
#25560=CARTESIAN_POINT('Ctrl Pts',(44.2593831730957,35.6142700898996,47.4859358376487));
#25561=CARTESIAN_POINT('Ctrl Pts',(44.2580394246438,35.6146013193269,47.4810999651133));
#25562=CARTESIAN_POINT('Ctrl Pts',(44.2551399889293,35.6153037434277,47.470821182123));
#25563=CARTESIAN_POINT('Ctrl Pts',(44.2535792094199,35.615674641107,47.4653798392673));
#25564=CARTESIAN_POINT('Ctrl Pts',(44.2492369480064,35.6166872387055,47.4504890420384));
#25565=CARTESIAN_POINT('Ctrl Pts',(44.2464069623751,35.6173261962535,47.441053739516));
#25566=CARTESIAN_POINT('Ctrl Pts',(44.2321571334049,35.6204450335939,47.3948336665334));
#25567=CARTESIAN_POINT('Ctrl Pts',(44.2197088382456,35.6228705310141,47.3583721736087));
#25568=CARTESIAN_POINT('Ctrl Pts',(44.1936662520892,35.627464050469,47.2889640981841));
#25569=CARTESIAN_POINT('Ctrl Pts',(44.1802349988333,35.6296367702057,47.2559742891568));
#25570=CARTESIAN_POINT('Ctrl Pts',(44.1197835874882,35.6387176826446,47.1185194841136));
#25571=CARTESIAN_POINT('Ctrl Pts',(44.0644222262479,35.6454430282479,47.0179800221821));
#25572=CARTESIAN_POINT('Ctrl Pts',(43.9532145863593,35.6574809902782,46.8527293430705));
#25573=CARTESIAN_POINT('Ctrl Pts',(43.9013984947038,35.6626874036156,46.7857078552327));
#25574=CARTESIAN_POINT('Ctrl Pts',(43.833701161272,35.6691912866582,46.7091269959231));
#25575=CARTESIAN_POINT('Ctrl Pts',(43.8218684200407,35.6703179789034,46.6961049522164));
#25576=CARTESIAN_POINT('Ctrl Pts',(43.8029354741763,35.672106124299,46.6758332745595));
#25577=CARTESIAN_POINT('Ctrl Pts',(43.7959531686412,35.6727625375185,46.6684744816957));
#25578=CARTESIAN_POINT('Ctrl Pts',(43.78275794,35.6739975928945,46.6547856305013));
#25579=CARTESIAN_POINT('Ctrl Pts',(43.7765587457916,35.674575627863,46.6484426628917));
#25580=CARTESIAN_POINT('Ctrl Pts',(43.7625640817177,35.6758757853019,46.6343195922553));
#25581=CARTESIAN_POINT('Ctrl Pts',(43.7547453335138,35.6765989293644,46.6265630973217));
#25582=CARTESIAN_POINT('Ctrl Pts',(43.7346478432983,35.678449773532,46.6069642174193));
#25583=CARTESIAN_POINT('Ctrl Pts',(43.7222778648127,35.6795815587051,46.5952171792515));
#25584=CARTESIAN_POINT('Ctrl Pts',(43.628538139522,35.6881056045999,46.5085332549671));
#25585=CARTESIAN_POINT('Ctrl Pts',(43.5410273426897,35.6957892969913,46.4405680380701));
#25586=CARTESIAN_POINT('Ctrl Pts',(43.3275591281659,35.7138287250294,46.3024062509263));
#25587=CARTESIAN_POINT('Ctrl Pts',(43.1985800840218,35.7242535564755,46.2380513281266));
#25588=CARTESIAN_POINT('Ctrl Pts',(43.0438461358926,35.7355353344091,46.1813605534341));
#25589=CARTESIAN_POINT('Ctrl Pts',(43.0239260948757,35.7369648983567,46.1744306089116));
#25590=CARTESIAN_POINT('Ctrl Pts',(42.9966245569341,35.7388895376939,46.1654318480802));
#25591=CARTESIAN_POINT('Ctrl Pts',(42.9893393207583,35.7393997819224,46.1630785711183));
#25592=CARTESIAN_POINT('Ctrl Pts',(42.9771006999296,35.7402511479475,46.1592055573119));
#25593=CARTESIAN_POINT('Ctrl Pts',(42.9721549114014,35.7405936137911,46.1576623117492));
#25594=CARTESIAN_POINT('Ctrl Pts',(42.9627328283422,35.7412429501227,46.1547639194843));
#25595=CARTESIAN_POINT('Ctrl Pts',(42.9582577449077,35.7415500410646,46.1534051011798));
#25596=CARTESIAN_POINT('Ctrl Pts',(42.9475924973663,35.742278885269,46.1502090101486));
#25597=CARTESIAN_POINT('Ctrl Pts',(42.9413979146882,35.7426997882691,46.1483865008586));
#25598=CARTESIAN_POINT('Ctrl Pts',(42.9193670539494,35.7441885097917,46.142024810198));
#25599=CARTESIAN_POINT('Ctrl Pts',(42.9034813877032,35.7452469520633,46.1376572607379));
#25600=CARTESIAN_POINT('Ctrl Pts',(42.7882470058594,35.7528297287946,46.1075574467411));
#25601=CARTESIAN_POINT('Ctrl Pts',(42.6870280143813,35.7589864323924,46.089582520301));
#25602=CARTESIAN_POINT('Ctrl Pts',(42.4776974887853,35.7715431291362,46.0694318675237));
#25603=CARTESIAN_POINT('Ctrl Pts',(42.3698779855397,35.7779231960003,46.0681042451951));
#25604=CARTESIAN_POINT('Ctrl Pts',(42.2068783852868,35.7879645727898,46.0797506246203));
#25605=CARTESIAN_POINT('Ctrl Pts',(42.1514464770122,35.7914472096446,46.0861364021845));
#25606=CARTESIAN_POINT('Ctrl Pts',(42.080927083342,35.7960033896666,46.0973755869808));
#25607=CARTESIAN_POINT('Ctrl Pts',(42.0655123784125,35.7970070020544,46.1000249499417));
#25608=CARTESIAN_POINT('Ctrl Pts',(42.0405744557355,35.7986438912036,46.10462397202));
#25609=CARTESIAN_POINT('Ctrl Pts',(42.0310305653726,35.7992734978333,46.1064587250703));
#25610=CARTESIAN_POINT('Ctrl Pts',(42.0127209129363,35.8004876402576,46.1101223204696));
#25611=CARTESIAN_POINT('Ctrl Pts',(42.0039532022826,35.8010718120072,46.111940238151));
#25612=CARTESIAN_POINT('Ctrl Pts',(41.9838884793858,35.8024151841456,46.1162464148082));
#25613=CARTESIAN_POINT('Ctrl Pts',(41.9726006469372,35.8031756731564,46.1187753588755));
#25614=CARTESIAN_POINT('Ctrl Pts',(41.9366831413262,35.8056110576489,46.1271623213788));
#25615=CARTESIAN_POINT('Ctrl Pts',(41.9121466022736,35.8072981816249,46.1334035143323));
#25616=CARTESIAN_POINT('Ctrl Pts',(41.7579383176441,35.8180550401724,46.1758765896848));
#25617=CARTESIAN_POINT('Ctrl Pts',(41.6322578000882,35.8275517630079,46.2251115547733));
#25618=CARTESIAN_POINT('Ctrl Pts',(41.4467387002653,35.8424713223208,46.3212023606692));
#25619=CARTESIAN_POINT('Ctrl Pts',(41.3827593667456,35.8477938873122,46.3591798238934));
#25620=CARTESIAN_POINT('Ctrl Pts',(41.2927309666345,35.8554231763513,46.4199141275866));
#25621=CARTESIAN_POINT('Ctrl Pts',(41.2648458632006,35.8578067979939,46.4398264707362));
#25622=CARTESIAN_POINT('Ctrl Pts',(41.2201887959747,35.8616405563775,46.4735469672153));
#25623=CARTESIAN_POINT('Ctrl Pts',(41.2030941675991,35.8631122080513,46.4869137947167));
#25624=CARTESIAN_POINT('Ctrl Pts',(41.1802122628839,35.8650836733035,46.5054364072132));
#25625=CARTESIAN_POINT('Ctrl Pts',(41.1742259127801,35.8655995971504,46.5103422041754));
#25626=CARTESIAN_POINT('Ctrl Pts',(41.1642684820652,35.866457782343,46.5186029589881));
#25627=CARTESIAN_POINT('Ctrl Pts',(41.1602811984603,35.8668014332912,46.5219381363983));
#25628=CARTESIAN_POINT('Ctrl Pts',(41.1527438123534,35.8674509862469,46.5282947679145));
#25629=CARTESIAN_POINT('Ctrl Pts',(41.1491911117259,35.8677571222345,46.5313130306487));
#25630=CARTESIAN_POINT('Ctrl Pts',(41.1407890093403,35.8684811643652,46.5385037929997));
#25631=CARTESIAN_POINT('Ctrl Pts',(41.1359493155519,35.8688982464469,46.5426876271479));
#25632=CARTESIAN_POINT('Ctrl Pts',(41.1189902317767,35.870360238262,46.5574965177927));
#25633=CARTESIAN_POINT('Ctrl Pts',(41.1069828718956,35.8713962040948,46.5682496482087));
#25634=CARTESIAN_POINT('Ctrl Pts',(41.0096141195906,35.879817860873,46.6576719015802));
#25635=CARTESIAN_POINT('Ctrl Pts',(40.9313663533926,35.8867284689508,46.743759473144));
#25636=CARTESIAN_POINT('Ctrl Pts',(40.8021594920841,35.8995046798798,46.9146104820451));
#25637=CARTESIAN_POINT('Ctrl Pts',(40.7490474419872,35.9053478185504,46.9972445070508));
#25638=CARTESIAN_POINT('Ctrl Pts',(40.6857641258392,35.9135497513982,47.1144651653818));
#25639=CARTESIAN_POINT('Ctrl Pts',(40.6699242881312,35.9157351135803,47.1458253177254));
#25640=CARTESIAN_POINT('Ctrl Pts',(40.6438905627417,35.9195831747945,47.201066198481));
#25641=CARTESIAN_POINT('Ctrl Pts',(40.6333060076736,35.921232701729,47.2247530651251));
#25642=CARTESIAN_POINT('Ctrl Pts',(40.6186040843262,35.9236566831083,47.2595200502337));
#25643=CARTESIAN_POINT('Ctrl Pts',(40.6141054950346,35.9244181856518,47.2704365885575));
#25644=CARTESIAN_POINT('Ctrl Pts',(40.6063698229777,35.9257635656237,47.2897087723692));
#25645=CARTESIAN_POINT('Ctrl Pts',(40.6030901870596,35.9263459855643,47.2980470389086));
#25646=CARTESIAN_POINT('Ctrl Pts',(40.5963810828625,35.9275630733627,47.3154596721654));
#25647=CARTESIAN_POINT('Ctrl Pts',(40.5929617435125,35.9281980620767,47.3245376454294));
#25648=CARTESIAN_POINT('Ctrl Pts',(40.5842371558487,35.9298574775942,47.3482409257297));
#25649=CARTESIAN_POINT('Ctrl Pts',(40.5790401940719,35.9308854772998,47.362905063542));
#25650=CARTESIAN_POINT('Ctrl Pts',(40.558040970974,35.9352113449188,47.4245149422172));
#25651=CARTESIAN_POINT('Ctrl Pts',(40.5438736871017,35.9385621867252,47.4719938729788));
#25652=CARTESIAN_POINT('Ctrl Pts',(40.5232940881895,35.9442469674777,47.5520957435843));
#25653=CARTESIAN_POINT('Ctrl Pts',(40.5158690386701,35.946550328313,47.5844357698192));
#25654=CARTESIAN_POINT('Ctrl Pts',(40.4836525613635,35.9579079144048,47.7434548103538));
#25655=CARTESIAN_POINT('Ctrl Pts',(40.4707855165445,35.9672308213055,47.8722096932965));
#25656=CARTESIAN_POINT('Ctrl Pts',(40.4708892210066,35.9783792649736,48.0298529101713));
#25657=CARTESIAN_POINT('Ctrl Pts',(40.4715433127891,35.980388420854,48.058433939243));
#25658=CARTESIAN_POINT('Ctrl Pts',(40.4745029935232,35.9849562189986,48.1240017126534));
#25659=CARTESIAN_POINT('Ctrl Pts',(40.4772396008765,35.9875006195136,48.160959697775));
#25660=CARTESIAN_POINT('Ctrl Pts',(40.4820365303732,35.9906477441484,48.2074928195425));
#25661=CARTESIAN_POINT('Ctrl Pts',(40.483106973208,35.9912984267554,48.2171595602671));
#25662=CARTESIAN_POINT('Ctrl Pts',(40.48491283704,35.9923197775349,48.2324122391863));
#25663=CARTESIAN_POINT('Ctrl Pts',(40.4855996816826,35.9926930533686,48.2380036006194));
#25664=CARTESIAN_POINT('Ctrl Pts',(40.4869456863818,35.9933967447851,48.2485779822284));
#25665=CARTESIAN_POINT('Ctrl Pts',(40.4875998221225,35.9937274159223,48.2535613935973));
#25666=CARTESIAN_POINT('Ctrl Pts',(40.4891828443403,35.9945019400442,48.2652666539683));
#25667=CARTESIAN_POINT('Ctrl Pts',(40.4901277284859,35.994944890912,48.2719862312696));
#25668=CARTESIAN_POINT('Ctrl Pts',(40.4933512971333,35.9963952288634,48.2940652637638));
#25669=CARTESIAN_POINT('Ctrl Pts',(40.495780033281,35.9973945932102,48.3094026678246));
#25670=CARTESIAN_POINT('Ctrl Pts',(40.5103908968587,36.0029329080415,48.3949686755102));
#25671=CARTESIAN_POINT('Ctrl Pts',(40.5262740071337,36.0072954823843,48.4645169124358));
#25672=CARTESIAN_POINT('Ctrl Pts',(40.5600992665858,36.0146766533295,48.582169941512));
#25673=CARTESIAN_POINT('Ctrl Pts',(40.5761742080762,36.0177232058786,48.6307267644071));
#25674=CARTESIAN_POINT('Ctrl Pts',(40.6395398287821,36.0284671413047,48.7993535669446));
#25675=CARTESIAN_POINT('Ctrl Pts',(40.6969134736692,36.0361772909899,48.9152470742577));
#25676=CARTESIAN_POINT('Ctrl Pts',(40.778941962411,36.0459147116489,49.0461174750438));
#25677=CARTESIAN_POINT('Ctrl Pts',(40.7928905407786,36.047534341355,49.0674221386184));
#25678=CARTESIAN_POINT('Ctrl Pts',(40.8137977561194,36.0499142845872,49.0980161298463));
#25679=CARTESIAN_POINT('Ctrl Pts',(40.8204253568025,36.0506621232496,49.1075291945575));
#25680=CARTESIAN_POINT('Ctrl Pts',(40.8323250300456,36.0519936024174,49.1242855482265));
#25681=CARTESIAN_POINT('Ctrl Pts',(40.8375626076014,36.0525759063517,49.1315530017028));
#25682=CARTESIAN_POINT('Ctrl Pts',(40.8485803594892,36.053793269538,49.1466184507041));
#25683=CARTESIAN_POINT('Ctrl Pts',(40.8543691393466,36.0544286532587,49.1544098099055));
#25684=CARTESIAN_POINT('Ctrl Pts',(40.8696049201544,36.0560902556816,49.1745962434354));
#25685=CARTESIAN_POINT('Ctrl Pts',(40.8791436051263,36.0571200648081,49.1869209060955));
#25686=CARTESIAN_POINT('Ctrl Pts',(40.9231176019948,36.0618218832734,49.2423379684117));
#25687=CARTESIAN_POINT('Ctrl Pts',(40.9592390822894,36.0655610290211,49.2840530303269));
#25688=CARTESIAN_POINT('Ctrl Pts',(41.0695135055077,36.0766418746174,49.4008852294146));
#25689=CARTESIAN_POINT('Ctrl Pts',(41.1480967349268,36.0841481440338,49.471532332966));
#25690=CARTESIAN_POINT('Ctrl Pts',(41.2700500592625,36.0950946170216,49.5643002220425));
#25691=CARTESIAN_POINT('Ctrl Pts',(41.3091103143498,36.0985054552505,49.5917857678542));
#25692=CARTESIAN_POINT('Ctrl Pts',(41.4045201770809,36.106562000376,49.6537598907998));
#25693=CARTESIAN_POINT('Ctrl Pts',(41.4617059300286,36.1111761188832,49.6868633639615));
#25694=CARTESIAN_POINT('Ctrl Pts',(41.5296176820638,36.1163260843162,49.7216511038361));
#25695=CARTESIAN_POINT('Ctrl Pts',(41.538790164072,36.117014927706,49.7262576668846));
#25696=CARTESIAN_POINT('Ctrl Pts',(41.5537069929559,36.1181237784755,49.7336006392286));
#25697=CARTESIAN_POINT('Ctrl Pts',(41.5594287343966,36.1185464174024,49.7363821527584));
#25698=CARTESIAN_POINT('Ctrl Pts',(41.5696542805438,36.1192968091254,49.7412907135717));
#25699=CARTESIAN_POINT('Ctrl Pts',(41.574152661941,36.1196252218318,49.7434286733582));
#25700=CARTESIAN_POINT('Ctrl Pts',(41.583996553106,36.1203401805565,49.748060560429));
#25701=CARTESIAN_POINT('Ctrl Pts',(41.5893452434245,36.1207262923272,49.7505474047297));
#25702=CARTESIAN_POINT('Ctrl Pts',(41.6046568312521,36.1218251110056,49.7575812161948));
#25703=CARTESIAN_POINT('Ctrl Pts',(41.6146473479717,36.1225342477433,49.7620680217135));
#25704=CARTESIAN_POINT('Ctrl Pts',(41.6801092164973,36.1271334040668,49.7908000016156));
#25705=CARTESIAN_POINT('Ctrl Pts',(41.736659542496,36.1308858498512,49.8125085912373));
#25706=CARTESIAN_POINT('Ctrl Pts',(41.7941388330275,36.1345714126848,49.8315225369224));
#25707=CARTESIAN_POINT('Ctrl Pts',(41.7941388317569,36.3061495715672,49.8315225365021));
#25708=CARTESIAN_POINT('Ctrl Pts',(41.7908818344471,36.3059224021124,49.8304451333276));
#25709=CARTESIAN_POINT('Ctrl Pts',(41.7876277152645,36.3056949455745,49.8293590436659));
#25710=CARTESIAN_POINT('Ctrl Pts',(41.7433255545585,36.3025916264315,49.8144413694751));
#25711=CARTESIAN_POINT('Ctrl Pts',(41.7027548568271,36.2996709716044,49.7992408149969));
#25712=CARTESIAN_POINT('Ctrl Pts',(41.5129913184719,36.2856236380944,49.7207602334871));
#25713=CARTESIAN_POINT('Ctrl Pts',(41.3716646382245,36.2739304407638,49.6402166971355));
#25714=CARTESIAN_POINT('Ctrl Pts',(41.2033214709907,36.2589999196495,49.5138868096297));
#25715=CARTESIAN_POINT('Ctrl Pts',(41.1656541819422,36.2555903400025,49.4833353647865));
#25716=CARTESIAN_POINT('Ctrl Pts',(41.1152000832895,36.2509656751783,49.4391583623508));
#25717=CARTESIAN_POINT('Ctrl Pts',(41.1014013252953,36.2496946090662,49.4267197188221));
#25718=CARTESIAN_POINT('Ctrl Pts',(41.0777227243126,36.2475056167022,49.404746865659));
#25719=CARTESIAN_POINT('Ctrl Pts',(41.0677611731111,36.2465822161296,49.3953030799677));
#25720=CARTESIAN_POINT('Ctrl Pts',(41.0532637890158,36.2452357783986,49.3812623963285));
#25721=CARTESIAN_POINT('Ctrl Pts',(41.0486491424598,36.2448068032589,49.3767480133658));
#25722=CARTESIAN_POINT('Ctrl Pts',(41.040510145783,36.244049651584,49.3687055049526));
#25723=CARTESIAN_POINT('Ctrl Pts',(41.0369767183921,36.2437207650918,49.3651867853233));
#25724=CARTESIAN_POINT('Ctrl Pts',(41.0293438611388,36.2430099399321,49.357526523088));
#25725=CARTESIAN_POINT('Ctrl Pts',(41.0252495324038,36.2426283962253,49.3533800892379));
#25726=CARTESIAN_POINT('Ctrl Pts',(41.013946139364,36.2415741298078,49.3418286232391));
#25727=CARTESIAN_POINT('Ctrl Pts',(41.0067775679538,36.2409044674379,49.3343839871123));
#25728=CARTESIAN_POINT('Ctrl Pts',(40.9674302083481,36.2372204400329,49.2928585671319));
#25729=CARTESIAN_POINT('Ctrl Pts',(40.9364391153363,36.2342874434137,49.2576684068972));
#25730=CARTESIAN_POINT('Ctrl Pts',(40.7958803198214,36.2206358269088,49.0858233743734));
#25731=CARTESIAN_POINT('Ctrl Pts',(40.7039737120503,36.2105604331078,48.9357966911778));
#25732=CARTESIAN_POINT('Ctrl Pts',(40.6117241073231,36.1964440349564,48.7256487404426));
#25733=CARTESIAN_POINT('Ctrl Pts',(40.5919917965607,36.193047714367,48.674983157969));
#25734=CARTESIAN_POINT('Ctrl Pts',(40.5694133467828,36.1885900208047,48.6088805628605));
#25735=CARTESIAN_POINT('Ctrl Pts',(40.56457813582,36.1875948067407,48.5941461036755));
#25736=CARTESIAN_POINT('Ctrl Pts',(40.5570117615196,36.1859683469113,48.5701146930645));
#25737=CARTESIAN_POINT('Ctrl Pts',(40.5541720195687,36.1853406851394,48.5608524506284));
#25738=CARTESIAN_POINT('Ctrl Pts',(40.5488401839491,36.1841280339897,48.5429826767567));
#25739=CARTESIAN_POINT('Ctrl Pts',(40.5463380586566,36.1835433911786,48.534378381351));
#25740=CARTESIAN_POINT('Ctrl Pts',(40.5407276538539,36.1821957008626,48.5145717158341));
#25741=CARTESIAN_POINT('Ctrl Pts',(40.5376605375903,36.181431335032,48.5033581473886));
#25742=CARTESIAN_POINT('Ctrl Pts',(40.5283953939592,36.1790328871414,48.4682398882855));
#25743=CARTESIAN_POINT('Ctrl Pts',(40.5225551060856,36.1773873613241,48.4442442662499));
#25744=CARTESIAN_POINT('Ctrl Pts',(40.4862671368741,36.1661856084915,48.2816243005021));
#25745=CARTESIAN_POINT('Ctrl Pts',(40.4707431824734,36.1561485615077,48.1401412126996));
#25746=CARTESIAN_POINT('Ctrl Pts',(40.4709683571867,36.1382629653343,47.8897689155703));
#25747=CARTESIAN_POINT('Ctrl Pts',(40.4802186425955,36.1305007920714,47.7814640440312));
#25748=CARTESIAN_POINT('Ctrl Pts',(40.5012919379288,36.1219987210722,47.6583590742255));
#25749=CARTESIAN_POINT('Ctrl Pts',(40.5042611201627,36.1208928690299,47.64225012882));
#25750=CARTESIAN_POINT('Ctrl Pts',(40.5086831317974,36.1193671354483,47.619862481187));
#25751=CARTESIAN_POINT('Ctrl Pts',(40.5099626809845,36.1189382312745,47.613550825054));
#25752=CARTESIAN_POINT('Ctrl Pts',(40.5122249145439,36.1182012418579,47.6026719156325));
#25753=CARTESIAN_POINT('Ctrl Pts',(40.5131926166968,36.1178923263549,47.5981016554198));
#25754=CARTESIAN_POINT('Ctrl Pts',(40.5152690945295,36.117242676471,47.5884676923484));
#25755=CARTESIAN_POINT('Ctrl Pts',(40.5163816950951,36.1169021737739,47.5834048622162));
#25756=CARTESIAN_POINT('Ctrl Pts',(40.5191919991851,36.1160604389258,47.5708581706228));
#25757=CARTESIAN_POINT('Ctrl Pts',(40.5209139994945,36.1155605792031,47.5633797379441));
#25758=CARTESIAN_POINT('Ctrl Pts',(40.5275677143037,36.1136868309566,47.53525212076));
#25759=CARTESIAN_POINT('Ctrl Pts',(40.5327957564722,36.1123288065494,47.5146736573835));
#25760=CARTESIAN_POINT('Ctrl Pts',(40.5767323183008,36.1017285302389,47.352966529564));
#25761=CARTESIAN_POINT('Ctrl Pts',(40.6310507611253,36.0931889930527,47.2165540505824));
#25762=CARTESIAN_POINT('Ctrl Pts',(40.7512827782719,36.0779600412097,46.9925768559419));
#25763=CARTESIAN_POINT('Ctrl Pts',(40.810151556689,36.0714072727013,46.9020258410857));
#25764=CARTESIAN_POINT('Ctrl Pts',(40.8867142086564,36.0634773229606,46.803422104243));
#25765=CARTESIAN_POINT('Ctrl Pts',(40.8973354425698,36.0623889670591,46.7901108542115));
#25766=CARTESIAN_POINT('Ctrl Pts',(40.915106928134,36.0605858587203,46.7684334436592));
#25767=CARTESIAN_POINT('Ctrl Pts',(40.9221551601202,36.059875216884,46.7599845813372));
#25768=CARTESIAN_POINT('Ctrl Pts',(40.9350126821654,36.0585865868372,46.7448373322373));
#25769=CARTESIAN_POINT('Ctrl Pts',(40.9407966492126,36.0580096499316,46.738117778635));
#25770=CARTESIAN_POINT('Ctrl Pts',(40.9532987577343,36.056768310838,46.7237942867901));
#25771=CARTESIAN_POINT('Ctrl Pts',(40.9600309578135,36.0561033316268,46.7162030309824));
#25772=CARTESIAN_POINT('Ctrl Pts',(40.9786130049928,36.0542770315661,46.6955798952041));
#25773=CARTESIAN_POINT('Ctrl Pts',(40.9905817006012,36.0531107037025,46.6826569081918));
#25774=CARTESIAN_POINT('Ctrl Pts',(41.0613941440343,36.0462656170772,46.6082681923181));
#25775=CARTESIAN_POINT('Ctrl Pts',(41.1240679172102,36.0404197920014,46.5505943433962));
#25776=CARTESIAN_POINT('Ctrl Pts',(41.2816697756335,36.0262161761693,46.4237299087403));
#25777=CARTESIAN_POINT('Ctrl Pts',(41.3795146820032,36.0177641336662,46.3586905121666));
#25778=CARTESIAN_POINT('Ctrl Pts',(41.5425881991134,36.004625859593,46.2705405070667));
#25779=CARTESIAN_POINT('Ctrl Pts',(41.6042094893347,35.9998586933071,46.2413344087271));
#25780=CARTESIAN_POINT('Ctrl Pts',(41.676822816558,35.9945598539716,46.2115189883723));
#25781=CARTESIAN_POINT('Ctrl Pts',(41.6864238503438,35.9938654994304,46.2076667001465));
#25782=CARTESIAN_POINT('Ctrl Pts',(41.7020003727046,35.9927496242606,46.2015618317022));
#25783=CARTESIAN_POINT('Ctrl Pts',(41.7079567197463,35.9923254182321,46.1992614220683));
#25784=CARTESIAN_POINT('Ctrl Pts',(41.71857971423,35.9915734324963,46.1952191933506));
#25785=CARTESIAN_POINT('Ctrl Pts',(41.7232417949656,35.9912449800183,46.1934658321132));
#25786=CARTESIAN_POINT('Ctrl Pts',(41.7334202243369,35.9905313223843,46.189682760773));
#25787=CARTESIAN_POINT('Ctrl Pts',(41.7389390819324,35.990146540647,46.1876601949854));
#25788=CARTESIAN_POINT('Ctrl Pts',(41.7546796651775,35.9890550258491,46.1819730112076));
#25789=CARTESIAN_POINT('Ctrl Pts',(41.7649234019374,35.9883517901926,46.178369358411));
#25790=CARTESIAN_POINT('Ctrl Pts',(41.836746004218,35.983467054265,46.153782331771));
#25791=CARTESIAN_POINT('Ctrl Pts',(41.8993283958585,35.9794452234469,46.1358367517752));
#25792=CARTESIAN_POINT('Ctrl Pts',(42.0895849158426,35.9675848869307,46.0915567467151));
#25793=CARTESIAN_POINT('Ctrl Pts',(42.2191311079365,35.9599710796708,46.0749541098837));
#25794=CARTESIAN_POINT('Ctrl Pts',(42.4252953261542,35.947460117554,46.0695409812214));
#25795=CARTESIAN_POINT('Ctrl Pts',(42.5012685751251,35.9427705950798,46.0720335745036));
#25796=CARTESIAN_POINT('Ctrl Pts',(42.5943548472393,35.9368236097639,46.0806052236105));
#25797=CARTESIAN_POINT('Ctrl Pts',(42.6117950567736,35.9357008495776,46.0824513211891));
#25798=CARTESIAN_POINT('Ctrl Pts',(42.6393662543867,35.9339112247117,46.0857505290942));
#25799=CARTESIAN_POINT('Ctrl Pts',(42.6495152871925,35.9332493058624,46.0870469542192));
#25800=CARTESIAN_POINT('Ctrl Pts',(42.6684311192652,35.9320095158898,46.0896163313034));
#25801=CARTESIAN_POINT('Ctrl Pts',(42.6772004288766,35.931432300051,46.0908690602191));
#25802=CARTESIAN_POINT('Ctrl Pts',(42.6967285598873,35.9301412959678,46.0937961098347));
#25803=CARTESIAN_POINT('Ctrl Pts',(42.7074823920295,35.9294265480794,46.0955011999353));
#25804=CARTESIAN_POINT('Ctrl Pts',(42.7390791986472,35.9273149556571,46.1007856659793));
#25805=CARTESIAN_POINT('Ctrl Pts',(42.7598778519137,35.9259101769431,46.1046167510428));
#25806=CARTESIAN_POINT('Ctrl Pts',(42.9195269029133,35.9150088225237,46.1367463244995));
#25807=CARTESIAN_POINT('Ctrl Pts',(43.0549154811712,35.905023343791,46.1799194009701));
#25808=CARTESIAN_POINT('Ctrl Pts',(43.2894912819307,35.8866877203995,46.2843087196769));
#25809=CARTESIAN_POINT('Ctrl Pts',(43.3902617793463,35.8784322864802,46.3404284612018));
#25810=CARTESIAN_POINT('Ctrl Pts',(43.4987940954171,35.8694980836158,46.4142965997338));
#25811=CARTESIAN_POINT('Ctrl Pts',(43.5120400941541,35.8684071984331,46.4235576100569));
#25812=CARTESIAN_POINT('Ctrl Pts',(43.530370224039,35.8668986388196,46.4367192449479));
#25813=CARTESIAN_POINT('Ctrl Pts',(43.5355532456459,35.8664721966729,46.4404800765311));
#25814=CARTESIAN_POINT('Ctrl Pts',(43.5444774267305,35.8657382843932,46.4470235952228));
#25815=CARTESIAN_POINT('Ctrl Pts',(43.5482273623742,35.8654299996637,46.4497941363977));
#25816=CARTESIAN_POINT('Ctrl Pts',(43.5561336524867,35.8647803051973,46.4556799187319));
#25817=CARTESIAN_POINT('Ctrl Pts',(43.560287539906,35.8644391347943,46.4587984032688));
#25818=CARTESIAN_POINT('Ctrl Pts',(43.5705879124514,35.8635934273743,46.4665965394425));
#25819=CARTESIAN_POINT('Ctrl Pts',(43.5767190602598,35.8630902914826,46.4712964669936));
#25820=CARTESIAN_POINT('Ctrl Pts',(43.5998868653791,35.8611893685858,46.4892780844755));
#25821=CARTESIAN_POINT('Ctrl Pts',(43.6167289914218,35.8598080454703,46.5028093468635));
#25822=CARTESIAN_POINT('Ctrl Pts',(43.659523046865,35.8562892674483,46.5383900580429));
#25823=CARTESIAN_POINT('Ctrl Pts',(43.6851256357352,35.8541752557778,46.5608494513904));
#25824=CARTESIAN_POINT('Ctrl Pts',(43.7640530244159,35.8475803960898,46.6338739839171));
#25825=CARTESIAN_POINT('Ctrl Pts',(43.8150927130189,35.8431965802839,46.6868150365677));
#25826=CARTESIAN_POINT('Ctrl Pts',(43.9515701068735,35.8307077584285,46.8455996379022));
#25827=CARTESIAN_POINT('Ctrl Pts',(44.0290021969505,35.8226131942831,46.9577157924064));
#25828=CARTESIAN_POINT('Ctrl Pts',(44.1060999263628,35.8124518070186,47.0992202502094));
#25829=CARTESIAN_POINT('Ctrl Pts',(44.1177522934067,35.8108442477041,47.121644673214));
#25830=CARTESIAN_POINT('Ctrl Pts',(44.1340868762421,35.8084789273793,47.1546486936775));
#25831=CARTESIAN_POINT('Ctrl Pts',(44.1391200498942,35.8077334244621,47.1650523561697));
#25832=CARTESIAN_POINT('Ctrl Pts',(44.1478847548956,35.8064047692532,47.1835922879146));
#25833=CARTESIAN_POINT('Ctrl Pts',(44.151653742113,35.805822936036,47.1917105518709));
#25834=CARTESIAN_POINT('Ctrl Pts',(44.159397203458,35.8046052028596,47.2086982265415));
#25835=CARTESIAN_POINT('Ctrl Pts',(44.1633614081801,35.8039689691548,47.2175720132274));
#25836=CARTESIAN_POINT('Ctrl Pts',(44.1735338007928,35.8023021150283,47.2408126986027));
#25837=CARTESIAN_POINT('Ctrl Pts',(44.1796344003739,35.801267860115,47.255225619736));
#25838=CARTESIAN_POINT('Ctrl Pts',(44.2067286928707,35.7965105598589,47.3214712301686));
#25839=CARTESIAN_POINT('Ctrl Pts',(44.2256358791604,35.792718398557,47.3741226822582));
#25840=CARTESIAN_POINT('Ctrl Pts',(44.2743292114223,35.7813950574353,47.5308158564398));
#25841=CARTESIAN_POINT('Ctrl Pts',(44.2976815220094,35.7736898371534,47.6366216758149));
#25842=CARTESIAN_POINT('Ctrl Pts',(44.3255694417088,35.7586877520378,47.8447628892218));
#25843=CARTESIAN_POINT('Ctrl Pts',(44.3310806472305,35.7514197856597,47.9466348595874));
#25844=CARTESIAN_POINT('Ctrl Pts',(44.3281053434859,35.7433574317197,48.0650064486664));
#25845=CARTESIAN_POINT('Ctrl Pts',(44.3274772022601,35.7422406665573,48.0815336351079));
#25846=CARTESIAN_POINT('Ctrl Pts',(44.3263078909733,35.7407023889753,48.1045097348343));
#25847=CARTESIAN_POINT('Ctrl Pts',(44.3259467303238,35.7402716663708,48.1109665283876));
#25848=CARTESIAN_POINT('Ctrl Pts',(44.3252683415991,35.7395324003787,48.1220911822459));
#25849=CARTESIAN_POINT('Ctrl Pts',(44.324966591475,35.7392230151275,48.1267598786032));
#25850=CARTESIAN_POINT('Ctrl Pts',(44.3242952234058,35.7385733765292,48.1365915133954));
#25851=CARTESIAN_POINT('Ctrl Pts',(44.3239218052795,35.7382333492813,48.1417541413393));
#25852=CARTESIAN_POINT('Ctrl Pts',(44.3229459950402,35.7373944653599,48.1545301998701));
#25853=CARTESIAN_POINT('Ctrl Pts',(44.3223191543518,35.7368969605862,48.1621417779022));
#25854=CARTESIAN_POINT('Ctrl Pts',(44.3198023000726,35.7350425317222,48.1906337806709));
#25855=CARTESIAN_POINT('Ctrl Pts',(44.3176170663376,35.7337010525619,48.2114875494207));
#25856=CARTESIAN_POINT('Ctrl Pts',(44.2980550952698,35.7234208661009,48.3727555854374));
#25857=CARTESIAN_POINT('Ctrl Pts',(44.2656163398082,35.7151418460771,48.5109269395549));
#25858=CARTESIAN_POINT('Ctrl Pts',(44.1806386617376,35.6999187395425,48.7507439527265));
#25859=CARTESIAN_POINT('Ctrl Pts',(44.1336637610375,35.6930747396447,48.8536366432757));
#25860=CARTESIAN_POINT('Ctrl Pts',(44.0695340042166,35.6848191184534,48.9666906860437));
#25861=CARTESIAN_POINT('Ctrl Pts',(44.0609042017732,35.6837268516629,48.9814437713339));
#25862=CARTESIAN_POINT('Ctrl Pts',(44.0463888459172,35.6819185960345,49.0055186731209));
#25863=CARTESIAN_POINT('Ctrl Pts',(44.040617275999,35.6812067590532,49.0149083600578));
#25864=CARTESIAN_POINT('Ctrl Pts',(44.030057571624,35.6799168475957,49.0317623285321));
#25865=CARTESIAN_POINT('Ctrl Pts',(44.0252977953554,35.6793398339539,49.0392440817163));
#25866=CARTESIAN_POINT('Ctrl Pts',(44.0149887796606,35.6780993117596,49.0552044713717));
#25867=CARTESIAN_POINT('Ctrl Pts',(44.0094239996943,35.6774352334189,49.0636727021876));
#25868=CARTESIAN_POINT('Ctrl Pts',(43.9940386556873,35.6756139639149,49.0866882640076));
#25869=CARTESIAN_POINT('Ctrl Pts',(43.9840860617096,35.6744518118159,49.1011457366162));
#25870=CARTESIAN_POINT('Ctrl Pts',(43.9254614808539,35.6676949988011,49.1838659003381));
#25871=CARTESIAN_POINT('Ctrl Pts',(43.8725847103486,35.6619383982858,49.2490244175262));
#25872=CARTESIAN_POINT('Ctrl Pts',(43.7402008631107,35.6482660365202,49.3920264201861));
#25873=CARTESIAN_POINT('Ctrl Pts',(43.6578626556174,35.6402746536078,49.4668519994474));
#25874=CARTESIAN_POINT('Ctrl Pts',(43.509472614925,35.6270165480556,49.579974857547));
#25875=CARTESIAN_POINT('Ctrl Pts',(43.4467459490937,35.6217111008548,49.622213174375));
#25876=CARTESIAN_POINT('Ctrl Pts',(43.3727258784532,35.6159057663049,49.6659698428098));
#25877=CARTESIAN_POINT('Ctrl Pts',(43.3637121254195,35.6152062067954,49.671200198315));
#25878=CARTESIAN_POINT('Ctrl Pts',(43.3490881131025,35.6140836415366,49.6795283173277));
#25879=CARTESIAN_POINT('Ctrl Pts',(43.343504171802,35.6136578995824,49.6826715353452));
#25880=CARTESIAN_POINT('Ctrl Pts',(43.3335504885774,35.6129042573395,49.6882093674803));
#25881=CARTESIAN_POINT('Ctrl Pts',(43.3291870242795,35.6125756722893,49.6906149351736));
#25882=CARTESIAN_POINT('Ctrl Pts',(43.3196705225722,35.6118629593536,49.6958133853857));
#25883=CARTESIAN_POINT('Ctrl Pts',(43.3145140552627,35.6114792455463,49.6985997036153));
#25884=CARTESIAN_POINT('Ctrl Pts',(43.2998373278348,35.6103938436981,49.7064441264416));
#25885=CARTESIAN_POINT('Ctrl Pts',(43.2902870760184,35.609695591704,49.7114460869402));
#25886=CARTESIAN_POINT('Ctrl Pts',(43.2247278569441,35.6049534876024,49.7450855450891));
#25887=CARTESIAN_POINT('Ctrl Pts',(43.1673829522442,35.6010588212352,49.7710518822208));
#25888=CARTESIAN_POINT('Ctrl Pts',(42.9901470169952,35.589472670939,49.8410766492329));
#25889=CARTESIAN_POINT('Ctrl Pts',(42.8670642537494,35.5820080623583,49.87608368658));
#25890=CARTESIAN_POINT('Ctrl Pts',(42.6623813635971,35.5694203850802,49.9128899579544));
#25891=CARTESIAN_POINT('Ctrl Pts',(42.5825392710102,35.564473379798,49.9221521976864));
#25892=CARTESIAN_POINT('Ctrl Pts',(42.4845441131643,35.5582328768642,49.9273590998363));
#25893=CARTESIAN_POINT('Ctrl Pts',(42.4667179102826,35.5570911111399,49.9280584775813));
#25894=CARTESIAN_POINT('Ctrl Pts',(42.4385884009676,35.5552779361556,49.9287715212269));
#25895=CARTESIAN_POINT('Ctrl Pts',(42.4282900071768,35.5546116976225,49.9289500549391));
#25896=CARTESIAN_POINT('Ctrl Pts',(42.4091374495548,35.5533679297623,49.929128677219));
#25897=CARTESIAN_POINT('Ctrl Pts',(42.4002837218606,35.5527910919753,49.9291502951684));
#25898=CARTESIAN_POINT('Ctrl Pts',(42.3806281957251,35.5515061874931,49.9290629791344));
#25899=CARTESIAN_POINT('Ctrl Pts',(42.3698268949531,35.5507972044922,49.9289242649511));
#25900=CARTESIAN_POINT('Ctrl Pts',(42.3383070151142,35.5487195603028,49.9282546681654));
#25901=CARTESIAN_POINT('Ctrl Pts',(42.3175956792675,35.5473433464123,49.9274806251665));
#25902=CARTESIAN_POINT('Ctrl Pts',(42.2706210967749,35.5441958828675,49.9249665696704));
#25903=CARTESIAN_POINT('Ctrl Pts',(42.2443733704894,35.5424185919533,49.9230224733435));
#25904=CARTESIAN_POINT('Ctrl Pts',(42.1568846838623,35.5364311704053,49.9147395729691));
#25905=CARTESIAN_POINT('Ctrl Pts',(42.0959131381018,35.5321529878954,49.9060069846049));
#25906=CARTESIAN_POINT('Ctrl Pts',(41.9536932002289,35.5219496391987,49.8786398142167));
#25907=CARTESIAN_POINT('Ctrl Pts',(41.8730838033419,35.5159882853997,49.8576372761027));
#25908=CARTESIAN_POINT('Ctrl Pts',(41.7941383590443,35.5100558711261,49.8315223801304));
#25909=CARTESIAN_POINT('Origin',(42.4,48.4493818343519,48.));
#25910=CARTESIAN_POINT('',(41.7941388327286,34.5440062296316,49.8315225368236));
#25911=CARTESIAN_POINT('',(41.7941388232987,34.7154586800303,49.8315225337042));
#25912=CARTESIAN_POINT('',(41.7941388317924,48.4493818343519,49.8315225365138));
#25913=CARTESIAN_POINT('',(40.4708707108034,35.1798577040826,48.000956906968));
#25914=CARTESIAN_POINT('Ctrl Pts',(41.7941388327286,34.5440062296316,49.8315225368236));
#25915=CARTESIAN_POINT('Ctrl Pts',(41.8146287093069,34.5454435391173,49.8383005154132));
#25916=CARTESIAN_POINT('Ctrl Pts',(41.835230775212,34.5468920470605,49.8447341404695));
#25917=CARTESIAN_POINT('Ctrl Pts',(41.9672793190937,34.5561994466028,49.8835508693276));
#25918=CARTESIAN_POINT('Ctrl Pts',(42.0813312735382,34.5643645427599,49.9061619822515));
#25919=CARTESIAN_POINT('Ctrl Pts',(42.3230981793342,34.5817048271349,49.9317823813768));
#25920=CARTESIAN_POINT('Ctrl Pts',(42.4505144809719,34.5908603568565,49.9326537421973));
#25921=CARTESIAN_POINT('Ctrl Pts',(42.5926065073978,34.600562613785,49.9195540731544));
#25922=CARTESIAN_POINT('Ctrl Pts',(42.6080974763127,34.6016131908161,49.9179365434389));
#25923=CARTESIAN_POINT('Ctrl Pts',(42.6298299468512,34.6030754112146,49.9154008722497));
#25924=CARTESIAN_POINT('Ctrl Pts',(42.6360886351394,34.6034951522501,49.9146395130674));
#25925=CARTESIAN_POINT('Ctrl Pts',(42.6474027119971,34.6042513355798,49.9132068524194));
#25926=CARTESIAN_POINT('Ctrl Pts',(42.6524593771967,34.6045883598486,49.9125461633796));
#25927=CARTESIAN_POINT('Ctrl Pts',(42.6628057918334,34.6052759366926,49.9111525814178));
#25928=CARTESIAN_POINT('Ctrl Pts',(42.6680952091926,34.6056263793087,49.9104177643177));
#25929=CARTESIAN_POINT('Ctrl Pts',(42.6816948079461,34.6065248086319,49.9084708847781));
#25930=CARTESIAN_POINT('Ctrl Pts',(42.6900003555086,34.6070710041341,49.9072264896981));
#25931=CARTESIAN_POINT('Ctrl Pts',(42.7250194690417,34.6093644351759,49.9017456312102));
#25932=CARTESIAN_POINT('Ctrl Pts',(42.7516519727824,34.611085205183,49.89700162607));
#25933=CARTESIAN_POINT('Ctrl Pts',(42.8242197198431,34.615731450677,49.882494301995));
#25934=CARTESIAN_POINT('Ctrl Pts',(42.8699138399239,34.6186102778029,49.8716112728415));
#25935=CARTESIAN_POINT('Ctrl Pts',(43.0535027705824,34.63014880764,49.8207368408108));
#25936=CARTESIAN_POINT('Ctrl Pts',(43.1871248014931,34.6385165746292,49.7670836490106));
#25937=CARTESIAN_POINT('Ctrl Pts',(43.3666926883881,34.6509975308675,49.6705349140436));
#25938=CARTESIAN_POINT('Ctrl Pts',(43.4184506412074,34.6547518753377,49.6394934714114));
#25939=CARTESIAN_POINT('Ctrl Pts',(43.4825409500819,34.6596564275427,49.5968485823097));
#25940=CARTESIAN_POINT('Ctrl Pts',(43.4962952787383,34.6607246403997,49.5874372230593));
#25941=CARTESIAN_POINT('Ctrl Pts',(43.5180575197084,34.6624409074155,49.5721287446336));
#25942=CARTESIAN_POINT('Ctrl Pts',(43.5261449589909,34.6630845948328,49.5663457256502));
#25943=CARTESIAN_POINT('Ctrl Pts',(43.5413853743694,34.6643089862316,49.5552688411638));
#25944=CARTESIAN_POINT('Ctrl Pts',(43.5485471498627,34.6648891946331,49.5499874777499));
#25945=CARTESIAN_POINT('Ctrl Pts',(43.5647421955796,34.6662124380743,49.5378707661184));
#25946=CARTESIAN_POINT('Ctrl Pts',(43.5737522450526,34.6669566526071,49.5310050729344));
#25947=CARTESIAN_POINT('Ctrl Pts',(43.6011611657212,34.66924568802,49.5097352081183));
#25948=CARTESIAN_POINT('Ctrl Pts',(43.6193586628681,34.6708005851701,49.4950762234985));
#25949=CARTESIAN_POINT('Ctrl Pts',(43.7062350914774,34.6783996728495,49.4224517086445));
#25950=CARTESIAN_POINT('Ctrl Pts',(43.7710637003188,34.6846227879505,49.3600732441528));
#25951=CARTESIAN_POINT('Ctrl Pts',(43.9299984607576,34.701363813366,49.1841945611365));
#25952=CARTESIAN_POINT('Ctrl Pts',(44.0158667269027,34.7120617658262,49.0640425893564));
#25953=CARTESIAN_POINT('Ctrl Pts',(44.1010605963668,34.724196908709,48.9103562469663));
#25954=CARTESIAN_POINT('Ctrl Pts',(44.1143316096657,34.7261431175128,48.8851118518895));
#25955=CARTESIAN_POINT('Ctrl Pts',(44.1309961406682,34.7286546009758,48.8516300806256));
#25956=CARTESIAN_POINT('Ctrl Pts',(44.1348985799097,34.7292479495889,48.8436517991411));
#25957=CARTESIAN_POINT('Ctrl Pts',(44.1411052651546,34.7301998493542,48.8307374313458));
#25958=CARTESIAN_POINT('Ctrl Pts',(44.143443891996,34.730560456305,48.8258181527966));
#25959=CARTESIAN_POINT('Ctrl Pts',(44.1479303311284,34.7312559399559,48.8162769676413));
#25960=CARTESIAN_POINT('Ctrl Pts',(44.1500806937478,34.7315909619938,48.8116563905705));
#25961=CARTESIAN_POINT('Ctrl Pts',(44.1552327396933,34.7323978372744,48.8004702999377));
#25962=CARTESIAN_POINT('Ctrl Pts',(44.1582159681456,34.7328685669796,48.7938962684301));
#25963=CARTESIAN_POINT('Ctrl Pts',(44.168564436003,34.7345145203125,48.7707472736971));
#25964=CARTESIAN_POINT('Ctrl Pts',(44.1757330303006,34.7356784473682,48.7540847345965));
#25965=CARTESIAN_POINT('Ctrl Pts',(44.1929153853969,34.7385350098019,48.7125420129986));
#25966=CARTESIAN_POINT('Ctrl Pts',(44.2026476083617,34.7402138716442,48.6875488684417));
#25967=CARTESIAN_POINT('Ctrl Pts',(44.2423281036799,34.7473685102786,48.5790046056423));
#25968=CARTESIAN_POINT('Ctrl Pts',(44.2670140746638,34.752654504719,48.4936395543732));
#25969=CARTESIAN_POINT('Ctrl Pts',(44.3136383257669,34.765839146129,48.2775497515533));
#25970=CARTESIAN_POINT('Ctrl Pts',(44.3281615562322,34.7737332214481,48.1457160683761));
#25971=CARTESIAN_POINT('Ctrl Pts',(44.3292600608276,34.7836740217639,47.9880535280753));
#25972=CARTESIAN_POINT('Ctrl Pts',(44.328935767948,34.7852889497652,47.9626662677429));
#25973=CARTESIAN_POINT('Ctrl Pts',(44.3277341735545,34.7876632483594,47.9257193055318));
#25974=CARTESIAN_POINT('Ctrl Pts',(44.3272535423683,34.7884102291815,47.914148737586));
#25975=CARTESIAN_POINT('Ctrl Pts',(44.3262165100452,34.7897407221687,47.8936387028876));
#25976=CARTESIAN_POINT('Ctrl Pts',(44.3257019688389,34.7903229045364,47.8846973904783));
#25977=CARTESIAN_POINT('Ctrl Pts',(44.3244996747751,34.7915405621749,47.8660675720539));
#25978=CARTESIAN_POINT('Ctrl Pts',(44.3238009766147,34.7921763657448,47.8563800501922));
#25979=CARTESIAN_POINT('Ctrl Pts',(44.3217884363655,34.7938402923106,47.831134568534));
#25980=CARTESIAN_POINT('Ctrl Pts',(44.3203588414175,34.7948720243876,47.8155868123115));
#25981=CARTESIAN_POINT('Ctrl Pts',(44.3129911160381,34.799596831881,47.7448823566654));
#25982=CARTESIAN_POINT('Ctrl Pts',(44.3048647643674,34.8033578560222,47.689985168909));
#25983=CARTESIAN_POINT('Ctrl Pts',(44.2742463006614,34.8145378656633,47.5308462042116));
#25984=CARTESIAN_POINT('Ctrl Pts',(44.2454685454515,34.8221252419197,47.4280334946921));
#25985=CARTESIAN_POINT('Ctrl Pts',(44.1721060353499,34.8371737681846,47.2305752110992));
#25986=CARTESIAN_POINT('Ctrl Pts',(44.1280200981106,34.8446068017118,47.1360989317836));
#25987=CARTESIAN_POINT('Ctrl Pts',(44.0683827459427,34.8528138956646,47.0313347922527));
#25988=CARTESIAN_POINT('Ctrl Pts',(44.0600600875846,34.8539248652839,47.0171399786565));
#25989=CARTESIAN_POINT('Ctrl Pts',(44.0482214396729,34.8554565479837,46.9975279106373));
#25990=CARTESIAN_POINT('Ctrl Pts',(44.0448586166162,34.8558863708531,46.9920196735845));
#25991=CARTESIAN_POINT('Ctrl Pts',(44.0390116847532,34.8566245687974,46.9825496976155));
#25992=CARTESIAN_POINT('Ctrl Pts',(44.0365407230539,34.8569337796565,46.9785799671355));
#25993=CARTESIAN_POINT('Ctrl Pts',(44.0313010219741,34.8575836193096,46.9702299361213));
#25994=CARTESIAN_POINT('Ctrl Pts',(44.0285290240318,34.8579240186846,46.9658517380292));
#25995=CARTESIAN_POINT('Ctrl Pts',(44.0216155114455,34.8587647820698,46.955029008799));
#25996=CARTESIAN_POINT('Ctrl Pts',(44.0174531324553,34.8592637816368,46.9485977893396));
#25997=CARTESIAN_POINT('Ctrl Pts',(44.0016700040355,34.8611298153396,46.9245271106344));
#25998=CARTESIAN_POINT('Ctrl Pts',(43.9897976183614,34.8624811563245,46.9070533594576));
#25999=CARTESIAN_POINT('Ctrl Pts',(43.8945879819627,34.8729480400896,46.7717593033089));
#26000=CARTESIAN_POINT('Ctrl Pts',(43.798544494788,34.8813789900665,46.663417414426));
#26001=CARTESIAN_POINT('Ctrl Pts',(43.6096183868487,34.8966051438272,46.4931972528051));
#26002=CARTESIAN_POINT('Ctrl Pts',(43.5218038554396,34.9032796625362,46.4267287112272));
#26003=CARTESIAN_POINT('Ctrl Pts',(43.4143897058633,34.9113453271464,46.3590104055715));
#26004=CARTESIAN_POINT('Ctrl Pts',(43.3998455492641,34.9124351143861,46.3501084362172));
#26005=CARTESIAN_POINT('Ctrl Pts',(43.3757184565577,34.914240216041,46.3357772682404));
#26006=CARTESIAN_POINT('Ctrl Pts',(43.3662034459825,34.914951405667,46.3302351363042));
#26007=CARTESIAN_POINT('Ctrl Pts',(43.3489398915821,34.9162407794639,46.3203767386885));
#26008=CARTESIAN_POINT('Ctrl Pts',(43.3412079839978,34.9168179090004,46.3160318458434));
#26009=CARTESIAN_POINT('Ctrl Pts',(43.3245676235295,34.9180593872843,46.3068313135474));
#26010=CARTESIAN_POINT('Ctrl Pts',(43.3156503077847,34.9187243113538,46.3019923444137));
#26011=CARTESIAN_POINT('Ctrl Pts',(43.2911590916462,34.9205497484386,46.2889512440294));
#26012=CARTESIAN_POINT('Ctrl Pts',(43.2755107668893,34.9217152585066,46.2808917329298));
#26013=CARTESIAN_POINT('Ctrl Pts',(43.1838649163437,34.9285383163638,46.2352662931577));
#26014=CARTESIAN_POINT('Ctrl Pts',(43.1055780297647,34.9343616236151,46.2025336385534));
#26015=CARTESIAN_POINT('Ctrl Pts',(42.9162923775565,34.9484067728668,46.1376660373835));
#26016=CARTESIAN_POINT('Ctrl Pts',(42.8040520637093,34.9567167124944,46.1101363008273));
#26017=CARTESIAN_POINT('Ctrl Pts',(42.6546459115141,34.9674361954427,46.0874155089848));
#26018=CARTESIAN_POINT('Ctrl Pts',(42.6191112912591,34.9699592329286,46.0830194450237));
#26019=CARTESIAN_POINT('Ctrl Pts',(42.5460978498607,34.97506576778,46.0760437476119));
#26020=CARTESIAN_POINT('Ctrl Pts',(42.508622916386,34.9776451999554,46.0735644960774));
#26021=CARTESIAN_POINT('Ctrl Pts',(42.4613351979706,34.9808289455994,46.0718205563258));
#26022=CARTESIAN_POINT('Ctrl Pts',(42.451570841787,34.9814825307748,46.0715346952266));
#26023=CARTESIAN_POINT('Ctrl Pts',(42.4361631572987,34.9825073913876,46.0712007303808));
#26024=CARTESIAN_POINT('Ctrl Pts',(42.4305212298557,34.9828813037757,46.0711032031259));
#26025=CARTESIAN_POINT('Ctrl Pts',(42.4198555492208,34.9835854728689,46.0709656426138));
#26026=CARTESIAN_POINT('Ctrl Pts',(42.4148321090907,34.9839159907461,46.0709204775525));
#26027=CARTESIAN_POINT('Ctrl Pts',(42.4030411243004,34.9846891879588,46.0708605272238));
#26028=CARTESIAN_POINT('Ctrl Pts',(42.3962736067944,34.9851309746168,46.0708617283214));
#26029=CARTESIAN_POINT('Ctrl Pts',(42.3740822399987,34.9865735058102,46.0709824444975));
#26030=CARTESIAN_POINT('Ctrl Pts',(42.3586593402792,34.9875663461566,46.0712513264068));
#26031=CARTESIAN_POINT('Ctrl Pts',(42.2729735814096,34.9930365788061,46.0737734822425));
#26032=CARTESIAN_POINT('Ctrl Pts',(42.2028639518154,34.9973423091948,46.0796813146554));
#26033=CARTESIAN_POINT('Ctrl Pts',(42.0989437653756,35.0036721499642,46.0941915309639));
#26034=CARTESIAN_POINT('Ctrl Pts',(42.0647954063096,35.0057434285244,46.0999003319764));
#26035=CARTESIAN_POINT('Ctrl Pts',(41.8856022494722,35.0166439346524,46.1348386251313));
#26036=CARTESIAN_POINT('Ctrl Pts',(41.7441426418191,35.0254054379438,46.1797589456742));
#26037=CARTESIAN_POINT('Ctrl Pts',(41.586741495243,35.0362944427867,46.2504972118644));
#26038=CARTESIAN_POINT('Ctrl Pts',(41.564468449651,35.0378623323715,46.2610243412815));
#26039=CARTESIAN_POINT('Ctrl Pts',(41.5321533793324,35.0401800885492,46.2770618839465));
#26040=CARTESIAN_POINT('Ctrl Pts',(41.5219485488789,35.0409184008936,46.2822400782885));
#26041=CARTESIAN_POINT('Ctrl Pts',(41.5040849495459,35.0422223909537,46.2915053032089));
#26042=CARTESIAN_POINT('Ctrl Pts',(41.4964064996441,35.0427866984068,46.2955538469719));
#26043=CARTESIAN_POINT('Ctrl Pts',(41.4881122493073,35.0434004687712,46.2999988764588));
#26044=CARTESIAN_POINT('Ctrl Pts',(41.4874689564455,35.043448099662,46.3003440982211));
#26045=CARTESIAN_POINT('Ctrl Pts',(41.478288531475,35.0441282333387,46.3052774683052));
#26046=CARTESIAN_POINT('Ctrl Pts',(41.4697860325811,35.0447630067461,46.3099294512836));
#26047=CARTESIAN_POINT('Ctrl Pts',(41.4524129202297,35.0460702103982,46.3196056390169));
#26048=CARTESIAN_POINT('Ctrl Pts',(41.4435463705405,35.0467428649969,46.3246364782388));
#26049=CARTESIAN_POINT('Ctrl Pts',(41.4215962689952,35.0484220343456,46.337321900789));
#26050=CARTESIAN_POINT('Ctrl Pts',(41.408562463227,35.0494315664336,46.3450607531512));
#26051=CARTESIAN_POINT('Ctrl Pts',(41.3720933263432,35.0522920930632,46.3672998263619));
#26052=CARTESIAN_POINT('Ctrl Pts',(41.3488763433923,35.0541555211183,46.3821492915892));
#26053=CARTESIAN_POINT('Ctrl Pts',(41.2711288938089,35.0605426066289,46.4342561984722));
#26054=CARTESIAN_POINT('Ctrl Pts',(41.2182006495391,35.0651447501022,46.473811143081));
#26055=CARTESIAN_POINT('Ctrl Pts',(41.0586929126367,35.079792566348,46.6062960609028));
#26056=CARTESIAN_POINT('Ctrl Pts',(40.9602319003895,35.0900495046597,46.7082636237771));
#26057=CARTESIAN_POINT('Ctrl Pts',(40.853772554026,35.1021180941536,46.8459659331852));
#26058=CARTESIAN_POINT('Ctrl Pts',(40.8344132325379,35.1043592485135,46.8723687117982));
#26059=CARTESIAN_POINT('Ctrl Pts',(40.8104074911616,35.1071872937489,46.9069193289909));
#26060=CARTESIAN_POINT('Ctrl Pts',(40.8051366416773,35.1078114444317,46.9146242243038));
#26061=CARTESIAN_POINT('Ctrl Pts',(40.7968230835735,35.1088006802971,46.9269682657223));
#26062=CARTESIAN_POINT('Ctrl Pts',(40.7937441786555,35.1091681114713,46.9315826815033));
#26063=CARTESIAN_POINT('Ctrl Pts',(40.7878985430584,35.1098676794292,46.9404260354128));
#26064=CARTESIAN_POINT('Ctrl Pts',(40.7851284937373,35.1102000255627,46.9446526104218));
#26065=CARTESIAN_POINT('Ctrl Pts',(40.7785790708313,35.1109879341656,46.9547319652195));
#26066=CARTESIAN_POINT('Ctrl Pts',(40.7748146925348,35.1114425062394,46.9605944900198));
#26067=CARTESIAN_POINT('Ctrl Pts',(40.762197250136,35.1129724329873,46.9804806325943));
#26068=CARTESIAN_POINT('Ctrl Pts',(40.7534929940613,35.1140385036843,46.994598432447));
#26069=CARTESIAN_POINT('Ctrl Pts',(40.7029142705954,35.1203086426507,47.0790531662067));
#26070=CARTESIAN_POINT('Ctrl Pts',(40.6653642216589,35.1252815775282,47.1518933474097));
#26071=CARTESIAN_POINT('Ctrl Pts',(40.5779738226526,35.1383676459323,47.3516854730591));
#26072=CARTESIAN_POINT('Ctrl Pts',(40.5367643163965,35.1463626087072,47.4818856220333));
#26073=CARTESIAN_POINT('Ctrl Pts',(40.4998866399512,35.1577774497081,47.6631184298773));
#26074=CARTESIAN_POINT('Ctrl Pts',(40.4919799584223,35.1608313585747,47.7112459894529));
#26075=CARTESIAN_POINT('Ctrl Pts',(40.4839777704355,35.164929856896,47.7749653076872));
#26076=CARTESIAN_POINT('Ctrl Pts',(40.4822351270031,35.1659225519383,47.7903343941973));
#26077=CARTESIAN_POINT('Ctrl Pts',(40.4797025763691,35.1675460408309,47.8153541692377));
#26078=CARTESIAN_POINT('Ctrl Pts',(40.4788001633346,35.1681732774932,47.824992971788));
#26079=CARTESIAN_POINT('Ctrl Pts',(40.4772376416884,35.1693586662352,47.8431544187014));
#26080=CARTESIAN_POINT('Ctrl Pts',(40.4765615538733,35.16991629992,47.8516754811227));
#26081=CARTESIAN_POINT('Ctrl Pts',(40.4753116091618,35.1710451685827,47.8688784638694));
#26082=CARTESIAN_POINT('Ctrl Pts',(40.4747398144819,35.1716164550315,47.877560329559));
#26083=CARTESIAN_POINT('Ctrl Pts',(40.4732507108879,35.1732800145079,47.9027697016922));
#26084=CARTESIAN_POINT('Ctrl Pts',(40.4724873877035,35.1743770835538,47.9193051782206));
#26085=CARTESIAN_POINT('Ctrl Pts',(40.4712150432388,35.176928393239,47.9575449889482));
#26086=CARTESIAN_POINT('Ctrl Pts',(40.4708594482203,35.1783872376127,47.9792516976681));
#26087=CARTESIAN_POINT('Ctrl Pts',(40.4708702383276,35.1798570188309,48.0009589212152));
#26088=CARTESIAN_POINT('Ctrl Pts',(40.470870237355,35.1798568862125,48.000956962571));
#26089=CARTESIAN_POINT('Ctrl Pts',(40.4709100302208,35.1852883880148,48.081174939798));
#26090=CARTESIAN_POINT('Ctrl Pts',(40.4759531835995,35.1908675616307,48.1613049946017));
#26091=CARTESIAN_POINT('Ctrl Pts',(40.5061098364464,35.2079432831597,48.4009270850374));
#26092=CARTESIAN_POINT('Ctrl Pts',(40.5462442780223,35.219701532293,48.557812136919));
#26093=CARTESIAN_POINT('Ctrl Pts',(40.6112379328665,35.2317426179312,48.7225806417626));
#26094=CARTESIAN_POINT('Ctrl Pts',(40.6172200976197,35.2328087880833,48.7372166411818));
#26095=CARTESIAN_POINT('Ctrl Pts',(40.6260452844213,35.2343214721451,48.7580725157763));
#26096=CARTESIAN_POINT('Ctrl Pts',(40.6287422958384,35.2347761307598,48.7643529427421));
#26097=CARTESIAN_POINT('Ctrl Pts',(40.6334832510485,35.2355621137002,48.7752331683621));
#26098=CARTESIAN_POINT('Ctrl Pts',(40.6355119016407,35.2358943464401,48.7798394981041));
#26099=CARTESIAN_POINT('Ctrl Pts',(40.6398392070688,35.2365944103947,48.7895619009939));
#26100=CARTESIAN_POINT('Ctrl Pts',(40.642142160466,35.2369619764881,48.7946759279418));
#26101=CARTESIAN_POINT('Ctrl Pts',(40.648452757878,35.2379559383835,48.8085278127995));
#26102=CARTESIAN_POINT('Ctrl Pts',(40.6525035270755,35.2385797579921,48.8172460167642));
#26103=CARTESIAN_POINT('Ctrl Pts',(40.6719347363676,35.2415078838264,48.8582614026467));
#26104=CARTESIAN_POINT('Ctrl Pts',(40.6881474603223,35.2437654796842,48.8901592315938));
#26105=CARTESIAN_POINT('Ctrl Pts',(40.7174590431839,35.2475778805207,48.9440618604684));
#26106=CARTESIAN_POINT('Ctrl Pts',(40.7301251654887,35.2491491837437,48.9662892948409));
#26107=CARTESIAN_POINT('Ctrl Pts',(40.8197978511772,35.2598156051154,49.1166213496377));
#26108=CARTESIAN_POINT('Ctrl Pts',(40.91102378168,35.268499514009,49.2356518021253));
#26109=CARTESIAN_POINT('Ctrl Pts',(41.045113969837,35.2802627543142,49.3739314389018));
#26110=CARTESIAN_POINT('Ctrl Pts',(41.0761756782416,35.2829275312723,49.403884803761));
#26111=CARTESIAN_POINT('Ctrl Pts',(41.123579819503,35.2869317443521,49.4466243903317));
#26112=CARTESIAN_POINT('Ctrl Pts',(41.1391672204477,35.2882389050776,49.4602298639794));
#26113=CARTESIAN_POINT('Ctrl Pts',(41.1644879576153,35.2903494662493,49.4816233703533));
#26114=CARTESIAN_POINT('Ctrl Pts',(41.1740834410048,35.2911464072972,49.4895725551921));
#26115=CARTESIAN_POINT('Ctrl Pts',(41.1923829451665,35.2926613327077,49.504435825919));
#26116=CARTESIAN_POINT('Ctrl Pts',(41.2010710606666,35.2933785263995,49.5113687489618));
#26117=CARTESIAN_POINT('Ctrl Pts',(41.2165872589449,35.2946560276261,49.5235323476396));
#26118=CARTESIAN_POINT('Ctrl Pts',(41.2233913778625,35.2952151126472,49.528793209131));
#26119=CARTESIAN_POINT('Ctrl Pts',(41.2369778324198,35.2963294001881,49.5391536627439));
#26120=CARTESIAN_POINT('Ctrl Pts',(41.2437590889536,35.2968845420465,49.5442543545477));
#26121=CARTESIAN_POINT('Ctrl Pts',(41.2620506463989,35.298379379519,49.557824780394));
#26122=CARTESIAN_POINT('Ctrl Pts',(41.2736215933389,35.2993222743936,49.5662114940219));
#26123=CARTESIAN_POINT('Ctrl Pts',(41.3173614785961,35.3028771979908,49.5971791043714));
#26124=CARTESIAN_POINT('Ctrl Pts',(41.3501229381969,35.3055213910521,49.6189024155884));
#26125=CARTESIAN_POINT('Ctrl Pts',(41.5090293379316,35.3182688100887,49.7174165848119));
#26126=CARTESIAN_POINT('Ctrl Pts',(41.6430385116812,35.3288445252337,49.7805461196931));
#26127=CARTESIAN_POINT('Ctrl Pts',(41.7866459223646,35.3396514468648,49.8290311424881));
#26128=CARTESIAN_POINT('Ctrl Pts',(41.7903904758723,35.3399328460002,49.8302825936515));
#26129=CARTESIAN_POINT('Ctrl Pts',(41.7941388318214,35.3402141276758,49.8315225365234));
#26130=CARTESIAN_POINT('',(40.4708702390927,35.3509292085261,48.0009604591324));
#26131=CARTESIAN_POINT('Ctrl Pts',(41.7941383590443,35.5100558711261,49.8315223801304));
#26132=CARTESIAN_POINT('Ctrl Pts',(41.7402688807148,35.5060078090118,49.8137025320672));
#26133=CARTESIAN_POINT('Ctrl Pts',(41.6871740605304,35.5019746911376,49.7935022709993));
#26134=CARTESIAN_POINT('Ctrl Pts',(41.5985161358713,35.4952389641539,49.755205567771));
#26135=CARTESIAN_POINT('Ctrl Pts',(41.5625139060136,35.4925036623722,49.738315429417));
#26136=CARTESIAN_POINT('Ctrl Pts',(41.5182730832123,35.4891644365375,49.7158663167832));
#26137=CARTESIAN_POINT('Ctrl Pts',(41.5095235635153,35.4885051449714,49.7113419585414));
#26138=CARTESIAN_POINT('Ctrl Pts',(41.4957512860461,35.4874695880772,49.7040861184335));
#26139=CARTESIAN_POINT('Ctrl Pts',(41.4907055038788,35.4870906612229,49.7013990587629));
#26140=CARTESIAN_POINT('Ctrl Pts',(41.4813506868729,35.4863891207655,49.6963637807018));
#26141=CARTESIAN_POINT('Ctrl Pts',(41.4770386946081,35.4860661579224,49.6940215660913));
#26142=CARTESIAN_POINT('Ctrl Pts',(41.4671183748088,35.4853240077362,49.6885838631581));
#26143=CARTESIAN_POINT('Ctrl Pts',(41.4615164830773,35.4849055580117,49.6854768704729));
#26144=CARTESIAN_POINT('Ctrl Pts',(41.4496637552893,35.4840213069379,49.6788255451118));
#26145=CARTESIAN_POINT('Ctrl Pts',(41.4434170169081,35.4835559483533,49.6752740639169));
#26146=CARTESIAN_POINT('Ctrl Pts',(41.4266517927132,35.482308401588,49.665618119815));
#26147=CARTESIAN_POINT('Ctrl Pts',(41.4161707595854,35.4815299723222,49.6594488531917));
#26148=CARTESIAN_POINT('Ctrl Pts',(41.3834890743421,35.4791051251109,49.6397935212714));
#26149=CARTESIAN_POINT('Ctrl Pts',(41.3615011986949,35.4774772603582,49.6259574499811));
#26150=CARTESIAN_POINT('Ctrl Pts',(41.2697896953883,35.4706730307226,49.5656274646212));
#26151=CARTESIAN_POINT('Ctrl Pts',(41.2028505569246,35.4656680059165,49.5150577699913));
#26152=CARTESIAN_POINT('Ctrl Pts',(41.0341413280169,35.4523719212485,49.3694200855606));
#26153=CARTESIAN_POINT('Ctrl Pts',(40.9390211678361,35.444101326672,49.2674449061153));
#26154=CARTESIAN_POINT('Ctrl Pts',(40.8406223051401,35.4337466277066,49.1360088050042));
#26155=CARTESIAN_POINT('Ctrl Pts',(40.8259486756661,35.4321468862919,49.1155882462738));
#26156=CARTESIAN_POINT('Ctrl Pts',(40.8051324009717,35.4297909576824,49.0853906869873));
#26157=CARTESIAN_POINT('Ctrl Pts',(40.7986713569576,35.4290468884698,49.0758355679571));
#26158=CARTESIAN_POINT('Ctrl Pts',(40.7873514190651,35.427719877505,49.0587668126784));
#26159=CARTESIAN_POINT('Ctrl Pts',(40.7824583407555,35.4271382435244,49.0512761698526));
#26160=CARTESIAN_POINT('Ctrl Pts',(40.772353399109,35.4259199987667,49.0355692955649));
#26161=CARTESIAN_POINT('Ctrl Pts',(40.7671512457259,35.4252830477511,49.0273471482827));
#26162=CARTESIAN_POINT('Ctrl Pts',(40.7537181136943,35.4236122241937,49.0057559265244));
#26163=CARTESIAN_POINT('Ctrl Pts',(40.745587885794,35.4225746851317,48.9923253319292));
#26164=CARTESIAN_POINT('Ctrl Pts',(40.7089714182371,35.417777439464,48.9301363753035));
#26165=CARTESIAN_POINT('Ctrl Pts',(40.6824733250095,35.4139471793126,48.8802456189056));
#26166=CARTESIAN_POINT('Ctrl Pts',(40.5834855215002,35.398050051463,48.672331570749));
#26167=CARTESIAN_POINT('Ctrl Pts',(40.5303324488016,35.3853919410592,48.5060468796598));
#26168=CARTESIAN_POINT('Ctrl Pts',(40.4932818941363,35.370442066012,48.2958716787038));
#26169=CARTESIAN_POINT('Ctrl Pts',(40.4876042984503,35.3676986420534,48.2566264638591));
#26170=CARTESIAN_POINT('Ctrl Pts',(40.4816948812438,35.3641396210497,48.2044814807771));
#26171=CARTESIAN_POINT('Ctrl Pts',(40.4803771739966,35.3632752261565,48.1917170621141));
#26172=CARTESIAN_POINT('Ctrl Pts',(40.4785940050237,35.3619901209192,48.1725758214111));
#26173=CARTESIAN_POINT('Ctrl Pts',(40.4780327471933,35.3615644775972,48.1662085848358));
#26174=CARTESIAN_POINT('Ctrl Pts',(40.4771170845702,35.3608315623895,48.1551952319816));
#26175=CARTESIAN_POINT('Ctrl Pts',(40.4767478509666,35.360523480978,48.150550452937));
#26176=CARTESIAN_POINT('Ctrl Pts',(40.4760423140712,35.359908606055,48.1412486448363));
#26177=CARTESIAN_POINT('Ctrl Pts',(40.4757060835667,35.3596018224487,48.1365916577401));
#26178=CARTESIAN_POINT('Ctrl Pts',(40.4750344638594,35.3589585419743,48.1267942318297));
#26179=CARTESIAN_POINT('Ctrl Pts',(40.4747027483597,35.358622249535,48.1216535526852));
#26180=CARTESIAN_POINT('Ctrl Pts',(40.4739614927812,35.3578236326744,48.1094026801593));
#26181=CARTESIAN_POINT('Ctrl Pts',(40.4735707234394,35.3573623096458,48.1022913675388));
#26182=CARTESIAN_POINT('Ctrl Pts',(40.4716692387488,35.354876560639,48.0637977357197));
#26183=CARTESIAN_POINT('Ctrl Pts',(40.470885883251,35.3528888685554,48.0323825261852));
#26184=CARTESIAN_POINT('Ctrl Pts',(40.4708702390927,35.3509292085261,48.0009604591324));
#26185=CARTESIAN_POINT('Ctrl Pts',(40.4708702403991,35.350929371948,48.0009630795115));
#26186=CARTESIAN_POINT('Ctrl Pts',(40.4707910326032,35.3410344229544,47.8423031615214));
#26187=CARTESIAN_POINT('Ctrl Pts',(40.4902846846639,35.3318563635985,47.6842154128848));
#26188=CARTESIAN_POINT('Ctrl Pts',(40.5492871826736,35.3172044227034,47.4491870401164));
#26189=CARTESIAN_POINT('Ctrl Pts',(40.5748924597533,35.3120584573135,47.3695138903177));
#26190=CARTESIAN_POINT('Ctrl Pts',(40.6120213416988,35.3056228606644,47.2754432141581));
#26191=CARTESIAN_POINT('Ctrl Pts',(40.6186829448132,35.3044995962526,47.25921680992));
#26192=CARTESIAN_POINT('Ctrl Pts',(40.6295395438284,35.3027157827095,47.2337657290518));
#26193=CARTESIAN_POINT('Ctrl Pts',(40.6335876517912,35.3020602338153,47.2244791463582));
#26194=CARTESIAN_POINT('Ctrl Pts',(40.6413160825334,35.3008261327034,47.2071241757825));
#26195=CARTESIAN_POINT('Ctrl Pts',(40.6449792742929,35.3002481815543,47.1990484146391));
#26196=CARTESIAN_POINT('Ctrl Pts',(40.653321488198,35.2989473262594,47.1809894459627));
#26197=CARTESIAN_POINT('Ctrl Pts',(40.658030645887,35.2982233935928,47.1710205841216));
#26198=CARTESIAN_POINT('Ctrl Pts',(40.6702623740337,35.2963688014655,47.1456916161123));
#26199=CARTESIAN_POINT('Ctrl Pts',(40.6779041054205,35.2952340267535,47.1303904513169));
#26200=CARTESIAN_POINT('Ctrl Pts',(40.7398154420948,35.2862215227583,47.0104415047958));
#26201=CARTESIAN_POINT('Ctrl Pts',(40.8033604325451,35.2780101349555,46.910884842358));
#26202=CARTESIAN_POINT('Ctrl Pts',(40.9420680301487,35.2619202148804,46.7320300148092));
#26203=CARTESIAN_POINT('Ctrl Pts',(41.0156710569347,35.2541000536149,46.6520579796041));
#26204=CARTESIAN_POINT('Ctrl Pts',(41.1175401158697,35.244428105604,46.5585682870385));
#26205=CARTESIAN_POINT('Ctrl Pts',(41.1399367493887,35.2423652604611,46.5389491665068));
#26206=CARTESIAN_POINT('Ctrl Pts',(41.1730358061858,35.2394174299215,46.5112823954314));
#26207=CARTESIAN_POINT('Ctrl Pts',(41.1833810859736,35.2385098238655,46.5028160835447));
#26208=CARTESIAN_POINT('Ctrl Pts',(41.1997936702361,35.2370924702989,46.4896669132269));
#26209=CARTESIAN_POINT('Ctrl Pts',(41.2058020970208,35.2365782653914,46.4849116724714));
#26210=CARTESIAN_POINT('Ctrl Pts',(41.2170232915207,35.2356268357001,46.4761391235322));
#26211=CARTESIAN_POINT('Ctrl Pts',(41.222228567798,35.2351889973718,46.4721124647835));
#26212=CARTESIAN_POINT('Ctrl Pts',(41.2313766593163,35.2344257820294,46.4651102836687));
#26213=CARTESIAN_POINT('Ctrl Pts',(41.2353104649982,35.2340996009585,46.4621231378867));
#26214=CARTESIAN_POINT('Ctrl Pts',(41.2436358564932,35.2334135762023,46.4558514979612));
#26215=CARTESIAN_POINT('Ctrl Pts',(41.2480300183165,35.2330539793792,46.4525705858092));
#26216=CARTESIAN_POINT('Ctrl Pts',(41.2597152560727,35.2321041158962,46.4439231327865));
#26217=CARTESIAN_POINT('Ctrl Pts',(41.2670303258039,35.2315160505334,46.4385890229912));
#26218=CARTESIAN_POINT('Ctrl Pts',(41.2987921764028,35.2289895744355,46.4157691904611));
#26219=CARTESIAN_POINT('Ctrl Pts',(41.323609643877,35.2270837263489,46.3988035824811));
#26220=CARTESIAN_POINT('Ctrl Pts',(41.4520312474011,35.2175080686372,46.3153485600807));
#26221=CARTESIAN_POINT('Ctrl Pts',(41.5614411559388,35.2102641733051,46.2582995067582));
#26222=CARTESIAN_POINT('Ctrl Pts',(41.7704204520914,35.1967898889338,46.1736238516972));
#26223=CARTESIAN_POINT('Ctrl Pts',(41.868187684998,35.1906169339228,46.1427997978727));
#26224=CARTESIAN_POINT('Ctrl Pts',(41.9971085864832,35.1823151196081,46.1131726920815));
#26225=CARTESIAN_POINT('Ctrl Pts',(42.0264358370739,35.1804170379924,46.1071480664431));
#26226=CARTESIAN_POINT('Ctrl Pts',(42.0681791444727,35.1776963703515,46.0995807151031));
#26227=CARTESIAN_POINT('Ctrl Pts',(42.0804892098758,35.1768917368142,46.0974723703642));
#26228=CARTESIAN_POINT('Ctrl Pts',(42.1017718063175,35.1754962563156,46.0940396788511));
#26229=CARTESIAN_POINT('Ctrl Pts',(42.1107349073189,35.174907222545,46.0926587870153));
#26230=CARTESIAN_POINT('Ctrl Pts',(42.1279473712841,35.1737733676104,46.0901310810871));
#26231=CARTESIAN_POINT('Ctrl Pts',(42.136195095606,35.1732288740278,46.0889743882014));
#26232=CARTESIAN_POINT('Ctrl Pts',(42.1556414032248,35.171942178823,46.0863754498353));
#26233=CARTESIAN_POINT('Ctrl Pts',(42.1668455705668,35.1711985760671,46.0849780561066));
#26234=CARTESIAN_POINT('Ctrl Pts',(42.2060702344192,35.1685870379329,46.0804352488309));
#26235=CARTESIAN_POINT('Ctrl Pts',(42.2341457191482,35.1667030205057,46.077805992582));
#26236=CARTESIAN_POINT('Ctrl Pts',(42.4401768850435,35.152762308989,46.0630585232234));
#26237=CARTESIAN_POINT('Ctrl Pts',(42.6189678031594,35.1399205916771,46.075062518069));
#26238=CARTESIAN_POINT('Ctrl Pts',(42.8608282290547,35.1223719875436,46.1254579197731));
#26239=CARTESIAN_POINT('Ctrl Pts',(42.9273529071344,35.1175411813774,46.1430747158722));
#26240=CARTESIAN_POINT('Ctrl Pts',(43.007320433484,35.1118331643388,46.1688972566215));
#26241=CARTESIAN_POINT('Ctrl Pts',(43.0217846940913,35.1108048476503,46.1737581770791));
#26242=CARTESIAN_POINT('Ctrl Pts',(43.0425502220222,35.1093360387243,46.181012052417));
#26243=CARTESIAN_POINT('Ctrl Pts',(43.0488985794319,35.1088880171073,46.1832670591772));
#26244=CARTESIAN_POINT('Ctrl Pts',(43.0599550355147,35.1081096699595,46.1872597839482));
#26245=CARTESIAN_POINT('Ctrl Pts',(43.0646683505914,35.1077784868233,46.1889826820685));
#26246=CARTESIAN_POINT('Ctrl Pts',(43.0746795499291,35.107076416936,46.1926865100509));
#26247=CARTESIAN_POINT('Ctrl Pts',(43.0799754803225,35.1067058251663,46.1946723582017));
#26248=CARTESIAN_POINT('Ctrl Pts',(43.0944545843509,35.105694628989,46.2001744310183));
#26249=CARTESIAN_POINT('Ctrl Pts',(43.1036198807677,35.1050567553901,46.2037376801119));
#26250=CARTESIAN_POINT('Ctrl Pts',(43.1483814677261,35.1019504984579,46.2215350981755));
#26251=CARTESIAN_POINT('Ctrl Pts',(43.1835779088949,35.0995359800672,46.2367591333242));
#26252=CARTESIAN_POINT('Ctrl Pts',(43.2505743275295,35.0949509912259,46.2681408680256));
#26253=CARTESIAN_POINT('Ctrl Pts',(43.2824251605889,35.0927762211357,46.2841507033565));
#26254=CARTESIAN_POINT('Ctrl Pts',(43.4148334958615,35.0836832440711,46.3553686232979));
#26255=CARTESIAN_POINT('Ctrl Pts',(43.510804973805,35.0769490411829,46.4186041567725));
#26256=CARTESIAN_POINT('Ctrl Pts',(43.6668603086326,35.0649000318803,46.5426821727144));
#26257=CARTESIAN_POINT('Ctrl Pts',(43.7295810104769,35.0596919360414,46.5996707648466));
#26258=CARTESIAN_POINT('Ctrl Pts',(43.8005667697892,35.0531863671815,46.6732502924301));
#26259=CARTESIAN_POINT('Ctrl Pts',(43.8126074833879,35.0520597991942,46.6860775791096));
#26260=CARTESIAN_POINT('Ctrl Pts',(43.8313100851585,35.0502719264175,46.7065562032921));
#26261=CARTESIAN_POINT('Ctrl Pts',(43.8380901301796,35.0496156609864,46.7140986872734));
#26262=CARTESIAN_POINT('Ctrl Pts',(43.8506855445385,35.0483809312922,46.7283347046998));
#26263=CARTESIAN_POINT('Ctrl Pts',(43.8565148729506,35.0478030742465,46.7350155760447));
#26264=CARTESIAN_POINT('Ctrl Pts',(43.8694784794013,35.0465033820213,46.7500813003261));
#26265=CARTESIAN_POINT('Ctrl Pts',(43.8765874051512,35.0457805263911,46.7584874613569));
#26266=CARTESIAN_POINT('Ctrl Pts',(43.8945217621835,35.0439305543827,46.780066410711));
#26267=CARTESIAN_POINT('Ctrl Pts',(43.9052450307496,35.0427993577656,46.7933224849028));
#26268=CARTESIAN_POINT('Ctrl Pts',(43.983883608601,35.0343117662949,46.8932147988588));
#26269=CARTESIAN_POINT('Ctrl Pts',(44.0444360973722,35.0266669205856,46.9853654748048));
#26270=CARTESIAN_POINT('Ctrl Pts',(44.1654091204863,35.0086315499937,47.2090063529896));
#26271=CARTESIAN_POINT('Ctrl Pts',(44.2195845043396,34.9981672353549,47.3431474463877));
#26272=CARTESIAN_POINT('Ctrl Pts',(44.2639737984576,34.986847708075,47.5024157689889));
#26273=CARTESIAN_POINT('Ctrl Pts',(44.2693085596672,34.98541633751,47.5228480455898));
#26274=CARTESIAN_POINT('Ctrl Pts',(44.2761197078823,34.9834897765473,47.5508051172287));
#26275=CARTESIAN_POINT('Ctrl Pts',(44.2778881025543,34.9829793763453,47.5582563184348));
#26276=CARTESIAN_POINT('Ctrl Pts',(44.2807782840316,34.9821278935009,47.5707652877429));
#26277=CARTESIAN_POINT('Ctrl Pts',(44.28192413927,34.9817854651245,47.5758173412128));
#26278=CARTESIAN_POINT('Ctrl Pts',(44.2840652326116,34.9811363153673,47.585436848361));
#26279=CARTESIAN_POINT('Ctrl Pts',(44.2850642385299,34.9808293728925,47.5900033838992));
#26280=CARTESIAN_POINT('Ctrl Pts',(44.2874024902125,34.9801010325886,47.6008809473366));
#26281=CARTESIAN_POINT('Ctrl Pts',(44.2887267061933,34.9796804829437,47.6071952005278));
#26282=CARTESIAN_POINT('Ctrl Pts',(44.2933144363477,34.9781937748502,47.6296305413415));
#26283=CARTESIAN_POINT('Ctrl Pts',(44.2964035368075,34.9771369616707,47.6457871264666));
#26284=CARTESIAN_POINT('Ctrl Pts',(44.3169410161658,34.9696741669035,47.7611849111638));
#26285=CARTESIAN_POINT('Ctrl Pts',(44.3267991839944,34.9636224366732,47.8616322056378));
#26286=CARTESIAN_POINT('Ctrl Pts',(44.3308895465952,34.9510878852683,48.0714600661437));
#26287=CARTESIAN_POINT('Ctrl Pts',(44.3237620215163,34.9446275369778,48.1804966275108));
#26288=CARTESIAN_POINT('Ctrl Pts',(44.299062238229,34.934476137338,48.3438912680237));
#26289=CARTESIAN_POINT('Ctrl Pts',(44.2882436519479,34.9309691664652,48.3990408313915));
#26290=CARTESIAN_POINT('Ctrl Pts',(44.2713494562757,34.9263854749343,48.4688703812571));
#26291=CARTESIAN_POINT('Ctrl Pts',(44.2674783415885,34.9253797720401,48.4840587176716));
#26292=CARTESIAN_POINT('Ctrl Pts',(44.2609064035717,34.9237404364646,48.5085906712521));
#26293=CARTESIAN_POINT('Ctrl Pts',(44.2583191876121,34.9231104965663,48.5179641927033));
#26294=CARTESIAN_POINT('Ctrl Pts',(44.2532151072212,34.9218963733623,48.5359257475557));
#26295=CARTESIAN_POINT('Ctrl Pts',(44.2507091271093,34.9213125589365,48.5445166322527));
#26296=CARTESIAN_POINT('Ctrl Pts',(44.2448330791886,34.91997095172,48.5641513872732));
#26297=CARTESIAN_POINT('Ctrl Pts',(44.2414234760309,34.9192118798823,48.5751829707751));
#26298=CARTESIAN_POINT('Ctrl Pts',(44.2302546745037,34.9167849900989,48.610201567812));
#26299=CARTESIAN_POINT('Ctrl Pts',(44.2221244811639,34.9151050605648,48.6340665574879));
#26300=CARTESIAN_POINT('Ctrl Pts',(44.1666592338434,34.9041664322035,48.7869903754927));
#26301=CARTESIAN_POINT('Ctrl Pts',(44.1061196249513,34.8944604748934,48.9108136201175));
#26302=CARTESIAN_POINT('Ctrl Pts',(43.9877161565048,34.8785772710473,49.0990537908569));
#26303=CARTESIAN_POINT('Ctrl Pts',(43.9377729480523,34.8724948295363,49.1679116577878));
#26304=CARTESIAN_POINT('Ctrl Pts',(43.866716044311,34.8647503090157,49.2533841444767));
#26305=CARTESIAN_POINT('Ctrl Pts',(43.8495730441084,34.8629429605096,49.2731715904035));
#26306=CARTESIAN_POINT('Ctrl Pts',(43.8200964089438,34.8599438900837,49.3058277224253));
#26307=CARTESIAN_POINT('Ctrl Pts',(43.8079779468813,34.8587401551891,49.3188851383942));
#26308=CARTESIAN_POINT('Ctrl Pts',(43.790732492187,34.8570698796681,49.3369581332117));
#26309=CARTESIAN_POINT('Ctrl Pts',(43.7857561942951,34.8565927695146,49.3421153783514));
#26310=CARTESIAN_POINT('Ctrl Pts',(43.7771994086913,34.8557808244713,49.3508849732577));
#26311=CARTESIAN_POINT('Ctrl Pts',(43.7736331919415,34.8554449064301,49.3545110847558));
#26312=CARTESIAN_POINT('Ctrl Pts',(43.7662061707503,34.8547505080362,49.3620033431059));
#26313=CARTESIAN_POINT('Ctrl Pts',(43.7623432387804,34.8543921999436,49.3658672370415));
#26314=CARTESIAN_POINT('Ctrl Pts',(43.752100855387,34.8534495116636,49.3760254894496));
#26315=CARTESIAN_POINT('Ctrl Pts',(43.7456937778531,34.8528672738467,49.3822919860276));
#26316=CARTESIAN_POINT('Ctrl Pts',(43.7182011406565,34.8503992269926,49.408809062208));
#26317=CARTESIAN_POINT('Ctrl Pts',(43.6966991771984,34.8485441541264,49.4286247529707));
#26318=CARTESIAN_POINT('Ctrl Pts',(43.5817327160059,34.838958364565,49.5298398547034));
#26319=CARTESIAN_POINT('Ctrl Pts',(43.48102658351,34.8316658507289,49.6025886101786));
#26320=CARTESIAN_POINT('Ctrl Pts',(43.2738953751537,34.817326565828,49.7237477629708));
#26321=CARTESIAN_POINT('Ctrl Pts',(43.1686983903165,34.8103202804322,49.7731602450541));
#26322=CARTESIAN_POINT('Ctrl Pts',(43.0399753166011,34.8016411173085,49.8200041543026));
#26323=CARTESIAN_POINT('Ctrl Pts',(43.0201267719649,34.8003006256163,49.8268624083264));
#26324=CARTESIAN_POINT('Ctrl Pts',(42.9898516257488,34.7982507809556,49.8367731252652));
#26325=CARTESIAN_POINT('Ctrl Pts',(42.9795042623673,34.7975492864027,49.8400639271551));
#26326=CARTESIAN_POINT('Ctrl Pts',(42.9606674079949,34.7962703604362,49.8458800216732));
#26327=CARTESIAN_POINT('Ctrl Pts',(42.9521872018552,34.7956939072857,49.8484345502355));
#26328=CARTESIAN_POINT('Ctrl Pts',(42.9338505096312,34.7944458174774,49.8538207452563));
#26329=CARTESIAN_POINT('Ctrl Pts',(42.9239884718509,34.7937735458424,49.8566323805848));
#26330=CARTESIAN_POINT('Ctrl Pts',(42.8971016034674,34.7919377531545,49.8640664574837));
#26331=CARTESIAN_POINT('Ctrl Pts',(42.8800353778499,34.7907692568002,49.8685341213847));
#26332=CARTESIAN_POINT('Ctrl Pts',(42.7873740701533,34.7844056379229,49.8914381538581));
#26333=CARTESIAN_POINT('Ctrl Pts',(42.7107869000632,34.7790726081068,49.9055197886155));
#26334=CARTESIAN_POINT('Ctrl Pts',(42.5051008804217,34.7645718249996,49.9306075358704));
#26335=CARTESIAN_POINT('Ctrl Pts',(42.3753871547979,34.7552242677233,49.9333084875517));
#26336=CARTESIAN_POINT('Ctrl Pts',(42.1826551680896,34.741549554268,49.917913597022));
#26337=CARTESIAN_POINT('Ctrl Pts',(42.1191997759921,34.7370886048187,49.9096555631087));
#26338=CARTESIAN_POINT('Ctrl Pts',(42.0456199791526,34.7320470361389,49.8963318283593));
#26339=CARTESIAN_POINT('Ctrl Pts',(42.0349904446744,34.7313219854366,49.8943145568442));
#26340=CARTESIAN_POINT('Ctrl Pts',(42.0186212939061,34.7302110600325,49.8910651196483));
#26341=CARTESIAN_POINT('Ctrl Pts',(42.0128695920834,34.729821785173,49.8898960431079));
#26342=CARTESIAN_POINT('Ctrl Pts',(42.0022458314604,34.7291048736054,49.8876861488563));
#26343=CARTESIAN_POINT('Ctrl Pts',(41.9973724785929,34.7287768438049,49.8866527118456));
#26344=CARTESIAN_POINT('Ctrl Pts',(41.9862508695943,34.7280300966293,49.884249221513));
#26345=CARTESIAN_POINT('Ctrl Pts',(41.9800053836516,34.727612079981,49.8828669620595));
#26346=CARTESIAN_POINT('Ctrl Pts',(41.9636401959279,34.7265199539365,49.8791595166354));
#26347=CARTESIAN_POINT('Ctrl Pts',(41.9535320307828,34.7258486186065,49.8767836133903));
#26348=CARTESIAN_POINT('Ctrl Pts',(41.893116594292,34.7218527854595,49.8620673518438));
#26349=CARTESIAN_POINT('Ctrl Pts',(41.8433080751587,34.7186276828276,49.8477875483252));
#26350=CARTESIAN_POINT('Ctrl Pts',(41.7941388232987,34.7154586800303,49.8315225337042));
#26351=CARTESIAN_POINT('Origin',(42.4,48.4493818343519,48.));
#26352=CARTESIAN_POINT('',(41.7941388605861,33.7518842900812,49.8315225460387));
#26353=CARTESIAN_POINT('',(41.7941388307093,33.9245485747014,49.8315225361556));
#26354=CARTESIAN_POINT('',(41.7941388317924,48.4493818343519,49.8315225365138));
#26355=CARTESIAN_POINT('Ctrl Pts',(41.7941388605861,33.7518842900812,49.8315225460387));
#26356=CARTESIAN_POINT('Ctrl Pts',(41.822232866932,33.7536518916214,49.8408159433448));
#26357=CARTESIAN_POINT('Ctrl Pts',(41.8505427048789,33.7554237930209,49.8494635973993));
#26358=CARTESIAN_POINT('Ctrl Pts',(41.9390087870209,33.7609551756864,49.8742753243044));
#26359=CARTESIAN_POINT('Ctrl Pts',(41.9997463210171,33.7647460998173,49.8881782151908));
#26360=CARTESIAN_POINT('Ctrl Pts',(42.0871543217508,33.7702702333918,49.903778733364));
#26361=CARTESIAN_POINT('Ctrl Pts',(42.1133543773063,33.7719344596225,49.9078993867084));
#26362=CARTESIAN_POINT('Ctrl Pts',(42.1602908109223,33.7749363406311,49.914292779316));
#26363=CARTESIAN_POINT('Ctrl Pts',(42.1809950745463,33.7762675639675,49.91677179882));
#26364=CARTESIAN_POINT('Ctrl Pts',(42.2125073581935,33.7783062277639,49.9200276957443));
#26365=CARTESIAN_POINT('Ctrl Pts',(42.2232888838593,33.7790059447404,49.9210499776618));
#26366=CARTESIAN_POINT('Ctrl Pts',(42.2420512235811,33.7802277014822,49.92266970193));
#26367=CARTESIAN_POINT('Ctrl Pts',(42.2500282833642,33.7807484300427,49.9233083683212));
#26368=CARTESIAN_POINT('Ctrl Pts',(42.2679610254475,33.7819220376976,49.9246318735474));
#26369=CARTESIAN_POINT('Ctrl Pts',(42.2779184515369,33.7825757694634,49.9252891285832));
#26370=CARTESIAN_POINT('Ctrl Pts',(42.3046863918602,33.7843389299273,49.926847495933));
#26371=CARTESIAN_POINT('Ctrl Pts',(42.3215040257394,33.7854527986798,49.9276058486636));
#26372=CARTESIAN_POINT('Ctrl Pts',(42.4009561856744,33.7907453579105,49.9301470983325));
#26373=CARTESIAN_POINT('Ctrl Pts',(42.4636370639459,33.7950112832498,49.929097602358));
#26374=CARTESIAN_POINT('Ctrl Pts',(42.6529815685964,33.8081735173773,49.9166893733019));
#26375=CARTESIAN_POINT('Ctrl Pts',(42.7786717357399,33.8173093371442,49.8958637648311));
#26376=CARTESIAN_POINT('Ctrl Pts',(42.9809484443892,33.8322197798767,49.8414208014523));
#26377=CARTESIAN_POINT('Ctrl Pts',(43.0590691797337,33.8380239895011,49.8149277386139));
#26378=CARTESIAN_POINT('Ctrl Pts',(43.145745860273,33.8443511675098,49.7791948218707));
#26379=CARTESIAN_POINT('Ctrl Pts',(43.1561898664617,33.8451115677599,49.7747811142232));
#26380=CARTESIAN_POINT('Ctrl Pts',(43.172082132481,33.8462649352774,49.7678991760523));
#26381=CARTESIAN_POINT('Ctrl Pts',(43.1775586212095,33.8466617091395,49.7654973545625));
#26382=CARTESIAN_POINT('Ctrl Pts',(43.1875706076989,33.8473857196794,49.7610507785014));
#26383=CARTESIAN_POINT('Ctrl Pts',(43.1921093776766,33.847713410377,49.7590139401158));
#26384=CARTESIAN_POINT('Ctrl Pts',(43.2023422647975,33.8484510431897,49.7543741455057));
#26385=CARTESIAN_POINT('Ctrl Pts',(43.2080316209621,33.8488603562039,49.7517610152487));
#26386=CARTESIAN_POINT('Ctrl Pts',(43.2227085533099,33.849914448055,49.7449331591289));
#26387=CARTESIAN_POINT('Ctrl Pts',(43.2316766320263,33.850556758547,49.7406766165279));
#26388=CARTESIAN_POINT('Ctrl Pts',(43.291606577009,33.8548397688464,49.7116630047079));
#26389=CARTESIAN_POINT('Ctrl Pts',(43.3414945753509,33.8583601345675,49.6847379095925));
#26390=CARTESIAN_POINT('Ctrl Pts',(43.5000139619265,33.8696313080522,49.5899386099328));
#26391=CARTESIAN_POINT('Ctrl Pts',(43.6030868347116,33.8771162984925,49.5134465912978));
#26392=CARTESIAN_POINT('Ctrl Pts',(43.7617847498799,33.8900687937594,49.3691450268038));
#26393=CARTESIAN_POINT('Ctrl Pts',(43.821755891981,33.8953819176344,49.3067605727313));
#26394=CARTESIAN_POINT('Ctrl Pts',(43.888708870321,33.9020059845809,49.2270293897812));
#26395=CARTESIAN_POINT('Ctrl Pts',(43.8998929007683,33.9031381900633,49.2133327971986));
#26396=CARTESIAN_POINT('Ctrl Pts',(43.9172059670459,33.9049331095973,49.1915250311266));
#26397=CARTESIAN_POINT('Ctrl Pts',(43.9234620486964,33.9055907181354,49.1835156212978));
#26398=CARTESIAN_POINT('Ctrl Pts',(43.9350574786617,33.9068268289098,49.168426173626));
#26399=CARTESIAN_POINT('Ctrl Pts',(43.9404118844503,33.9074047137297,49.161358001576));
#26400=CARTESIAN_POINT('Ctrl Pts',(43.9522911470585,33.9087029632722,49.145449896967));
#26401=CARTESIAN_POINT('Ctrl Pts',(43.9587895524967,33.9094243363076,49.1365906889546));
#26402=CARTESIAN_POINT('Ctrl Pts',(43.9751326445211,33.9112675886956,49.1139065253));
#26403=CARTESIAN_POINT('Ctrl Pts',(43.9848710461081,33.9123934958351,49.1000065139391));
#26404=CARTESIAN_POINT('Ctrl Pts',(44.0634051406204,33.9217063028889,48.9847035949815));
#26405=CARTESIAN_POINT('Ctrl Pts',(44.1225667772653,33.9302559084962,48.8771040053248));
#26406=CARTESIAN_POINT('Ctrl Pts',(44.2057662416209,33.9451935126621,48.6843912200507));
#26407=CARTESIAN_POINT('Ctrl Pts',(44.234918345372,33.9514748609294,48.6018787104879));
#26408=CARTESIAN_POINT('Ctrl Pts',(44.2744041595347,33.9618614540488,48.4601301510694));
#26409=CARTESIAN_POINT('Ctrl Pts',(44.2877539665317,33.9660189564635,48.4018671269507));
#26410=CARTESIAN_POINT('Ctrl Pts',(44.3002745969006,33.970764309379,48.3325847339285));
#26411=CARTESIAN_POINT('Ctrl Pts',(44.3020830922692,33.9714784137988,48.3220808465803));
#26412=CARTESIAN_POINT('Ctrl Pts',(44.3047470050473,33.9725762548199,48.3058029772046));
#26413=CARTESIAN_POINT('Ctrl Pts',(44.3056633960849,33.9729632690532,48.3000393926898));
#26414=CARTESIAN_POINT('Ctrl Pts',(44.3073144007316,33.9736782628013,48.2893427150847));
#26415=CARTESIAN_POINT('Ctrl Pts',(44.3080560377137,33.9740066158058,48.2844109488446));
#26416=CARTESIAN_POINT('Ctrl Pts',(44.3097126228468,33.9747569820751,48.2730967317232));
#26417=CARTESIAN_POINT('Ctrl Pts',(44.3106147069066,33.9751782686558,48.2667125258596));
#26418=CARTESIAN_POINT('Ctrl Pts',(44.3129086928837,33.9762844969707,48.2498684293201));
#26419=CARTESIAN_POINT('Ctrl Pts',(44.3142468349627,33.9769665484997,48.2394012658995));
#26420=CARTESIAN_POINT('Ctrl Pts',(44.3257343374219,33.9831849895461,48.143280453926));
#26421=CARTESIAN_POINT('Ctrl Pts',(44.3302157675812,33.9884399286319,48.0570355704692));
#26422=CARTESIAN_POINT('Ctrl Pts',(44.3276721578753,33.9985245239661,47.8891793323548));
#26423=CARTESIAN_POINT('Ctrl Pts',(44.3212602332266,34.0033524974198,47.8077488620513));
#26424=CARTESIAN_POINT('Ctrl Pts',(44.2966692910322,34.0137850425702,47.6357481252508));
#26425=CARTESIAN_POINT('Ctrl Pts',(44.2771100328848,34.0193981362937,47.5455896322356));
#26426=CARTESIAN_POINT('Ctrl Pts',(44.2445294432212,34.0267122473274,47.4344796095866));
#26427=CARTESIAN_POINT('Ctrl Pts',(44.2374562652596,34.0282190477954,47.4119042816743));
#26428=CARTESIAN_POINT('Ctrl Pts',(44.2263673909003,34.0304709975937,47.3786673279568));
#26429=CARTESIAN_POINT('Ctrl Pts',(44.2226693515696,34.0312057004179,47.3679014621302));
#26430=CARTESIAN_POINT('Ctrl Pts',(44.2159090450167,34.0325207850789,47.3487733177477));
#26431=CARTESIAN_POINT('Ctrl Pts',(44.2128837225318,34.033099924758,47.3403982598858));
#26432=CARTESIAN_POINT('Ctrl Pts',(44.2063690206875,34.0343277501909,47.3227469160133));
#26433=CARTESIAN_POINT('Ctrl Pts',(44.202865932548,34.0349768811725,47.3134760006393));
#26434=CARTESIAN_POINT('Ctrl Pts',(44.1933332323262,34.0367145428095,47.2888239280374));
#26435=CARTESIAN_POINT('Ctrl Pts',(44.1871773215702,34.037807293458,47.273492821955));
#26436=CARTESIAN_POINT('Ctrl Pts',(44.1584582388205,34.0427780331259,47.2045434525091));
#26437=CARTESIAN_POINT('Ctrl Pts',(44.1336758491486,34.0467304939546,47.1518883694762));
#26438=CARTESIAN_POINT('Ctrl Pts',(44.0386686874587,34.0608229742627,46.9716508100176));
#26439=CARTESIAN_POINT('Ctrl Pts',(43.9564258887153,34.0713329470031,46.8509715297968));
#26440=CARTESIAN_POINT('Ctrl Pts',(43.8305802676179,34.0849998679582,46.7049271815965));
#26441=CARTESIAN_POINT('Ctrl Pts',(43.7984418401567,34.088319077317,46.6702878052449));
#26442=CARTESIAN_POINT('Ctrl Pts',(43.7458736411927,34.0934469748352,46.6176454355684));
#26443=CARTESIAN_POINT('Ctrl Pts',(43.7262802320962,34.0952973005341,46.5988358662521));
#26444=CARTESIAN_POINT('Ctrl Pts',(43.700106436352,34.0976832655497,46.5747503585811));
#26445=CARTESIAN_POINT('Ctrl Pts',(43.6938805498566,34.098244647818,46.5690959447452));
#26446=CARTESIAN_POINT('Ctrl Pts',(43.6836392776758,34.099157787683,46.559916215332));
#26447=CARTESIAN_POINT('Ctrl Pts',(43.6796459530222,34.0995113150944,46.5563666190093));
#26448=CARTESIAN_POINT('Ctrl Pts',(43.6718136874222,34.1001996894999,46.5494626896049));
#26449=CARTESIAN_POINT('Ctrl Pts',(43.6679761272525,34.1005346379584,46.5461069207236));
#26450=CARTESIAN_POINT('Ctrl Pts',(43.6593679387113,34.1012808933833,46.538639464254));
#26451=CARTESIAN_POINT('Ctrl Pts',(43.6545903417644,34.1016916133191,46.5345358081608));
#26452=CARTESIAN_POINT('Ctrl Pts',(43.6379587537702,34.1031098144803,46.5203912639077));
#26453=CARTESIAN_POINT('Ctrl Pts',(43.6260032655341,34.1041090369793,46.510469900359));
#26454=CARTESIAN_POINT('Ctrl Pts',(43.5144048639429,34.113265076725,46.4201131076715));
#26455=CARTESIAN_POINT('Ctrl Pts',(43.4070898477608,34.1208376588896,46.3496302408002));
#26456=CARTESIAN_POINT('Ctrl Pts',(43.1786794086179,34.1362127229208,46.2302526907813));
#26457=CARTESIAN_POINT('Ctrl Pts',(43.0580482310038,34.1439878431679,46.1819478068621));
#26458=CARTESIAN_POINT('Ctrl Pts',(42.9131658630505,34.1535383970897,46.1402551869565));
#26459=CARTESIAN_POINT('Ctrl Pts',(42.8927444220757,34.1548884716449,46.1347405406489));
#26460=CARTESIAN_POINT('Ctrl Pts',(42.8616774375999,34.1569501218697,46.1268969292018));
#26461=CARTESIAN_POINT('Ctrl Pts',(42.8510956127996,34.1576537004727,46.1243204137463));
#26462=CARTESIAN_POINT('Ctrl Pts',(42.8318658413446,34.1589349807853,46.1198103902428));
#26463=CARTESIAN_POINT('Ctrl Pts',(42.8232252530903,34.1595116886301,46.1178465911896));
#26464=CARTESIAN_POINT('Ctrl Pts',(42.8045757816949,34.1607586916989,46.1137429265483));
#26465=CARTESIAN_POINT('Ctrl Pts',(42.7945628234948,34.1614296100013,46.1116230562385));
#26466=CARTESIAN_POINT('Ctrl Pts',(42.7673414443359,34.1632576027063,46.1060858992027));
#26467=CARTESIAN_POINT('Ctrl Pts',(42.7501028552816,34.164419580178,46.1028235944153));
#26468=CARTESIAN_POINT('Ctrl Pts',(42.6579389246497,34.1706568500298,46.0866809810984));
#26469=CARTESIAN_POINT('Ctrl Pts',(42.5823550218172,34.1758634698669,46.0780046345243));
#26470=CARTESIAN_POINT('Ctrl Pts',(42.3764480937858,34.1902812780343,46.066623744375));
#26471=CARTESIAN_POINT('Ctrl Pts',(42.2460421317458,34.1996848832864,46.0726207067847));
#26472=CARTESIAN_POINT('Ctrl Pts',(42.0529119774787,34.2135001337758,46.1012365076659));
#26473=CARTESIAN_POINT('Ctrl Pts',(41.9890891160381,34.2180403938353,46.1140182900721));
#26474=CARTESIAN_POINT('Ctrl Pts',(41.9155003542557,34.2231591837011,46.1326701960611));
#26475=CARTESIAN_POINT('Ctrl Pts',(41.9049953446786,34.2238870637065,46.1354274194632));
#26476=CARTESIAN_POINT('Ctrl Pts',(41.8888402157113,34.2250014560545,46.1398137739898));
#26477=CARTESIAN_POINT('Ctrl Pts',(41.8831735240769,34.2253913999013,46.1413802119356));
#26478=CARTESIAN_POINT('Ctrl Pts',(41.8727177472141,34.2261090285339,46.1443220086038));
#26479=CARTESIAN_POINT('Ctrl Pts',(41.8679268370499,34.2264371112157,46.1456900118711));
#26480=CARTESIAN_POINT('Ctrl Pts',(41.8570058982627,34.2271833349804,46.1488542026762));
#26481=CARTESIAN_POINT('Ctrl Pts',(41.8508794513008,34.2276007805745,46.1506622852088));
#26482=CARTESIAN_POINT('Ctrl Pts',(41.8348500160493,34.2286901989678,46.1554796901142));
#26483=CARTESIAN_POINT('Ctrl Pts',(41.824961912613,34.2293594209598,46.1585383828746));
#26484=CARTESIAN_POINT('Ctrl Pts',(41.7501110949605,34.2344073203972,46.1823537487832));
#26485=CARTESIAN_POINT('Ctrl Pts',(41.6862578720286,34.2386111744229,46.2064649945738));
#26486=CARTESIAN_POINT('Ctrl Pts',(41.5165427710139,34.2498404528727,46.2810542431062));
#26487=CARTESIAN_POINT('Ctrl Pts',(41.4137929734696,34.2567139827875,46.3378723595751));
#26488=CARTESIAN_POINT('Ctrl Pts',(41.2464251629701,34.2689351904334,46.4514371182954));
#26489=CARTESIAN_POINT('Ctrl Pts',(41.1792645126794,34.2741681040886,46.5038101457411));
#26490=CARTESIAN_POINT('Ctrl Pts',(41.102638404023,34.2807018327569,46.5721674471779));
#26491=CARTESIAN_POINT('Ctrl Pts',(41.0896539549867,34.2818299135345,46.5840741125088));
#26492=CARTESIAN_POINT('Ctrl Pts',(41.0694492480694,34.2836197650522,46.6031176660628));
#26493=CARTESIAN_POINT('Ctrl Pts',(41.0621189340754,34.2842764793782,46.6101367674373));
#26494=CARTESIAN_POINT('Ctrl Pts',(41.0484874040636,34.2855117997793,46.6233973286953));
#26495=CARTESIAN_POINT('Ctrl Pts',(41.0421731589124,34.2860897960855,46.6296250597706));
#26496=CARTESIAN_POINT('Ctrl Pts',(41.0281192077104,34.2873894689447,46.643678947646));
#26497=CARTESIAN_POINT('Ctrl Pts',(41.0204031390884,34.2881121637219,46.6515281989891));
#26498=CARTESIAN_POINT('Ctrl Pts',(41.0009159954926,34.2899610812866,46.6716940291253));
#26499=CARTESIAN_POINT('Ctrl Pts',(40.9892403401556,34.2910913745722,46.6841010850821));
#26500=CARTESIAN_POINT('Ctrl Pts',(40.8936505525185,34.30053715089,46.7884134603802));
#26501=CARTESIAN_POINT('Ctrl Pts',(40.8186616933008,34.3092274526194,46.8880695941978));
#26502=CARTESIAN_POINT('Ctrl Pts',(40.7036961735488,34.3249268822896,47.0762404764824));
#26503=CARTESIAN_POINT('Ctrl Pts',(40.6597895922981,34.3318390663899,47.1618790247895));
#26504=CARTESIAN_POINT('Ctrl Pts',(40.6094580324446,34.3409325254711,47.2812374673108));
#26505=CARTESIAN_POINT('Ctrl Pts',(40.597270890511,34.3432569320642,47.3123750029397));
#26506=CARTESIAN_POINT('Ctrl Pts',(40.5786469511589,34.3470064002948,47.3638631204653));
#26507=CARTESIAN_POINT('Ctrl Pts',(40.5717278269332,34.348451890723,47.3840308349642));
#26508=CARTESIAN_POINT('Ctrl Pts',(40.5627702807873,34.3503942691453,47.4116220472493));
#26509=CARTESIAN_POINT('Ctrl Pts',(40.5604401227929,34.3509066791423,47.4189482642897));
#26510=CARTESIAN_POINT('Ctrl Pts',(40.5566110700961,34.35176064346,47.4312410710871));
#26511=CARTESIAN_POINT('Ctrl Pts',(40.5550883199822,34.3521035591689,47.4362000699688));
#26512=CARTESIAN_POINT('Ctrl Pts',(40.5522324946862,34.3527529681196,47.4456358415189));
#26513=CARTESIAN_POINT('Ctrl Pts',(40.550895650163,34.3530596870152,47.4501113944811));
#26514=CARTESIAN_POINT('Ctrl Pts',(40.5477560653823,34.3537866687357,47.4607631708681));
#26515=CARTESIAN_POINT('Ctrl Pts',(40.5459679271681,34.3542060914673,47.4669436924442));
#26516=CARTESIAN_POINT('Ctrl Pts',(40.5397491837934,34.3556844769308,47.4888480452854));
#26517=CARTESIAN_POINT('Ctrl Pts',(40.5354872685443,34.3567342316163,47.5046196039287));
#26518=CARTESIAN_POINT('Ctrl Pts',(40.5039981188426,34.3648008905328,47.6273160302459));
#26519=CARTESIAN_POINT('Ctrl Pts',(40.4857856548616,34.3713906875167,47.7363592224183));
#26520=CARTESIAN_POINT('Ctrl Pts',(40.4729574251635,34.381001334332,47.8969355725878));
#26521=CARTESIAN_POINT('Ctrl Pts',(40.4709138645376,34.3840211774907,47.947636469111));
#26522=CARTESIAN_POINT('Ctrl Pts',(40.4707861256103,34.3930358092416,48.0977350015402));
#26523=CARTESIAN_POINT('Ctrl Pts',(40.4783802582461,34.3990998965189,48.1969569761711));
#26524=CARTESIAN_POINT('Ctrl Pts',(40.4961681072347,34.4064865455506,48.3118534100388));
#26525=CARTESIAN_POINT('Ctrl Pts',(40.4989743511027,34.4075672804918,48.328526830668));
#26526=CARTESIAN_POINT('Ctrl Pts',(40.5039616422314,34.40936046529,48.3559513875274));
#26527=CARTESIAN_POINT('Ctrl Pts',(40.5060159146132,34.410068885306,48.3667248566709));
#26528=CARTESIAN_POINT('Ctrl Pts',(40.5098967328105,34.4113552991853,48.3861745728868));
#26529=CARTESIAN_POINT('Ctrl Pts',(40.5116914518943,34.4119322605123,48.394856916009));
#26530=CARTESIAN_POINT('Ctrl Pts',(40.5156747691385,34.413175678189,48.413478606991));
#26531=CARTESIAN_POINT('Ctrl Pts',(40.517882293313,34.4138427268711,48.4234135868458));
#26532=CARTESIAN_POINT('Ctrl Pts',(40.5241549233981,34.4156800395814,48.4506248946602));
#26533=CARTESIAN_POINT('Ctrl Pts',(40.5283799102703,34.4168554100861,48.4678629616182));
#26534=CARTESIAN_POINT('Ctrl Pts',(40.5549316371666,34.4238949726744,48.57007368465));
#26535=CARTESIAN_POINT('Ctrl Pts',(40.582800968148,34.4299378299245,48.6534867852099));
#26536=CARTESIAN_POINT('Ctrl Pts',(40.6464316700164,34.4416829137335,48.8079729171388));
#26537=CARTESIAN_POINT('Ctrl Pts',(40.6810960239106,34.4473483890802,48.8793122636293));
#26538=CARTESIAN_POINT('Ctrl Pts',(40.7430166382132,34.4563440869029,48.9890056276619));
#26539=CARTESIAN_POINT('Ctrl Pts',(40.7674581965911,34.4596748902882,49.0288505782284));
#26540=CARTESIAN_POINT('Ctrl Pts',(40.824926217424,34.4669968685006,49.1153229112449));
#26541=CARTESIAN_POINT('Ctrl Pts',(40.8586282703096,34.4709673971012,49.1614547548541));
#26542=CARTESIAN_POINT('Ctrl Pts',(40.9005475816166,34.4754900603971,49.2137890641451));
#26543=CARTESIAN_POINT('Ctrl Pts',(40.9068245480763,34.4761571194766,49.2215025694966));
#26544=CARTESIAN_POINT('Ctrl Pts',(40.9171534908594,34.4772379022806,49.2339967787161));
#26545=CARTESIAN_POINT('Ctrl Pts',(40.9211695155563,34.4776540510741,49.2388067728988));
#26546=CARTESIAN_POINT('Ctrl Pts',(40.9284161351557,34.4783975626133,49.2474005921585));
#26547=CARTESIAN_POINT('Ctrl Pts',(40.9316379861234,34.4787255343173,49.2511915546809));
#26548=CARTESIAN_POINT('Ctrl Pts',(40.938761774172,34.4794450204533,49.259508280677));
#26549=CARTESIAN_POINT('Ctrl Pts',(40.9426700885461,34.4798360582377,49.2640283989205));
#26550=CARTESIAN_POINT('Ctrl Pts',(40.9540404841992,34.4809633185002,49.2770558677993));
#26551=CARTESIAN_POINT('Ctrl Pts',(40.9615566492439,34.4816956758803,49.2855159868407));
#26552=CARTESIAN_POINT('Ctrl Pts',(41.0237176309969,34.4876535480489,49.3542558866026));
#26553=CARTESIAN_POINT('Ctrl Pts',(41.0820586461966,34.4926284061482,49.4110975074084));
#26554=CARTESIAN_POINT('Ctrl Pts',(41.1636066726752,34.499097073166,49.4810650375875));
#26555=CARTESIAN_POINT('Ctrl Pts',(41.183733102733,34.5006577960072,49.497637131573));
#26556=CARTESIAN_POINT('Ctrl Pts',(41.3237425838724,34.5113172752224,49.6082364214939));
#26557=CARTESIAN_POINT('Ctrl Pts',(41.4540469681758,34.5203205575784,49.6881711066788));
#26558=CARTESIAN_POINT('Ctrl Pts',(41.612259052673,34.5313176092528,49.7611034498652));
#26559=CARTESIAN_POINT('Ctrl Pts',(41.6322804190894,34.5327092175118,49.7699230900791));
#26560=CARTESIAN_POINT('Ctrl Pts',(41.662747235911,34.5348289892727,49.7827298630114));
#26561=CARTESIAN_POINT('Ctrl Pts',(41.6730848933726,34.5355486080241,49.7869700114368));
#26562=CARTESIAN_POINT('Ctrl Pts',(41.6911659544066,34.5368081644647,49.7942033782588));
#26563=CARTESIAN_POINT('Ctrl Pts',(41.6988930012064,34.5373467295258,49.7972368901701));
#26564=CARTESIAN_POINT('Ctrl Pts',(41.7151285381673,34.5384790448898,49.8034900597894));
#26565=CARTESIAN_POINT('Ctrl Pts',(41.7236406861229,34.5390731192959,49.8066995845257));
#26566=CARTESIAN_POINT('Ctrl Pts',(41.7440293527125,34.5404972112604,49.8142228979678));
#26567=CARTESIAN_POINT('Ctrl Pts',(41.7559260520934,34.5413290818809,49.8184803959012));
#26568=CARTESIAN_POINT('Ctrl Pts',(41.7766008805053,34.5427765967051,49.825651012675));
#26569=CARTESIAN_POINT('Ctrl Pts',(41.7853595582974,34.5433903872487,49.828618383941));
#26570=CARTESIAN_POINT('Ctrl Pts',(41.7941388327286,34.5440062296316,49.8315225368236));
#26571=CARTESIAN_POINT('Ctrl Pts',(41.7941388232987,34.7154586800303,49.8315225337042));
#26572=CARTESIAN_POINT('Ctrl Pts',(41.7736344100669,34.714137152034,49.8247397463239));
#26573=CARTESIAN_POINT('Ctrl Pts',(41.7532411651284,34.7128254112523,49.8176117253353));
#26574=CARTESIAN_POINT('Ctrl Pts',(41.6271329352352,34.7047064784872,49.7711411799934));
#26575=CARTESIAN_POINT('Ctrl Pts',(41.5249219055423,34.6980803716224,49.7229346514742));
#26576=CARTESIAN_POINT('Ctrl Pts',(41.3547263418778,34.6861683763357,49.6235908599801));
#26577=CARTESIAN_POINT('Ctrl Pts',(41.2848160891351,34.6809832881044,49.5763903433538));
#26578=CARTESIAN_POINT('Ctrl Pts',(41.2043303672012,34.6745036307842,49.5140097467574));
#26579=CARTESIAN_POINT('Ctrl Pts',(41.1905885079584,34.6733782777764,49.5030552864632));
#26580=CARTESIAN_POINT('Ctrl Pts',(41.1691584495875,34.6715918978665,49.485487936064));
#26581=CARTESIAN_POINT('Ctrl Pts',(41.1613692318657,34.6709358959196,49.4789993725914));
#26582=CARTESIAN_POINT('Ctrl Pts',(41.1468637234907,34.6697013977175,49.4667210548757));
#26583=CARTESIAN_POINT('Ctrl Pts',(41.1401354822522,34.6691235064202,49.4609457802432));
#26584=CARTESIAN_POINT('Ctrl Pts',(41.1251388869164,34.6678233882103,49.447892616609));
#26585=CARTESIAN_POINT('Ctrl Pts',(41.1168926267176,34.6671001378894,49.4405899301812));
#26586=CARTESIAN_POINT('Ctrl Pts',(41.0960280359407,34.6652484731519,49.4217914893404));
#26587=CARTESIAN_POINT('Ctrl Pts',(41.0834991368043,34.664115965684,49.4101983432949));
#26588=CARTESIAN_POINT('Ctrl Pts',(40.9901410290625,34.6555176897455,49.3214844283058));
#26589=CARTESIAN_POINT('Ctrl Pts',(40.9160080019861,34.6477543087434,49.2376523656323));
#26590=CARTESIAN_POINT('Ctrl Pts',(40.7646708514727,34.6297048927616,49.0332428084735));
#26591=CARTESIAN_POINT('Ctrl Pts',(40.6927653889899,34.6193591071956,48.909530119822));
#26592=CARTESIAN_POINT('Ctrl Pts',(40.6266638153182,34.6081534980392,48.7597786306435));
#26593=CARTESIAN_POINT('Ctrl Pts',(40.6184864860376,34.6067280235633,48.7404015671077));
#26594=CARTESIAN_POINT('Ctrl Pts',(40.6077700144833,34.6048080346261,48.713801581663));
#26595=CARTESIAN_POINT('Ctrl Pts',(40.6049549031321,34.6042984403167,48.7066923829105));
#26596=CARTESIAN_POINT('Ctrl Pts',(40.6003044281203,34.6034479237766,48.6947411138338));
#26597=CARTESIAN_POINT('Ctrl Pts',(40.5984461786398,34.6031056622551,48.6899081080428));
#26598=CARTESIAN_POINT('Ctrl Pts',(40.5949466041338,34.602456536956,48.6806957222437));
#26599=CARTESIAN_POINT('Ctrl Pts',(40.5933017158332,34.6021494540292,48.6763177798676));
#26600=CARTESIAN_POINT('Ctrl Pts',(40.5894226091523,34.6014204126906,48.6658782188268));
#26601=CARTESIAN_POINT('Ctrl Pts',(40.5872028686953,34.6009993062913,48.6598112261992));
#26602=CARTESIAN_POINT('Ctrl Pts',(40.5794225896686,34.599508774122,48.6382105136989));
#26603=CARTESIAN_POINT('Ctrl Pts',(40.5740307096626,34.5984487558299,48.6226162231555));
#26604=CARTESIAN_POINT('Ctrl Pts',(40.5377887331214,34.5911151990029,48.5132753584692));
#26605=CARTESIAN_POINT('Ctrl Pts',(40.5139684058475,34.5851808520025,48.4173394212657));
#26606=CARTESIAN_POINT('Ctrl Pts',(40.4798757025177,34.5729010128965,48.2146520463806));
#26607=CARTESIAN_POINT('Ctrl Pts',(40.470937742682,34.5665778950104,48.1080289255605));
#26608=CARTESIAN_POINT('Ctrl Pts',(40.4708333613994,34.5564348863422,47.9425099688844));
#26609=CARTESIAN_POINT('Ctrl Pts',(40.4734761269368,34.5527783222373,47.8838373373454));
#26610=CARTESIAN_POINT('Ctrl Pts',(40.4802886718039,34.5479826264789,47.8088839201435));
#26611=CARTESIAN_POINT('Ctrl Pts',(40.4820004146344,34.5469207897803,47.7924078457148));
#26612=CARTESIAN_POINT('Ctrl Pts',(40.4850759691509,34.5452124806315,47.7661049639124));
#26613=CARTESIAN_POINT('Ctrl Pts',(40.4863038044424,34.5445703048624,47.756262853006));
#26614=CARTESIAN_POINT('Ctrl Pts',(40.488777293159,34.5433473166793,47.7376080584221));
#26615=CARTESIAN_POINT('Ctrl Pts',(40.490008147775,34.5427669876256,47.7287936466426));
#26616=CARTESIAN_POINT('Ctrl Pts',(40.492948963966,34.5414414167135,47.7087475776204));
#26617=CARTESIAN_POINT('Ctrl Pts',(40.4946972276487,34.5406949776956,47.697521961392));
#26618=CARTESIAN_POINT('Ctrl Pts',(40.5003738303096,34.5383914862416,47.6630763254425));
#26619=CARTESIAN_POINT('Ctrl Pts',(40.5046281589263,34.5368241686635,47.6399130003809));
#26620=CARTESIAN_POINT('Ctrl Pts',(40.5274451431771,34.5291132401199,47.5273247891242));
#26621=CARTESIAN_POINT('Ctrl Pts',(40.5519156806787,34.5227845801798,47.4392294293796));
#26622=CARTESIAN_POINT('Ctrl Pts',(40.5938546242095,34.5139449615261,47.3213817972854));
#26623=CARTESIAN_POINT('Ctrl Pts',(40.606014716584,34.5115432484839,47.2898588304252));
#26624=CARTESIAN_POINT('Ctrl Pts',(40.6684763460492,34.4999529559415,47.1397978064199));
#26625=CARTESIAN_POINT('Ctrl Pts',(40.7297373496898,34.4906722932919,47.0261674606001));
#26626=CARTESIAN_POINT('Ctrl Pts',(40.8105494858338,34.4808633455891,46.9066428596439));
#26627=CARTESIAN_POINT('Ctrl Pts',(40.8193852843851,34.4798179224778,46.8939078105948));
#26628=CARTESIAN_POINT('Ctrl Pts',(40.8320219355145,34.4783617239059,46.8761552962382));
#26629=CARTESIAN_POINT('Ctrl Pts',(40.8356950351829,34.4779429339551,46.8710482257117));
#26630=CARTESIAN_POINT('Ctrl Pts',(40.8423880914217,34.4771880181418,46.8618375968035));
#26631=CARTESIAN_POINT('Ctrl Pts',(40.8453994436085,34.4768513156563,46.8577278669155));
#26632=CARTESIAN_POINT('Ctrl Pts',(40.8516022775547,34.4761638615906,46.8493325414793));
#26633=CARTESIAN_POINT('Ctrl Pts',(40.8547953360493,34.4758132234346,46.8450482022128));
#26634=CARTESIAN_POINT('Ctrl Pts',(40.8630639234661,34.4749133805269,46.8340493591683));
#26635=CARTESIAN_POINT('Ctrl Pts',(40.8681657341044,34.474365978798,46.8273546195002));
#26636=CARTESIAN_POINT('Ctrl Pts',(40.8899579860983,34.4720595443514,46.7991431410104));
#26637=CARTESIAN_POINT('Ctrl Pts',(40.9070601148937,34.4703273563418,46.7779464984727));
#26638=CARTESIAN_POINT('Ctrl Pts',(40.9551641154516,34.4656406715753,46.7208434696636));
#26639=CARTESIAN_POINT('Ctrl Pts',(40.9870514483697,34.4627338248905,46.6857058268726));
#26640=CARTESIAN_POINT('Ctrl Pts',(41.1230594356058,34.4509512566825,46.5465127260641));
#26641=CARTESIAN_POINT('Ctrl Pts',(41.2376204997747,34.4423777813987,46.4533656544679));
#26642=CARTESIAN_POINT('Ctrl Pts',(41.4094368960537,34.4298669406586,46.3436362567685));
#26643=CARTESIAN_POINT('Ctrl Pts',(41.4585308642693,34.4263319487138,46.3152474816919));
#26644=CARTESIAN_POINT('Ctrl Pts',(41.5232640980222,34.4216794729383,46.2815289692503));
#26645=CARTESIAN_POINT('Ctrl Pts',(41.5378226533404,34.4206337603073,46.2741788267945));
#26646=CARTESIAN_POINT('Ctrl Pts',(41.5613320777075,34.4189452705604,46.2626813927565));
#26647=CARTESIAN_POINT('Ctrl Pts',(41.5702248176386,34.4183066128894,46.2584165343914));
#26648=CARTESIAN_POINT('Ctrl Pts',(41.5872145536802,34.4170863214498,46.2504281107125));
#26649=CARTESIAN_POINT('Ctrl Pts',(41.5953054363182,34.4165051389295,46.2466920885897));
#26650=CARTESIAN_POINT('Ctrl Pts',(41.6138614546028,34.4151719588054,46.2382792125491));
#26651=CARTESIAN_POINT('Ctrl Pts',(41.6243428875763,34.4144187129018,46.233639340402));
#26652=CARTESIAN_POINT('Ctrl Pts',(41.6569739743552,34.4120727323447,46.2195408052784));
#26653=CARTESIAN_POINT('Ctrl Pts',(41.679259138378,34.4104691756755,46.2104036377965));
#26654=CARTESIAN_POINT('Ctrl Pts',(41.7908416108944,34.4024298586531,46.1670757824099));
#26655=CARTESIAN_POINT('Ctrl Pts',(41.8824110558163,34.3957904454417,46.1391448249262));
#26656=CARTESIAN_POINT('Ctrl Pts',(42.0765388355219,34.3817022610537,46.0953716637936));
#26657=CARTESIAN_POINT('Ctrl Pts',(42.1790789029037,34.3742532981493,46.0807737329932));
#26658=CARTESIAN_POINT('Ctrl Pts',(42.3045996033678,34.3653671237185,46.0731007426699));
#26659=CARTESIAN_POINT('Ctrl Pts',(42.3269285160482,34.3637957572839,46.0721248480569));
#26660=CARTESIAN_POINT('Ctrl Pts',(42.3900835719622,34.3593858541335,46.0704634951674));
#26661=CARTESIAN_POINT('Ctrl Pts',(42.4309245140834,34.3565747163837,46.0706856937661));
#26662=CARTESIAN_POINT('Ctrl Pts',(42.4816550139389,34.3531571768992,46.0725733110281));
#26663=CARTESIAN_POINT('Ctrl Pts',(42.4915764605684,34.3524923511301,46.073019215219));
#26664=CARTESIAN_POINT('Ctrl Pts',(42.5072215255904,34.3514500513356,46.0738434659282));
#26665=CARTESIAN_POINT('Ctrl Pts',(42.5129474911528,34.3510698597161,46.074170745972));
#26666=CARTESIAN_POINT('Ctrl Pts',(42.5231629178346,34.3503939669628,46.0748003486684));
#26667=CARTESIAN_POINT('Ctrl Pts',(42.52765276865,34.3500977345464,46.0750928404023));
#26668=CARTESIAN_POINT('Ctrl Pts',(42.5384417123617,34.3493878605732,46.0758336022027));
#26669=CARTESIAN_POINT('Ctrl Pts',(42.5447396709526,34.348975074723,46.0762970955537));
#26670=CARTESIAN_POINT('Ctrl Pts',(42.5639917450296,34.3477178146806,46.0778090188657));
#26671=CARTESIAN_POINT('Ctrl Pts',(42.5769379543931,34.3468786985053,46.0789574593663));
#26672=CARTESIAN_POINT('Ctrl Pts',(42.6070985618807,34.3449365433872,46.0819404596966));
#26673=CARTESIAN_POINT('Ctrl Pts',(42.6243020729385,34.3438384305827,46.0838760896714));
#26674=CARTESIAN_POINT('Ctrl Pts',(42.6846920885585,34.3400104591402,46.0914953052686));
#26675=CARTESIAN_POINT('Ctrl Pts',(42.7277122577768,34.3373316629538,46.0984098926137));
#26676=CARTESIAN_POINT('Ctrl Pts',(42.8979650741293,34.3267943054036,46.131724777663));
#26677=CARTESIAN_POINT('Ctrl Pts',(43.0226210813281,34.319200828351,46.1694900570796));
#26678=CARTESIAN_POINT('Ctrl Pts',(43.2135143751342,34.3066600068771,46.2491000313097));
#26679=CARTESIAN_POINT('Ctrl Pts',(43.2826496305194,34.3019143930515,46.282914128506));
#26680=CARTESIAN_POINT('Ctrl Pts',(43.3648896758272,34.2959043319797,46.3294192913414));
#26681=CARTESIAN_POINT('Ctrl Pts',(43.3800822120019,34.294778212502,46.3382867830182));
#26682=CARTESIAN_POINT('Ctrl Pts',(43.4039264307158,34.2929844244083,46.3526447831909));
#26683=CARTESIAN_POINT('Ctrl Pts',(43.4126595222887,34.2923217410566,46.3579987290396));
#26684=CARTESIAN_POINT('Ctrl Pts',(43.4288636403157,34.2910812537836,46.3681113331778));
#26685=CARTESIAN_POINT('Ctrl Pts',(43.436345364754,34.2905041115909,46.3728524062623));
#26686=CARTESIAN_POINT('Ctrl Pts',(43.452937656056,34.2892142194341,46.3835275869757));
#26687=CARTESIAN_POINT('Ctrl Pts',(43.4620311817534,34.2885005176829,46.3894874945066));
#26688=CARTESIAN_POINT('Ctrl Pts',(43.4885985306213,34.2863951060906,46.4072226214974));
#26689=CARTESIAN_POINT('Ctrl Pts',(43.5059299081967,34.284995532206,46.4192073139162));
#26690=CARTESIAN_POINT('Ctrl Pts',(43.5449147628843,34.2817861684991,46.4471203621731));
#26691=CARTESIAN_POINT('Ctrl Pts',(43.5664382155553,34.2799699909406,46.463221957552));
#26692=CARTESIAN_POINT('Ctrl Pts',(43.6377105715531,34.2738034232425,46.5189004658649));
#26693=CARTESIAN_POINT('Ctrl Pts',(43.685834317894,34.2693803966815,46.5604820103819));
#26694=CARTESIAN_POINT('Ctrl Pts',(43.8164074579208,34.2566491297421,46.6850836931713));
#26695=CARTESIAN_POINT('Ctrl Pts',(43.8934820205152,34.248209175436,46.7733277084184));
#26696=CARTESIAN_POINT('Ctrl Pts',(43.9960217720389,34.2358812936198,46.9148268861911));
#26697=CARTESIAN_POINT('Ctrl Pts',(44.027833738085,34.2318585489961,46.9631562856298));
#26698=CARTESIAN_POINT('Ctrl Pts',(44.0625315462494,34.227284725118,47.0214138525988));
#26699=CARTESIAN_POINT('Ctrl Pts',(44.0675677480391,34.2266158074294,47.030020718664));
#26700=CARTESIAN_POINT('Ctrl Pts',(44.0756632346923,34.2255326904695,47.0441053224634));
#26701=CARTESIAN_POINT('Ctrl Pts',(44.0787628613103,34.2251160483018,47.0495594869302));
#26702=CARTESIAN_POINT('Ctrl Pts',(44.0842723809218,34.2243721102896,47.0593651904989));
#26703=CARTESIAN_POINT('Ctrl Pts',(44.0866920942789,34.2240442009699,47.0637110067902));
#26704=CARTESIAN_POINT('Ctrl Pts',(44.0919770294843,34.2233253979913,47.0732897546476));
#26705=CARTESIAN_POINT('Ctrl Pts',(44.0948347989453,34.2229349764343,47.0785266396701));
#26706=CARTESIAN_POINT('Ctrl Pts',(44.1030234076882,34.2218109574066,47.0936992974386));
#26707=CARTESIAN_POINT('Ctrl Pts',(44.1082915996159,34.2210811921113,47.1036688580291));
#26708=CARTESIAN_POINT('Ctrl Pts',(44.1500506195605,34.2152376746012,47.1843995987182));
#26709=CARTESIAN_POINT('Ctrl Pts',(44.1822211566163,34.2103638776719,47.2573209482297));
#26710=CARTESIAN_POINT('Ctrl Pts',(44.2261060932149,34.2027279359412,47.3762227334435));
#26711=CARTESIAN_POINT('Ctrl Pts',(44.2407929808769,34.1999194035777,47.4209983456804));
#26712=CARTESIAN_POINT('Ctrl Pts',(44.2901736097783,34.1892744357211,47.5925132829831));
#26713=CARTESIAN_POINT('Ctrl Pts',(44.3135261446433,34.181431994643,47.7221257827038));
#26714=CARTESIAN_POINT('Ctrl Pts',(44.3254635815525,34.1715483270752,47.8784343190382));
#26715=CARTESIAN_POINT('Ctrl Pts',(44.3268976819529,34.1699320239683,47.9038051682644));
#26716=CARTESIAN_POINT('Ctrl Pts',(44.3282553253072,34.1675562038338,47.9407706925516));
#26717=CARTESIAN_POINT('Ctrl Pts',(44.3285761737111,34.1668091025453,47.9523487356526));
#26718=CARTESIAN_POINT('Ctrl Pts',(44.3289601657586,34.1654786114553,47.9728814676753));
#26719=CARTESIAN_POINT('Ctrl Pts',(44.3290652575292,34.1648965533401,47.9818351016017));
#26720=CARTESIAN_POINT('Ctrl Pts',(44.3291543594468,34.1636793767602,48.000496218967));
#26721=CARTESIAN_POINT('Ctrl Pts',(44.3291274379879,34.1630439317222,48.0102034778088));
#26722=CARTESIAN_POINT('Ctrl Pts',(44.3288662832867,34.1613814427322,48.0355061024532));
#26723=CARTESIAN_POINT('Ctrl Pts',(44.3285161806463,34.1603507993887,48.0510993021979));
#26724=CARTESIAN_POINT('Ctrl Pts',(44.3260644755211,34.1556369434249,48.1219810445436));
#26725=CARTESIAN_POINT('Ctrl Pts',(44.3217741909449,34.1518861599262,48.1771627790495));
#26726=CARTESIAN_POINT('Ctrl Pts',(44.3023561440426,34.1407520101972,48.3374004372218));
#26727=CARTESIAN_POINT('Ctrl Pts',(44.2809280236383,34.133202004805,48.4414783396028));
#26728=CARTESIAN_POINT('Ctrl Pts',(44.2215524234029,34.1181391953374,48.6437914149364));
#26729=CARTESIAN_POINT('Ctrl Pts',(44.1839023151928,34.1106540765545,48.7417664032641));
#26730=CARTESIAN_POINT('Ctrl Pts',(44.1313511312328,34.1024004279503,48.8510206023347));
#26731=CARTESIAN_POINT('Ctrl Pts',(44.1240359668639,34.1012904341845,48.8657440928809));
#26732=CARTESIAN_POINT('Ctrl Pts',(44.113589698086,34.0997599475827,48.8861120163784));
#26733=CARTESIAN_POINT('Ctrl Pts',(44.1106173914101,34.0993303610339,48.8918364772232));
#26734=CARTESIAN_POINT('Ctrl Pts',(44.1054417204342,34.0985925176906,48.9016833934746));
#26735=CARTESIAN_POINT('Ctrl Pts',(44.1032520046775,34.098283426285,48.9058129020926));
#26736=CARTESIAN_POINT('Ctrl Pts',(44.0986036244992,34.0976337827002,48.914502664616));
#26737=CARTESIAN_POINT('Ctrl Pts',(44.0961415605915,34.0972934601029,48.9190610449175));
#26738=CARTESIAN_POINT('Ctrl Pts',(44.0899937586306,34.0964528030713,48.9303345249455));
#26739=CARTESIAN_POINT('Ctrl Pts',(44.0862862822213,34.0959538332971,48.9370377856661));
#26740=CARTESIAN_POINT('Ctrl Pts',(44.0722024681212,34.094087407084,48.9621475556392));
#26741=CARTESIAN_POINT('Ctrl Pts',(44.0615634464517,34.0927356551824,48.9804060462587));
#26742=CARTESIAN_POINT('Ctrl Pts',(43.9758500720868,34.0822583505986,49.1221011685673));
#26743=CARTESIAN_POINT('Ctrl Pts',(43.8874148799443,34.0738188392439,49.2369408846394));
#26744=CARTESIAN_POINT('Ctrl Pts',(43.7106633216603,34.0585919388743,49.4197740122959));
#26745=CARTESIAN_POINT('Ctrl Pts',(43.6277647783039,34.0519264285021,49.4920407261029));
#26746=CARTESIAN_POINT('Ctrl Pts',(43.525420231481,34.0438709979065,49.5669277164846));
#26747=CARTESIAN_POINT('Ctrl Pts',(43.5115301556426,34.0427815018497,49.5768112916504));
#26748=CARTESIAN_POINT('Ctrl Pts',(43.4884581062062,34.0409768927757,49.5927720144369));
#26749=CARTESIAN_POINT('Ctrl Pts',(43.4793516640338,34.0402659023675,49.5989570713383));
#26750=CARTESIAN_POINT('Ctrl Pts',(43.462815903176,34.0389768988408,49.6099824617884));
#26751=CARTESIAN_POINT('Ctrl Pts',(43.4554051507959,34.0383999398061,49.6148501895122));
#26752=CARTESIAN_POINT('Ctrl Pts',(43.4394457314425,34.0371588402641,49.6251762976705));
#26753=CARTESIAN_POINT('Ctrl Pts',(43.4308870772458,34.0364941248507,49.6306186722871));
#26754=CARTESIAN_POINT('Ctrl Pts',(43.4073641967515,34.0346692984092,49.645317457184));
#26755=CARTESIAN_POINT('Ctrl Pts',(43.3923159207897,34.0335041938853,49.6544368341254));
#26756=CARTESIAN_POINT('Ctrl Pts',(43.3040973561307,34.0266852062186,49.7062614211115));
#26757=CARTESIAN_POINT('Ctrl Pts',(43.2283122551228,34.0208657820593,49.7443094033136));
#26758=CARTESIAN_POINT('Ctrl Pts',(43.0442965321068,34.0068456735775,49.8219932047957));
#26759=CARTESIAN_POINT('Ctrl Pts',(42.934524557441,33.9985578098691,49.8571639739744));
#26760=CARTESIAN_POINT('Ctrl Pts',(42.7874137792579,33.9878622838169,49.8901667252651));
#26761=CARTESIAN_POINT('Ctrl Pts',(42.7523312915999,33.9853429822515,49.8970193922127));
#26762=CARTESIAN_POINT('Ctrl Pts',(42.6796802841621,33.9802135813446,49.9091251551202));
#26763=CARTESIAN_POINT('Ctrl Pts',(42.6421046813481,33.977608306934,49.9142533009877));
#26764=CARTESIAN_POINT('Ctrl Pts',(42.5946572175901,33.9743977082551,49.9193090201219));
#26765=CARTESIAN_POINT('Ctrl Pts',(42.5849068868708,33.9737421302353,49.9202728973442));
#26766=CARTESIAN_POINT('Ctrl Pts',(42.5695246532774,33.9727149284583,49.9216752715797));
#26767=CARTESIAN_POINT('Ctrl Pts',(42.5638976063124,33.9723406470981,49.9221633734295));
#26768=CARTESIAN_POINT('Ctrl Pts',(42.5532649692532,33.9716363255582,49.923038639793));
#26769=CARTESIAN_POINT('Ctrl Pts',(42.5482600526952,33.971306020113,49.923430975703));
#26770=CARTESIAN_POINT('Ctrl Pts',(42.5365205609455,33.9705340550481,49.9243051413645));
#26771=CARTESIAN_POINT('Ctrl Pts',(42.5297849179846,33.9700932804375,49.9247711601863));
#26772=CARTESIAN_POINT('Ctrl Pts',(42.5077366134428,33.9686570758189,49.9261803497274));
#26773=CARTESIAN_POINT('Ctrl Pts',(42.4924146729377,33.9676694564246,49.9269762534963));
#26774=CARTESIAN_POINT('Ctrl Pts',(42.407601478846,33.9622522050573,49.9303679329371));
#26775=CARTESIAN_POINT('Ctrl Pts',(42.338011332789,33.9579906248667,49.9293878959466));
#26776=CARTESIAN_POINT('Ctrl Pts',(42.2558673635155,33.9530216921476,49.9237805773473));
#26777=CARTESIAN_POINT('Ctrl Pts',(42.2431242641098,33.9522526453641,49.9227833825839));
#26778=CARTESIAN_POINT('Ctrl Pts',(42.0879226409082,33.942898762641,49.9090850916708));
#26779=CARTESIAN_POINT('Ctrl Pts',(41.9473024329846,33.934513571059,49.8807077063168));
#26780=CARTESIAN_POINT('Ctrl Pts',(41.8054451023481,33.9252876654991,49.83523361896));
#26781=CARTESIAN_POINT('Ctrl Pts',(41.7997875373724,33.9249184736924,49.8333911083169));
#26782=CARTESIAN_POINT('Ctrl Pts',(41.7941388307093,33.9245485747014,49.8315225361556));
#26783=CARTESIAN_POINT('Origin',(42.4,48.4493818343519,48.));
#26784=CARTESIAN_POINT('',(41.7941388318293,32.9600825139687,49.8315225365261));
#26785=CARTESIAN_POINT('',(41.7941386107368,33.1302767167271,49.8315224633894));
#26786=CARTESIAN_POINT('',(41.7941388317924,48.4493818343519,49.8315225365138));
#26787=CARTESIAN_POINT('',(40.4708700098857,33.595812472054,47.9998047017072));
#26788=CARTESIAN_POINT('Ctrl Pts',(41.7941388318293,32.9600825139687,49.8315225365261));
#26789=CARTESIAN_POINT('Ctrl Pts',(41.7953186904234,32.9601663481406,49.8319128295701));
#26790=CARTESIAN_POINT('Ctrl Pts',(41.7964989385408,32.96025012569,49.8323019866228));
#26791=CARTESIAN_POINT('Ctrl Pts',(41.8074347217258,32.9610255945063,49.8358960726686));
#26792=CARTESIAN_POINT('Ctrl Pts',(41.8172155782641,32.9617133763165,49.8390242869177));
#26793=CARTESIAN_POINT('Ctrl Pts',(41.8325719318299,32.9627836727442,49.8438008937735));
#26794=CARTESIAN_POINT('Ctrl Pts',(41.8381305218923,32.9631691422879,49.8455023815245));
#26795=CARTESIAN_POINT('Ctrl Pts',(41.8484292519326,32.963879613329,49.8486039852025));
#26796=CARTESIAN_POINT('Ctrl Pts',(41.853167063099,32.9642049968126,49.8500110064993));
#26797=CARTESIAN_POINT('Ctrl Pts',(41.8641032042128,32.9649527583359,49.8532131069759));
#26798=CARTESIAN_POINT('Ctrl Pts',(41.8703051771815,32.9653743871948,49.8549953081474));
#26799=CARTESIAN_POINT('Ctrl Pts',(41.8897094124839,32.9666862959985,49.8604660633937));
#26800=CARTESIAN_POINT('Ctrl Pts',(41.9029424657429,32.9675705193253,49.8640451417003));
#26801=CARTESIAN_POINT('Ctrl Pts',(41.934163780273,32.969634628917,49.872133282967));
#26802=CARTESIAN_POINT('Ctrl Pts',(41.9521813974567,32.9708086936235,49.8765247044895));
#26803=CARTESIAN_POINT('Ctrl Pts',(42.0173909704829,32.9750055970131,49.8914254355859));
#26804=CARTESIAN_POINT('Ctrl Pts',(42.0649132838724,32.9779661704232,49.9004203193478));
#26805=CARTESIAN_POINT('Ctrl Pts',(42.2701120368626,32.9905209442041,49.9313217360774));
#26806=CARTESIAN_POINT('Ctrl Pts',(42.4298198635288,32.9997730285489,49.9354550882161));
#26807=CARTESIAN_POINT('Ctrl Pts',(42.6337471679586,33.0124489288368,49.9154626299033));
#26808=CARTESIAN_POINT('Ctrl Pts',(42.6790939757978,33.0153187514563,49.9093823248533));
#26809=CARTESIAN_POINT('Ctrl Pts',(42.7390826266652,33.0192044457541,49.8991561530089));
#26810=CARTESIAN_POINT('Ctrl Pts',(42.7539552427885,33.0201751233684,49.8964405569936));
#26811=CARTESIAN_POINT('Ctrl Pts',(42.7782215459435,33.0217715719931,49.8917143726683));
#26812=CARTESIAN_POINT('Ctrl Pts',(42.7876350334175,33.0223940088909,49.8898078952314));
#26813=CARTESIAN_POINT('Ctrl Pts',(42.8058355595821,33.0236037187869,49.88598010434));
#26814=CARTESIAN_POINT('Ctrl Pts',(42.8146241848908,33.0241906990608,49.8840674712064));
#26815=CARTESIAN_POINT('Ctrl Pts',(42.8351429601558,33.0255679193441,49.8794515321867));
#26816=CARTESIAN_POINT('Ctrl Pts',(42.8468617121143,33.0263596998118,49.8766997779757));
#26817=CARTESIAN_POINT('Ctrl Pts',(42.8850194248434,33.0289553197575,49.8673620680394));
#26818=CARTESIAN_POINT('Ctrl Pts',(42.9113437233241,33.0307735580331,49.8603258861709));
#26819=CARTESIAN_POINT('Ctrl Pts',(42.9734838867121,33.0351335756086,49.8422979954103));
#26820=CARTESIAN_POINT('Ctrl Pts',(43.0091448939716,33.0376902351268,49.8308161715355));
#26821=CARTESIAN_POINT('Ctrl Pts',(43.1483926194421,33.0478895167737,49.7814637033356));
#26822=CARTESIAN_POINT('Ctrl Pts',(43.2489772839104,33.0557523263012,49.7357813889152));
#26823=CARTESIAN_POINT('Ctrl Pts',(43.4315226840048,33.0707100241287,49.6331967620152));
#26824=CARTESIAN_POINT('Ctrl Pts',(43.5140842262934,33.077776278928,49.5780338907871));
#26825=CARTESIAN_POINT('Ctrl Pts',(43.6050026831629,33.0856492456122,49.506579795194));
#26826=CARTESIAN_POINT('Ctrl Pts',(43.6178294314941,33.0867620416732,49.496230485587));
#26827=CARTESIAN_POINT('Ctrl Pts',(43.6354959037276,33.0882958077293,49.4815985053386));
#26828=CARTESIAN_POINT('Ctrl Pts',(43.6404486907668,33.0887259199215,49.4774543335341));
#26829=CARTESIAN_POINT('Ctrl Pts',(43.6489522536572,33.0894644614497,49.4702661990964));
#26830=CARTESIAN_POINT('Ctrl Pts',(43.6525129035598,33.0897737286028,49.4672340834742));
#26831=CARTESIAN_POINT('Ctrl Pts',(43.6599945078234,33.0904235385697,49.4608159483897));
#26832=CARTESIAN_POINT('Ctrl Pts',(43.6639129112251,33.090763852916,49.4574270303344));
#26833=CARTESIAN_POINT('Ctrl Pts',(43.6735864582969,33.0916041003394,49.4489922948326));
#26834=CARTESIAN_POINT('Ctrl Pts',(43.6793253923399,33.0921026726923,49.4439278661354));
#26835=CARTESIAN_POINT('Ctrl Pts',(43.7007525059521,33.0939651711712,49.4247910772649));
#26836=CARTESIAN_POINT('Ctrl Pts',(43.7162405514744,33.0953134812532,49.4104955138197));
#26837=CARTESIAN_POINT('Ctrl Pts',(43.8352730273186,33.1057215945155,49.2969592282737));
#26838=CARTESIAN_POINT('Ctrl Pts',(43.9277054657483,33.114104716562,49.186692474482));
#26839=CARTESIAN_POINT('Ctrl Pts',(44.0684071870154,33.129330097107,48.9748105176583));
#26840=CARTESIAN_POINT('Ctrl Pts',(44.1216618013576,33.1360583872588,48.8773334182646));
#26841=CARTESIAN_POINT('Ctrl Pts',(44.1731093514986,33.1441841280524,48.7602084695542));
#26842=CARTESIAN_POINT('Ctrl Pts',(44.1797636101396,33.145274588024,48.7444965760592));
#26843=CARTESIAN_POINT('Ctrl Pts',(44.1903691091641,33.1470805903501,48.7185000605846));
#26844=CARTESIAN_POINT('Ctrl Pts',(44.1944423039464,33.1477920010868,48.7082659765924));
#26845=CARTESIAN_POINT('Ctrl Pts',(44.2016367961264,33.1490816338544,48.689728992555));
#26846=CARTESIAN_POINT('Ctrl Pts',(44.2047889167095,33.1496587996724,48.6814383244502));
#26847=CARTESIAN_POINT('Ctrl Pts',(44.2114232035588,33.150900198946,48.663619946832));
#26848=CARTESIAN_POINT('Ctrl Pts',(44.2148876040374,33.1515650065902,48.6540859532607));
#26849=CARTESIAN_POINT('Ctrl Pts',(44.2241542407218,33.1533897162905,48.6279437516083));
#26850=CARTESIAN_POINT('Ctrl Pts',(44.2298046190934,33.1545546082354,48.6112831341076));
#26851=CARTESIAN_POINT('Ctrl Pts',(44.2612933771678,33.1613640205664,48.5140849419269));
#26852=CARTESIAN_POINT('Ctrl Pts',(44.2820370660458,33.1671734954347,48.4320061139792));
#26853=CARTESIAN_POINT('Ctrl Pts',(44.3179971184581,33.1811309907199,48.2364212826673));
#26854=CARTESIAN_POINT('Ctrl Pts',(44.3286331670262,33.1893639050772,48.1223901988786));
#26855=CARTESIAN_POINT('Ctrl Pts',(44.3293184578406,33.2009469725281,47.9591607664161));
#26856=CARTESIAN_POINT('Ctrl Pts',(44.3276616290696,33.2043904701352,47.9102289745482));
#26857=CARTESIAN_POINT('Ctrl Pts',(44.3221671059239,33.2096670442245,47.8339444162044));
#26858=CARTESIAN_POINT('Ctrl Pts',(44.3196008534083,33.211545062821,47.8065223693508));
#26859=CARTESIAN_POINT('Ctrl Pts',(44.3154446220935,33.2139825251905,47.7704541251514));
#26860=CARTESIAN_POINT('Ctrl Pts',(44.3143816983917,33.2145680886297,47.7617519589095));
#26861=CARTESIAN_POINT('Ctrl Pts',(44.312565460166,33.2155105616394,47.7476801410565));
#26862=CARTESIAN_POINT('Ctrl Pts',(44.3118487806834,33.2158694557297,47.742306010448));
#26863=CARTESIAN_POINT('Ctrl Pts',(44.3104126404319,33.2165640847963,47.7318727713187));
#26864=CARTESIAN_POINT('Ctrl Pts',(44.3096957252774,33.2168999481932,47.7268134245772));
#26865=CARTESIAN_POINT('Ctrl Pts',(44.3079069675801,33.2177123768437,47.714541188286));
#26866=CARTESIAN_POINT('Ctrl Pts',(44.3068143001939,33.2181877795474,47.707331315447));
#26867=CARTESIAN_POINT('Ctrl Pts',(44.3027885625952,33.2198685171367,47.6817478591484));
#26868=CARTESIAN_POINT('Ctrl Pts',(44.2996304879592,33.2210619116883,47.6634100264469));
#26869=CARTESIAN_POINT('Ctrl Pts',(44.2911018851939,33.2240057298827,47.6178396992821));
#26870=CARTESIAN_POINT('Ctrl Pts',(44.2854079298247,33.2257412685869,47.590671361096));
#26871=CARTESIAN_POINT('Ctrl Pts',(44.2577342328735,33.233305196498,47.471499711805));
#26872=CARTESIAN_POINT('Ctrl Pts',(44.2295903638975,33.2389211727187,47.3810566933012));
#26873=CARTESIAN_POINT('Ctrl Pts',(44.1492324289635,33.2520011945866,47.1770340505047));
#26874=CARTESIAN_POINT('Ctrl Pts',(44.0924104824532,33.259468182306,47.0657469356983));
#26875=CARTESIAN_POINT('Ctrl Pts',(44.011507463395,33.2689353248774,46.9392279370948));
#26876=CARTESIAN_POINT('Ctrl Pts',(43.9973361392626,33.2705583094985,46.9180060837714));
#26877=CARTESIAN_POINT('Ctrl Pts',(43.9761144432601,33.2729422803106,46.8875520389554));
#26878=CARTESIAN_POINT('Ctrl Pts',(43.9693946658616,33.2736907307929,46.878091992469));
#26879=CARTESIAN_POINT('Ctrl Pts',(43.9573358549892,33.2750229145319,46.8614360508531));
#26880=CARTESIAN_POINT('Ctrl Pts',(43.9520312193295,33.2756053063924,46.8542155869397));
#26881=CARTESIAN_POINT('Ctrl Pts',(43.9408779912796,33.2768224642894,46.8392538162203));
#26882=CARTESIAN_POINT('Ctrl Pts',(43.9350209236629,33.2774575520803,46.8315191720671));
#26883=CARTESIAN_POINT('Ctrl Pts',(43.9196164281323,33.2791175132561,46.8114922309382));
#26884=CARTESIAN_POINT('Ctrl Pts',(43.9099782965825,33.2801459639018,46.7992709192493));
#26885=CARTESIAN_POINT('Ctrl Pts',(43.8656534700592,33.2848316080301,46.7444440242126));
#26886=CARTESIAN_POINT('Ctrl Pts',(43.8293073318363,33.2885553696674,46.7032192061571));
#26887=CARTESIAN_POINT('Ctrl Pts',(43.6663871739683,33.3047738978995,46.5336111420908));
#26888=CARTESIAN_POINT('Ctrl Pts',(43.5239437738078,33.317925218574,46.4217836072068));
#26889=CARTESIAN_POINT('Ctrl Pts',(43.3319841340414,33.3334264671964,46.3104176019223));
#26890=CARTESIAN_POINT('Ctrl Pts',(43.2952246908517,33.3363007122261,46.2906561343631));
#26891=CARTESIAN_POINT('Ctrl Pts',(43.2488954268112,33.3397832980558,46.2676550381549));
#26892=CARTESIAN_POINT('Ctrl Pts',(43.2399058684298,33.3404526620956,46.2632787629403));
#26893=CARTESIAN_POINT('Ctrl Pts',(43.2256918169036,33.3415005546835,46.2564952940968));
#26894=CARTESIAN_POINT('Ctrl Pts',(43.2204900386621,33.3418818467267,46.254041313601));
#26895=CARTESIAN_POINT('Ctrl Pts',(43.2112003227081,33.3425587798449,46.2497095015205));
#26896=CARTESIAN_POINT('Ctrl Pts',(43.2071168009612,33.3428549607239,46.2478227079271));
#26897=CARTESIAN_POINT('Ctrl Pts',(43.1973022454277,33.3435635487638,46.2433294781586));
#26898=CARTESIAN_POINT('Ctrl Pts',(43.1915650142085,33.3439751101778,46.2407367951565));
#26899=CARTESIAN_POINT('Ctrl Pts',(43.1740398741993,33.3452245179412,46.2329201858732));
#26900=CARTESIAN_POINT('Ctrl Pts',(43.16221191232,33.346057104507,46.2277861814108));
#26901=CARTESIAN_POINT('Ctrl Pts',(43.1345489394738,33.3479816503892,46.2161070783065));
#26902=CARTESIAN_POINT('Ctrl Pts',(43.1186762272578,33.3490688069227,46.2096534902874));
#26903=CARTESIAN_POINT('Ctrl Pts',(43.0627827297541,33.352844497365,46.1877912571463));
#26904=CARTESIAN_POINT('Ctrl Pts',(43.0223339327698,33.3554834718571,46.1735054237523));
#26905=CARTESIAN_POINT('Ctrl Pts',(42.8587376015324,33.3659112582664,46.1217927081223));
#26906=CARTESIAN_POINT('Ctrl Pts',(42.7324604371075,33.3734346525349,46.095380584877));
#26907=CARTESIAN_POINT('Ctrl Pts',(42.5259986634939,33.386011197573,46.0733713862907));
#26908=CARTESIAN_POINT('Ctrl Pts',(42.447076264542,33.3908773958595,46.069830296513));
#26909=CARTESIAN_POINT('Ctrl Pts',(42.3504620928467,33.3970232202314,46.0714248713425));
#26910=CARTESIAN_POINT('Ctrl Pts',(42.3327646551156,33.3981565380207,46.0719607353575));
#26911=CARTESIAN_POINT('Ctrl Pts',(42.3048161975778,33.399959360026,46.073192251241));
#26912=CARTESIAN_POINT('Ctrl Pts',(42.2945587777466,33.4006237948302,46.0737263437411));
#26913=CARTESIAN_POINT('Ctrl Pts',(42.2754639641827,33.4018660707545,46.074873562242));
#26914=CARTESIAN_POINT('Ctrl Pts',(42.2666255449576,33.4024432366123,46.0754656989546));
#26915=CARTESIAN_POINT('Ctrl Pts',(42.2469768074779,33.4037312719323,46.0769180831016));
#26916=CARTESIAN_POINT('Ctrl Pts',(42.2361691005566,33.4044430779363,46.0778086503261));
#26917=CARTESIAN_POINT('Ctrl Pts',(42.2045327668332,33.4065367224479,46.0806842674953));
#26918=CARTESIAN_POINT('Ctrl Pts',(42.183728797864,33.4079262900342,46.0829170522529));
#26919=CARTESIAN_POINT('Ctrl Pts',(42.0420094291098,33.4174830506306,46.1004632009105));
#26920=CARTESIAN_POINT('Ctrl Pts',(41.9227661322724,33.4260031163009,46.1268648298564));
#26921=CARTESIAN_POINT('Ctrl Pts',(41.6759944079796,33.4444698487727,46.2066056006236));
#26922=CARTESIAN_POINT('Ctrl Pts',(41.5500470341744,33.4544091234816,46.2627513858675));
#26923=CARTESIAN_POINT('Ctrl Pts',(41.4184457887428,33.4647425956015,46.3391841860948));
#26924=CARTESIAN_POINT('Ctrl Pts',(41.40584203483,33.4657313362626,46.3466979073526));
#26925=CARTESIAN_POINT('Ctrl Pts',(41.3876202688925,33.467158095573,46.3578445398051));
#26926=CARTESIAN_POINT('Ctrl Pts',(41.3819338365237,33.4676029528798,46.3613638092927));
#26927=CARTESIAN_POINT('Ctrl Pts',(41.3721489303378,33.4683676108035,46.3674901754991));
#26928=CARTESIAN_POINT('Ctrl Pts',(41.3680418239031,33.4686883108822,46.370083292477));
#26929=CARTESIAN_POINT('Ctrl Pts',(41.3600178312467,33.4693143027092,46.3751919148607));
#26930=CARTESIAN_POINT('Ctrl Pts',(41.3561002351077,33.4696196825899,46.377706097262));
#26931=CARTESIAN_POINT('Ctrl Pts',(41.3475959602797,33.4702821384447,46.3832074178879));
#26932=CARTESIAN_POINT('Ctrl Pts',(41.3430127999091,33.4706388593795,46.3861999575491));
#26933=CARTESIAN_POINT('Ctrl Pts',(41.3242429816438,33.4720988375252,46.3985698311004));
#26934=CARTESIAN_POINT('Ctrl Pts',(41.3101673588831,33.4731914889035,46.4081153902553));
#26935=CARTESIAN_POINT('Ctrl Pts',(41.2760412776411,33.4758400445203,46.4319232608155));
#26936=CARTESIAN_POINT('Ctrl Pts',(41.256133482745,33.4773846325138,46.4463857051398));
#26937=CARTESIAN_POINT('Ctrl Pts',(41.175722009438,33.4836459561585,46.5071861728937));
#26938=CARTESIAN_POINT('Ctrl Pts',(41.1177090026685,33.4882182505514,46.556711637405));
#26939=CARTESIAN_POINT('Ctrl Pts',(40.954639900109,33.5017301648309,46.7135378804928));
#26940=CARTESIAN_POINT('Ctrl Pts',(40.8590178068249,33.5106056928517,46.8297782824284));
#26941=CARTESIAN_POINT('Ctrl Pts',(40.7645757458919,33.5216183625093,46.9765109416924));
#26942=CARTESIAN_POINT('Ctrl Pts',(40.7517148550166,33.5231772809653,46.9973543309314));
#26943=CARTESIAN_POINT('Ctrl Pts',(40.7334455663328,33.5254842412462,47.0282648380315));
#26944=CARTESIAN_POINT('Ctrl Pts',(40.7277239229533,33.5262208849937,47.0381446999251));
#26945=CARTESIAN_POINT('Ctrl Pts',(40.7176825507375,33.5275395657983,47.0558441064268));
#26946=CARTESIAN_POINT('Ctrl Pts',(40.7133287693741,33.5281203544738,47.063644027769));
#26947=CARTESIAN_POINT('Ctrl Pts',(40.7043163397013,33.5293419064085,47.0800568697133));
#26948=CARTESIAN_POINT('Ctrl Pts',(40.6996687951179,33.5299830457604,47.0886755646507));
#26949=CARTESIAN_POINT('Ctrl Pts',(40.6876115585847,33.5316764808529,47.1114485801996));
#26950=CARTESIAN_POINT('Ctrl Pts',(40.6803118643439,33.5327326256403,47.1256599690234));
#26951=CARTESIAN_POINT('Ctrl Pts',(40.6465937002536,33.537762133512,47.1933601627854));
#26952=CARTESIAN_POINT('Ctrl Pts',(40.6224917368732,33.5418147210434,47.2479597426087));
#26953=CARTESIAN_POINT('Ctrl Pts',(40.5315982645981,33.559234177284,47.4827631838862));
#26954=CARTESIAN_POINT('Ctrl Pts',(40.4894041321976,33.5733327954885,47.6712655305593));
#26955=CARTESIAN_POINT('Ctrl Pts',(40.4738280786925,33.5884426344774,47.8898403558821));
#26956=CARTESIAN_POINT('Ctrl Pts',(40.4724733640557,33.5902856073116,47.9168455301474));
#26957=CARTESIAN_POINT('Ctrl Pts',(40.4714386997071,33.5926726381177,47.9523919948821));
#26958=CARTESIAN_POINT('Ctrl Pts',(40.4712471664463,33.593241967605,47.9609138788479));
#26959=CARTESIAN_POINT('Ctrl Pts',(40.4710275626631,33.5941628232089,47.9747734582345));
#26960=CARTESIAN_POINT('Ctrl Pts',(40.4709651513888,33.5945161947454,47.9801103798958));
#26961=CARTESIAN_POINT('Ctrl Pts',(40.4708998108434,33.5950876399803,47.9887719463951));
#26962=CARTESIAN_POINT('Ctrl Pts',(40.4708833261889,33.5953064695646,47.992096331295));
#26963=CARTESIAN_POINT('Ctrl Pts',(40.4708719661489,33.5956207966647,47.9968821027511));
#26964=CARTESIAN_POINT('Ctrl Pts',(40.4708701578227,33.5957166803179,47.9983433992123));
#26965=CARTESIAN_POINT('Ctrl Pts',(40.4708700098857,33.595812472054,47.9998047017072));
#26966=CARTESIAN_POINT('Ctrl Pts',(40.4708700099162,33.5958124522899,47.9998044002066));
#26967=CARTESIAN_POINT('Ctrl Pts',(40.4708697946754,33.5959516095111,48.0019272426965));
#26968=CARTESIAN_POINT('Ctrl Pts',(40.470873083443,33.5960905727951,48.0040500985418));
#26969=CARTESIAN_POINT('Ctrl Pts',(40.4708990793297,33.5966216441967,48.0121741096659));
#26970=CARTESIAN_POINT('Ctrl Pts',(40.4709462852895,33.5970124153758,48.018175235026));
#26971=CARTESIAN_POINT('Ctrl Pts',(40.4712176332909,33.5984170233649,48.039825692079));
#26972=CARTESIAN_POINT('Ctrl Pts',(40.4716042156344,33.599422376138,48.0554728765029));
#26973=CARTESIAN_POINT('Ctrl Pts',(40.477090972764,33.6089007483902,48.2042121123139));
#26974=CARTESIAN_POINT('Ctrl Pts',(40.4957720003608,33.6167487655348,48.3364635187303));
#26975=CARTESIAN_POINT('Ctrl Pts',(40.5581542086279,33.6321720120768,48.5872065853432));
#26976=CARTESIAN_POINT('Ctrl Pts',(40.6001147342978,33.6397042286158,48.7054181231331));
#26977=CARTESIAN_POINT('Ctrl Pts',(40.6617330816396,33.6489138541125,48.8368827699757));
#26978=CARTESIAN_POINT('Ctrl Pts',(40.6705256046548,33.6501949526996,48.8549052097697));
#26979=CARTESIAN_POINT('Ctrl Pts',(40.6844225789574,33.6521724029519,48.8822983756932));
#26980=CARTESIAN_POINT('Ctrl Pts',(40.6893266662366,33.6528617368829,48.8917696165075));
#26981=CARTESIAN_POINT('Ctrl Pts',(40.6984047588779,33.6541228092482,48.9089516283029));
#26982=CARTESIAN_POINT('Ctrl Pts',(40.7025533012742,33.6546936324673,48.91667558488));
#26983=CARTESIAN_POINT('Ctrl Pts',(40.7117329755502,33.6559450662528,48.9334907445219));
#26984=CARTESIAN_POINT('Ctrl Pts',(40.7167851699566,33.6566264182588,48.9425700741526));
#26985=CARTESIAN_POINT('Ctrl Pts',(40.7309041500913,33.6585107104021,48.9674678409121));
#26986=CARTESIAN_POINT('Ctrl Pts',(40.7401220331586,33.6597190703504,48.9831988993021));
#26987=CARTESIAN_POINT('Ctrl Pts',(40.7964204122374,33.6669741954003,49.0762278874777));
#26988=CARTESIAN_POINT('Ctrl Pts',(40.8486634499625,33.6732105262355,49.1502541312575));
#26989=CARTESIAN_POINT('Ctrl Pts',(41.0080928153998,33.6909569061505,49.3454495183805));
#26990=CARTESIAN_POINT('Ctrl Pts',(41.1255898463136,33.7027390807372,49.4572293861175));
#26991=CARTESIAN_POINT('Ctrl Pts',(41.2745885857356,33.715446239185,49.5670180719793));
#26992=CARTESIAN_POINT('Ctrl Pts',(41.2937911710712,33.7170451371238,49.5806323541973));
#26993=CARTESIAN_POINT('Ctrl Pts',(41.3198330695504,33.7191571983177,49.5983884548569));
#26994=CARTESIAN_POINT('Ctrl Pts',(41.3264549837018,33.7196894766737,49.6028435212977));
#26995=CARTESIAN_POINT('Ctrl Pts',(41.3369754202764,33.7205273589121,49.6098269740103));
#26996=CARTESIAN_POINT('Ctrl Pts',(41.3408556649265,33.7208347381251,49.6123825296669));
#26997=CARTESIAN_POINT('Ctrl Pts',(41.3489363895087,33.7214713684119,49.6176627926158));
#26998=CARTESIAN_POINT('Ctrl Pts',(41.3531382849628,33.7218004518453,49.6203851931379));
#26999=CARTESIAN_POINT('Ctrl Pts',(41.3632499927675,33.7225878036512,49.6268808011352));
#27000=CARTESIAN_POINT('Ctrl Pts',(41.3691699455604,33.7230450365598,49.6306382557813));
#27001=CARTESIAN_POINT('Ctrl Pts',(41.3890007711875,33.7245647568971,49.6430739278929));
#27002=CARTESIAN_POINT('Ctrl Pts',(41.4030022151625,33.7256182730635,49.6516073483795));
#27003=CARTESIAN_POINT('Ctrl Pts',(41.496572606915,33.7325424930416,49.7070118121792));
#27004=CARTESIAN_POINT('Ctrl Pts',(41.5793201541263,33.7381168304548,49.7483018042725));
#27005=CARTESIAN_POINT('Ctrl Pts',(41.7072797968519,33.7463971195383,49.8010554698369));
#27006=CARTESIAN_POINT('Ctrl Pts',(41.750448339765,33.7491353965649,49.8170698772558));
#27007=CARTESIAN_POINT('Ctrl Pts',(41.7941388605861,33.7518842900812,49.8315225460387));
#27008=CARTESIAN_POINT('',(40.4708705770534,33.7661543955568,47.998507880119));
#27009=CARTESIAN_POINT('Ctrl Pts',(41.7941388307093,33.9245485747014,49.8315225361556));
#27010=CARTESIAN_POINT('Ctrl Pts',(41.7577101570787,33.9221630853456,49.8194720599174));
#27011=CARTESIAN_POINT('Ctrl Pts',(41.7216499126753,33.919747935102,49.8063376981226));
#27012=CARTESIAN_POINT('Ctrl Pts',(41.6721239936713,33.916342924668,49.7866063831014));
#27013=CARTESIAN_POINT('Ctrl Pts',(41.6583072392263,33.9153833094827,49.7809148426992));
#27014=CARTESIAN_POINT('Ctrl Pts',(41.6357568074188,33.9138004955479,49.7713177007099));
#27015=CARTESIAN_POINT('Ctrl Pts',(41.6269834246552,33.9131805208813,49.7675065552918));
#27016=CARTESIAN_POINT('Ctrl Pts',(41.6101671936861,33.9119839751127,49.7600524561992));
#27017=CARTESIAN_POINT('Ctrl Pts',(41.6021202830792,33.9114077496624,49.7564192163166));
#27018=CARTESIAN_POINT('Ctrl Pts',(41.5834579273818,33.9100627010319,49.7478383118413));
#27019=CARTESIAN_POINT('Ctrl Pts',(41.5728621269732,33.9092924530192,49.7428490036098));
#27020=CARTESIAN_POINT('Ctrl Pts',(41.5505418541287,33.9076556806712,49.7320895361342));
#27021=CARTESIAN_POINT('Ctrl Pts',(41.5388293080813,33.9067883757841,49.726296129811));
#27022=CARTESIAN_POINT('Ctrl Pts',(41.5073774945448,33.9044362483245,49.7103393033766));
#27023=CARTESIAN_POINT('Ctrl Pts',(41.4877538391498,33.9029437869971,49.699953629553));
#27024=CARTESIAN_POINT('Ctrl Pts',(41.4264463053549,33.898200848844,49.6661398347804));
#27025=CARTESIAN_POINT('Ctrl Pts',(41.3854542788225,33.8949099262014,49.6415008672024));
#27026=CARTESIAN_POINT('Ctrl Pts',(41.2664937755088,33.8850039734284,49.563838560819));
#27027=CARTESIAN_POINT('Ctrl Pts',(41.1914533101373,33.8782722009199,49.5065987327768));
#27028=CARTESIAN_POINT('Ctrl Pts',(41.1033473067491,33.8698656614669,49.4285602274032));
#27029=CARTESIAN_POINT('Ctrl Pts',(41.086076801076,33.8681918379977,49.4126918902211));
#27030=CARTESIAN_POINT('Ctrl Pts',(41.0101210583499,33.8607240253493,49.3403047716349));
#27031=CARTESIAN_POINT('Ctrl Pts',(40.9547550180589,33.8549855406866,49.2804102494003));
#27032=CARTESIAN_POINT('Ctrl Pts',(40.8967052463432,33.848772810804,49.2090318186555));
#27033=CARTESIAN_POINT('Ctrl Pts',(40.89013939599,33.8480670473135,49.2008222280647));
#27034=CARTESIAN_POINT('Ctrl Pts',(40.8796630087054,33.8469365137764,49.1875013239249));
#27035=CARTESIAN_POINT('Ctrl Pts',(40.8757104733839,33.8465089464433,49.1824235296359));
#27036=CARTESIAN_POINT('Ctrl Pts',(40.8687411854549,33.8457533265661,49.173377112424));
#27037=CARTESIAN_POINT('Ctrl Pts',(40.8657143283979,33.8454245750284,49.1694164720017));
#27038=CARTESIAN_POINT('Ctrl Pts',(40.859173633292,33.8447129445219,49.1607888651527));
#27039=CARTESIAN_POINT('Ctrl Pts',(40.8556656247062,33.8443304687488,49.1561176502947));
#27040=CARTESIAN_POINT('Ctrl Pts',(40.8457984003808,33.8432521375782,49.1428535420998));
#27041=CARTESIAN_POINT('Ctrl Pts',(40.8394891933334,33.8425596478857,49.1342234638338));
#27042=CARTESIAN_POINT('Ctrl Pts',(40.7979102660093,33.8379725222562,49.0763457873987));
#27043=CARTESIAN_POINT('Ctrl Pts',(40.7649013630548,33.8342161062244,49.0255075905095));
#27044=CARTESIAN_POINT('Ctrl Pts',(40.6716256790824,33.822957510933,48.8658624054197));
#27045=CARTESIAN_POINT('Ctrl Pts',(40.6194341382613,33.815681771896,48.7527172064729));
#27046=CARTESIAN_POINT('Ctrl Pts',(40.5583554019501,33.8044841936345,48.5776035394629));
#27047=CARTESIAN_POINT('Ctrl Pts',(40.5409769658268,33.8007472056475,48.5189538589396));
#27048=CARTESIAN_POINT('Ctrl Pts',(40.5183146786319,33.7948036316806,48.4265659547894));
#27049=CARTESIAN_POINT('Ctrl Pts',(40.5110906628393,33.7926555272956,48.3933439412882));
#27050=CARTESIAN_POINT('Ctrl Pts',(40.502227458627,33.7896146649027,48.3466763360272));
#27051=CARTESIAN_POINT('Ctrl Pts',(40.4998460770096,33.7887454647032,48.3333768956079));
#27052=CARTESIAN_POINT('Ctrl Pts',(40.4962212876742,33.7873326429179,48.3118311985335));
#27053=CARTESIAN_POINT('Ctrl Pts',(40.4948912812381,33.786791785299,48.3035998154362));
#27054=CARTESIAN_POINT('Ctrl Pts',(40.4923221345089,33.7856998811604,48.2870174053014));
#27055=CARTESIAN_POINT('Ctrl Pts',(40.4910843684486,33.7851488039661,48.2786663546546));
#27056=CARTESIAN_POINT('Ctrl Pts',(40.4886642909931,33.7840177823943,48.2615651444948));
#27057=CARTESIAN_POINT('Ctrl Pts',(40.4874871610685,33.783437687554,48.2528144652574));
#27058=CARTESIAN_POINT('Ctrl Pts',(40.4848931123223,33.7820860766254,48.2324746812769));
#27059=CARTESIAN_POINT('Ctrl Pts',(40.4835212601344,33.7813131583152,48.2208802799362));
#27060=CARTESIAN_POINT('Ctrl Pts',(40.4794041147951,33.7787897749827,48.1831516443121));
#27061=CARTESIAN_POINT('Ctrl Pts',(40.4770876389665,33.7770260544021,48.1569745700284));
#27062=CARTESIAN_POINT('Ctrl Pts',(40.4723157732544,33.7722574473275,48.0867358104789));
#27063=CARTESIAN_POINT('Ctrl Pts',(40.4708364529626,33.7692244710891,48.0426261768473));
#27064=CARTESIAN_POINT('Ctrl Pts',(40.4708705770534,33.7661543955568,47.998507880119));
#27065=CARTESIAN_POINT('Ctrl Pts',(40.470870575219,33.7661545607265,47.9985102536787));
#27066=CARTESIAN_POINT('Ctrl Pts',(40.4709446203108,33.7594822623403,47.9026264355607));
#27067=CARTESIAN_POINT('Ctrl Pts',(40.4781671589483,33.7526397519906,47.8068858209778));
#27068=CARTESIAN_POINT('Ctrl Pts',(40.5036561422422,33.7404401451449,47.6380137778734));
#27069=CARTESIAN_POINT('Ctrl Pts',(40.5191417216402,33.7350982340165,47.5646524109731));
#27070=CARTESIAN_POINT('Ctrl Pts',(40.5452646994695,33.7281964461131,47.4688759573871));
#27071=CARTESIAN_POINT('Ctrl Pts',(40.5521184949608,33.7265180951439,47.4455003667425));
#27072=CARTESIAN_POINT('Ctrl Pts',(40.5644675957776,33.7237106187548,47.4061581389536));
#27073=CARTESIAN_POINT('Ctrl Pts',(40.5697330027675,33.7225712662827,47.3901228569832));
#27074=CARTESIAN_POINT('Ctrl Pts',(40.577483951902,33.7209745010812,47.3675231131903));
#27075=CARTESIAN_POINT('Ctrl Pts',(40.5797957365942,33.7205076893603,47.3609004762885));
#27076=CARTESIAN_POINT('Ctrl Pts',(40.5838372432206,33.7197077696069,47.3495224832631));
#27077=CARTESIAN_POINT('Ctrl Pts',(40.5855496322938,33.7193736585046,47.3447610935809));
#27078=CARTESIAN_POINT('Ctrl Pts',(40.5891706845084,33.7186771656562,47.3348156176651));
#27079=CARTESIAN_POINT('Ctrl Pts',(40.5910828977674,33.7183149963777,47.3296329427092));
#27080=CARTESIAN_POINT('Ctrl Pts',(40.5962513020657,33.7173508128748,47.3158081571448));
#27081=CARTESIAN_POINT('Ctrl Pts',(40.5995473805147,33.7167511194016,47.3071809641446));
#27082=CARTESIAN_POINT('Ctrl Pts',(40.6144372449003,33.7141067638727,47.2690320626725));
#27083=CARTESIAN_POINT('Ctrl Pts',(40.6266967945813,33.712098505794,47.2397733921818));
#27084=CARTESIAN_POINT('Ctrl Pts',(40.6895788338157,33.702506035351,47.0995086561721));
#27085=CARTESIAN_POINT('Ctrl Pts',(40.749936364981,33.6953276008729,46.9931627861734));
#27086=CARTESIAN_POINT('Ctrl Pts',(40.8656691395636,33.6832711018941,46.8279401574051));
#27087=CARTESIAN_POINT('Ctrl Pts',(40.9153965532164,33.6784734587323,46.7655581759631));
#27088=CARTESIAN_POINT('Ctrl Pts',(40.9896583151381,33.6716224583645,46.6833971171577));
#27089=CARTESIAN_POINT('Ctrl Pts',(41.011032699567,33.6696830104915,46.6608672579265));
#27090=CARTESIAN_POINT('Ctrl Pts',(41.0494385482491,33.6662443569971,46.6222942784321));
#27091=CARTESIAN_POINT('Ctrl Pts',(41.0662357017407,33.6647550303344,46.6060265385081));
#27092=CARTESIAN_POINT('Ctrl Pts',(41.091531568693,33.6625307983258,46.5824037815255));
#27093=CARTESIAN_POINT('Ctrl Pts',(41.0998059447579,33.6618061048589,46.5748108601734));
#27094=CARTESIAN_POINT('Ctrl Pts',(41.1082996038705,33.6610649354082,46.56715224594));
#27095=CARTESIAN_POINT('Ctrl Pts',(41.1084532278421,33.6610515308523,46.5670137701275));
#27096=CARTESIAN_POINT('Ctrl Pts',(41.1086756462365,33.661032124901,46.5668133482176));
#27097=CARTESIAN_POINT('Ctrl Pts',(41.1087444228499,33.6610261243387,46.5667513823664));
#27098=CARTESIAN_POINT('Ctrl Pts',(41.1088890192633,33.6610135090956,46.5666211238009));
#27099=CARTESIAN_POINT('Ctrl Pts',(41.1089648402508,33.6610068943501,46.5665528319453));
#27100=CARTESIAN_POINT('Ctrl Pts',(41.1091244099496,33.6609929736928,46.5664091306749));
#27101=CARTESIAN_POINT('Ctrl Pts',(41.1092081596368,33.6609856677441,46.566333722775));
#27102=CARTESIAN_POINT('Ctrl Pts',(41.1093846143402,33.6609702751865,46.5661748716266));
#27103=CARTESIAN_POINT('Ctrl Pts',(41.1094773209908,33.6609621884952,46.5660914298952));
#27104=CARTESIAN_POINT('Ctrl Pts',(41.1096728932206,33.660945129651,46.5659154370968));
#27105=CARTESIAN_POINT('Ctrl Pts',(41.109775760615,33.6609361574151,46.5658228881514));
#27106=CARTESIAN_POINT('Ctrl Pts',(41.1099930718877,33.660917204076,46.5656274172961));
#27107=CARTESIAN_POINT('Ctrl Pts',(41.1101075181197,33.6609072228627,46.5655244980206));
#27108=CARTESIAN_POINT('Ctrl Pts',(41.116723669867,33.6603302363395,46.5595761531432));
#27109=CARTESIAN_POINT('Ctrl Pts',(41.1232649344167,33.6597613834462,46.5537750637779));
#27110=CARTESIAN_POINT('Ctrl Pts',(41.1374159057535,33.6585340503031,46.5413961696784));
#27111=CARTESIAN_POINT('Ctrl Pts',(41.14503804824,33.657874983064,46.5348330395502));
#27112=CARTESIAN_POINT('Ctrl Pts',(41.1658381770873,33.6560816395355,46.5172042440036));
#27113=CARTESIAN_POINT('Ctrl Pts',(41.1791132017874,33.6549426547532,46.5062550243418));
#27114=CARTESIAN_POINT('Ctrl Pts',(41.2446734677681,33.6493429744936,46.4536388030264));
#27115=CARTESIAN_POINT('Ctrl Pts',(41.2989484878609,33.644782300511,46.4145359965361));
#27116=CARTESIAN_POINT('Ctrl Pts',(41.4738054157305,33.6303150570237,46.3018733718941));
#27117=CARTESIAN_POINT('Ctrl Pts',(41.6005019610822,33.6201107085544,46.2386748087182));
#27118=CARTESIAN_POINT('Ctrl Pts',(41.7932950843798,33.6055762069179,46.1676273526643));
#27119=CARTESIAN_POINT('Ctrl Pts',(41.8547346921109,33.60108764539,46.1484147501434));
#27120=CARTESIAN_POINT('Ctrl Pts',(41.9275132984825,33.5960192286536,46.1295946377345));
#27121=CARTESIAN_POINT('Ctrl Pts',(41.938023881319,33.5952932350344,46.1269709074746));
#27122=CARTESIAN_POINT('Ctrl Pts',(41.9542653892263,33.5941811771665,46.1230616164485));
#27123=CARTESIAN_POINT('Ctrl Pts',(41.9599808148327,33.5937917021623,46.1217135048521));
#27124=CARTESIAN_POINT('Ctrl Pts',(41.9705560105203,33.5930746091724,46.1192700268231));
#27125=CARTESIAN_POINT('Ctrl Pts',(41.9754138581071,33.5927465964314,46.1181673875824));
#27126=CARTESIAN_POINT('Ctrl Pts',(41.9865154189666,33.5920001256666,46.1156927210258));
#27127=CARTESIAN_POINT('Ctrl Pts',(41.9927617207576,33.5915823662802,46.1143329012906));
#27128=CARTESIAN_POINT('Ctrl Pts',(42.0091580018697,33.5904913632957,46.1108487037066));
#27129=CARTESIAN_POINT('Ctrl Pts',(42.0193187109911,33.5898208845378,46.108775038394));
#27130=CARTESIAN_POINT('Ctrl Pts',(42.1007475426901,33.5844888223533,46.0928393477876));
#27131=CARTESIAN_POINT('Ctrl Pts',(42.1727385082922,33.58002594182,46.0829270902785));
#27132=CARTESIAN_POINT('Ctrl Pts',(42.3582149927332,33.5687805380094,46.0679883744019));
#27133=CARTESIAN_POINT('Ctrl Pts',(42.4718886470002,33.5621168448057,46.0688739277242));
#27134=CARTESIAN_POINT('Ctrl Pts',(42.6688548502872,33.5501567681826,46.0878322112025));
#27135=CARTESIAN_POINT('Ctrl Pts',(42.7522510928083,33.5449632010191,46.1014255062303));
#27136=CARTESIAN_POINT('Ctrl Pts',(42.851611688321,33.5384739952655,46.1243938266848));
#27137=CARTESIAN_POINT('Ctrl Pts',(42.8686851968918,33.5373481942929,46.1285872214407));
#27138=CARTESIAN_POINT('Ctrl Pts',(42.8955112093577,33.5355612644794,46.1355660368666));
#27139=CARTESIAN_POINT('Ctrl Pts',(42.9053034145217,33.5349051659131,46.1381960859865));
#27140=CARTESIAN_POINT('Ctrl Pts',(42.9236191949162,33.5336705837348,46.1432705862479));
#27141=CARTESIAN_POINT('Ctrl Pts',(42.9321475646179,33.5330927059163,46.1456968580571));
#27142=CARTESIAN_POINT('Ctrl Pts',(42.9512302314874,33.5317927472586,46.1512682535257));
#27143=CARTESIAN_POINT('Ctrl Pts',(42.961774861972,33.5310696441081,46.1544451147646));
#27144=CARTESIAN_POINT('Ctrl Pts',(42.9885856671546,33.529218608992,46.1627736697961));
#27145=CARTESIAN_POINT('Ctrl Pts',(43.0048114704977,33.5280865887297,46.1680511117441));
#27146=CARTESIAN_POINT('Ctrl Pts',(43.1262279158077,33.5195247487279,46.2093306625557));
#27147=CARTESIAN_POINT('Ctrl Pts',(43.2281819595729,33.5118003424118,46.2541447299368));
#27148=CARTESIAN_POINT('Ctrl Pts',(43.451303072693,33.4937554192538,46.3761770115563));
#27149=CARTESIAN_POINT('Ctrl Pts',(43.5688746615877,33.4833705861484,46.4586453551129));
#27150=CARTESIAN_POINT('Ctrl Pts',(43.6920322224882,33.4721274355821,46.5672967103158));
#27151=CARTESIAN_POINT('Ctrl Pts',(43.7075947682726,33.470700009798,46.5814859915852));
#27152=CARTESIAN_POINT('Ctrl Pts',(43.7284904768798,33.4687778459379,46.6011740165443));
#27153=CARTESIAN_POINT('Ctrl Pts',(43.7340272009866,33.46826798504,46.6064532619715));
#27154=CARTESIAN_POINT('Ctrl Pts',(43.7432591085678,33.4674171492287,46.615361295422));
#27155=CARTESIAN_POINT('Ctrl Pts',(43.7469713050219,33.46707483289,46.6189722376017));
#27156=CARTESIAN_POINT('Ctrl Pts',(43.7540076110993,33.466425700679,46.6258719818359));
#27157=CARTESIAN_POINT('Ctrl Pts',(43.7573343628105,33.4661186650114,46.6291579777673));
#27158=CARTESIAN_POINT('Ctrl Pts',(43.7652266711699,33.4653898581532,46.6370104955061));
#27159=CARTESIAN_POINT('Ctrl Pts',(43.769781348461,33.464968937699,46.6415879441911));
#27160=CARTESIAN_POINT('Ctrl Pts',(43.785879479902,33.4634796861801,46.6579298558259));
#27161=CARTESIAN_POINT('Ctrl Pts',(43.7972954420798,33.462420741738,46.6698196754207));
#27162=CARTESIAN_POINT('Ctrl Pts',(43.8790807914162,33.4548002532459,46.7572147631744));
#27163=CARTESIAN_POINT('Ctrl Pts',(43.9434516116396,33.4486105989604,46.8381231547602));
#27164=CARTESIAN_POINT('Ctrl Pts',(44.0608511484558,33.4360462363811,47.0127770823984));
#27165=CARTESIAN_POINT('Ctrl Pts',(44.1131334975787,33.4296908144134,47.106575372752));
#27166=CARTESIAN_POINT('Ctrl Pts',(44.1803082964872,33.4196834491732,47.2549216646809));
#27167=CARTESIAN_POINT('Ctrl Pts',(44.2010575065381,33.4162085561959,47.3065807017735));
#27168=CARTESIAN_POINT('Ctrl Pts',(44.2247354371408,33.4116613712007,47.3737993000641));
#27169=CARTESIAN_POINT('Ctrl Pts',(44.229747702195,33.4106586690996,47.3885999221372));
#27170=CARTESIAN_POINT('Ctrl Pts',(44.2375832320637,33.4090230178869,47.4126970310406));
#27171=CARTESIAN_POINT('Ctrl Pts',(44.2405171057321,33.4083937303086,47.4219570172841));
#27172=CARTESIAN_POINT('Ctrl Pts',(44.2460202418425,33.4071800353667,47.4397929258847));
#27173=CARTESIAN_POINT('Ctrl Pts',(44.248599991518,33.4065959905332,47.4483653691301));
#27174=CARTESIAN_POINT('Ctrl Pts',(44.2543765016882,33.4052526736635,47.4680562231594));
#27175=CARTESIAN_POINT('Ctrl Pts',(44.2575330748931,33.4044921115334,47.4791859665201));
#27176=CARTESIAN_POINT('Ctrl Pts',(44.2672821678355,33.4020555180509,47.5147766990358));
#27177=CARTESIAN_POINT('Ctrl Pts',(44.273492809607,33.4003672379884,47.5393385904564));
#27178=CARTESIAN_POINT('Ctrl Pts',(44.3095123852677,33.3896487011657,47.6945929645876));
#27179=CARTESIAN_POINT('Ctrl Pts',(44.3261094619838,33.3801956015534,47.8279501394247));
#27180=CARTESIAN_POINT('Ctrl Pts',(44.33022959864,33.3652891717794,48.0366626884876));
#27181=CARTESIAN_POINT('Ctrl Pts',(44.3273597465556,33.3599362648445,48.1114253059605));
#27182=CARTESIAN_POINT('Ctrl Pts',(44.3168491310644,33.3522704902663,48.2200273810585));
#27183=CARTESIAN_POINT('Ctrl Pts',(44.3126270148121,33.3498800194191,48.254127572478));
#27184=CARTESIAN_POINT('Ctrl Pts',(44.3042495367701,33.3460366210024,48.3095946972419));
#27185=CARTESIAN_POINT('Ctrl Pts',(44.300639585825,33.3445620486916,48.3310354029378));
#27186=CARTESIAN_POINT('Ctrl Pts',(44.2952531306863,33.3425874328491,48.3600251308901));
#27187=CARTESIAN_POINT('Ctrl Pts',(44.2937926297597,33.3420712116308,48.367630255532));
#27188=CARTESIAN_POINT('Ctrl Pts',(44.2912753032388,33.3412127382144,48.3803252600361));
#27189=CARTESIAN_POINT('Ctrl Pts',(44.2902436423086,33.3408690935911,48.3854199667271));
#27190=CARTESIAN_POINT('Ctrl Pts',(44.2882482533916,33.3402197128571,48.3950731545546));
#27191=CARTESIAN_POINT('Ctrl Pts',(44.2872885862118,33.339913741829,48.3996324028355));
#27192=CARTESIAN_POINT('Ctrl Pts',(44.2849734562484,33.3391902976939,48.4104369202839));
#27193=CARTESIAN_POINT('Ctrl Pts',(44.283603449281,33.3387736460443,48.4166790671348));
#27194=CARTESIAN_POINT('Ctrl Pts',(44.2786764828325,33.3373142425497,48.4386067863631));
#27195=CARTESIAN_POINT('Ctrl Pts',(44.2749542924982,33.3362803948793,48.4542550846753));
#27196=CARTESIAN_POINT('Ctrl Pts',(44.2425093830252,33.32779383224,48.5834556618117));
#27197=CARTESIAN_POINT('Ctrl Pts',(44.2036913347476,33.3208251464297,48.6942380720401));
#27198=CARTESIAN_POINT('Ctrl Pts',(44.1146336972522,33.3080297382683,48.889412988651));
#27199=CARTESIAN_POINT('Ctrl Pts',(44.0675642757087,33.302227158385,48.9748085971785));
#27200=CARTESIAN_POINT('Ctrl Pts',(43.9950999146802,33.2940772709602,49.0855516694621));
#27201=CARTESIAN_POINT('Ctrl Pts',(43.9751551546788,33.2919008363048,49.1142944795289));
#27202=CARTESIAN_POINT('Ctrl Pts',(43.93912773796,33.2880671710243,49.1633129199431));
#27203=CARTESIAN_POINT('Ctrl Pts',(43.9233978411,33.2864229762585,49.1838370073156));
#27204=CARTESIAN_POINT('Ctrl Pts',(43.8999024351224,33.2840055293503,49.2132494541325));
#27205=CARTESIAN_POINT('Ctrl Pts',(43.8924599475655,33.2832451317841,49.2223930822742));
#27206=CARTESIAN_POINT('Ctrl Pts',(43.8792175031877,33.281901155543,49.2383611489627));
#27207=CARTESIAN_POINT('Ctrl Pts',(43.8734529068069,33.2813190263296,49.2452145533517));
#27208=CARTESIAN_POINT('Ctrl Pts',(43.8613429344916,33.2801020060131,49.2594100009605));
#27209=CARTESIAN_POINT('Ctrl Pts',(43.8549894740085,33.279466790463,49.2667447838414));
#27210=CARTESIAN_POINT('Ctrl Pts',(43.8382909709405,33.2778055825467,49.285731080911));
#27211=CARTESIAN_POINT('Ctrl Pts',(43.8278597979883,33.2767760011228,49.297305554779));
#27212=CARTESIAN_POINT('Ctrl Pts',(43.7835214135272,33.2724323367416,49.3453210192894));
#27213=CARTESIAN_POINT('Ctrl Pts',(43.7483532368508,33.2690647230517,49.3805661620126));
#27214=CARTESIAN_POINT('Ctrl Pts',(43.6877403430423,33.2633811774886,49.4367845943652));
#27215=CARTESIAN_POINT('Ctrl Pts',(43.6630490104862,33.2610966942403,49.4585376821571));
#27216=CARTESIAN_POINT('Ctrl Pts',(43.5388102197891,33.2497579320187,49.5624709153666));
#27217=CARTESIAN_POINT('Ctrl Pts',(43.4317452958379,33.240434672214,49.6351457647133));
#27218=CARTESIAN_POINT('Ctrl Pts',(43.2622224315419,33.2268029387459,49.7268966899198));
#27219=CARTESIAN_POINT('Ctrl Pts',(43.204731412823,33.2223598924433,49.7544254983683));
#27220=CARTESIAN_POINT('Ctrl Pts',(43.1360089690752,33.2173357402022,49.7832414879358));
#27221=CARTESIAN_POINT('Ctrl Pts',(43.1260049059889,33.2166113051601,49.7873377679189));
#27222=CARTESIAN_POINT('Ctrl Pts',(43.1105184392174,33.2155011185706,49.7935273985152));
#27223=CARTESIAN_POINT('Ctrl Pts',(43.1050602236732,33.2151119737899,49.7956801120914));
#27224=CARTESIAN_POINT('Ctrl Pts',(43.094949353236,33.2143951819622,49.7996146180047));
#27225=CARTESIAN_POINT('Ctrl Pts',(43.0902996278164,33.2140671428868,49.8014032867925));
#27226=CARTESIAN_POINT('Ctrl Pts',(43.0796616313177,33.2133202212445,49.8054483020394));
#27227=CARTESIAN_POINT('Ctrl Pts',(43.0736690241318,33.212902040751,49.8076928813392));
#27228=CARTESIAN_POINT('Ctrl Pts',(43.0579155674641,33.211809190619,49.8135042472926));
#27229=CARTESIAN_POINT('Ctrl Pts',(43.0481367195893,33.2111373010809,49.8170221113304));
#27230=CARTESIAN_POINT('Ctrl Pts',(42.9707719748347,33.2058691534773,49.8441494240722));
#27231=CARTESIAN_POINT('Ctrl Pts',(42.9019396003338,33.201465876567,49.8640619171313));
#27232=CARTESIAN_POINT('Ctrl Pts',(42.7208009233592,33.1902279944947,49.905697629329));
#27233=CARTESIAN_POINT('Ctrl Pts',(42.6073957504876,33.1835191647837,49.9213497216503));
#27234=CARTESIAN_POINT('Ctrl Pts',(42.4087919508234,33.1715019817115,49.9309631090335));
#27235=CARTESIAN_POINT('Ctrl Pts',(42.3241462218332,33.1662989232456,49.929491999622));
#27236=CARTESIAN_POINT('Ctrl Pts',(42.2223489390126,33.159799033062,49.9210132772347));
#27237=CARTESIAN_POINT('Ctrl Pts',(42.2048424434905,33.1586727381356,49.9193137851873));
#27238=CARTESIAN_POINT('Ctrl Pts',(42.1772829802555,33.1568852053856,49.9162574262944));
#27239=CARTESIAN_POINT('Ctrl Pts',(42.1672130080796,33.156229003779,49.9150602091267));
#27240=CARTESIAN_POINT('Ctrl Pts',(42.1483570994117,33.1549943376775,49.912667514997));
#27241=CARTESIAN_POINT('Ctrl Pts',(42.1395690242208,33.15441647991,49.9114907467126));
#27242=CARTESIAN_POINT('Ctrl Pts',(42.1198869960356,33.1531167116274,49.9087169740905));
#27243=CARTESIAN_POINT('Ctrl Pts',(42.1089980475039,33.1523937800412,49.9070872128073));
#27244=CARTESIAN_POINT('Ctrl Pts',(42.0812799696924,33.1505434684253,49.902695702609));
#27245=CARTESIAN_POINT('Ctrl Pts',(42.0644727116037,33.1494120054724,49.8998038849541));
#27246=CARTESIAN_POINT('Ctrl Pts',(41.9617558750778,33.1424370821867,49.8807251295363));
#27247=CARTESIAN_POINT('Ctrl Pts',(41.8770401022699,33.1364193757565,49.8589459942695));
#27248=CARTESIAN_POINT('Ctrl Pts',(41.7941386107368,33.1302767167271,49.8315224633894));
#27249=CARTESIAN_POINT('Origin',(42.4,48.4493818343519,48.));
#27250=CARTESIAN_POINT('',(41.7941388784248,32.1635431008229,49.8315225519397));
#27251=CARTESIAN_POINT('',(41.794138831786,32.3337813919524,49.8315225365117));
#27252=CARTESIAN_POINT('',(41.7941388317924,48.4493818343519,49.8315225365138));
#27253=CARTESIAN_POINT('Ctrl Pts',(41.7941388784247,32.1635431008229,49.8315225519397));
#27254=CARTESIAN_POINT('Ctrl Pts',(41.9072674988879,32.1719168560421,49.8689450957153));
#27255=CARTESIAN_POINT('Ctrl Pts',(42.0236406174219,32.1805157140677,49.8958120447913));
#27256=CARTESIAN_POINT('Ctrl Pts',(42.20716904871,32.1936272155024,49.9206027649335));
#27257=CARTESIAN_POINT('Ctrl Pts',(42.2729945361483,32.1982372720411,49.9260764020955));
#27258=CARTESIAN_POINT('Ctrl Pts',(42.3498899796364,32.2034257326079,49.9285099792403));
#27259=CARTESIAN_POINT('Ctrl Pts',(42.3608053169991,32.2041575925035,49.9287626978604));
#27260=CARTESIAN_POINT('Ctrl Pts',(42.3776231368258,32.2052774610604,49.9290092425017));
#27261=CARTESIAN_POINT('Ctrl Pts',(42.3835242178087,32.2056689348062,49.9290686697401));
#27262=CARTESIAN_POINT('Ctrl Pts',(42.3944001447044,32.2063876162718,49.929128286455));
#27263=CARTESIAN_POINT('Ctrl Pts',(42.3993747525962,32.206715240161,49.9291363130827));
#27264=CARTESIAN_POINT('Ctrl Pts',(42.4106970710997,32.2074584357207,49.9291107850804));
#27265=CARTESIAN_POINT('Ctrl Pts',(42.4170446197297,32.2078733289184,49.9290651446303));
#27266=CARTESIAN_POINT('Ctrl Pts',(42.4336590813188,32.2089549631484,49.9288636688096));
#27267=CARTESIAN_POINT('Ctrl Pts',(42.4439253377381,32.2096189857862,49.928657191538));
#27268=CARTESIAN_POINT('Ctrl Pts',(42.5210456161652,32.2145778952333,49.9264900091652));
#27269=CARTESIAN_POINT('Ctrl Pts',(42.5877666014461,32.2187036080615,49.9211354884859));
#27270=CARTESIAN_POINT('Ctrl Pts',(42.771526612617,32.2299373844789,49.896720162025));
#27271=CARTESIAN_POINT('Ctrl Pts',(42.8872859530086,32.2368808631999,49.8703297503966));
#27272=CARTESIAN_POINT('Ctrl Pts',(43.0757791759041,32.2488584447555,49.8086569179086));
#27273=CARTESIAN_POINT('Ctrl Pts',(43.1500402324937,32.2537610988222,49.7791443966971));
#27274=CARTESIAN_POINT('Ctrl Pts',(43.2409655065399,32.2601303653587,49.7363028001725));
#27275=CARTESIAN_POINT('Ctrl Pts',(43.2595332099424,32.2614508257434,49.7271864418577));
#27276=CARTESIAN_POINT('Ctrl Pts',(43.2875279337964,32.263473811028,49.7128784018791));
#27277=CARTESIAN_POINT('Ctrl Pts',(43.2970644118627,32.2641687024878,49.7079033011462));
#27278=CARTESIAN_POINT('Ctrl Pts',(43.3135784728637,32.2653823190737,49.6991115842605));
#27279=CARTESIAN_POINT('Ctrl Pts',(43.3205750505281,32.2658997455274,49.6953310517387));
#27280=CARTESIAN_POINT('Ctrl Pts',(43.336247648067,32.2670662343823,49.6867368913846));
#27281=CARTESIAN_POINT('Ctrl Pts',(43.3449102563945,32.267716146239,49.6818994025632));
#27282=CARTESIAN_POINT('Ctrl Pts',(43.3680932681234,32.2694696130528,49.6687176049584));
#27283=CARTESIAN_POINT('Ctrl Pts',(43.382542691734,32.270577591519,49.6602508392984));
#27284=CARTESIAN_POINT('Ctrl Pts',(43.4501924220265,32.2758380482185,49.6194184627264));
#27285=CARTESIAN_POINT('Ctrl Pts',(43.5019101204656,32.2800772407709,49.5846806877562));
#27286=CARTESIAN_POINT('Ctrl Pts',(43.680809607114,32.2955474235228,49.4515206917045));
#27287=CARTESIAN_POINT('Ctrl Pts',(43.7972575939745,32.3072347153004,49.3397933837717));
#27288=CARTESIAN_POINT('Ctrl Pts',(43.920588247354,32.321009022085,49.1876810011976));
#27289=CARTESIAN_POINT('Ctrl Pts',(43.9419488358847,32.3234542644864,49.1598141515082));
#27290=CARTESIAN_POINT('Ctrl Pts',(43.9754730232617,32.3273732629032,49.1135141428578));
#27291=CARTESIAN_POINT('Ctrl Pts',(43.988101208106,32.3288699291328,49.0954285232397));
#27292=CARTESIAN_POINT('Ctrl Pts',(44.0047465253204,32.3308667354981,49.0706966286458));
#27293=CARTESIAN_POINT('Ctrl Pts',(44.0090372287352,32.3313837093015,49.064237700323));
#27294=CARTESIAN_POINT('Ctrl Pts',(44.0161279930828,32.332241610232,49.0534228385389));
#27295=CARTESIAN_POINT('Ctrl Pts',(44.0189496384977,32.3325839551696,49.0490812348157));
#27296=CARTESIAN_POINT('Ctrl Pts',(44.0242708119744,32.3332313197712,49.040821063987));
#27297=CARTESIAN_POINT('Ctrl Pts',(44.0267736899045,32.333536573062,49.0369047790675));
#27298=CARTESIAN_POINT('Ctrl Pts',(44.0326593460827,32.3342562910065,49.0276216528783));
#27299=CARTESIAN_POINT('Ctrl Pts',(44.0360298785954,32.3346699547353,49.0222470547464));
#27300=CARTESIAN_POINT('Ctrl Pts',(44.0477149962201,32.3361097203392,49.0034083205503));
#27301=CARTESIAN_POINT('Ctrl Pts',(44.0558906448,32.3371272244244,48.9898581604743));
#27302=CARTESIAN_POINT('Ctrl Pts',(44.126084419954,32.3459680817708,48.870216343279));
#27303=CARTESIAN_POINT('Ctrl Pts',(44.1780091022977,32.3532560005212,48.758509138183));
#27304=CARTESIAN_POINT('Ctrl Pts',(44.2635559725403,32.3685730568418,48.5163611983905));
#27305=CARTESIAN_POINT('Ctrl Pts',(44.2948870187581,32.3765832389472,48.3858327060392));
#27306=CARTESIAN_POINT('Ctrl Pts',(44.3152879526994,32.3864279861685,48.2316932707008));
#27307=CARTESIAN_POINT('Ctrl Pts',(44.3177634957114,32.3878070290787,48.2102209026224));
#27308=CARTESIAN_POINT('Ctrl Pts',(44.3209533750396,32.3899047584419,48.1777684170449));
#27309=CARTESIAN_POINT('Ctrl Pts',(44.3219354649262,32.3906150374623,48.1668158852367));
#27310=CARTESIAN_POINT('Ctrl Pts',(44.3235349546635,32.3918991621102,48.1470826562151));
#27311=CARTESIAN_POINT('Ctrl Pts',(44.3241860021117,32.3924719340927,48.1383049331604));
#27312=CARTESIAN_POINT('Ctrl Pts',(44.325459242284,32.3937100982808,48.1193839702669));
#27313=CARTESIAN_POINT('Ctrl Pts',(44.3260613979636,32.3943761019677,48.1092396934337));
#27314=CARTESIAN_POINT('Ctrl Pts',(44.3274654402131,32.3961743825997,48.0819415896934));
#27315=CARTESIAN_POINT('Ctrl Pts',(44.3281184584628,32.397311277062,48.0647813627441));
#27316=CARTESIAN_POINT('Ctrl Pts',(44.3302693579628,32.4031172147902,47.9776641487525));
#27317=CARTESIAN_POINT('Ctrl Pts',(44.328189180088,32.4078962732452,47.9076792845813));
#27318=CARTESIAN_POINT('Ctrl Pts',(44.3110442345745,32.4221162405019,47.7042742287412));
#27319=CARTESIAN_POINT('Ctrl Pts',(44.285858338118,32.4317985392029,47.5721256201118));
#27320=CARTESIAN_POINT('Ctrl Pts',(44.2279007330723,32.4460255095263,47.379687547101));
#27321=CARTESIAN_POINT('Ctrl Pts',(44.2053143237983,32.4506940112294,47.3167351872062));
#27322=CARTESIAN_POINT('Ctrl Pts',(44.1752770885707,32.4559392091753,47.244981069327));
#27323=CARTESIAN_POINT('Ctrl Pts',(44.1709651886289,32.4566727127537,47.2349218070907));
#27324=CARTESIAN_POINT('Ctrl Pts',(44.1641938356677,32.4577946333787,47.2194888999038));
#27325=CARTESIAN_POINT('Ctrl Pts',(44.1617949926255,32.4581865277781,47.2140891440796));
#27326=CARTESIAN_POINT('Ctrl Pts',(44.1573236891308,32.4589067273784,47.204147671498));
#27327=CARTESIAN_POINT('Ctrl Pts',(44.1552584075879,32.4592354407962,47.1996029729894));
#27328=CARTESIAN_POINT('Ctrl Pts',(44.1505115886838,32.4599820751124,47.1892642271349));
#27329=CARTESIAN_POINT('Ctrl Pts',(44.1478189150676,32.4603993080739,47.183475439117));
#27330=CARTESIAN_POINT('Ctrl Pts',(44.1406958594543,32.4614869901734,47.1683587822512));
#27331=CARTESIAN_POINT('Ctrl Pts',(44.1362191641368,32.4621547102715,47.1590527867186));
#27332=CARTESIAN_POINT('Ctrl Pts',(44.1019492792773,32.4671520972365,47.0892540723202));
#27333=CARTESIAN_POINT('Ctrl Pts',(44.0690739812981,32.4713111038475,47.0303177679003));
#27334=CARTESIAN_POINT('Ctrl Pts',(43.9704788921546,32.4825378230482,46.8734946451555));
#27335=CARTESIAN_POINT('Ctrl Pts',(43.8987796684108,32.4894476872849,46.7797216508117));
#27336=CARTESIAN_POINT('Ctrl Pts',(43.7612920859757,32.501710969413,46.6304469887103));
#27337=CARTESIAN_POINT('Ctrl Pts',(43.6995356524249,32.5069475363231,46.571715719001));
#27338=CARTESIAN_POINT('Ctrl Pts',(43.6205611780423,32.5134855858658,46.5059840691251));
#27339=CARTESIAN_POINT('Ctrl Pts',(43.6068611354089,32.5146142087247,46.4948955658153));
#27340=CARTESIAN_POINT('Ctrl Pts',(43.5850319934505,32.5164049424466,46.4777172293808));
#27341=CARTESIAN_POINT('Ctrl Pts',(43.5770032213669,32.5170619953196,46.4715010403762));
#27342=CARTESIAN_POINT('Ctrl Pts',(43.5618669668022,32.5182979714027,46.4599719335952));
#27343=CARTESIAN_POINT('Ctrl Pts',(43.5547711471058,32.5188762846609,46.4546440904322));
#27344=CARTESIAN_POINT('Ctrl Pts',(43.5387867249415,32.5201766991738,46.4428138721542));
#27345=CARTESIAN_POINT('Ctrl Pts',(43.5298787483716,32.5208998194795,46.4363383207764));
#27346=CARTESIAN_POINT('Ctrl Pts',(43.507041857916,32.5227498842846,46.4200343405437));
#27347=CARTESIAN_POINT('Ctrl Pts',(43.4930374578308,32.523880902984,46.41031379066));
#27348=CARTESIAN_POINT('Ctrl Pts',(43.3755261892693,32.5333447578064,46.3310353330669));
#27349=CARTESIAN_POINT('Ctrl Pts',(43.2656461821844,32.5420539341752,46.2714918286313));
#27350=CARTESIAN_POINT('Ctrl Pts',(43.0629307744464,32.5577232508734,46.1858426480931));
#27351=CARTESIAN_POINT('Ctrl Pts',(42.9724165083657,32.5645847819425,46.1552820997704));
#27352=CARTESIAN_POINT('Ctrl Pts',(42.847258456564,32.5736596534812,46.1231286693996));
#27353=CARTESIAN_POINT('Ctrl Pts',(42.8142878400042,32.5760118153956,46.1155764874121));
#27354=CARTESIAN_POINT('Ctrl Pts',(42.76005978089,32.5798009182823,46.104647349928));
#27355=CARTESIAN_POINT('Ctrl Pts',(42.7389150499263,32.5812587968835,46.1007524126144));
#27356=CARTESIAN_POINT('Ctrl Pts',(42.7101012725517,32.5832149873657,46.0959413764203));
#27357=CARTESIAN_POINT('Ctrl Pts',(42.7024862646245,32.583729099547,46.0947167911337));
#27358=CARTESIAN_POINT('Ctrl Pts',(42.6897323012163,32.5845851188412,46.0927441927253));
#27359=CARTESIAN_POINT('Ctrl Pts',(42.6845973682915,32.5849284008608,46.0919712107347));
#27360=CARTESIAN_POINT('Ctrl Pts',(42.6748449752091,32.5855777035339,46.0905433901941));
#27361=CARTESIAN_POINT('Ctrl Pts',(42.6702281713484,32.585883954827,46.0898845475474));
#27362=CARTESIAN_POINT('Ctrl Pts',(42.6592581644352,32.5866090550458,46.0883596381499));
#27363=CARTESIAN_POINT('Ctrl Pts',(42.652902893998,32.5870270721889,46.0875084842133));
#27364=CARTESIAN_POINT('Ctrl Pts',(42.6304603840889,32.5884963505454,46.0846166111892));
#27365=CARTESIAN_POINT('Ctrl Pts',(42.6143512496176,32.5895385409978,46.0827469915871));
#27366=CARTESIAN_POINT('Ctrl Pts',(42.4850058390888,32.5978207633293,46.069385917015));
#27367=CARTESIAN_POINT('Ctrl Pts',(42.3709627678726,32.6046046755424,46.0677317354184));
#27368=CARTESIAN_POINT('Ctrl Pts',(42.199508063046,32.6148591444999,46.0804379344875));
#27369=CARTESIAN_POINT('Ctrl Pts',(42.1418137764107,32.61831778222,46.0873434197811));
#27370=CARTESIAN_POINT('Ctrl Pts',(42.0253488323188,32.6254341855636,46.1066493960196));
#27371=CARTESIAN_POINT('Ctrl Pts',(41.9666712275647,32.6290909575149,46.1192115100373));
#27372=CARTESIAN_POINT('Ctrl Pts',(41.8836648453543,32.6344358740224,46.1410730047344));
#27373=CARTESIAN_POINT('Ctrl Pts',(41.858788533113,32.6360600985312,46.1481626369091));
#27374=CARTESIAN_POINT('Ctrl Pts',(41.8145202562716,32.638995881271,46.1617470482715));
#27375=CARTESIAN_POINT('Ctrl Pts',(41.795074576193,32.6403014119288,46.1680541423516));
#27376=CARTESIAN_POINT('Ctrl Pts',(41.7655701204336,32.6423083984655,46.1781447208892));
#27377=CARTESIAN_POINT('Ctrl Pts',(41.7554362509301,32.643002488637,46.1817053330758));
#27378=CARTESIAN_POINT('Ctrl Pts',(41.7378184886579,32.6442177117306,46.1880612545936));
#27379=CARTESIAN_POINT('Ctrl Pts',(41.7303211737441,32.6447375736612,46.1908187936251));
#27380=CARTESIAN_POINT('Ctrl Pts',(41.7134514200507,32.6459135721128,46.1971427775912));
#27381=CARTESIAN_POINT('Ctrl Pts',(41.7040892876526,32.6465705913145,46.2007358751415));
#27382=CARTESIAN_POINT('Ctrl Pts',(41.6788571043233,32.6483534441502,46.2106461389446));
#27383=CARTESIAN_POINT('Ctrl Pts',(41.6630425555437,32.6494838996218,46.2171012342195));
#27384=CARTESIAN_POINT('Ctrl Pts',(41.5866986574307,32.6550061990478,46.2494521465143));
#27385=CARTESIAN_POINT('Ctrl Pts',(41.5274425534871,32.6594949575766,46.2782222468132));
#27386=CARTESIAN_POINT('Ctrl Pts',(41.3483422745964,32.6737047918526,46.376801661231));
#27387=CARTESIAN_POINT('Ctrl Pts',(41.2344706722456,32.6837145263455,46.4565326928062));
#27388=CARTESIAN_POINT('Ctrl Pts',(41.078929807297,32.6983541272594,46.5925399494304));
#27389=CARTESIAN_POINT('Ctrl Pts',(41.0301176815546,32.7031107570334,46.6400019240119));
#27390=CARTESIAN_POINT('Ctrl Pts',(40.9764713200649,32.7084384051924,46.6979905269358));
#27391=CARTESIAN_POINT('Ctrl Pts',(40.9691002675374,32.7091727474729,46.7060956217653));
#27392=CARTESIAN_POINT('Ctrl Pts',(40.957868754177,32.7102946880727,46.7186589871109));
#27393=CARTESIAN_POINT('Ctrl Pts',(40.9539591642678,32.7106857955974,46.7230727408368));
#27394=CARTESIAN_POINT('Ctrl Pts',(40.9467856978513,32.711404357457,46.7312464631874));
#27395=CARTESIAN_POINT('Ctrl Pts',(40.9435161452909,32.7117322202043,46.7350011355502));
#27396=CARTESIAN_POINT('Ctrl Pts',(40.9361042419745,32.7124763221332,46.7435796118587));
#27397=CARTESIAN_POINT('Ctrl Pts',(40.9319711763515,32.712891880276,46.7484112664765));
#27398=CARTESIAN_POINT('Ctrl Pts',(40.9212374439471,32.7139730228975,46.7610855833468));
#27399=CARTESIAN_POINT('Ctrl Pts',(40.9146751626316,32.7146359244242,46.7689606961952));
#27400=CARTESIAN_POINT('Ctrl Pts',(40.8665597502601,32.7195140008489,46.8276468457977));
#27401=CARTESIAN_POINT('Ctrl Pts',(40.8275565177226,32.7235672602918,46.8805026272857));
#27402=CARTESIAN_POINT('Ctrl Pts',(40.7253373814637,32.734802680076,47.0349405868066));
#27403=CARTESIAN_POINT('Ctrl Pts',(40.6687627797713,32.7418105329177,47.1405502067055));
#27404=CARTESIAN_POINT('Ctrl Pts',(40.5891398750078,32.7541954312319,47.3294562505877));
#27405=CARTESIAN_POINT('Ctrl Pts',(40.5612244083232,32.7594495861638,47.4103009963779));
#27406=CARTESIAN_POINT('Ctrl Pts',(40.5341224851497,32.7660074182651,47.5097401241126));
#27407=CARTESIAN_POINT('Ctrl Pts',(40.5297182559861,32.7671368207791,47.5268194729658));
#27408=CARTESIAN_POINT('Ctrl Pts',(40.5231482510522,32.7689284119007,47.5538238027289));
#27409=CARTESIAN_POINT('Ctrl Pts',(40.5208255501855,32.7695855304553,47.5637098818977));
#27410=CARTESIAN_POINT('Ctrl Pts',(40.516620345962,32.7708213975887,47.582265240335));
#27411=CARTESIAN_POINT('Ctrl Pts',(40.5147193690435,32.7713995343598,47.5909300930363));
#27412=CARTESIAN_POINT('Ctrl Pts',(40.5105941049486,32.7726992451858,47.6103732097248));
#27413=CARTESIAN_POINT('Ctrl Pts',(40.5084021672772,32.7734218354066,47.621157944987));
#27414=CARTESIAN_POINT('Ctrl Pts',(40.5030543846781,32.7752699561995,47.6486742468806));
#27415=CARTESIAN_POINT('Ctrl Pts',(40.5000276082617,32.7763995483212,47.6654296319288));
#27416=CARTESIAN_POINT('Ctrl Pts',(40.4795850524721,32.7846844393458,47.7878348228267));
#27417=CARTESIAN_POINT('Ctrl Pts',(40.4707733022669,32.7921116273483,47.8947143130847));
#27418=CARTESIAN_POINT('Ctrl Pts',(40.4709430630594,32.8053188321743,48.0810943779638));
#27419=CARTESIAN_POINT('Ctrl Pts',(40.4759095343439,32.8110110823264,48.1603507283172));
#27420=CARTESIAN_POINT('Ctrl Pts',(40.4958199445622,32.8224447983019,48.3197732298439));
#27421=CARTESIAN_POINT('Ctrl Pts',(40.5109929409353,32.828172398129,48.3997649671017));
#27422=CARTESIAN_POINT('Ctrl Pts',(40.5337810751144,32.8343753664206,48.4887535475341));
#27423=CARTESIAN_POINT('Ctrl Pts',(40.536472685262,32.8350812860896,48.4989178941643));
#27424=CARTESIAN_POINT('Ctrl Pts',(40.5409461469989,32.8362121840939,48.5152696127213));
#27425=CARTESIAN_POINT('Ctrl Pts',(40.5426760608043,32.836639958625,48.521470794975));
#27426=CARTESIAN_POINT('Ctrl Pts',(40.5458013062818,32.837395982998,48.5324609276981));
#27427=CARTESIAN_POINT('Ctrl Pts',(40.5471842024917,32.8377249321392,48.5372532529651));
#27428=CARTESIAN_POINT('Ctrl Pts',(40.5502282394737,32.8384370248065,48.5476505853408));
#27429=CARTESIAN_POINT('Ctrl Pts',(40.5518962766661,32.8388197645047,48.5532534317115));
#27430=CARTESIAN_POINT('Ctrl Pts',(40.5566900453146,32.8398991390048,48.5690918212364));
#27431=CARTESIAN_POINT('Ctrl Pts',(40.5598755762821,32.8405923999654,48.5793092507478));
#27432=CARTESIAN_POINT('Ctrl Pts',(40.5817250468115,32.8451947037126,48.6473911697807));
#27433=CARTESIAN_POINT('Ctrl Pts',(40.6030325594261,32.8489645139326,48.7043782832065));
#27434=CARTESIAN_POINT('Ctrl Pts',(40.6614775561044,32.8579933715375,48.8406760965728));
#27435=CARTESIAN_POINT('Ctrl Pts',(40.7013874549419,32.8631725591656,48.9186475439191));
#27436=CARTESIAN_POINT('Ctrl Pts',(40.8088560185719,32.875637202009,49.097488627115));
#27437=CARTESIAN_POINT('Ctrl Pts',(40.8808926557693,32.882951708786,49.1952103076591));
#27438=CARTESIAN_POINT('Ctrl Pts',(40.9729666537279,32.8917284831323,49.2982329611719));
#27439=CARTESIAN_POINT('Ctrl Pts',(40.9844907360234,32.8928176643121,49.3107884980936));
#27440=CARTESIAN_POINT('Ctrl Pts',(41.0037301866482,32.8946219828419,49.33120034385));
#27441=CARTESIAN_POINT('Ctrl Pts',(41.0113493116389,32.8953330021545,49.3391463715941));
#27442=CARTESIAN_POINT('Ctrl Pts',(41.0252288712522,32.8966222150939,49.3533756179059));
#27443=CARTESIAN_POINT('Ctrl Pts',(41.0314654642989,32.8971993556388,49.3596817420832));
#27444=CARTESIAN_POINT('Ctrl Pts',(41.0449308612265,32.8984410221111,49.3731107653558));
#27445=CARTESIAN_POINT('Ctrl Pts',(41.05217280408,32.8991061245981,49.3802200505857));
#27446=CARTESIAN_POINT('Ctrl Pts',(41.072135949775,32.9009324807351,49.3995105666265));
#27447=CARTESIAN_POINT('Ctrl Pts',(41.0849681527182,32.9020987394458,49.4115749953383));
#27448=CARTESIAN_POINT('Ctrl Pts',(41.1606741716367,32.9089368881136,49.4808230883911));
#27449=CARTESIAN_POINT('Ctrl Pts',(41.2270979607387,32.9147754136375,49.5339695961183));
#27450=CARTESIAN_POINT('Ctrl Pts',(41.3924096041987,32.9289219182915,49.6492081059154));
#27451=CARTESIAN_POINT('Ctrl Pts',(41.4938597452921,32.9373218283312,49.7070538543969));
#27452=CARTESIAN_POINT('Ctrl Pts',(41.6227314563021,32.9473627504026,49.7657932404724));
#27453=CARTESIAN_POINT('Ctrl Pts',(41.645765002433,32.94913352297,49.7757538680722));
#27454=CARTESIAN_POINT('Ctrl Pts',(41.7101550212048,32.9540072854119,49.8021197059625));
#27455=CARTESIAN_POINT('Ctrl Pts',(41.7518972880076,32.9570810654367,49.8175491834415));
#27456=CARTESIAN_POINT('Ctrl Pts',(41.7941388318293,32.9600825139687,49.8315225365261));
#27457=CARTESIAN_POINT('Ctrl Pts',(41.7941386107368,33.1302767167271,49.8315224633894));
#27458=CARTESIAN_POINT('Ctrl Pts',(41.7615147270867,33.127859421335,49.8207305938566));
#27459=CARTESIAN_POINT('Ctrl Pts',(41.7291717434368,33.1254237180773,49.8090646017079));
#27460=CARTESIAN_POINT('Ctrl Pts',(41.6149606743047,33.1166972958759,49.7643819978487));
#27461=CARTESIAN_POINT('Ctrl Pts',(41.5350796627018,33.1103547917976,49.7266278222783));
#27462=CARTESIAN_POINT('Ctrl Pts',(41.4061633483993,33.0999288319688,49.6544993513602));
#27463=CARTESIAN_POINT('Ctrl Pts',(41.3556279388961,33.0957902366805,49.6230735941093));
#27464=CARTESIAN_POINT('Ctrl Pts',(41.297850656533,33.091063592458,49.5833264650798));
#27465=CARTESIAN_POINT('Ctrl Pts',(41.2891304590911,33.0903503774043,49.5772205762432));
#27466=CARTESIAN_POINT('Ctrl Pts',(41.2757115790359,33.0892536778906,49.5676581627451));
#27467=CARTESIAN_POINT('Ctrl Pts',(41.2709774423454,33.0888669250832,49.5642521009344));
#27468=CARTESIAN_POINT('Ctrl Pts',(41.2622246661972,33.0881522788655,49.5578943182576));
#27469=CARTESIAN_POINT('Ctrl Pts',(41.2582020374948,33.0878240133612,49.554948497781));
#27470=CARTESIAN_POINT('Ctrl Pts',(41.2490030964146,33.0870736841918,49.5481570543374));
#27471=CARTESIAN_POINT('Ctrl Pts',(41.2438346079019,33.0866523482214,49.5443010477344));
#27472=CARTESIAN_POINT('Ctrl Pts',(41.2302549001728,33.0855456816944,49.534063371676));
#27473=CARTESIAN_POINT('Ctrl Pts',(41.2218764321198,33.0848632461135,49.5276383399584));
#27474=CARTESIAN_POINT('Ctrl Pts',(41.1405643025086,33.0782391709025,49.4642172178386));
#27475=CARTESIAN_POINT('Ctrl Pts',(41.0717589759254,33.0726223398984,49.4021022875851));
#27476=CARTESIAN_POINT('Ctrl Pts',(40.9990185411646,33.0663226256873,49.3262540637331));
#27477=CARTESIAN_POINT('Ctrl Pts',(40.9904520660688,33.0655745477457,49.3171459732951));
#27478=CARTESIAN_POINT('Ctrl Pts',(40.9262198504802,33.059912931797,49.247508338125));
#27479=CARTESIAN_POINT('Ctrl Pts',(40.8743876223578,33.0550375394858,49.1835588172295));
#27480=CARTESIAN_POINT('Ctrl Pts',(40.7787915528492,33.0450471402053,49.0488590267635));
#27481=CARTESIAN_POINT('Ctrl Pts',(40.7352052952309,33.0399403918666,48.9782014859006));
#27482=CARTESIAN_POINT('Ctrl Pts',(40.688091078958,33.0335489588917,48.8895037288625));
#27483=CARTESIAN_POINT('Ctrl Pts',(40.6800897137146,33.0324278142054,48.8739322698421));
#27484=CARTESIAN_POINT('Ctrl Pts',(40.6677978270342,33.0306466047338,48.8491882413673));
#27485=CARTESIAN_POINT('Ctrl Pts',(40.6633655759673,33.0299915151533,48.8400868455566));
#27486=CARTESIAN_POINT('Ctrl Pts',(40.6551851871595,33.0287578144078,48.8229474331243));
#27487=CARTESIAN_POINT('Ctrl Pts',(40.6514204334554,33.0281798003556,48.8149176055436));
#27488=CARTESIAN_POINT('Ctrl Pts',(40.6430955762017,33.0268781883101,48.7968382438436));
#27489=CARTESIAN_POINT('Ctrl Pts',(40.6385661008055,33.0261535565662,48.7867750322433));
#27490=CARTESIAN_POINT('Ctrl Pts',(40.6272237306765,33.0242959656867,48.7609865608202));
#27491=CARTESIAN_POINT('Ctrl Pts',(40.6205337051132,33.0231588685262,48.7452086418029));
#27492=CARTESIAN_POINT('Ctrl Pts',(40.5682651120988,33.0139277823888,48.6172185293761));
#27493=CARTESIAN_POINT('Ctrl Pts',(40.5331443989851,33.005480343087,48.5010507189353));
#27494=CARTESIAN_POINT('Ctrl Pts',(40.4917450432384,32.9906207077751,48.2963315506964));
#27495=CARTESIAN_POINT('Ctrl Pts',(40.4802380464948,32.9843115903462,48.2091975567793));
#27496=CARTESIAN_POINT('Ctrl Pts',(40.4721369186006,32.9752353741278,48.0809137529819));
#27497=CARTESIAN_POINT('Ctrl Pts',(40.4708577562553,32.9723849732908,48.0401711806233));
#27498=CARTESIAN_POINT('Ctrl Pts',(40.4708773732771,32.9679288131525,47.9753400246355));
#27499=CARTESIAN_POINT('Ctrl Pts',(40.4713353791613,32.9662914876989,47.9512646773269));
#27500=CARTESIAN_POINT('Ctrl Pts',(40.4725581146939,32.9641183941057,47.9188851465437));
#27501=CARTESIAN_POINT('Ctrl Pts',(40.4729260522475,32.9635628696974,47.9105693183467));
#27502=CARTESIAN_POINT('Ctrl Pts',(40.4735907117892,32.9626919997224,47.8974680838602));
#27503=CARTESIAN_POINT('Ctrl Pts',(40.4738514622092,32.9623747088496,47.8926810773693));
#27504=CARTESIAN_POINT('Ctrl Pts',(40.4744253604253,32.9617231808707,47.8828219845888));
#27505=CARTESIAN_POINT('Ctrl Pts',(40.4747407062539,32.9613890864397,47.8777501236156));
#27506=CARTESIAN_POINT('Ctrl Pts',(40.475547395764,32.9605881755256,47.8655540033088));
#27507=CARTESIAN_POINT('Ctrl Pts',(40.4760582699671,32.9601224414514,47.8584310225197));
#27508=CARTESIAN_POINT('Ctrl Pts',(40.4779692693259,32.9585126584404,47.8337109881351));
#27509=CARTESIAN_POINT('Ctrl Pts',(40.4795714084917,32.9573792573921,47.8161298191591));
#27510=CARTESIAN_POINT('Ctrl Pts',(40.4841149842176,32.9546122004852,47.7728525498307));
#27511=CARTESIAN_POINT('Ctrl Pts',(40.487332296015,32.9529912285091,47.7471883201765));
#27512=CARTESIAN_POINT('Ctrl Pts',(40.5030641468658,32.9462333323331,47.6393198699513));
#27513=CARTESIAN_POINT('Ctrl Pts',(40.5203709789221,32.9412653538758,47.5578997366747));
#27514=CARTESIAN_POINT('Ctrl Pts',(40.5807614609927,32.9279539466273,47.3431120367659));
#27515=CARTESIAN_POINT('Ctrl Pts',(40.6331874290855,32.9196337565058,47.2129177703834));
#27516=CARTESIAN_POINT('Ctrl Pts',(40.7099032863855,32.9093818880291,47.0696092234485));
#27517=CARTESIAN_POINT('Ctrl Pts',(40.7209247792119,32.9079444066352,47.0498630447721));
#27518=CARTESIAN_POINT('Ctrl Pts',(40.7379976636677,32.9057666619252,47.0205002769766));
#27519=CARTESIAN_POINT('Ctrl Pts',(40.7437913048257,32.9050356301211,47.0107355144459));
#27520=CARTESIAN_POINT('Ctrl Pts',(40.7539917679356,32.9037618961415,46.9938841586329));
#27521=CARTESIAN_POINT('Ctrl Pts',(40.7583590416499,32.9032206478411,46.9867738917276));
#27522=CARTESIAN_POINT('Ctrl Pts',(40.7675623655489,32.9020883782403,46.9720058595979));
#27523=CARTESIAN_POINT('Ctrl Pts',(40.7724064791666,32.9014970682631,46.9643533859073));
#27524=CARTESIAN_POINT('Ctrl Pts',(40.7840204656009,32.9000901291989,46.9462889687548));
#27525=CARTESIAN_POINT('Ctrl Pts',(40.7908372837079,32.8992727607925,46.9359078361565));
#27526=CARTESIAN_POINT('Ctrl Pts',(40.8141873958028,32.8965005492696,46.9010861664034));
#27527=CARTESIAN_POINT('Ctrl Pts',(40.8311803527963,32.8945284543902,46.8769603837267));
#27528=CARTESIAN_POINT('Ctrl Pts',(40.9495979977378,32.881074625599,46.7167714976733));
#27529=CARTESIAN_POINT('Ctrl Pts',(41.0680281891642,32.8688951677033,46.5942366766812));
#27530=CARTESIAN_POINT('Ctrl Pts',(41.2651054740751,32.8509873867075,46.4378631845213));
#27531=CARTESIAN_POINT('Ctrl Pts',(41.332483331483,32.8452145362849,46.3910660896583));
#27532=CARTESIAN_POINT('Ctrl Pts',(41.4116435852658,32.8389696709358,46.3432547657331));
#27533=CARTESIAN_POINT('Ctrl Pts',(41.4206909434239,32.8382635219546,46.337890810566));
#27534=CARTESIAN_POINT('Ctrl Pts',(41.4353450787058,32.8371324903369,46.3293639335814));
#27535=CARTESIAN_POINT('Ctrl Pts',(41.4409244611659,32.8367048066551,46.3261546972988));
#27536=CARTESIAN_POINT('Ctrl Pts',(41.4508532638451,32.8359490706671,46.3205096373435));
#27537=CARTESIAN_POINT('Ctrl Pts',(41.4551961758112,32.8356203183103,46.3180626822602));
#27538=CARTESIAN_POINT('Ctrl Pts',(41.4646476200966,32.8349088020585,46.3127855540667));
#27539=CARTESIAN_POINT('Ctrl Pts',(41.4697595417082,32.8345264404781,46.3099617302722));
#27540=CARTESIAN_POINT('Ctrl Pts',(41.4842590282512,32.8334486511038,46.3020379385212));
#27541=CARTESIAN_POINT('Ctrl Pts',(41.493676421316,32.8327565844146,46.296992579891));
#27542=CARTESIAN_POINT('Ctrl Pts',(41.5566350324331,32.8281793079464,46.2639327504259));
#27543=CARTESIAN_POINT('Ctrl Pts',(41.6114310020281,32.8244316562747,46.2383659602684));
#27544=CARTESIAN_POINT('Ctrl Pts',(41.7485416370087,32.8154058173238,46.182075593339));
#27545=CARTESIAN_POINT('Ctrl Pts',(41.8319246032079,32.81020979572,46.1543188741337));
#27546=CARTESIAN_POINT('Ctrl Pts',(42.0342894251511,32.7977232185353,46.1019752839152));
#27547=CARTESIAN_POINT('Ctrl Pts',(42.1542519273775,32.7904040371647,46.0827508575401));
#27548=CARTESIAN_POINT('Ctrl Pts',(42.2922506237716,32.7816202483702,46.0738058197902));
#27549=CARTESIAN_POINT('Ctrl Pts',(42.3092985065227,32.7805293188496,46.0729278277196));
#27550=CARTESIAN_POINT('Ctrl Pts',(42.3373620300573,32.778722857676,46.0718557198696));
#27551=CARTESIAN_POINT('Ctrl Pts',(42.3483718960755,32.7780114644838,46.0715295151742));
#27552=CARTESIAN_POINT('Ctrl Pts',(42.3682480128104,32.7767220794704,46.0711109472227));
#27553=CARTESIAN_POINT('Ctrl Pts',(42.3771133139427,32.7761451453899,46.0709853909832));
#27554=CARTESIAN_POINT('Ctrl Pts',(42.3961150243766,32.7749044872833,46.0708472825056));
#27555=CARTESIAN_POINT('Ctrl Pts',(42.4062512608656,32.7742401912574,46.0708535007625));
#27556=CARTESIAN_POINT('Ctrl Pts',(42.433955540078,32.7724175289279,46.0710888406797));
#27557=CARTESIAN_POINT('Ctrl Pts',(42.4515208891821,32.7712541878074,46.0714780783368));
#27558=CARTESIAN_POINT('Ctrl Pts',(42.5532357004277,32.7644710652349,46.0751226037742));
#27559=CARTESIAN_POINT('Ctrl Pts',(42.6370937402029,32.7586878041765,46.0836448113319));
#27560=CARTESIAN_POINT('Ctrl Pts',(42.8311038473629,32.7448819182853,46.1162912055346));
#27561=CARTESIAN_POINT('Ctrl Pts',(42.9402395245262,32.736779565787,46.1446434519515));
#27562=CARTESIAN_POINT('Ctrl Pts',(43.1157247084538,32.7235535862841,46.2070375847799));
#27563=CARTESIAN_POINT('Ctrl Pts',(43.1837136784464,32.7183818255549,46.2356951968113));
#27564=CARTESIAN_POINT('Ctrl Pts',(43.2592278210297,32.7127030014276,46.2727542088044));
#27565=CARTESIAN_POINT('Ctrl Pts',(43.2685166728648,32.7120056694562,46.2774062370224));
#27566=CARTESIAN_POINT('Ctrl Pts',(43.2834647895333,32.7108859854207,46.2850441834349));
#27567=CARTESIAN_POINT('Ctrl Pts',(43.2891474252043,32.7104609186149,46.2879835438041));
#27568=CARTESIAN_POINT('Ctrl Pts',(43.299228663118,32.7097080230181,46.2932618290844));
#27569=CARTESIAN_POINT('Ctrl Pts',(43.303632935062,32.7093795146122,46.2955895760596));
#27570=CARTESIAN_POINT('Ctrl Pts',(43.3132053279991,32.7086664465512,46.3006963145658));
#27571=CARTESIAN_POINT('Ctrl Pts',(43.3183698100338,32.7082823048892,46.3034818360255));
#27572=CARTESIAN_POINT('Ctrl Pts',(43.3330142327483,32.7071944280713,46.31146693848));
#27573=CARTESIAN_POINT('Ctrl Pts',(43.3424634626311,32.7064941539107,46.3167228115757));
#27574=CARTESIAN_POINT('Ctrl Pts',(43.4073298375056,32.7016950211493,46.3535204147001));
#27575=CARTESIAN_POINT('Ctrl Pts',(43.4612038690275,32.6977495003872,46.3877169585655));
#27576=CARTESIAN_POINT('Ctrl Pts',(43.6188245052923,32.6860217710254,46.4990975467148));
#27577=CARTESIAN_POINT('Ctrl Pts',(43.7166001581044,32.678467968548,46.5840877198615));
#27578=CARTESIAN_POINT('Ctrl Pts',(43.8293819805125,32.6684938429855,46.7039826863542));
#27579=CARTESIAN_POINT('Ctrl Pts',(43.8529035644283,32.6663334550125,46.7304076329116));
#27580=CARTESIAN_POINT('Ctrl Pts',(43.9063426028066,32.661208189995,46.7938739041656));
#27581=CARTESIAN_POINT('Ctrl Pts',(43.9356402995454,32.6582249806155,46.8314040515661));
#27582=CARTESIAN_POINT('Ctrl Pts',(43.9725025054451,32.6542080375318,46.8824072071422));
#27583=CARTESIAN_POINT('Ctrl Pts',(43.9813376568428,32.6532235633975,46.8949439049024));
#27584=CARTESIAN_POINT('Ctrl Pts',(43.99548729691,32.6516102644668,46.9155388507849));
#27585=CARTESIAN_POINT('Ctrl Pts',(44.0008925529039,32.6509849133545,46.9235341495559));
#27586=CARTESIAN_POINT('Ctrl Pts',(44.0112077975302,32.6497736531223,46.9390416941349));
#27587=CARTESIAN_POINT('Ctrl Pts',(44.0161258140627,32.6491880673004,46.9465483199852));
#27588=CARTESIAN_POINT('Ctrl Pts',(44.0274511110583,32.6478203858908,46.9641006784119));
#27589=CARTESIAN_POINT('Ctrl Pts',(44.0338179963109,32.6470368124478,46.9741719113712));
#27590=CARTESIAN_POINT('Ctrl Pts',(44.0540731472851,32.6444954929287,47.0068787481755));
#27591=CARTESIAN_POINT('Ctrl Pts',(44.0675869142557,32.6427241715028,47.0297414979195));
#27592=CARTESIAN_POINT('Ctrl Pts',(44.0984068780175,32.6384970282286,47.0844299140084));
#27593=CARTESIAN_POINT('Ctrl Pts',(44.1152965745122,32.6360275145451,47.116477572618));
#27594=CARTESIAN_POINT('Ctrl Pts',(44.209513071513,32.6213025006089,47.3081469800617));
#27595=CARTESIAN_POINT('Ctrl Pts',(44.2654163227491,32.6083776283653,47.4773104515767));
#27596=CARTESIAN_POINT('Ctrl Pts',(44.3054846192847,32.5928440791353,47.6955959439858));
#27597=CARTESIAN_POINT('Ctrl Pts',(44.3120160775499,32.589764410194,47.739752635199));
#27598=CARTESIAN_POINT('Ctrl Pts',(44.3181514334363,32.5860719052369,47.7942293858239));
#27599=CARTESIAN_POINT('Ctrl Pts',(44.3192119884425,32.5853892211959,47.8043681471091));
#27600=CARTESIAN_POINT('Ctrl Pts',(44.3207493955662,32.5843251557278,47.8202838212652));
#27601=CARTESIAN_POINT('Ctrl Pts',(44.321280646642,32.583940873049,47.8260551107366));
#27602=CARTESIAN_POINT('Ctrl Pts',(44.322216999829,32.5832314044185,47.8367553397053));
#27603=CARTESIAN_POINT('Ctrl Pts',(44.3226291568514,32.5829058468177,47.841683419876));
#27604=CARTESIAN_POINT('Ctrl Pts',(44.3235375472108,32.5821561998802,47.8530719817408));
#27605=CARTESIAN_POINT('Ctrl Pts',(44.3240201877445,32.5817328729143,47.8595334266394));
#27606=CARTESIAN_POINT('Ctrl Pts',(44.3254318188024,32.5804105765569,47.8798064653185));
#27607=CARTESIAN_POINT('Ctrl Pts',(44.3262447371161,32.5795177967145,47.8936260652181));
#27608=CARTESIAN_POINT('Ctrl Pts',(44.3278097648141,32.5774304088608,47.9262115443997));
#27609=CARTESIAN_POINT('Ctrl Pts',(44.3284367594633,32.5762417983661,47.9449823059044));
#27610=CARTESIAN_POINT('Ctrl Pts',(44.3297155327105,32.5719725214781,48.013041969864));
#27611=CARTESIAN_POINT('Ctrl Pts',(44.3287524257359,32.5689563944188,48.0623449278515));
#27612=CARTESIAN_POINT('Ctrl Pts',(44.3162504896511,32.5558853102316,48.2781704342769));
#27613=CARTESIAN_POINT('Ctrl Pts',(44.285022401705,32.5461921927418,48.4428158778149));
#27614=CARTESIAN_POINT('Ctrl Pts',(44.220990190609,32.5334096322984,48.6379814136542));
#27615=CARTESIAN_POINT('Ctrl Pts',(44.2078928390235,32.5309830755487,48.6742022871535));
#27616=CARTESIAN_POINT('Ctrl Pts',(44.1885021972832,32.5276140217928,48.7231898224253));
#27617=CARTESIAN_POINT('Ctrl Pts',(44.1831382407902,32.5267025539517,48.73631625386));
#27618=CARTESIAN_POINT('Ctrl Pts',(44.1743421410815,32.5252391859063,48.7571817278413));
#27619=CARTESIAN_POINT('Ctrl Pts',(44.1710028497136,32.5246904467517,48.7649595447407));
#27620=CARTESIAN_POINT('Ctrl Pts',(44.164014236772,32.5235557022868,48.7809462400385));
#27621=CARTESIAN_POINT('Ctrl Pts',(44.1603585503434,32.5229694899477,48.7891520936953));
#27622=CARTESIAN_POINT('Ctrl Pts',(44.1517012749385,32.5215979875712,48.8082254106238));
#27623=CARTESIAN_POINT('Ctrl Pts',(44.1466556898427,32.5208111961935,48.8190723784543));
#27624=CARTESIAN_POINT('Ctrl Pts',(44.129972898071,32.5182491598198,48.8540817049404));
#27625=CARTESIAN_POINT('Ctrl Pts',(44.117933087236,32.5164600339134,48.8780475904377));
#27626=CARTESIAN_POINT('Ctrl Pts',(44.0882494272282,32.5121827663386,48.9341853765786));
#27627=CARTESIAN_POINT('Ctrl Pts',(44.0701801158531,32.5096804963287,48.9661193139892));
#27628=CARTESIAN_POINT('Ctrl Pts',(43.9963660500525,32.4998334922583,49.0883053980668));
#27629=CARTESIAN_POINT('Ctrl Pts',(43.9341310325276,32.4922852062604,49.1744064812181));
#27630=CARTESIAN_POINT('Ctrl Pts',(43.7969518240043,32.4772203905606,49.3345624314687));
#27631=CARTESIAN_POINT('Ctrl Pts',(43.7223765700516,32.469731523701,49.4084941399137));
#27632=CARTESIAN_POINT('Ctrl Pts',(43.6295781301487,32.4614744149673,49.4865902059251));
#27633=CARTESIAN_POINT('Ctrl Pts',(43.6168646142309,32.4603643981281,49.49701482067));
#27634=CARTESIAN_POINT('Ctrl Pts',(43.5989795460197,32.4588339056251,49.5113014934771));
#27635=CARTESIAN_POINT('Ctrl Pts',(43.5939199674711,32.4584043359862,49.5153017092899));
#27636=CARTESIAN_POINT('Ctrl Pts',(43.5851593075931,32.4576665117619,49.5221569627609));
#27637=CARTESIAN_POINT('Ctrl Pts',(43.5814677765303,32.4573574227233,49.5250240318914));
#27638=CARTESIAN_POINT('Ctrl Pts',(43.5736659969172,32.4567080597173,49.5310380403035));
#27639=CARTESIAN_POINT('Ctrl Pts',(43.5695534419046,32.4563680145791,49.5341818994897));
#27640=CARTESIAN_POINT('Ctrl Pts',(43.5593293723149,32.4555280737974,49.5419327276482));
#27641=CARTESIAN_POINT('Ctrl Pts',(43.5532029182652,32.4550295412523,49.546520017413));
#27642=CARTESIAN_POINT('Ctrl Pts',(43.5300763445239,32.4531648316923,49.5636226007144));
#27643=CARTESIAN_POINT('Ctrl Pts',(43.5128977574236,32.4518143452906,49.5758955714776));
#27644=CARTESIAN_POINT('Ctrl Pts',(43.3768404747242,32.4413564985689,49.6697648057039));
#27645=CARTESIAN_POINT('Ctrl Pts',(43.2493393069896,32.4329333940499,49.7380925822542));
#27646=CARTESIAN_POINT('Ctrl Pts',(43.013035733349,32.4177010972683,49.8324515719433));
#27647=CARTESIAN_POINT('Ctrl Pts',(42.9073716629756,32.4110112709358,49.8644733350024));
#27648=CARTESIAN_POINT('Ctrl Pts',(42.7828843201844,32.4029288151265,49.8908285766093));
#27649=CARTESIAN_POINT('Ctrl Pts',(42.766162744866,32.4018394593182,49.8941377783271));
#27650=CARTESIAN_POINT('Ctrl Pts',(42.7385785185858,32.4000353175995,49.8992177911765));
#27651=CARTESIAN_POINT('Ctrl Pts',(42.7277404434161,32.3993246588688,49.9011180460505));
#27652=CARTESIAN_POINT('Ctrl Pts',(42.708147300367,32.3980364239191,49.9043808171335));
#27653=CARTESIAN_POINT('Ctrl Pts',(42.6993979158559,32.3974599027952,49.9057759414372));
#27654=CARTESIAN_POINT('Ctrl Pts',(42.6806229527741,32.3962199386853,49.9086372032618));
#27655=CARTESIAN_POINT('Ctrl Pts',(42.6705948488278,32.3955559226203,49.9100847196975));
#27656=CARTESIAN_POINT('Ctrl Pts',(42.6431475437532,32.3937335437654,49.9138261449776));
#27657=CARTESIAN_POINT('Ctrl Pts',(42.6257080266696,32.3925702005636,49.9159611407884));
#27658=CARTESIAN_POINT('Ctrl Pts',(42.5243698113536,32.3857768113485,49.9269645121615));
#27659=CARTESIAN_POINT('Ctrl Pts',(42.4400022139649,32.3799825382938,49.9305585625719));
#27660=CARTESIAN_POINT('Ctrl Pts',(42.2416140427867,32.3660557013752,49.9259995763934));
#27661=CARTESIAN_POINT('Ctrl Pts',(42.1280088908297,32.357838023745,49.9132638553038));
#27662=CARTESIAN_POINT('Ctrl Pts',(41.9456239564482,32.3446288845988,49.8762387891454));
#27663=CARTESIAN_POINT('Ctrl Pts',(41.8758919321985,32.3395798094311,49.8579673498479));
#27664=CARTESIAN_POINT('Ctrl Pts',(41.8029333694424,32.3344039767775,49.8344141902643));
#27665=CARTESIAN_POINT('Ctrl Pts',(41.7985335092115,32.3340922710875,49.8329762802391));
#27666=CARTESIAN_POINT('Ctrl Pts',(41.794138831786,32.3337813919524,49.8315225365117));
#27667=CARTESIAN_POINT('Origin',(42.4,47.1748,48.));
#27668=CARTESIAN_POINT('',(40.0365300974769,46.7157731502363,48.0006787984381));
#27669=CARTESIAN_POINT('',(43.4903488624466,46.9748,50.0969334274272));
#27670=CARTESIAN_POINT('Ctrl Pts',(40.0365300974771,46.7157731502717,48.0006787990958));
#27671=CARTESIAN_POINT('Ctrl Pts',(40.0365388030446,46.7174032156133,48.030990193079));
#27672=CARTESIAN_POINT('Ctrl Pts',(40.0371305975263,46.7190332809549,48.0612934096708));
#27673=CARTESIAN_POINT('Ctrl Pts',(40.0383046853366,46.7206633462965,48.0915733672902));
#27674=CARTESIAN_POINT('Ctrl Pts',(40.0413609422814,46.7249065540677,48.1703948403946));
#27675=CARTESIAN_POINT('Ctrl Pts',(40.0483732154124,46.7291497618388,48.2492105493059));
#27676=CARTESIAN_POINT('Ctrl Pts',(40.0593432685315,46.73339296961,48.3275919814818));
#27677=CARTESIAN_POINT('Ctrl Pts',(40.0702973976645,46.737630017996,48.4058596361922));
#27678=CARTESIAN_POINT('Ctrl Pts',(40.0851978327039,46.7418670663821,48.4836938069707));
#27679=CARTESIAN_POINT('Ctrl Pts',(40.1039943670488,46.7461041147681,48.5606679715807));
#27680=CARTESIAN_POINT('Ctrl Pts',(40.1227687031728,46.7503361593095,48.6375512316929));
#27681=CARTESIAN_POINT('Ctrl Pts',(40.145429883651,46.754568203851,48.7135760523368));
#27682=CARTESIAN_POINT('Ctrl Pts',(40.1718763758854,46.7588002483924,48.7883245249022));
#27683=CARTESIAN_POINT('Ctrl Pts',(40.1983057184753,46.7630295485978,48.8630245256433));
#27684=CARTESIAN_POINT('Ctrl Pts',(40.228515344752,46.7672588488033,48.9364493817146));
#27685=CARTESIAN_POINT('Ctrl Pts',(40.2623537838844,46.7714881490088,49.0081959609255));
#27686=CARTESIAN_POINT('Ctrl Pts',(40.2961807462329,46.7757160147874,49.0799182062722));
#27687=CARTESIAN_POINT('Ctrl Pts',(40.3336338779797,46.7799438805661,49.1499628826561));
#27688=CARTESIAN_POINT('Ctrl Pts',(40.3745140131288,46.7841717463447,49.2179478469492));
#27689=CARTESIAN_POINT('Ctrl Pts',(40.4153929270747,46.7883994858252,49.2859307803428));
#27690=CARTESIAN_POINT('Ctrl Pts',(40.4596983989203,46.7926272253058,49.3518537239599));
#27691=CARTESIAN_POINT('Ctrl Pts',(40.5071865997293,46.7968549647863,49.4153613929508));
#27692=CARTESIAN_POINT('Ctrl Pts',(40.5547205133257,46.8010867739463,49.4789301952869));
#27693=CARTESIAN_POINT('Ctrl Pts',(40.6054429958083,46.8053185831063,49.5400787030201));
#27694=CARTESIAN_POINT('Ctrl Pts',(40.6590687276934,46.8095503922663,49.5984832642242));
#27695=CARTESIAN_POINT('Ctrl Pts',(40.7127192606394,46.8137841585718,49.6569148366229));
#27696=CARTESIAN_POINT('Ctrl Pts',(40.7692753849433,46.8180179248772,49.7125996052308));
#27697=CARTESIAN_POINT('Ctrl Pts',(40.8284153563963,46.8222516911827,49.7652512990759));
#27698=CARTESIAN_POINT('Ctrl Pts',(40.8876603719865,46.8264929774838,49.8179965126102));
#27699=CARTESIAN_POINT('Ctrl Pts',(40.9494980405442,46.8307342637849,49.8676975919985));
#27700=CARTESIAN_POINT('Ctrl Pts',(41.013574195887,46.834975550086,49.9141091741564));
#27701=CARTESIAN_POINT('Ctrl Pts',(41.073569654564,46.8389467296247,49.9575650298424));
#27702=CARTESIAN_POINT('Ctrl Pts',(41.1355270033101,46.8429179091634,49.998137282269));
#27703=CARTESIAN_POINT('Ctrl Pts',(41.1991358615461,46.8468890887021,50.0356610134979));
#27704=CARTESIAN_POINT('Ctrl Pts',(41.2670255033899,46.8511275228456,50.0757100372411));
#27705=CARTESIAN_POINT('Ctrl Pts',(41.3370471788954,46.8553659569892,50.1124337060636));
#27706=CARTESIAN_POINT('Ctrl Pts',(41.4088418280244,46.8596043911328,50.1455991981323));
#27707=CARTESIAN_POINT('Ctrl Pts',(41.4805339567318,46.8638367729304,50.1787173309581));
#27708=CARTESIAN_POINT('Ctrl Pts',(41.5539936093392,46.868069154728,50.2082871826824));
#27709=CARTESIAN_POINT('Ctrl Pts',(41.6288353142845,46.8723015365256,50.2341207372041));
#27710=CARTESIAN_POINT('Ctrl Pts',(41.7035917373713,46.8765290955391,50.2599248544816));
#27711=CARTESIAN_POINT('Ctrl Pts',(41.779726642607,46.8807566545526,50.2820009830718));
#27712=CARTESIAN_POINT('Ctrl Pts',(41.8568340596542,46.8849842135661,50.3002089474977));
#27713=CARTESIAN_POINT('Ctrl Pts',(41.9338934632194,46.8892091401502,50.3184055741326));
#27714=CARTESIAN_POINT('Ctrl Pts',(42.0119237218414,46.8934340667344,50.3327387101318));
#27715=CARTESIAN_POINT('Ctrl Pts',(42.090504335332,46.8976589933185,50.3431181947251));
#27716=CARTESIAN_POINT('Ctrl Pts',(42.1690604450329,46.901882602444,50.353494442684));
#27717=CARTESIAN_POINT('Ctrl Pts',(42.24816610469,46.9061062115694,50.3599194261523));
#27718=CARTESIAN_POINT('Ctrl Pts',(42.3273927376713,46.9103298206949,50.3623544667042));
#27719=CARTESIAN_POINT('Ctrl Pts',(42.4066192926496,46.9145534256619,50.3647895048586));
#27720=CARTESIAN_POINT('Ctrl Pts',(42.4859663524167,46.918777030629,50.3632345949384));
#27721=CARTESIAN_POINT('Ctrl Pts',(42.5650038545159,46.9230006355961,50.3577031553813));
#27722=CARTESIAN_POINT('Ctrl Pts',(42.6441216143524,46.9272285293751,50.3521660989864));
#27723=CARTESIAN_POINT('Ctrl Pts',(42.7229287201695,46.931456423154,50.3426444797425));
#27724=CARTESIAN_POINT('Ctrl Pts',(42.8009993411237,46.935684316933,50.3292037200121));
#27725=CARTESIAN_POINT('Ctrl Pts',(42.8791081960042,46.9399142812601,50.3157563778695));
#27726=CARTESIAN_POINT('Ctrl Pts',(42.9564793898032,46.9441442455872,50.2983861744852));
#27727=CARTESIAN_POINT('Ctrl Pts',(43.0326989421299,46.9483742099143,50.2772093644476));
#27728=CARTESIAN_POINT('Ctrl Pts',(43.1090582419274,46.9526119298211,50.2559937270284));
#27729=CARTESIAN_POINT('Ctrl Pts',(43.1842612353293,46.956849649728,50.2309576849966));
#27730=CARTESIAN_POINT('Ctrl Pts',(43.2579109006931,46.9610873696348,50.2022668610711));
#27731=CARTESIAN_POINT('Ctrl Pts',(43.3275881903807,46.9650965234593,50.1751235082784));
#27732=CARTESIAN_POINT('Ctrl Pts',(43.3958750636315,46.9691056772837,50.1447095516255));
#27733=CARTESIAN_POINT('Ctrl Pts',(43.4624562730563,46.9731148311082,50.1112027635316));
#27734=CARTESIAN_POINT('Ctrl Pts',(43.4717849733108,46.9736765540721,50.106508123928));
#27735=CARTESIAN_POINT('Ctrl Pts',(43.4810826793527,46.9742382770361,50.1017515928794));
#27736=CARTESIAN_POINT('Ctrl Pts',(43.4903488624466,46.9748,50.0969334274272));
#27737=CARTESIAN_POINT('',(41.309406738763,46.9748,50.0968063285493));
#27738=CARTESIAN_POINT('Origin',(42.4,46.9748,48.));
#27739=CARTESIAN_POINT('',(40.036080165837,46.8369518497283,48.0019190348969));
#27740=CARTESIAN_POINT('Ctrl Pts',(41.309406738763,46.9748,50.0968063285493));
#27741=CARTESIAN_POINT('Ctrl Pts',(40.6110438901808,46.9327247525314,49.7335730598435));
#27742=CARTESIAN_POINT('Ctrl Pts',(40.0689346244942,46.8867753691075,48.9289907544835));
#27743=CARTESIAN_POINT('Ctrl Pts',(40.0334053491648,46.8408259856836,48.0740634180572));
#27744=CARTESIAN_POINT('Ctrl Pts',(40.0338853815248,46.8369518497283,48.0019208166272));
#27745=CARTESIAN_POINT('',(40.0365304449332,46.0432018497572,48.0014502318932));
#27746=CARTESIAN_POINT('Ctrl Pts',(40.0365307787896,46.8369518497283,48.0019186690884));
#27747=CARTESIAN_POINT('Ctrl Pts',(40.036468137554,46.8328034394031,47.9247554765118));
#27748=CARTESIAN_POINT('Ctrl Pts',(40.0401885216025,46.8286550290779,47.8474148710146));
#27749=CARTESIAN_POINT('Ctrl Pts',(40.0477175957458,46.8245066187527,47.7703090521241));
#27750=CARTESIAN_POINT('Ctrl Pts',(40.0554430041532,46.8202500311042,47.6911925591568));
#27751=CARTESIAN_POINT('Ctrl Pts',(40.0671786223162,46.8159934434557,47.6123237804389));
#27752=CARTESIAN_POINT('Ctrl Pts',(40.0828950922958,46.8117368558072,47.5341510034429));
#27753=CARTESIAN_POINT('Ctrl Pts',(40.0981734160342,46.8075989339839,47.4581575395153));
#27754=CARTESIAN_POINT('Ctrl Pts',(40.1172134465915,46.8034610121605,47.3828222978298));
#27755=CARTESIAN_POINT('Ctrl Pts',(40.1399357060372,46.7993230903372,47.3085523678148));
#27756=CARTESIAN_POINT('Ctrl Pts',(40.1626453859003,46.7951874593657,47.2343235553977));
#27757=CARTESIAN_POINT('Ctrl Pts',(40.189033110172,46.7910518283942,47.1611593525195));
#27758=CARTESIAN_POINT('Ctrl Pts',(40.2189688712524,46.7869161974227,47.0894541986622));
#27759=CARTESIAN_POINT('Ctrl Pts',(40.2488982284564,46.7827814511479,47.0177643840154));
#27760=CARTESIAN_POINT('Ctrl Pts',(40.2823739274349,46.7786467048732,46.9475334505543));
#27761=CARTESIAN_POINT('Ctrl Pts',(40.3192175308638,46.7745119585984,46.8791366019735));
#27762=CARTESIAN_POINT('Ctrl Pts',(40.35795205641,46.7701650049809,46.8072294259084));
#27763=CARTESIAN_POINT('Ctrl Pts',(40.4004092074394,46.7658180513634,46.7373501821476));
#27764=CARTESIAN_POINT('Ctrl Pts',(40.4463276425709,46.7614710977458,46.6699042287424));
#27765=CARTESIAN_POINT('Ctrl Pts',(40.4900580006794,46.757331282488,46.6056721684177));
#27766=CARTESIAN_POINT('Ctrl Pts',(40.5369269476158,46.7531914672301,46.5436471628575));
#27767=CARTESIAN_POINT('Ctrl Pts',(40.5866664300395,46.7490516519722,46.4841465094033));
#27768=CARTESIAN_POINT('Ctrl Pts',(40.6364392548573,46.7449090616281,46.4246059702458));
#27769=CARTESIAN_POINT('Ctrl Pts',(40.6890861058771,46.7407664712841,46.3675935029111));
#27770=CARTESIAN_POINT('Ctrl Pts',(40.7443021294053,46.73662388094,46.313389493034));
#27771=CARTESIAN_POINT('Ctrl Pts',(40.7996058292231,46.7324747126693,46.2590994138211));
#27772=CARTESIAN_POINT('Ctrl Pts',(40.8574864657606,46.7283255443986,46.2076270003678));
#27773=CARTESIAN_POINT('Ctrl Pts',(40.9176070793061,46.7241763761279,46.1592116717078));
#27774=CARTESIAN_POINT('Ctrl Pts',(40.9264355250731,46.723567089148,46.1521020951723));
#27775=CARTESIAN_POINT('Ctrl Pts',(40.9353122254245,46.7229578021681,46.1450583620089));
#27776=CARTESIAN_POINT('Ctrl Pts',(40.9442360662148,46.7223485151882,46.1380811483875));
#27777=CARTESIAN_POINT('Ctrl Pts',(41.0063218352461,46.71810952756,46.0895386336163));
#27778=CARTESIAN_POINT('Ctrl Pts',(41.0709556443962,46.7138705399317,46.0440130955615));
#27779=CARTESIAN_POINT('Ctrl Pts',(41.1378123220411,46.7096315523034,46.0017826178044));
#27780=CARTESIAN_POINT('Ctrl Pts',(41.2045716917168,46.7053987343996,45.9596136052917));
#27781=CARTESIAN_POINT('Ctrl Pts',(41.2735471120876,46.7011659164958,45.9207303769664));
#27782=CARTESIAN_POINT('Ctrl Pts',(41.3443813107765,46.6969330985919,45.885370097662));
#27783=CARTESIAN_POINT('Ctrl Pts',(41.4151318134713,46.6927052820844,45.8500515992174));
#27784=CARTESIAN_POINT('Ctrl Pts',(41.48773631278,46.6884774655769,45.8182479854144));
#27785=CARTESIAN_POINT('Ctrl Pts',(41.5618109117649,46.6842496490694,45.7901517035634));
#27786=CARTESIAN_POINT('Ctrl Pts',(41.6358374850734,46.6800245736331,45.7620736377131));
#27787=CARTESIAN_POINT('Ctrl Pts',(41.7113318293812,46.6757994981968,45.7376982985315));
#27788=CARTESIAN_POINT('Ctrl Pts',(41.7878890338709,46.6715744227605,45.7171704824835));
#27789=CARTESIAN_POINT('Ctrl Pts',(41.8644204008238,46.6673507732584,45.6966495944342));
#27790=CARTESIAN_POINT('Ctrl Pts',(41.9420134635277,46.6631271237564,45.6799737721795));
#27791=CARTESIAN_POINT('Ctrl Pts',(42.020248499192,46.6589034742543,45.6672378521302));
#27792=CARTESIAN_POINT('Ctrl Pts',(42.0984814496739,46.6546799373243,45.6545022715288));
#27793=CARTESIAN_POINT('Ctrl Pts',(42.177355876536,46.6504564003943,45.645706458409));
#27794=CARTESIAN_POINT('Ctrl Pts',(42.2564436959489,46.6462328634644,45.6408938072933));
#27795=CARTESIAN_POINT('Ctrl Pts',(42.3356086411391,46.6420052077766,45.6360764629206));
#27796=CARTESIAN_POINT('Ctrl Pts',(42.4149869259069,46.6377775520889,45.6352500688633));
#27797=CARTESIAN_POINT('Ctrl Pts',(42.4941478032849,46.6335498964012,45.63840591294));
#27798=CARTESIAN_POINT('Ctrl Pts',(42.5733457062223,46.6293202633312,45.6415632330854));
#27799=CARTESIAN_POINT('Ctrl Pts',(42.6523255319369,46.6250906302612,45.6487064602432));
#27800=CARTESIAN_POINT('Ctrl Pts',(42.7306615533172,46.6208609971912,45.6597749300425));
#27801=CARTESIAN_POINT('Ctrl Pts',(42.8091383540487,46.6166237629565,45.6708632912272));
#27802=CARTESIAN_POINT('Ctrl Pts',(42.8869685772243,46.6123865287218,45.6858909022939));
#27803=CARTESIAN_POINT('Ctrl Pts',(42.9637367902861,46.6081492944871,45.7047459242651));
#27804=CARTESIAN_POINT('Ctrl Pts',(43.0363670745302,46.6041404539189,45.7225846305548));
#27805=CARTESIAN_POINT('Ctrl Pts',(43.1080465470771,46.6001316133506,45.7438487227785));
#27806=CARTESIAN_POINT('Ctrl Pts',(43.1784391621289,46.5961227727824,45.7684035060603));
#27807=CARTESIAN_POINT('Ctrl Pts',(43.2529342276332,46.59188029876,45.7943893312448));
#27808=CARTESIAN_POINT('Ctrl Pts',(43.3262630340169,46.5876378247375,45.8241569755966));
#27809=CARTESIAN_POINT('Ctrl Pts',(43.3980154719991,46.5833953507151,45.8575818432084));
#27810=CARTESIAN_POINT('Ctrl Pts',(43.4696664379429,46.5791588763841,45.8909594414932));
#27811=CARTESIAN_POINT('Ctrl Pts',(43.5397450425771,46.5749224020531,45.9279837952047));
#27812=CARTESIAN_POINT('Ctrl Pts',(43.6078584146434,46.5706859277222,45.9684812353623));
#27813=CARTESIAN_POINT('Ctrl Pts',(43.6758952397014,46.5664542144157,46.0089331637827));
#27814=CARTESIAN_POINT('Ctrl Pts',(43.741970821366,46.5622225011092,46.0528501842038));
#27815=CARTESIAN_POINT('Ctrl Pts',(43.8057156423378,46.5579907878028,46.1000121122));
#27816=CARTESIAN_POINT('Ctrl Pts',(43.8694213494987,46.5537616710749,46.1471451016455));
#27817=CARTESIAN_POINT('Ctrl Pts',(43.9307987599507,46.5495325543469,46.1975187689448));
#27818=CARTESIAN_POINT('Ctrl Pts',(43.9895072149921,46.545303437619,46.2508695719335));
#27819=CARTESIAN_POINT('Ctrl Pts',(44.0481978050543,46.5410756078111,46.3042041402762));
#27820=CARTESIAN_POINT('Ctrl Pts',(44.1042207068267,46.5368477780031,46.3605137309542));
#27821=CARTESIAN_POINT('Ctrl Pts',(44.1572693933893,46.5326199481951,46.4194954223548));
#27822=CARTESIAN_POINT('Ctrl Pts',(44.2103183446974,46.5283920972877,46.4784774081104));
#27823=CARTESIAN_POINT('Ctrl Pts',(44.2603927397304,46.5241642463803,46.5401311725002));
#27824=CARTESIAN_POINT('Ctrl Pts',(44.3072248952418,46.5199363954729,46.604119045237));
#27825=CARTESIAN_POINT('Ctrl Pts',(44.3541046881307,46.5157042440218,46.6681720060403));
#27826=CARTESIAN_POINT('Ctrl Pts',(44.3977353768617,46.5114720925707,46.734563439658));
#27827=CARTESIAN_POINT('Ctrl Pts',(44.437891733117,46.5072399411196,46.8029253469423));
#27828=CARTESIAN_POINT('Ctrl Pts',(44.4780678610049,46.5030057059002,46.8713209133193));
#27829=CARTESIAN_POINT('Ctrl Pts',(44.5147660320134,46.4987714706807,46.9416884710826));
#27830=CARTESIAN_POINT('Ctrl Pts',(44.547807487796,46.4945372354613,47.0136362555997));
#27831=CARTESIAN_POINT('Ctrl Pts',(44.5809092578639,46.4902952710161,47.0857153744996));
#27832=CARTESIAN_POINT('Ctrl Pts',(44.6103408005741,46.4860533065709,47.1593800489095));
#27833=CARTESIAN_POINT('Ctrl Pts',(44.6359720053084,46.4818113421257,47.2342195925873));
#27834=CARTESIAN_POINT('Ctrl Pts',(44.6599686046557,46.477839904876,47.304286316473));
#27835=CARTESIAN_POINT('Ctrl Pts',(44.6806345420483,46.4738684676263,47.3753823760291));
#27836=CARTESIAN_POINT('Ctrl Pts',(44.6979037062447,46.4698970303766,47.4471627746552));
#27837=CARTESIAN_POINT('Ctrl Pts',(44.7163012908706,46.465666087173,47.5236335258272));
#27838=CARTESIAN_POINT('Ctrl Pts',(44.7309131367711,46.4614351439694,47.601172016668));
#27839=CARTESIAN_POINT('Ctrl Pts',(44.7416203849523,46.4572042007659,47.6793687262976));
#27840=CARTESIAN_POINT('Ctrl Pts',(44.7523119331019,46.4529794613917,47.757450776139));
#27841=CARTESIAN_POINT('Ctrl Pts',(44.7591101888584,46.4487547220176,47.8361886662048));
#27842=CARTESIAN_POINT('Ctrl Pts',(44.7619468026331,46.4445299826435,47.9151604901508));
#27843=CARTESIAN_POINT('Ctrl Pts',(44.7647800501454,46.4403102568462,47.994038596764));
#27844=CARTESIAN_POINT('Ctrl Pts',(44.7636609808645,46.4360905310489,48.0731496179231));
#27845=CARTESIAN_POINT('Ctrl Pts',(44.7585729628223,46.4318708052516,48.1520658408181));
#27846=CARTESIAN_POINT('Ctrl Pts',(44.753488254408,46.4276538242799,48.2309307306931));
#27847=CARTESIAN_POINT('Ctrl Pts',(44.7444397511366,46.4234368433081,48.3096006055514));
#27848=CARTESIAN_POINT('Ctrl Pts',(44.7314628968383,46.4192198623364,48.3876482962253));
#27849=CARTESIAN_POINT('Ctrl Pts',(44.7184904069863,46.4150042996427,48.4656697374749));
#27850=CARTESIAN_POINT('Ctrl Pts',(44.7015922664761,46.410788736949,48.5430689462409));
#27851=CARTESIAN_POINT('Ctrl Pts',(44.6808555329728,46.4065731742553,48.6194259266509));
#27852=CARTESIAN_POINT('Ctrl Pts',(44.6601192594321,46.4023577050672,48.6957812133826));
#27853=CARTESIAN_POINT('Ctrl Pts',(44.6355446866869,46.3981422358791,48.7710938639706));
#27854=CARTESIAN_POINT('Ctrl Pts',(44.607269160561,46.393926766691,48.844957569193));
#27855=CARTESIAN_POINT('Ctrl Pts',(44.5789654189238,46.3897070909811,48.9188949813449));
#27856=CARTESIAN_POINT('Ctrl Pts',(44.5469535149943,46.3854874152712,48.9913801193012));
#27857=CARTESIAN_POINT('Ctrl Pts',(44.5114193257397,46.3812677395612,49.0620258338633));
#27858=CARTESIAN_POINT('Ctrl Pts',(44.475868192399,46.3770460517455,49.1327052350548));
#27859=CARTESIAN_POINT('Ctrl Pts',(44.4367916606371,46.3728243639297,49.2015430558924));
#27860=CARTESIAN_POINT('Ctrl Pts',(44.3944207928808,46.368602676114,49.2681782768304));
#27861=CARTESIAN_POINT('Ctrl Pts',(44.351972081892,46.3643732322658,49.3349359191698));
#27862=CARTESIAN_POINT('Ctrl Pts',(44.3062172138798,46.3601437884176,49.3994824907559));
#27863=CARTESIAN_POINT('Ctrl Pts',(44.2574295424309,46.3559143445693,49.4614875763431));
#27864=CARTESIAN_POINT('Ctrl Pts',(44.2103539895295,46.3518333257031,49.5213167012023));
#27865=CARTESIAN_POINT('Ctrl Pts',(44.160455266942,46.347752306837,49.5787795148342));
#27866=CARTESIAN_POINT('Ctrl Pts',(44.1080108339183,46.3436712879708,49.6336123873545));
#27867=CARTESIAN_POINT('Ctrl Pts',(44.0535718997629,46.3394350648955,49.6905305951521));
#27868=CARTESIAN_POINT('Ctrl Pts',(43.9961814398514,46.3351988418203,49.7448325979865));
#27869=CARTESIAN_POINT('Ctrl Pts',(43.936120942695,46.3309626187451,49.7961967849637));
#27870=CARTESIAN_POINT('Ctrl Pts',(43.876147494277,46.3267325354438,49.8474865272078));
#27871=CARTESIAN_POINT('Ctrl Pts',(43.8135120470264,46.3225024521424,49.895846606812));
#27872=CARTESIAN_POINT('Ctrl Pts',(43.7485337409041,46.3182723688411,49.9409912906923));
#27873=CARTESIAN_POINT('Ctrl Pts',(43.6836313490918,46.3140472275562,49.9860832319308));
#27874=CARTESIAN_POINT('Ctrl Pts',(43.6163919210402,46.3098220862713,50.0279669762023));
#27875=CARTESIAN_POINT('Ctrl Pts',(43.5471673742967,46.3055969449864,50.0663972164735));
#27876=CARTESIAN_POINT('Ctrl Pts',(43.4779871230811,46.3013745072925,50.104802865933));
#27877=CARTESIAN_POINT('Ctrl Pts',(43.4068246834519,46.2971520695987,50.139759170389));
#27878=CARTESIAN_POINT('Ctrl Pts',(43.3340596051936,46.2929296319048,50.1710649679007));
#27879=CARTESIAN_POINT('Ctrl Pts',(43.2613183859169,46.2887085787083,50.2023605005372));
#27880=CARTESIAN_POINT('Ctrl Pts',(43.1869760021201,46.2844875255119,50.2300077177604));
#27881=CARTESIAN_POINT('Ctrl Pts',(43.1114338203614,46.2802664723154,50.2538527813826));
#27882=CARTESIAN_POINT('Ctrl Pts',(43.0358928401895,46.2760454862598,50.2776974657211));
#27883=CARTESIAN_POINT('Ctrl Pts',(42.9591525477985,46.2718245002041,50.297739976718));
#27884=CARTESIAN_POINT('Ctrl Pts',(42.8816299450365,46.2676035141484,50.313876193089));
#27885=CARTESIAN_POINT('Ctrl Pts',(42.8040300298219,46.2633783185491,50.3300285019339));
#27886=CARTESIAN_POINT('Ctrl Pts',(42.7256467061207,46.2591531229497,50.3422666381228));
#27887=CARTESIAN_POINT('Ctrl Pts',(42.6469070693722,46.2549279273503,50.3505376704052));
#27888=CARTESIAN_POINT('Ctrl Pts',(42.5681297338577,46.2507007088224,50.3588126626718));
#27889=CARTESIAN_POINT('Ctrl Pts',(42.4889962145655,46.2464734902945,50.3631167416678));
#27890=CARTESIAN_POINT('Ctrl Pts',(42.4099360502211,46.2422462717666,50.3634491142832));
#27891=CARTESIAN_POINT('Ctrl Pts',(42.3307317140436,46.238011344605,50.3637820930037));
#27892=CARTESIAN_POINT('Ctrl Pts',(42.2516014700193,46.2337764174434,50.3601289143807));
#27893=CARTESIAN_POINT('Ctrl Pts',(42.1729719753434,46.2295414902819,50.352540906535));
#27894=CARTESIAN_POINT('Ctrl Pts',(42.0981105523535,46.2255095087095,50.3453165301439));
#27895=CARTESIAN_POINT('Ctrl Pts',(42.0237033312112,46.2214775271372,50.3345258847114));
#27896=CARTESIAN_POINT('Ctrl Pts',(41.9501083644202,46.2174455455649,50.3202560111193));
#27897=CARTESIAN_POINT('Ctrl Pts',(41.8727846904032,46.2132092826473,50.3052631508462));
#27898=CARTESIAN_POINT('Ctrl Pts',(41.7960649488134,46.2089730197297,50.2863724086812));
#27899=CARTESIAN_POINT('Ctrl Pts',(41.7203719128066,46.204736756812,50.2636466385012));
#27900=CARTESIAN_POINT('Ctrl Pts',(41.6447882987843,46.2005066178435,50.2409537207342));
#27901=CARTESIAN_POINT('Ctrl Pts',(41.570228888495,46.1962764788749,50.214436918126));
#27902=CARTESIAN_POINT('Ctrl Pts',(41.4971066353727,46.1920463399063,50.1842101577028));
#27903=CARTESIAN_POINT('Ctrl Pts',(41.4240693987772,46.1878211191631,50.1540185408109));
#27904=CARTESIAN_POINT('Ctrl Pts',(41.3524664302149,46.1835958984199,50.1201257160476));
#27905=CARTESIAN_POINT('Ctrl Pts',(41.2826944044649,46.1793706776768,50.0826950441882));
#27906=CARTESIAN_POINT('Ctrl Pts',(41.2129667851216,46.1751481460754,50.0452881950803));
#27907=CARTESIAN_POINT('Ctrl Pts',(41.1450682079941,46.170925614474,50.0043481891993));
#27908=CARTESIAN_POINT('Ctrl Pts',(41.0793731559787,46.1667030828726,49.9600855031733));
#27909=CARTESIAN_POINT('Ctrl Pts',(41.0136994210225,46.1624819214194,49.9158371797253));
#27910=CARTESIAN_POINT('Ctrl Pts',(40.9502281801745,46.1582607599662,49.8682685789824));
#27911=CARTESIAN_POINT('Ctrl Pts',(40.8893059061183,46.1540395985131,49.8176341203914));
#27912=CARTESIAN_POINT('Ctrl Pts',(40.8283843952242,46.1498184899376,49.7670002960889));
#27913=CARTESIAN_POINT('Ctrl Pts',(40.7700121475917,46.1455973813621,49.7133009911954));
#27914=CARTESIAN_POINT('Ctrl Pts',(40.7145022701864,46.1413762727866,49.656830662347));
#27915=CARTESIAN_POINT('Ctrl Pts',(40.6589367479696,46.1371509328419,49.600303725901));
#27916=CARTESIAN_POINT('Ctrl Pts',(40.6062396574617,46.1329255928971,49.5410005519791));
#27917=CARTESIAN_POINT('Ctrl Pts',(40.556686505751,46.1287002529523,49.4792517712748));
#27918=CARTESIAN_POINT('Ctrl Pts',(40.5071094875762,46.1244728779417,49.4174732502814));
#27919=CARTESIAN_POINT('Ctrl Pts',(40.4606796999622,46.1202455029312,49.3532471567354));
#27920=CARTESIAN_POINT('Ctrl Pts',(40.4176301137086,46.1160181279206,49.2869343708305));
#27921=CARTESIAN_POINT('Ctrl Pts',(40.3745018326491,46.1117830252526,49.2205003649032));
#27922=CARTESIAN_POINT('Ctrl Pts',(40.334766336029,46.1075479225846,49.1519724513163));
#27923=CARTESIAN_POINT('Ctrl Pts',(40.2986111943904,46.1033128199166,49.0817372733518));
#27924=CARTESIAN_POINT('Ctrl Pts',(40.2641984329235,46.0992818143307,49.0148868527386));
#27925=CARTESIAN_POINT('Ctrl Pts',(40.2330290190821,46.0952508087449,48.9464902572754));
#27926=CARTESIAN_POINT('Ctrl Pts',(40.2052232828249,46.0912198031591,48.8768954342714));
#27927=CARTESIAN_POINT('Ctrl Pts',(40.1722934482226,46.0864459555618,48.7944755339493));
#27928=CARTESIAN_POINT('Ctrl Pts',(40.1439755541144,46.0816721079645,48.7101123332651));
#27929=CARTESIAN_POINT('Ctrl Pts',(40.120474792554,46.0768982603672,48.6243038278903));
#27930=CARTESIAN_POINT('Ctrl Pts',(40.0970606245411,46.0721420030253,48.5388115021787));
#27931=CARTESIAN_POINT('Ctrl Pts',(40.0784282945429,46.0673857456834,48.451884719801));
#27932=CARTESIAN_POINT('Ctrl Pts',(40.0647341399482,46.0626294883415,48.3640381899976));
#27933=CARTESIAN_POINT('Ctrl Pts',(40.0511258291351,46.0579030462842,48.2767423388258));
#27934=CARTESIAN_POINT('Ctrl Pts',(40.0423940921215,46.0531766042269,48.1885384689497));
#27935=CARTESIAN_POINT('Ctrl Pts',(40.0386443754894,46.0484501621696,48.0999502650926));
#27936=CARTESIAN_POINT('Ctrl Pts',(40.0372564615572,46.0467007246988,48.0671603733686));
#27937=CARTESIAN_POINT('Ctrl Pts',(40.0365506126886,46.044951287228,48.0343179932933));
#27938=CARTESIAN_POINT('Ctrl Pts',(40.0365304449332,46.0432018497572,48.0014502318932));
#27939=CARTESIAN_POINT('',(40.0365307281522,45.2494518497012,47.9981447557607));
#27940=CARTESIAN_POINT('Ctrl Pts',(40.0365304449329,46.0432018497283,48.0014502313506));
#27941=CARTESIAN_POINT('Ctrl Pts',(40.0364813749074,46.0389453039821,47.92147987956));
#27942=CARTESIAN_POINT('Ctrl Pts',(40.0404954577654,46.0346887582359,47.8414969742251));
#27943=CARTESIAN_POINT('Ctrl Pts',(40.0485500040157,46.0304322124897,47.7619383330201));
#27944=CARTESIAN_POINT('Ctrl Pts',(40.0566059305006,46.0261749373378,47.6823660585711));
#27945=CARTESIAN_POINT('Ctrl Pts',(40.0687036493595,46.0219176621859,47.6032186482942));
#27946=CARTESIAN_POINT('Ctrl Pts',(40.0847686849002,46.0176603870341,47.5249269545835));
#27947=CARTESIAN_POINT('Ctrl Pts',(40.1013302642617,46.0132715265106,47.444215393414));
#27948=CARTESIAN_POINT('Ctrl Pts',(40.1221083414989,46.0088826659872,47.3644138266163));
#27949=CARTESIAN_POINT('Ctrl Pts',(40.146965226529,46.0044938054638,47.285979866929));
#27950=CARTESIAN_POINT('Ctrl Pts',(40.1711228133691,46.0002284166553,47.2097524880741));
#27951=CARTESIAN_POINT('Ctrl Pts',(40.1991325077043,45.9959630278468,47.1348171927995));
#27952=CARTESIAN_POINT('Ctrl Pts',(40.2308187522828,45.9916976390382,47.0615741076399));
#27953=CARTESIAN_POINT('Ctrl Pts',(40.2638808462144,45.9872470426574,46.9851507323358));
#27954=CARTESIAN_POINT('Ctrl Pts',(40.3009457822569,45.9827964462766,46.9105703714617));
#27955=CARTESIAN_POINT('Ctrl Pts',(40.3417616972024,45.9783458498957,46.8382575458404));
#27956=CARTESIAN_POINT('Ctrl Pts',(40.3825776121478,45.9738952535149,46.7659447202191));
#27957=CARTESIAN_POINT('Ctrl Pts',(40.4271441402953,45.969444657134,46.6958998578033));
#27958=CARTESIAN_POINT('Ctrl Pts',(40.475160823061,45.9649940607532,46.6285100861397));
#27959=CARTESIAN_POINT('Ctrl Pts',(40.5208583018578,45.9607584280099,46.5643752379089));
#27960=CARTESIAN_POINT('Ctrl Pts',(40.5698515301063,45.9565227952666,46.5024049717847));
#27961=CARTESIAN_POINT('Ctrl Pts',(40.6219082101963,45.9522871625233,46.4429579235189));
#27962=CARTESIAN_POINT('Ctrl Pts',(40.6738894361484,45.9480576691653,46.3835970414428));
#27963=CARTESIAN_POINT('Ctrl Pts',(40.7289249895938,45.9438281758073,46.3267524645397));
#27964=CARTESIAN_POINT('Ctrl Pts',(40.7867401564744,45.9395986824493,46.2727527339238));
#27965=CARTESIAN_POINT('Ctrl Pts',(40.844487815944,45.935374127625,46.2188160556557));
#27966=CARTESIAN_POINT('Ctrl Pts',(40.9050082980373,45.9311495728006,46.1677179413873));
#27967=CARTESIAN_POINT('Ctrl Pts',(40.9679886427238,45.9269250179762,46.1197516351472));
#27968=CARTESIAN_POINT('Ctrl Pts',(41.030928717424,45.922703164356,46.0718159988326));
#27969=CARTESIAN_POINT('Ctrl Pts',(41.0963251605837,45.9184813107357,46.0270084796002));
#27970=CARTESIAN_POINT('Ctrl Pts',(41.1638313257595,45.9142594571154,45.9855826029031));
#27971=CARTESIAN_POINT('Ctrl Pts',(41.2313154046507,45.9100389847773,45.9441702796897));
#27972=CARTESIAN_POINT('Ctrl Pts',(41.3009074352502,45.9058185124392,45.9061376473717));
#27973=CARTESIAN_POINT('Ctrl Pts',(41.3722323850144,45.901598040101,45.8716945307389));
#27974=CARTESIAN_POINT('Ctrl Pts',(41.4435562684949,45.8973776308575,45.8372519290189));
#27975=CARTESIAN_POINT('Ctrl Pts',(41.5166125964427,45.893157221614,45.8063989391994));
#27976=CARTESIAN_POINT('Ctrl Pts',(41.5910037258426,45.8889368123705,45.7792984285818));
#27977=CARTESIAN_POINT('Ctrl Pts',(41.6654692406122,45.8847121830445,45.7521708195517));
#27978=CARTESIAN_POINT('Ctrl Pts',(41.7412717810415,45.8804875537185,45.7288033462231));
#27979=CARTESIAN_POINT('Ctrl Pts',(41.8179963668233,45.8762629243925,45.7093096647803));
#27980=CARTESIAN_POINT('Ctrl Pts',(41.8947577790358,45.8720362673199,45.6898066267185));
#27981=CARTESIAN_POINT('Ctrl Pts',(41.9724416575127,45.8678096102473,45.6741811772827));
#27982=CARTESIAN_POINT('Ctrl Pts',(42.0506231235046,45.8635829531747,45.6624957242669));
#27983=CARTESIAN_POINT('Ctrl Pts',(42.1289474554155,45.8593485724654,45.6507889176867));
#27984=CARTESIAN_POINT('Ctrl Pts',(42.2077707234904,45.855114191756,45.6430365404894));
#27985=CARTESIAN_POINT('Ctrl Pts',(42.2866634220723,45.8508798110466,45.6392490048708));
#27986=CARTESIAN_POINT('Ctrl Pts',(42.3618816895894,45.8468426468135,45.6356378738978));
#27987=CARTESIAN_POINT('Ctrl Pts',(42.4371627077019,45.8428054825804,45.6356304479901));
#27988=CARTESIAN_POINT('Ctrl Pts',(42.5121381794019,45.8387683183473,45.6391917761876));
#27989=CARTESIAN_POINT('Ctrl Pts',(42.5907984845178,45.8345327388547,45.6429281336426));
#27990=CARTESIAN_POINT('Ctrl Pts',(42.6694212910057,45.8302971593621,45.6506072440683));
#27991=CARTESIAN_POINT('Ctrl Pts',(42.747579313366,45.8260615798695,45.662227756641));
#27992=CARTESIAN_POINT('Ctrl Pts',(42.8256240675031,45.8218321386664,45.6738314285264));
#27993=CARTESIAN_POINT('Ctrl Pts',(42.9032049148108,45.8176026974633,45.689365091158));
#27994=CARTESIAN_POINT('Ctrl Pts',(42.9798969335152,45.8133732562601,45.7087754393339));
#27995=CARTESIAN_POINT('Ctrl Pts',(43.0564994371497,45.8091487516688,45.7281631317146));
#27996=CARTESIAN_POINT('Ctrl Pts',(43.1322147211502,45.8049242470775,45.7514184033096));
#27997=CARTESIAN_POINT('Ctrl Pts',(43.206626859008,45.8006997424861,45.7784366875493));
#27998=CARTESIAN_POINT('Ctrl Pts',(43.2809914377693,45.7964779379062,45.8054377035688));
#27999=CARTESIAN_POINT('Ctrl Pts',(43.3540540835199,45.7922561333263,45.8361967989557));
#28000=CARTESIAN_POINT('Ctrl Pts',(43.4254140506975,45.7880343287464,45.8705595886402));
#28001=CARTESIAN_POINT('Ctrl Pts',(43.4967506918237,45.7838139041844,45.9049111458616));
#28002=CARTESIAN_POINT('Ctrl Pts',(43.5663853370023,45.7795934796223,45.9428638548478));
#28003=CARTESIAN_POINT('Ctrl Pts',(43.6339386382233,45.7753730550603,45.9842158156193));
#28004=CARTESIAN_POINT('Ctrl Pts',(43.7014909509352,45.7711526922558,46.0255671712864));
#28005=CARTESIAN_POINT('Ctrl Pts',(43.7669615806392,45.7669323294514,46.0703174336924));
#28006=CARTESIAN_POINT('Ctrl Pts',(43.8299984406264,45.7627119666469,46.1182202836926));
#28007=CARTESIAN_POINT('Ctrl Pts',(43.8930983699963,45.7584873813022,46.1661710612574));
#28008=CARTESIAN_POINT('Ctrl Pts',(43.9537592908116,45.7542627959576,46.2172804427092));
#28009=CARTESIAN_POINT('Ctrl Pts',(44.0116611256183,45.7500382106129,46.2712609054369));
#28010=CARTESIAN_POINT('Ctrl Pts',(44.0695907699354,45.7458115962539,46.3252672942902));
#28011=CARTESIAN_POINT('Ctrl Pts',(44.1247583611697,45.741584981895,46.3821471740817));
#28012=CARTESIAN_POINT('Ctrl Pts',(44.1768815691912,45.737358367536,46.4415769733578));
#28013=CARTESIAN_POINT('Ctrl Pts',(44.2291000594114,45.733124026847,46.501115411418));
#28014=CARTESIAN_POINT('Ctrl Pts',(44.2782627537765,45.728889686158,46.5632127143961));
#28015=CARTESIAN_POINT('Ctrl Pts',(44.3241285495196,45.7246553454689,46.6275132912033));
#28016=CARTESIAN_POINT('Ctrl Pts',(44.3678631671639,45.7206177556265,46.6888261082035));
#28017=CARTESIAN_POINT('Ctrl Pts',(44.408600301503,45.716580165784,46.7521416755179));
#28018=CARTESIAN_POINT('Ctrl Pts',(44.4461700576661,45.7125425759415,46.8171312262086));
#28019=CARTESIAN_POINT('Ctrl Pts',(44.4855806562007,45.70830715233,46.8853051339683));
#28020=CARTESIAN_POINT('Ctrl Pts',(44.5216553535162,45.7040717287186,46.955580438681));
#28021=CARTESIAN_POINT('Ctrl Pts',(44.554164114165,45.6998363051072,47.0275970947473));
#28022=CARTESIAN_POINT('Ctrl Pts',(44.586625737438,45.6956070228173,47.0995093273874));
#28023=CARTESIAN_POINT('Ctrl Pts',(44.6155315003955,45.6913777405275,47.173157473115));
#28024=CARTESIAN_POINT('Ctrl Pts',(44.6406963388631,45.6871484582376,47.2481553631864));
#28025=CARTESIAN_POINT('Ctrl Pts',(44.6658317809674,45.6829241163935,47.3230656443018));
#28026=CARTESIAN_POINT('Ctrl Pts',(44.6872348339817,45.6786997745494,47.3993220938773));
#28027=CARTESIAN_POINT('Ctrl Pts',(44.704768410672,45.6744754327053,47.4765183727499));
#28028=CARTESIAN_POINT('Ctrl Pts',(44.7222907712953,45.6702537931336,47.553665269876));
#28029=CARTESIAN_POINT('Ctrl Pts',(44.7359484647868,45.666032153562,47.631750346571));
#28030=CARTESIAN_POINT('Ctrl Pts',(44.7456545142861,45.6618105139903,47.7103530761266));
#28031=CARTESIAN_POINT('Ctrl Pts',(44.7553573862834,45.657590256471,47.7889300732429));
#28032=CARTESIAN_POINT('Ctrl Pts',(44.7611111255918,45.6533699989517,47.8680239212373));
#28033=CARTESIAN_POINT('Ctrl Pts',(44.762880292075,45.6491497414323,47.9472063808419));
#28034=CARTESIAN_POINT('Ctrl Pts',(44.7646494319101,45.6449295474805,48.0263876477634));
#28035=CARTESIAN_POINT('Ctrl Pts',(44.7624341090695,45.6407093535286,48.1056570543583));
#28036=CARTESIAN_POINT('Ctrl Pts',(44.7562509892401,45.6364891595768,48.1845852556551));
#28037=CARTESIAN_POINT('Ctrl Pts',(44.7500616853169,45.6322647447663,48.2635923975843));
#28038=CARTESIAN_POINT('Ctrl Pts',(44.7398966937245,45.6280403299558,48.3422571834517));
#28039=CARTESIAN_POINT('Ctrl Pts',(44.7258246503668,45.6238159151453,48.4201548960159));
#28040=CARTESIAN_POINT('Ctrl Pts',(44.7117458521016,45.6195894725177,48.4980900012906));
#28041=CARTESIAN_POINT('Ctrl Pts',(44.6937563726085,45.61536302989,48.575256841995));
#28042=CARTESIAN_POINT('Ctrl Pts',(44.6719755873081,45.6111365872623,48.6512429435902));
#28043=CARTESIAN_POINT('Ctrl Pts',(44.6501549847554,45.606902418314,48.7273679546755));
#28044=CARTESIAN_POINT('Ctrl Pts',(44.6245293791978,45.6026682493656,48.8023074681743));
#28045=CARTESIAN_POINT('Ctrl Pts',(44.5952673796896,45.5984340804172,48.8756663591636));
#28046=CARTESIAN_POINT('Ctrl Pts',(44.5673536082888,45.5943949981233,48.9456452856793));
#28047=CARTESIAN_POINT('Ctrl Pts',(44.5361313352964,45.5903559158295,49.014185724706));
#28048=CARTESIAN_POINT('Ctrl Pts',(44.5017853702595,45.5863168335356,49.0809665574213));
#28049=CARTESIAN_POINT('Ctrl Pts',(44.4657689987264,45.5820813115931,49.1509952574382));
#28050=CARTESIAN_POINT('Ctrl Pts',(44.4261804483698,45.5778457896507,49.2193550564107));
#28051=CARTESIAN_POINT('Ctrl Pts',(44.3831981053932,45.5736102677082,49.2856576977037));
#28052=CARTESIAN_POINT('Ctrl Pts',(44.3402780710023,45.5693808857144,49.3518642245573));
#28053=CARTESIAN_POINT('Ctrl Pts',(44.2939742669022,45.5651515037207,49.4160191252013));
#28054=CARTESIAN_POINT('Ctrl Pts',(44.2445113775134,45.560922121727,49.4777578350743));
#28055=CARTESIAN_POINT('Ctrl Pts',(44.1951062482349,45.5566976785788,49.5394244497921));
#28056=CARTESIAN_POINT('Ctrl Pts',(44.1425496563542,45.5524732354305,49.5986801161953));
#28057=CARTESIAN_POINT('Ctrl Pts',(44.0871092040993,45.5482487922823,49.6551897094724));
#28058=CARTESIAN_POINT('Ctrl Pts',(44.0317042035504,45.5440270504778,49.7116631673753));
#28059=CARTESIAN_POINT('Ctrl Pts',(43.9734193305794,45.5398053086733,49.7653937032946));
#28060=CARTESIAN_POINT('Ctrl Pts',(43.9125612275284,45.5355835668688,49.8160806628225));
#28061=CARTESIAN_POINT('Ctrl Pts',(43.8517230359666,45.5313632063293,49.8667510386451));
#28062=CARTESIAN_POINT('Ctrl Pts',(43.7883136464435,45.5271428457898,49.9143795152516));
#28063=CARTESIAN_POINT('Ctrl Pts',(43.7226740674798,45.5229224852502,49.9587046107355));
#28064=CARTESIAN_POINT('Ctrl Pts',(43.6570354671272,45.5187021876314,50.0030290453829));
#28065=CARTESIAN_POINT('Ctrl Pts',(43.5891671331395,45.5144818900127,50.0440499352498));
#28066=CARTESIAN_POINT('Ctrl Pts',(43.5194391916917,45.5102615923939,50.081549023445));
#28067=CARTESIAN_POINT('Ctrl Pts',(43.4496415081877,45.5060370736232,50.1190856183191));
#28068=CARTESIAN_POINT('Ctrl Pts',(43.3779809160197,45.5018125548525,50.1530931520212));
#28069=CARTESIAN_POINT('Ctrl Pts',(43.3048517638537,45.4975880360818,50.1833995800931));
#28070=CARTESIAN_POINT('Ctrl Pts',(43.231687503134,45.4933614891631,50.2137205579695));
#28071=CARTESIAN_POINT('Ctrl Pts',(43.1570537205715,45.4891349422444,50.2403367326149));
#28072=CARTESIAN_POINT('Ctrl Pts',(43.0813619174185,45.4849083953257,50.2631253563141));
#28073=CARTESIAN_POINT('Ctrl Pts',(43.0055317583089,45.4806741227627,50.2859556350103));
#28074=CARTESIAN_POINT('Ctrl Pts',(42.928640170997,45.4764398501998,50.3049442696378));
#28075=CARTESIAN_POINT('Ctrl Pts',(42.8511106996711,45.4722055776368,50.3200193054245));
#28076=CARTESIAN_POINT('Ctrl Pts',(42.7771720069113,45.4681674154678,50.3343961407145));
#28077=CARTESIAN_POINT('Ctrl Pts',(42.7026535677558,45.4641292532988,50.3452138526462));
#28078=CARTESIAN_POINT('Ctrl Pts',(42.6279251674152,45.4600910911298,50.3524541566115));
#28079=CARTESIAN_POINT('Ctrl Pts',(42.549544776891,45.4558555832591,50.3600482955162));
#28080=CARTESIAN_POINT('Ctrl Pts',(42.4706354580106,45.4516200753884,50.3637352971135));
#28081=CARTESIAN_POINT('Ctrl Pts',(42.3916202483146,45.4473845675177,50.3634551446266));
#28082=CARTESIAN_POINT('Ctrl Pts',(42.3127195816137,45.4431551995757,50.3631753982577));
#28083=CARTESIAN_POINT('Ctrl Pts',(42.2337137943035,45.4389258316337,50.3589399197566));
#28084=CARTESIAN_POINT('Ctrl Pts',(42.1550310453491,45.4346964636918,50.3507404476371));
#28085=CARTESIAN_POINT('Ctrl Pts',(42.0764401763512,45.4304720344962,50.3425505502612));
#28086=CARTESIAN_POINT('Ctrl Pts',(41.9981720604984,45.4262476053006,50.3304059060715));
#28087=CARTESIAN_POINT('Ctrl Pts',(41.9206533154213,45.4220231761051,50.3143502753221));
#28088=CARTESIAN_POINT('Ctrl Pts',(41.8431841390787,45.4178014481866,50.2983049112159));
#28089=CARTESIAN_POINT('Ctrl Pts',(41.7664638407974,45.4135797202681,50.2783536191345));
#28090=CARTESIAN_POINT('Ctrl Pts',(41.6909111680883,45.4093579923496,50.254591641375));
#28091=CARTESIAN_POINT('Ctrl Pts',(41.6153832131594,45.4051376456098,50.230837437574));
#28092=CARTESIAN_POINT('Ctrl Pts',(41.5410225726666,45.40091729887,50.2032751643405));
#28093=CARTESIAN_POINT('Ctrl Pts',(41.468233640797,45.3966969521302,50.1720501588954));
#28094=CARTESIAN_POINT('Ctrl Pts',(41.3954457923024,45.3924766682052,50.1408256181967));
#28095=CARTESIAN_POINT('Ctrl Pts',(41.3242300367412,45.3882563842802,50.1059386399121));
#28096=CARTESIAN_POINT('Ctrl Pts',(41.2549701672457,45.3840361003551,50.0675824343911));
#28097=CARTESIAN_POINT('Ctrl Pts',(41.1856410192716,45.3798115950122,50.0291878623589));
#28098=CARTESIAN_POINT('Ctrl Pts',(41.1182720771132,45.3755870896693,49.9873173589389));
#28099=CARTESIAN_POINT('Ctrl Pts',(41.0532213720964,45.3713625843265,49.9422095068046));
#28100=CARTESIAN_POINT('Ctrl Pts',(40.9881394349135,45.3671360507127,49.8970799974734));
#28101=CARTESIAN_POINT('Ctrl Pts',(40.9253783244348,45.3629095170989,49.8487103299414));
#28102=CARTESIAN_POINT('Ctrl Pts',(40.8652638913551,45.3586829834851,49.7973801817427));
#28103=CARTESIAN_POINT('Ctrl Pts',(40.8050395703519,45.3544487238564,49.7459562031092));
#28104=CARTESIAN_POINT('Ctrl Pts',(40.747471936393,45.3502144642278,49.6915612531637));
#28105=CARTESIAN_POINT('Ctrl Pts',(40.6928506369372,45.3459802045991,49.6345126163766));
#28106=CARTESIAN_POINT('Ctrl Pts',(40.6407573763549,45.3419419193074,49.5801043629731));
#28107=CARTESIAN_POINT('Ctrl Pts',(40.5913439603892,45.3379036340156,49.5232829229293));
#28108=CARTESIAN_POINT('Ctrl Pts',(40.5448258364757,45.3338653487239,49.4643494336707));
#28109=CARTESIAN_POINT('Ctrl Pts',(40.4960866490667,45.3296342506682,49.4026020944407));
#28110=CARTESIAN_POINT('Ctrl Pts',(40.4503371423291,45.3254031526125,49.338296520154));
#28111=CARTESIAN_POINT('Ctrl Pts',(40.4078575312895,45.3211720545568,49.2717542314694));
#28112=CARTESIAN_POINT('Ctrl Pts',(40.3654379737318,45.31694693801,49.2053060137055));
#28113=CARTESIAN_POINT('Ctrl Pts',(40.3262793873813,45.3127218214632,49.136627749403));
#28114=CARTESIAN_POINT('Ctrl Pts',(40.2906215083225,45.3084967049163,49.0660735526915));
#28115=CARTESIAN_POINT('Ctrl Pts',(40.2550028702488,45.3042762380498,48.9955969998628));
#28116=CARTESIAN_POINT('Ctrl Pts',(40.2228775010959,45.3000557711832,48.9232490303305));
#28117=CARTESIAN_POINT('Ctrl Pts',(40.1944407853412,45.2958353043166,48.8494109673965));
#28118=CARTESIAN_POINT('Ctrl Pts',(40.1660249639791,45.2916179385146,48.7756271583185));
#28119=CARTESIAN_POINT('Ctrl Pts',(40.1412925829797,45.2874005727126,48.7003558668539));
#28120=CARTESIAN_POINT('Ctrl Pts',(40.1203915607568,45.2831832069106,48.6239998434545));
#28121=CARTESIAN_POINT('Ctrl Pts',(40.0994998459173,45.2789677191335,48.5476778219702));
#28122=CARTESIAN_POINT('Ctrl Pts',(40.082436222452,45.2747522313564,48.4702724813342));
#28123=CARTESIAN_POINT('Ctrl Pts',(40.0692987721116,45.2705367435793,48.3922017685062));
#28124=CARTESIAN_POINT('Ctrl Pts',(40.0561590716584,45.2663205337958,48.3141176841405));
#28125=CARTESIAN_POINT('Ctrl Pts',(40.0469469719495,45.2621043240124,48.2353684624106));
#28126=CARTESIAN_POINT('Ctrl Pts',(40.0417092274347,45.2578881142289,48.1563811783223));
#28127=CARTESIAN_POINT('Ctrl Pts',(40.0382158055873,45.255076026062,48.103698978355));
#28128=CARTESIAN_POINT('Ctrl Pts',(40.0364893083885,45.2522639378952,48.0509110511116));
#28129=CARTESIAN_POINT('Ctrl Pts',(40.0365307281518,45.2494518497283,47.9981447562687));
#28130=CARTESIAN_POINT('',(40.0365300816234,44.4557018497661,47.9993788486445));
#28131=CARTESIAN_POINT('Ctrl Pts',(40.0365307281522,45.2494518497012,47.9981447557607));
#28132=CARTESIAN_POINT('Ctrl Pts',(40.0366033020995,45.2445246297871,47.9056899238653));
#28133=CARTESIAN_POINT('Ctrl Pts',(40.0421048202983,45.239597409873,47.8134622725509));
#28134=CARTESIAN_POINT('Ctrl Pts',(40.0529320912302,45.2346701899588,47.7220383614186));
#28135=CARTESIAN_POINT('Ctrl Pts',(40.0638750024599,45.2296903450405,47.6296380003228));
#28136=CARTESIAN_POINT('Ctrl Pts',(40.0802579395256,45.2247105001222,47.5380587616016));
#28137=CARTESIAN_POINT('Ctrl Pts',(40.1019249589366,45.2197306552039,47.4478754247985));
#28138=CARTESIAN_POINT('Ctrl Pts',(40.1194607788405,45.2157003055753,47.3748871322));
#28139=CARTESIAN_POINT('Ctrl Pts',(40.140456810413,45.2116699559466,47.3028128097879));
#28140=CARTESIAN_POINT('Ctrl Pts',(40.1648076914569,45.207639606318,47.231946756579));
#28141=CARTESIAN_POINT('Ctrl Pts',(40.1903980876707,45.2034041027364,47.1574734602552));
#28142=CARTESIAN_POINT('Ctrl Pts',(40.2197632084637,45.1991685991548,47.084138962129));
#28143=CARTESIAN_POINT('Ctrl Pts',(40.2527822542417,45.1949330955732,47.0123531029762));
#28144=CARTESIAN_POINT('Ctrl Pts',(40.2857534331853,45.1907037320887,46.9406713098784));
#28145=CARTESIAN_POINT('Ctrl Pts',(40.3223678237371,45.1864743686043,46.8705341203382));
#28146=CARTESIAN_POINT('Ctrl Pts',(40.3624554064291,45.1822450051198,46.8023345750545));
#28147=CARTESIAN_POINT('Ctrl Pts',(40.4024961755055,45.178020580616,46.734214672071));
#28148=CARTESIAN_POINT('Ctrl Pts',(40.4460018402179,45.1737961561122,46.6680283193652));
#28149=CARTESIAN_POINT('Ctrl Pts',(40.4927556815083,45.1695717316084,46.6041455840664));
#28150=CARTESIAN_POINT('Ctrl Pts',(40.5394796248446,45.1653500085223,46.5403037002365));
#28151=CARTESIAN_POINT('Ctrl Pts',(40.5894473456508,45.1611282854361,46.4787628877371));
#28152=CARTESIAN_POINT('Ctrl Pts',(40.6423985406384,45.1569065623499,46.4198647048592));
#28153=CARTESIAN_POINT('Ctrl Pts',(40.6953324104342,45.1526862205765,46.360985792978));
#28154=CARTESIAN_POINT('Ctrl Pts',(40.7512475025109,45.1484658788031,46.304748142587));
#28155=CARTESIAN_POINT('Ctrl Pts',(40.8098438798882,45.1442455370297,46.2514594787163));
#28156=CARTESIAN_POINT('Ctrl Pts',(40.8684393833551,45.1400252581988,46.1981716095965));
#28157=CARTESIAN_POINT('Ctrl Pts',(40.9297157445013,45.1358049793678,46.1478329543665));
#28158=CARTESIAN_POINT('Ctrl Pts',(40.9933380050967,45.1315847005369,46.1007126407532));
#28159=CARTESIAN_POINT('Ctrl Pts',(41.0570239026048,45.1273602004552,46.0535451959746));
#28160=CARTESIAN_POINT('Ctrl Pts',(41.1230600087996,45.1231357003735,46.0096028033464));
#28161=CARTESIAN_POINT('Ctrl Pts',(41.1910807598299,45.1189112002919,45.9691123340651));
#28162=CARTESIAN_POINT('Ctrl Pts',(41.2591341674404,45.114684672039,45.928602425418));
#28163=CARTESIAN_POINT('Ctrl Pts',(41.3291737025875,45.1104581437862,45.8915479613691));
#28164=CARTESIAN_POINT('Ctrl Pts',(41.4008097497902,45.1062316155333,45.8581294892581));
#28165=CARTESIAN_POINT('Ctrl Pts',(41.4725767445262,45.1019973613733,45.8246499296548));
#28166=CARTESIAN_POINT('Ctrl Pts',(41.5459456469414,45.0977631072133,45.7948198203616));
#28167=CARTESIAN_POINT('Ctrl Pts',(41.6205076318713,45.0935288530533,45.7687711706485));
#28168=CARTESIAN_POINT('Ctrl Pts',(41.6916195367968,45.0894905233396,45.7439278258319));
#28169=CARTESIAN_POINT('Ctrl Pts',(41.7638162025467,45.0854521936259,45.7225238010962));
#28170=CARTESIAN_POINT('Ctrl Pts',(41.8367342512713,45.0814138639122,45.7046302831114));
#28171=CARTESIAN_POINT('Ctrl Pts',(41.9132125189615,45.077178363014,45.68586311528));
#28172=CARTESIAN_POINT('Ctrl Pts',(41.9907751193135,45.0729428621159,45.6708866715058));
#28173=CARTESIAN_POINT('Ctrl Pts',(42.069012013743,45.0687073612177,45.6598210765299));
#28174=CARTESIAN_POINT('Ctrl Pts',(42.1471354899157,45.0644780004294,45.6487715230969));
#28175=CARTESIAN_POINT('Ctrl Pts',(42.2259308582106,45.0602486396411,45.6416216250712));
#28176=CARTESIAN_POINT('Ctrl Pts',(42.3049755817985,45.0560192788528,45.6384410232125));
#28177=CARTESIAN_POINT('Ctrl Pts',(42.3839279980922,45.0517948570513,45.6352641356151));
#28178=CARTESIAN_POINT('Ctrl Pts',(42.4631287244875,45.0475704352499,45.636047351779));
#28179=CARTESIAN_POINT('Ctrl Pts',(42.5421492814504,45.0433460134484,45.6408086082975));
#28180=CARTESIAN_POINT('Ctrl Pts',(42.6211193065925,45.0391242930672,45.6455668201024));
#28181=CARTESIAN_POINT('Ctrl Pts',(42.6999089237416,45.0349025726859,45.6542979950814));
#28182=CARTESIAN_POINT('Ctrl Pts',(42.7780900513668,45.0306808523046,45.6669679912274));
#28183=CARTESIAN_POINT('Ctrl Pts',(42.8562455987824,45.0264605132348,45.6796338418569));
#28184=CARTESIAN_POINT('Ctrl Pts',(42.93379258905,45.022240174165,45.6962358795983));
#28185=CARTESIAN_POINT('Ctrl Pts',(43.0103099538483,45.0180198350952,45.7166883258885));
#28186=CARTESIAN_POINT('Ctrl Pts',(43.0868261775518,45.0137995589629,45.7371404671738));
#28187=CARTESIAN_POINT('Ctrl Pts',(43.1623123532194,45.0095792828305,45.7614427803804));
#28188=CARTESIAN_POINT('Ctrl Pts',(43.2363609277338,45.0053590066982,45.7894591522751));
#28189=CARTESIAN_POINT('Ctrl Pts',(43.3104835684002,45.0011345092879,45.8175035471921));
#28190=CARTESIAN_POINT('Ctrl Pts',(43.3831652954117,44.9969100118777,45.8492692553728));
#28191=CARTESIAN_POINT('Ctrl Pts',(43.4540175371904,44.9926855144674,45.8845715629701));
#28192=CARTESIAN_POINT('Ctrl Pts',(43.5249037951369,44.9884589888755,45.9198908192084));
#28193=CARTESIAN_POINT('Ctrl Pts',(43.5939584085004,44.9842324632837,45.9587498268391));
#28194=CARTESIAN_POINT('Ctrl Pts',(43.660818753645,44.9800059376918,46.0009185831095));
#28195=CARTESIAN_POINT('Ctrl Pts',(43.7278013174142,44.975771686143,46.0431644225505));
#28196=CARTESIAN_POINT('Ctrl Pts',(43.7925812130381,44.9715374345943,46.0887318294391));
#28197=CARTESIAN_POINT('Ctrl Pts',(43.8548262464889,44.9673031830455,46.137348386459));
#28198=CARTESIAN_POINT('Ctrl Pts',(43.9141915126665,44.9632648291991,46.183715697843));
#28199=CARTESIAN_POINT('Ctrl Pts',(43.9712510336822,44.9592264753528,46.2328560001001));
#28200=CARTESIAN_POINT('Ctrl Pts',(44.0257483506338,44.9551881215064,46.2845021884854));
#28201=CARTESIAN_POINT('Ctrl Pts',(44.082906129461,44.9509526224233,46.3386696517316));
#28202=CARTESIAN_POINT('Ctrl Pts',(44.1374624215625,44.9467171233403,46.3957998168079));
#28203=CARTESIAN_POINT('Ctrl Pts',(44.189094371249,44.9424816242572,46.4556128167894));
#28204=CARTESIAN_POINT('Ctrl Pts',(44.2406514707316,44.9382522653252,46.5153391065988));
#28205=CARTESIAN_POINT('Ctrl Pts',(44.2892923423664,44.9340229063932,46.5777401556207));
#28206=CARTESIAN_POINT('Ctrl Pts',(44.3347298274189,44.9297935474612,46.6424982741095));
#28207=CARTESIAN_POINT('Ctrl Pts',(44.3801142506296,44.9255691275696,46.7071807681435));
#28208=CARTESIAN_POINT('Ctrl Pts',(44.4223024529642,44.921344707678,46.7742144795354));
#28209=CARTESIAN_POINT('Ctrl Pts',(44.4610475453567,44.9171202877864,46.8432487490047));
#28210=CARTESIAN_POINT('Ctrl Pts',(44.4997678608552,44.9128985693467,46.9122388721146));
#28211=CARTESIAN_POINT('Ctrl Pts',(44.5350492074518,44.908676850907,46.9832266059233));
#28212=CARTESIAN_POINT('Ctrl Pts',(44.566688710933,44.9044551324673,47.0558334517599));
#28213=CARTESIAN_POINT('Ctrl Pts',(44.598317862011,44.9002347953682,47.128416540734));
#28214=CARTESIAN_POINT('Ctrl Pts',(44.6263073487521,44.8960144582691,47.2026172598375));
#28215=CARTESIAN_POINT('Ctrl Pts',(44.6505015188027,44.89179412117,47.278035073728));
#28216=CARTESIAN_POINT('Ctrl Pts',(44.6746953278965,44.8875738470348,47.3534517624478));
#28217=CARTESIAN_POINT('Ctrl Pts',(44.6950937907522,44.8833535728996,47.4300850625351));
#28218=CARTESIAN_POINT('Ctrl Pts',(44.7115908994855,44.8791332987644,47.5075185746487));
#28219=CARTESIAN_POINT('Ctrl Pts',(44.7281045091421,44.8749088033792,47.5850295381794));
#28220=CARTESIAN_POINT('Ctrl Pts',(44.7407088713939,44.870684307994,47.6633418524846));
#28221=CARTESIAN_POINT('Ctrl Pts',(44.7493491216818,44.8664598126088,47.7420287896819));
#28222=CARTESIAN_POINT('Ctrl Pts',(44.7579935201187,44.8622332890606,47.8207535041575));
#28223=CARTESIAN_POINT('Ctrl Pts',(44.7626699875375,44.8580067655124,47.8998527306407));
#28224=CARTESIAN_POINT('Ctrl Pts',(44.7633757862348,44.8537802419642,47.9788970632581));
#28225=CARTESIAN_POINT('Ctrl Pts',(44.7640828751094,44.8495459924666,48.0580858863779));
#28226=CARTESIAN_POINT('Ctrl Pts',(44.7608048110432,44.845311742969,48.1372191449375));
#28227=CARTESIAN_POINT('Ctrl Pts',(44.7535909903321,44.8410774934714,48.2158700792777));
#28228=CARTESIAN_POINT('Ctrl Pts',(44.7467108837934,44.8370391220145,48.2908825905824));
#28229=CARTESIAN_POINT('Ctrl Pts',(44.7362511936526,44.8330007505575,48.3654560672734));
#28230=CARTESIAN_POINT('Ctrl Pts',(44.7222978216176,44.8289623791005,48.4392303138562));
#28231=CARTESIAN_POINT('Ctrl Pts',(44.7076633288885,44.8247268783501,48.516605780697));
#28232=CARTESIAN_POINT('Ctrl Pts',(44.6891297353807,44.8204913775997,48.5933961188597));
#28233=CARTESIAN_POINT('Ctrl Pts',(44.6667577552311,44.8162558768493,48.6691783917608));
#28234=CARTESIAN_POINT('Ctrl Pts',(44.6444182073185,44.8120265162244,48.7448508045328));
#28235=CARTESIAN_POINT('Ctrl Pts',(44.6182514545177,44.8077971555994,48.8195176077341));
#28236=CARTESIAN_POINT('Ctrl Pts',(44.5883693327607,44.8035677949744,48.892765425144));
#28237=CARTESIAN_POINT('Ctrl Pts',(44.5585221070795,44.7993433733592,48.9659277044048));
#28238=CARTESIAN_POINT('Ctrl Pts',(44.5249683107645,44.7951189517439,49.0376738584772));
#28239=CARTESIAN_POINT('Ctrl Pts',(44.4878692935888,44.7908945301286,49.1076065428613));
#28240=CARTESIAN_POINT('Ctrl Pts',(44.4507940004999,44.7866728099473,49.1774945066785));
#28241=CARTESIAN_POINT('Ctrl Pts',(44.4101782056166,44.782451089766,49.2455708890191));
#28242=CARTESIAN_POINT('Ctrl Pts',(44.3662304840665,44.7782293695847,49.3114603022691));
#28243=CARTESIAN_POINT('Ctrl Pts',(44.3222971419844,44.7740090307284,49.3773281568426));
#28244=CARTESIAN_POINT('Ctrl Pts',(44.2750342982299,44.7697886918722,49.4410100730306));
#28245=CARTESIAN_POINT('Ctrl Pts',(44.2246946079982,44.765568353016,49.5021584565026));
#28246=CARTESIAN_POINT('Ctrl Pts',(44.1743556686358,44.7613480771105,49.5633059278825));
#28247=CARTESIAN_POINT('Ctrl Pts',(44.1209402733613,44.7571278012051,49.6219195801549));
#28248=CARTESIAN_POINT('Ctrl Pts',(44.064741276658,44.7529075252996,49.6776849891118));
#28249=CARTESIAN_POINT('Ctrl Pts',(44.0084860678758,44.7486830281359,49.733506176459));
#28250=CARTESIAN_POINT('Ctrl Pts',(43.9494420297357,44.7444585309721,49.7864730980574));
#28251=CARTESIAN_POINT('Ctrl Pts',(43.8879383714039,44.7402340338083,49.8363087550311));
#28252=CARTESIAN_POINT('Ctrl Pts',(43.8264051853199,44.7360075084741,49.8861683379789));
#28253=CARTESIAN_POINT('Ctrl Pts',(43.7624104062164,44.7317809831398,49.9328933843703));
#28254=CARTESIAN_POINT('Ctrl Pts',(43.6963136956999,44.7275544578055,49.9762492867148));
#28255=CARTESIAN_POINT('Ctrl Pts',(43.6300961627024,44.7233202065304,50.0196844421363));
#28256=CARTESIAN_POINT('Ctrl Pts',(43.5617694265342,44.7190859552553,50.0597379090438));
#28257=CARTESIAN_POINT('Ctrl Pts',(43.4917191273015,44.7148517039801,50.0962203576876));
#28258=CARTESIAN_POINT('Ctrl Pts',(43.4249096700583,44.7108133482183,50.1310149641275));
#28259=CARTESIAN_POINT('Ctrl Pts',(43.3565329421062,44.7067749924565,50.1625615514277));
#28260=CARTESIAN_POINT('Ctrl Pts',(43.2869383457606,44.7027366366947,50.1907375040656));
#28261=CARTESIAN_POINT('Ctrl Pts',(43.2139462788801,44.6985011363925,50.220288950979));
#28262=CARTESIAN_POINT('Ctrl Pts',(43.1393369414077,44.6942656360903,50.2462445959887));
#28263=CARTESIAN_POINT('Ctrl Pts',(43.0634988806087,44.6900301357881,50.2684266962657));
#28264=CARTESIAN_POINT('Ctrl Pts',(42.9877707608884,44.6858007756148,50.2905766395492));
#28265=CARTESIAN_POINT('Ctrl Pts',(42.9108179017726,44.6815714154415,50.3089637707813));
#28266=CARTESIAN_POINT('Ctrl Pts',(42.833048466458,44.6773420552683,50.3234585140687));
#28267=CARTESIAN_POINT('Ctrl Pts',(42.7553698496655,44.6731176341079,50.3379363305113));
#28268=CARTESIAN_POINT('Ctrl Pts',(42.6768770106461,44.6688932129475,50.3485307062118));
#28269=CARTESIAN_POINT('Ctrl Pts',(42.5979914160436,44.664668791787,50.3551623808292));
#28270=CARTESIAN_POINT('Ctrl Pts',(42.5191562672544,44.6604470720623,50.3617898146188));
#28271=CARTESIAN_POINT('Ctrl Pts',(42.4399293278184,44.6562253523376,50.3644595377019));
#28272=CARTESIAN_POINT('Ctrl Pts',(42.3607391465437,44.6520036326129,50.3631438860734));
#28273=CARTESIAN_POINT('Ctrl Pts',(42.2815748759114,44.6477832942144,50.3618286649196));
#28274=CARTESIAN_POINT('Ctrl Pts',(42.2024478084901,44.6435629558158,50.3565306661472));
#28275=CARTESIAN_POINT('Ctrl Pts',(42.1237869651027,44.6393426174173,50.3472743342551));
#28276=CARTESIAN_POINT('Ctrl Pts',(42.0451272950326,44.63512234197,50.3380181404319));
#28277=CARTESIAN_POINT('Ctrl Pts',(41.9669343011522,44.6309020665227,50.3248037870308));
#28278=CARTESIAN_POINT('Ctrl Pts',(41.8896308547567,44.6266817910753,50.3077074720345));
#28279=CARTESIAN_POINT('Ctrl Pts',(41.8122500868648,44.6224572943672,50.2905940567312));
#28280=CARTESIAN_POINT('Ctrl Pts',(41.7357611032287,44.618232797659,50.2695910249086));
#28281=CARTESIAN_POINT('Ctrl Pts',(41.6605749669654,44.6140083009508,50.2448253966449));
#28282=CARTESIAN_POINT('Ctrl Pts',(41.5853527340113,44.6097817760715,50.2200478784601));
#28283=CARTESIAN_POINT('Ctrl Pts',(41.5114350329334,44.6055552511922,50.1915043345427));
#28284=CARTESIAN_POINT('Ctrl Pts',(41.4392137490155,44.6013287263129,50.1593703297071));
#28285=CARTESIAN_POINT('Ctrl Pts',(41.3668604469842,44.5970944754862,50.1271775849756));
#28286=CARTESIAN_POINT('Ctrl Pts',(41.2962101784068,44.5928602246595,50.0913814771134));
#28287=CARTESIAN_POINT('Ctrl Pts',(41.2276308028632,44.5886259738328,50.0522039144551));
#28288=CARTESIAN_POINT('Ctrl Pts',(41.1622241446536,44.5845876139848,50.0148388403353));
#28289=CARTESIAN_POINT('Ctrl Pts',(41.0987012852547,44.5805492541368,49.9743984905189));
#28290=CARTESIAN_POINT('Ctrl Pts',(41.0373543723427,44.5765108942888,49.9311103889541));
#28291=CARTESIAN_POINT('Ctrl Pts',(40.9734456513011,44.5723038950978,49.8860146037548));
#28292=CARTESIAN_POINT('Ctrl Pts',(40.9116484640583,44.5680968959068,49.837651354278));
#28293=CARTESIAN_POINT('Ctrl Pts',(40.8523197968065,44.5638898967158,49.7862464638294));
#28294=CARTESIAN_POINT('Ctrl Pts',(40.7930773333072,44.5596890102379,49.7349162639925));
#28295=CARTESIAN_POINT('Ctrl Pts',(40.7362966266365,44.5554881237599,49.6805535054133));
#28296=CARTESIAN_POINT('Ctrl Pts',(40.6823050293388,44.5512872372819,49.6234267549432));
#28297=CARTESIAN_POINT('Ctrl Pts',(40.62837581227,44.5470912043788,49.5663660069613));
#28298=CARTESIAN_POINT('Ctrl Pts',(40.5772296285932,44.5428951714757,49.5065479552999));
#28299=CARTESIAN_POINT('Ctrl Pts',(40.5291588834611,44.5386991385726,49.4442797366049));
#28300=CARTESIAN_POINT('Ctrl Pts',(40.4811179883224,44.5345057112367,49.3820501839615));
#28301=CARTESIAN_POINT('Ctrl Pts',(40.4361490329949,44.5303122839007,49.3173738591201));
#28302=CARTESIAN_POINT('Ctrl Pts',(40.3945049441187,44.5261188565648,49.2505918685708));
#28303=CARTESIAN_POINT('Ctrl Pts',(40.3528732643496,44.5219266787864,49.1838297777216));
#28304=CARTESIAN_POINT('Ctrl Pts',(40.3145647359826,44.5177345010081,49.1149636708361));
#28305=CARTESIAN_POINT('Ctrl Pts',(40.2797887364826,44.5135423232298,49.0443632696307));
#28306=CARTESIAN_POINT('Ctrl Pts',(40.2450118677341,44.5093500406653,48.9737611037231));
#28307=CARTESIAN_POINT('Ctrl Pts',(40.2137679116889,44.5051577581008,48.9014249857457));
#28308=CARTESIAN_POINT('Ctrl Pts',(40.1862193708099,44.5009654755363,48.8277474051441));
#28309=CARTESIAN_POINT('Ctrl Pts',(40.1586435762283,44.4967690455572,48.753996935496));
#28310=CARTESIAN_POINT('Ctrl Pts',(40.1347706618192,44.492572615578,48.6789028011075));
#28311=CARTESIAN_POINT('Ctrl Pts',(40.1147139350392,44.4883761855988,48.6028748146972));
#28312=CARTESIAN_POINT('Ctrl Pts',(40.0946464483958,44.4841775043543,48.5268060414345));
#28313=CARTESIAN_POINT('Ctrl Pts',(40.0783993219462,44.4799788231098,48.449802885319));
#28314=CARTESIAN_POINT('Ctrl Pts',(40.0660346410796,44.4757801418653,48.3722850309365));
#28315=CARTESIAN_POINT('Ctrl Pts',(40.0536493071805,44.4715744474597,48.2946376965637));
#28316=CARTESIAN_POINT('Ctrl Pts',(40.0451594155884,44.467368753054,48.2164744211785));
#28317=CARTESIAN_POINT('Ctrl Pts',(40.0405750864627,44.4631630586483,48.1382190952057));
#28318=CARTESIAN_POINT('Ctrl Pts',(40.037864108291,44.4606759890209,48.0919422082909));
#28319=CARTESIAN_POINT('Ctrl Pts',(40.0365179253812,44.4581889193935,48.0456331351725));
#28320=CARTESIAN_POINT('Ctrl Pts',(40.0365300816234,44.4557018497661,47.9993788486445));
#28321=CARTESIAN_POINT('',(40.0365310047746,43.6619518497613,48.0021793366867));
#28322=CARTESIAN_POINT('Ctrl Pts',(40.0365300816236,44.4557018497283,47.9993788479416));
#28323=CARTESIAN_POINT('Ctrl Pts',(40.0365389068377,44.4538962837798,47.9657991026046));
#28324=CARTESIAN_POINT('Ctrl Pts',(40.0372633394702,44.4520907178314,47.9322296454892));
#28325=CARTESIAN_POINT('Ctrl Pts',(40.0387022762554,44.450285151883,47.8986910628888));
#28326=CARTESIAN_POINT('Ctrl Pts',(40.0420777371408,44.4460496515486,47.8200161864904));
#28327=CARTESIAN_POINT('Ctrl Pts',(40.0493959105134,44.4418141512142,47.7413606516739));
#28328=CARTESIAN_POINT('Ctrl Pts',(40.0606574248334,44.4375786508797,47.6631517301321));
#28329=CARTESIAN_POINT('Ctrl Pts',(40.0719026135347,44.4333492906754,47.5850561866845));
#28330=CARTESIAN_POINT('Ctrl Pts',(40.0870797247141,44.4291199304711,47.507406431426));
#28331=CARTESIAN_POINT('Ctrl Pts',(40.1061374221056,44.4248905702667,47.4306276133884));
#28332=CARTESIAN_POINT('Ctrl Pts',(40.1251728640626,44.4206661490772,47.3539384570727));
#28333=CARTESIAN_POINT('Ctrl Pts',(40.1480797743804,44.4164417278876,47.2781186700249));
#28334=CARTESIAN_POINT('Ctrl Pts',(40.1747555143851,44.412217306698,47.203584643455));
#28335=CARTESIAN_POINT('Ctrl Pts',(40.2014141957622,44.4079955869454,47.1290982799758));
#28336=CARTESIAN_POINT('Ctrl Pts',(40.2318367655739,44.4037738671927,47.0558964857531));
#28337=CARTESIAN_POINT('Ctrl Pts',(40.2658706969478,44.39955214744,46.9843807018602));
#28338=CARTESIAN_POINT('Ctrl Pts',(40.2998934925749,44.3953318090147,46.9128883176051));
#28339=CARTESIAN_POINT('Ctrl Pts',(40.3375251019218,44.3911114705895,46.8430812717631));
#28340=CARTESIAN_POINT('Ctrl Pts',(40.3785653847968,44.3868911321642,46.775339827806));
#28341=CARTESIAN_POINT('Ctrl Pts',(40.419605055496,44.3826708566914,46.7075993943114));
#28342=CARTESIAN_POINT('Ctrl Pts',(40.4640530543128,44.3784505812186,46.6419249021921));
#28343=CARTESIAN_POINT('Ctrl Pts',(40.5116646964617,44.3742303057459,46.5786695590712));
#28344=CARTESIAN_POINT('Ctrl Pts',(40.5593239613443,44.3700058090144,46.5153509458712));
#28345=CARTESIAN_POINT('Ctrl Pts',(40.6101529078774,44.365781312283,46.454456691243));
#28346=CARTESIAN_POINT('Ctrl Pts',(40.6638655006203,44.3615568155516,46.3963081839195));
#28347=CARTESIAN_POINT('Ctrl Pts',(40.71760388064,44.3573302906503,46.338131759648));
#28348=CARTESIAN_POINT('Ctrl Pts',(40.7742283289578,44.3531037657489,46.2827040375186));
#28349=CARTESIAN_POINT('Ctrl Pts',(40.8334165876995,44.3488772408475,46.2303088254713));
#28350=CARTESIAN_POINT('Ctrl Pts',(40.8927130405837,44.3446429900011,46.1778178367419));
#28351=CARTESIAN_POINT('Ctrl Pts',(40.9545823011305,44.3404087391546,46.1283707287589));
#28352=CARTESIAN_POINT('Ctrl Pts',(41.0186699022907,44.3361744883081,46.082210229962));
#28353=CARTESIAN_POINT('Ctrl Pts',(41.0797925871386,44.3321361286977,46.0381852770958));
#28354=CARTESIAN_POINT('Ctrl Pts',(41.1429325758987,44.3280977690873,45.9971497222663));
#28355=CARTESIAN_POINT('Ctrl Pts',(41.2077616859249,44.3240594094768,45.9592750691601));
#28356=CARTESIAN_POINT('Ctrl Pts',(41.275755559475,44.3198239092118,45.919551488611));
#28357=CARTESIAN_POINT('Ctrl Pts',(41.3458661400769,44.3155884089467,45.8831543034111));
#28358=CARTESIAN_POINT('Ctrl Pts',(41.4177344202536,44.3113529086816,45.8503151924653));
#28359=CARTESIAN_POINT('Ctrl Pts',(41.4894985142388,44.3071235485474,45.8175236878055));
#28360=CARTESIAN_POINT('Ctrl Pts',(41.5630148244236,44.3028941884131,45.7882802077816));
#28361=CARTESIAN_POINT('Ctrl Pts',(41.6378980160727,44.2986648282789,45.7627715791645));
#28362=CARTESIAN_POINT('Ctrl Pts',(41.7126937596841,44.2944404071601,45.7372927393354));
#28363=CARTESIAN_POINT('Ctrl Pts',(41.7888527707718,44.2902159860414,45.7155402342941));
#28364=CARTESIAN_POINT('Ctrl Pts',(41.8659693260067,44.2859915649227,45.6976530061404));
#28365=CARTESIAN_POINT('Ctrl Pts',(41.9430365666652,44.2817698452413,45.6797772165303));
#28366=CARTESIAN_POINT('Ctrl Pts',(42.0210596801459,44.2775481255598,45.6657619036346));
#28367=CARTESIAN_POINT('Ctrl Pts',(42.0996185275127,44.2733264058784,45.6556959642814));
#28368=CARTESIAN_POINT('Ctrl Pts',(42.1781516707776,44.2691060675247,45.6456333184584));
#28369=CARTESIAN_POINT('Ctrl Pts',(42.2572197346683,44.264885729171,45.6395175398692));
#28370=CARTESIAN_POINT('Ctrl Pts',(42.3363946328045,44.2606653908173,45.6373860243019));
#28371=CARTESIAN_POINT('Ctrl Pts',(42.4155683499277,44.2564451154163,45.6352545405294));
#28372=CARTESIAN_POINT('Ctrl Pts',(42.4948484289113,44.2522248400153,45.6371072129401));
#28373=CARTESIAN_POINT('Ctrl Pts',(42.5738054398561,44.2480045646143,45.6429293370846));
#28374=CARTESIAN_POINT('Ctrl Pts',(42.6528414262107,44.2437800679545,45.64875728471));
#28375=CARTESIAN_POINT('Ctrl Pts',(42.731553229808,44.2395555712946,45.6585625807997));
#28376=CARTESIAN_POINT('Ctrl Pts',(42.8095158109758,44.2353310746348,45.6722785300941));
#28377=CARTESIAN_POINT('Ctrl Pts',(42.8875158217775,44.231104549805,45.6860010643803));
#28378=CARTESIAN_POINT('Ctrl Pts',(42.9647654353776,44.2268780249753,45.7036378874573));
#28379=CARTESIAN_POINT('Ctrl Pts',(43.0408516225767,44.2226515001455,45.7250715090929));
#28380=CARTESIAN_POINT('Ctrl Pts',(43.1170768927797,44.2184172493698,45.7465443106716));
#28381=CARTESIAN_POINT('Ctrl Pts',(43.1921340409633,44.2141829985941,45.7718276291732));
#28382=CARTESIAN_POINT('Ctrl Pts',(43.2656271620513,44.2099487478184,45.8007546618854));
#28383=CARTESIAN_POINT('Ctrl Pts',(43.3357202468722,44.2059103875694,45.8283434338343));
#28384=CARTESIAN_POINT('Ctrl Pts',(43.4043905078659,44.2018720273204,45.8592460549525));
#28385=CARTESIAN_POINT('Ctrl Pts',(43.4713161614431,44.1978336670714,45.8932792963634));
#28386=CARTESIAN_POINT('Ctrl Pts',(43.5415089141829,44.1935981668218,45.9289739331971));
#28387=CARTESIAN_POINT('Ctrl Pts',(43.6100491956043,44.1893626665722,45.968248331619));
#28388=CARTESIAN_POINT('Ctrl Pts',(43.6765479372573,44.1851271663226,46.0109258925862));
#28389=CARTESIAN_POINT('Ctrl Pts',(43.7429502768371,44.1808978062043,46.0535415846329));
#28390=CARTESIAN_POINT('Ctrl Pts',(43.8073165622004,44.1766684460859,46.0995503907936));
#28391=CARTESIAN_POINT('Ctrl Pts',(43.8692812039775,44.1724390859676,46.1487293054395));
#28392=CARTESIAN_POINT('Ctrl Pts',(43.931173483894,44.1682146648655,46.1978507893045));
#28393=CARTESIAN_POINT('Ctrl Pts',(43.9906693278038,44.1639902437633,46.2501347347698));
#28394=CARTESIAN_POINT('Ctrl Pts',(44.0474323886332,44.1597658226611,46.3053150836269));
#28395=CARTESIAN_POINT('Ctrl Pts',(44.1041591505548,44.1555441029967,46.3604601456908));
#28396=CARTESIAN_POINT('Ctrl Pts',(44.1581562623044,44.1513223833322,46.4184976086617));
#28397=CARTESIAN_POINT('Ctrl Pts',(44.2091216675651,44.1471006636677,46.4791222163348));
#28398=CARTESIAN_POINT('Ctrl Pts',(44.2600703971697,44.1428803253313,46.5397269879032));
#28399=CARTESIAN_POINT('Ctrl Pts',(44.3079890881949,44.1386599869949,46.6029168643068));
#28400=CARTESIAN_POINT('Ctrl Pts',(44.3526146986442,44.1344396486585,46.6683520436922));
#28401=CARTESIAN_POINT('Ctrl Pts',(44.3972396434315,44.1302193732751,46.7337862470079));
#28402=CARTESIAN_POINT('Ctrl Pts',(44.4385713419416,44.1259990978918,46.801465298217));
#28403=CARTESIAN_POINT('Ctrl Pts',(44.476389843107,44.1217788225084,46.8710200797436));
#28404=CARTESIAN_POINT('Ctrl Pts',(44.5142461715825,44.1175543258667,46.9406444322529));
#28405=CARTESIAN_POINT('Ctrl Pts',(44.548582058289,44.1133298292249,47.0121478496339));
#28406=CARTESIAN_POINT('Ctrl Pts',(44.5792236529652,44.1091053325832,47.0851367800284));
#28407=CARTESIAN_POINT('Ctrl Pts',(44.6098799585901,44.1048788077717,47.1581607522156));
#28408=CARTESIAN_POINT('Ctrl Pts',(44.6368382790136,44.1006522829603,47.2326712162209));
#28409=CARTESIAN_POINT('Ctrl Pts',(44.6599739815353,44.0964257581489,47.3082572416832));
#28410=CARTESIAN_POINT('Ctrl Pts',(44.6831519753458,44.0921915073917,47.3839814358669));
#28411=CARTESIAN_POINT('Ctrl Pts',(44.702493273436,44.0879572566346,47.4607846638789));
#28412=CARTESIAN_POINT('Ctrl Pts',(44.7179239802904,44.0837230058774,47.5382437195935));
#28413=CARTESIAN_POINT('Ctrl Pts',(44.7326408119428,44.0796846454734,47.6121192648726));
#28414=CARTESIAN_POINT('Ctrl Pts',(44.7438008675764,44.0756462850694,47.6865909396363));
#28415=CARTESIAN_POINT('Ctrl Pts',(44.7513841656328,44.0716079246653,47.7612889895468));
#28416=CARTESIAN_POINT('Ctrl Pts',(44.7593376561077,44.0673724243897,47.8396335599491));
#28417=CARTESIAN_POINT('Ctrl Pts',(44.7633864936398,44.0631369241141,47.9185249761328));
#28418=CARTESIAN_POINT('Ctrl Pts',(44.7634687202651,44.0589014238385,47.997540482027));
#28419=CARTESIAN_POINT('Ctrl Pts',(44.7635508276879,44.0546720636938,48.0764414405206));
#28420=CARTESIAN_POINT('Ctrl Pts',(44.7596777428528,44.050442703549,48.1554656661121));
#28421=CARTESIAN_POINT('Ctrl Pts',(44.75183923902,44.0462133434043,48.2341850437283));
#28422=CARTESIAN_POINT('Ctrl Pts',(44.7440098889341,44.0419889222752,48.3128124934352));
#28423=CARTESIAN_POINT('Ctrl Pts',(44.7322243683506,44.037764501146,48.3911353379879));
#28424=CARTESIAN_POINT('Ctrl Pts',(44.7165244787904,44.0335400800169,48.4687267648265));
#28425=CARTESIAN_POINT('Ctrl Pts',(44.7008346290126,44.0293183603252,48.546268573416));
#28426=CARTESIAN_POINT('Ctrl Pts',(44.6812354713363,44.0250966406335,48.623079433845));
#28427=CARTESIAN_POINT('Ctrl Pts',(44.6578203249055,44.0208749209417,48.698740167261));
#28428=CARTESIAN_POINT('Ctrl Pts',(44.6344128398059,44.0166545825778,48.7743761448232));
#28429=CARTESIAN_POINT('Ctrl Pts',(44.6071919838615,44.0124342442139,48.8488622945803));
#28430=CARTESIAN_POINT('Ctrl Pts',(44.5763012364911,44.0082139058499,48.9217935609165));
#28431=CARTESIAN_POINT('Ctrl Pts',(44.5454109499037,44.0039936304388,48.9947237393711));
#28432=CARTESIAN_POINT('Ctrl Pts',(44.5108510649889,43.9997733550277,49.0660986488462));
#28433=CARTESIAN_POINT('Ctrl Pts',(44.472813028337,43.9955530796166,49.135533614851));
#28434=CARTESIAN_POINT('Ctrl Pts',(44.4347369447869,43.9913285829469,49.2050380319977));
#28435=CARTESIAN_POINT('Ctrl Pts',(44.3931759858738,43.9871040862772,49.272598216875));
#28436=CARTESIAN_POINT('Ctrl Pts',(44.3483670882485,43.9828795896075,49.3378550483256));
#28437=CARTESIAN_POINT('Ctrl Pts',(44.3035366779883,43.978653064768,49.4031432094106));
#28438=CARTESIAN_POINT('Ctrl Pts',(44.2554555078394,43.9744265399285,49.4661254405331));
#28439=CARTESIAN_POINT('Ctrl Pts',(44.2044017565428,43.9702000150889,49.5264746122636));
#28440=CARTESIAN_POINT('Ctrl Pts',(44.1532546807014,43.9659657643038,49.5869341002556));
#28441=CARTESIAN_POINT('Ctrl Pts',(44.0991244873708,43.9617315135187,49.6447505675384));
#28442=CARTESIAN_POINT('Ctrl Pts',(44.0423271279393,43.9574972627335,49.6996329149951));
#28443=CARTESIAN_POINT('Ctrl Pts',(43.9881574046413,43.9534589025755,49.7519762211881));
#28444=CARTESIAN_POINT('Ctrl Pts',(43.9315621344702,43.9494205424176,49.80165068022));
#28445=CARTESIAN_POINT('Ctrl Pts',(43.8728414812907,43.9453821822596,49.8484394531305));
#28446=CARTESIAN_POINT('Ctrl Pts',(43.8112542695525,43.9411466819943,49.8975123075383));
#28447=CARTESIAN_POINT('Ctrl Pts',(43.7470947611614,43.9369111817289,49.9435970781654));
#28448=CARTESIAN_POINT('Ctrl Pts',(43.6806849871049,43.9326756814635,49.9864129491886));
#28449=CARTESIAN_POINT('Ctrl Pts',(43.6143714861415,43.9284463213291,50.0291667507891));
#28450=CARTESIAN_POINT('Ctrl Pts',(43.5458145887447,43.9242169611948,50.0686608111637));
#28451=CARTESIAN_POINT('Ctrl Pts',(43.4753688191252,43.9199876010604,50.1046549227257));
#28452=CARTESIAN_POINT('Ctrl Pts',(43.4050053155588,43.9157631799417,50.1406070006282));
#28453=CARTESIAN_POINT('Ctrl Pts',(43.3327577389102,43.9115387588231,50.1730670393305));
#28454=CARTESIAN_POINT('Ctrl Pts',(43.2590076647864,43.9073143377044,50.2018392931225));
#28455=CARTESIAN_POINT('Ctrl Pts',(43.1853047524407,43.9030926180232,50.2305931476022));
#28456=CARTESIAN_POINT('Ctrl Pts',(43.1101016857122,43.8988708983421,50.2556637277048));
#28457=CARTESIAN_POINT('Ctrl Pts',(43.0338014906415,43.8946491786609,50.2769027452574));
#28458=CARTESIAN_POINT('Ctrl Pts',(42.9575262606545,43.8904288403075,50.2981348134981));
#28459=CARTESIAN_POINT('Ctrl Pts',(42.8801550669499,43.8862085019542,50.3155376827934));
#28460=CARTESIAN_POINT('Ctrl Pts',(42.8021061938115,43.8819881636009,50.3290128917201));
#28461=CARTESIAN_POINT('Ctrl Pts',(42.7240584848924,43.8777678882004,50.3424878996433));
#28462=CARTESIAN_POINT('Ctrl Pts',(42.6453335793691,43.8735476127999,50.3520352851183));
#28463=CARTESIAN_POINT('Ctrl Pts',(42.5663585702586,43.8693273373994,50.3576079544745));
#28464=CARTESIAN_POINT('Ctrl Pts',(42.4873045677405,43.8651028407404,50.3631861977983));
#28465=CARTESIAN_POINT('Ctrl Pts',(42.4080004312113,43.8608783440813,50.3647817500414));
#28466=CARTESIAN_POINT('Ctrl Pts',(42.3288763723535,43.8566538474222,50.3623996000868));
#28467=CARTESIAN_POINT('Ctrl Pts',(42.2497143262418,43.8524273225933,50.3600163064683));
#28468=CARTESIAN_POINT('Ctrl Pts',(42.1707329985079,43.8482007977645,50.3536515440794));
#28469=CARTESIAN_POINT('Ctrl Pts',(42.0923580065131,43.8439742729356,50.3433622948113));
#28470=CARTESIAN_POINT('Ctrl Pts',(42.0138397476598,43.839740022161,50.3330542371404));
#28471=CARTESIAN_POINT('Ctrl Pts',(41.9359305022217,43.8355057713864,50.3188074422433));
#28472=CARTESIAN_POINT('Ctrl Pts',(41.8590460197369,43.8312715206118,50.3007301519599));
#28473=CARTESIAN_POINT('Ctrl Pts',(41.7857184690927,43.8272331603591,50.2834891772415));
#28474=CARTESIAN_POINT('Ctrl Pts',(41.7133232936402,43.8231948001064,50.2627644257604));
#28475=CARTESIAN_POINT('Ctrl Pts',(41.6422052471526,43.8191564398537,50.2386910357298));
#28476=CARTESIAN_POINT('Ctrl Pts',(41.567615441922,43.8149209395893,50.2134424587187));
#28477=CARTESIAN_POINT('Ctrl Pts',(41.4941471084168,43.810685439325,50.1844139801348));
#28478=CARTESIAN_POINT('Ctrl Pts',(41.4222106366493,43.8064499390606,50.151724518106));
#28479=CARTESIAN_POINT('Ctrl Pts',(41.350378449933,43.8022205789273,50.1190824454213));
#28480=CARTESIAN_POINT('Ctrl Pts',(41.2800741386975,43.7979912187939,50.0827901211133));
#28481=CARTESIAN_POINT('Ctrl Pts',(41.2116915188455,43.7937618586606,50.0430157597327));
#28482=CARTESIAN_POINT('Ctrl Pts',(41.1433887557167,43.7895374375431,50.0032878465604));
#28483=CARTESIAN_POINT('Ctrl Pts',(41.0770036280594,43.7853130164255,49.9600862115607));
#28484=CARTESIAN_POINT('Ctrl Pts',(41.0129071926658,43.781088595308,49.9136258737647));
#28485=CARTESIAN_POINT('Ctrl Pts',(40.9488517457316,43.776866875628,49.8671952464769));
#28486=CARTESIAN_POINT('Ctrl Pts',(40.8870824651688,43.772645155948,49.8175103271596));
#28487=CARTESIAN_POINT('Ctrl Pts',(40.827942099151,43.7684234362679,49.7648298493844));
#28488=CARTESIAN_POINT('Ctrl Pts',(40.7688210835978,43.7642030979158,49.7121666084272));
#28489=CARTESIAN_POINT('Ctrl Pts',(40.7123276247838,43.7599827595637,49.6565100671843));
#28490=CARTESIAN_POINT('Ctrl Pts',(40.6587708197668,43.7557624212116,49.5981587476857));
#28491=CARTESIAN_POINT('Ctrl Pts',(40.6052148136326,43.7515421458123,49.5398082985876));
#28492=CARTESIAN_POINT('Ctrl Pts',(40.5545956906101,43.7473218704131,49.4787634978217));
#28493=CARTESIAN_POINT('Ctrl Pts',(40.5071841114854,43.7431015950139,49.4153580653272));
#28494=CARTESIAN_POINT('Ctrl Pts',(40.4597251097368,43.7388770983561,49.3518892126294));
#28495=CARTESIAN_POINT('Ctrl Pts',(40.4154803425935,43.7346526016983,49.2860553882291));
#28496=CARTESIAN_POINT('Ctrl Pts',(40.3746783551241,43.7304281050406,49.2182211111687));
#28497=CARTESIAN_POINT('Ctrl Pts',(40.3338567787273,43.726201580213,49.1503542670495));
#28498=CARTESIAN_POINT('Ctrl Pts',(40.2964814964142,43.7219750553854,49.0804854714386));
#28499=CARTESIAN_POINT('Ctrl Pts',(40.2627348401853,43.7177485305579,49.0090035072002));
#28500=CARTESIAN_POINT('Ctrl Pts',(40.2289264962002,43.7135142797846,48.9373908763276));
#28501=CARTESIAN_POINT('Ctrl Pts',(40.1987602118412,43.7092800290114,48.8641596195118));
#28502=CARTESIAN_POINT('Ctrl Pts',(40.1723698696445,43.7050457782381,48.789717951697));
#28503=CARTESIAN_POINT('Ctrl Pts',(40.1472004323646,43.7010074179747,48.7187202027812));
#28504=CARTESIAN_POINT('Ctrl Pts',(40.1254653561815,43.6969690577113,48.6466219139841));
#28505=CARTESIAN_POINT('Ctrl Pts',(40.107237494923,43.6929306974479,48.573786141531));
#28506=CARTESIAN_POINT('Ctrl Pts',(40.0822668479016,43.6873984812843,48.4740072185593));
#28507=CARTESIAN_POINT('Ctrl Pts',(40.0637993296254,43.6818662651206,48.3725403527942));
#28508=CARTESIAN_POINT('Ctrl Pts',(40.0520163089416,43.676334048957,48.2701166922342));
#28509=CARTESIAN_POINT('Ctrl Pts',(40.0418054672349,43.6715399825584,48.1813591645122));
#28510=CARTESIAN_POINT('Ctrl Pts',(40.0366137200381,43.6667459161599,48.0918832185466));
#28511=CARTESIAN_POINT('Ctrl Pts',(40.0365310047746,43.6619518497613,48.0021793366867));
#28512=CARTESIAN_POINT('',(40.0365300407226,42.8682018496837,47.9995612592237));
#28513=CARTESIAN_POINT('Ctrl Pts',(40.0365310047741,43.6619518497283,48.0021793360685));
#28514=CARTESIAN_POINT('Ctrl Pts',(40.0364589799385,43.657777385097,47.9240690949938));
#28515=CARTESIAN_POINT('Ctrl Pts',(40.0402633944012,43.6536029204657,47.8458562414444));
#28516=CARTESIAN_POINT('Ctrl Pts',(40.047948045871,43.6494284558344,47.767961111066));
#28517=CARTESIAN_POINT('Ctrl Pts',(40.0556277589757,43.6452566738271,47.6901160382075));
#28518=CARTESIAN_POINT('Ctrl Pts',(40.0671827163339,43.6410848918198,47.6125887614653));
#28519=CARTESIAN_POINT('Ctrl Pts',(40.0825646803434,43.6369131098125,47.535797479425));
#28520=CARTESIAN_POINT('Ctrl Pts',(40.0979418366337,43.6327426317191,47.4590301989312));
#28521=CARTESIAN_POINT('Ctrl Pts',(40.1171435311434,43.6285721536257,47.3829989284983));
#28522=CARTESIAN_POINT('Ctrl Pts',(40.1400701839293,43.6244016755323,47.308112966349));
#28523=CARTESIAN_POINT('Ctrl Pts',(40.1629972380133,43.6202311244407,47.2332256934285));
#28524=CARTESIAN_POINT('Ctrl Pts',(40.1896492365983,43.6160605733491,47.1594842284149));
#28525=CARTESIAN_POINT('Ctrl Pts',(40.2198768503229,43.6118900222574,47.0872823584798));
#28526=CARTESIAN_POINT('Ctrl Pts',(40.2501347668174,43.6077152902453,47.0150081071564));
#28527=CARTESIAN_POINT('Ctrl Pts',(40.283975266881,43.6035405582332,46.9442769767219));
#28528=CARTESIAN_POINT('Ctrl Pts',(40.32120133412,43.5993658262211,46.875461629096));
#28529=CARTESIAN_POINT('Ctrl Pts',(40.3584475512711,43.5951888344891,46.806609032754));
#28530=CARTESIAN_POINT('Ctrl Pts',(40.3990827308522,43.5910118427571,46.7396746935101));
#28531=CARTESIAN_POINT('Ctrl Pts',(40.4428658481235,43.5868348510251,46.6750032632272));
#28532=CARTESIAN_POINT('Ctrl Pts',(40.4867236541362,43.5826507338467,46.6102215112487));
#28533=CARTESIAN_POINT('Ctrl Pts',(40.5337398262852,43.5784666166684,46.5477107572811));
#28534=CARTESIAN_POINT('Ctrl Pts',(40.5836327163485,43.57428249949,46.4877829746427));
#28535=CARTESIAN_POINT('Ctrl Pts',(40.6137518212058,43.5717566513406,46.4516060531041));
#28536=CARTESIAN_POINT('Ctrl Pts',(40.6449185295089,43.5692308031913,46.4163697355742));
#28537=CARTESIAN_POINT('Ctrl Pts',(40.6770647487152,43.566704955042,46.3821358027387));
#28538=CARTESIAN_POINT('Ctrl Pts',(40.7309695410664,43.562469454776,46.3247302015069));
#28539=CARTESIAN_POINT('Ctrl Pts',(40.7878489354429,43.5582339545099,46.2699124753785));
#28540=CARTESIAN_POINT('Ctrl Pts',(40.8474245481059,43.5539984542439,46.2180067600926));
#28541=CARTESIAN_POINT('Ctrl Pts',(40.9069137950403,43.5497690941088,46.1661762916185));
#28542=CARTESIAN_POINT('Ctrl Pts',(40.9690911474661,43.5455397339738,46.1172497565619));
#28543=CARTESIAN_POINT('Ctrl Pts',(41.033640235542,43.5413103738387,46.071515767508));
#28544=CARTESIAN_POINT('Ctrl Pts',(41.098113943666,43.5370859527194,46.0258351862713));
#28545=CARTESIAN_POINT('Ctrl Pts',(41.1649535025596,43.5328615316002,45.9833400122769));
#28546=CARTESIAN_POINT('Ctrl Pts',(41.2338093885432,43.5286371104809,45.9442787400404));
#28547=CARTESIAN_POINT('Ctrl Pts',(41.3026212424893,43.524415390799,45.9052424467491));
#28548=CARTESIAN_POINT('Ctrl Pts',(41.3734464572018,43.5201936711172,45.8696359277568));
#28549=CARTESIAN_POINT('Ctrl Pts',(41.4459074680793,43.5159719514354,45.8376637908426));
#28550=CARTESIAN_POINT('Ctrl Pts',(41.5183447700367,43.5117516130814,45.8057021150693));
#28551=CARTESIAN_POINT('Ctrl Pts',(41.592416376295,43.5075312747275,45.7773726494351));
#28552=CARTESIAN_POINT('Ctrl Pts',(41.6677224692794,43.5033109363735,45.7528328814034));
#28553=CARTESIAN_POINT('Ctrl Pts',(41.7430274389571,43.4990906609724,45.7282934794203));
#28554=CARTESIAN_POINT('Ctrl Pts',(41.8195664120887,43.4948703855714,45.7075438068233));
#28555=CARTESIAN_POINT('Ctrl Pts',(41.8969234796218,43.4906501101703,45.6906917798734));
#28556=CARTESIAN_POINT('Ctrl Pts',(41.9743579222437,43.4864256135106,45.6738228969707));
#28557=CARTESIAN_POINT('Ctrl Pts',(42.0526116342033,43.482201116851,45.66085954771));
#28558=CARTESIAN_POINT('Ctrl Pts',(42.1312581434926,43.4779766201913,45.6518585529272));
#28559=CARTESIAN_POINT('Ctrl Pts',(42.2099424107654,43.4737500953619,45.6428532367904));
#28560=CARTESIAN_POINT('Ctrl Pts',(42.2890193819993,43.4695235705324,45.6378140946676));
#28561=CARTESIAN_POINT('Ctrl Pts',(42.3680596681864,43.465297045703,45.636745833368));
#28562=CARTESIAN_POINT('Ctrl Pts',(42.4472444373668,43.4610627949278,45.6356756193225));
#28563=CARTESIAN_POINT('Ctrl Pts',(42.5263919172336,43.4568285441527,45.6385907732392));
#28564=CARTESIAN_POINT('Ctrl Pts',(42.6050751258938,43.4525942933775,45.6454438563416));
#28565=CARTESIAN_POINT('Ctrl Pts',(42.6801181875456,43.4485559331304,45.6519798930197));
#28566=CARTESIAN_POINT('Ctrl Pts',(42.75473863647,43.4445175728833,45.6620974688143));
#28567=CARTESIAN_POINT('Ctrl Pts',(42.8285758901674,43.4404792126362,45.6757123355171));
#28568=CARTESIAN_POINT('Ctrl Pts',(42.9060176458659,43.4362437123701,45.6899918371003));
#28569=CARTESIAN_POINT('Ctrl Pts',(42.9828921603495,43.4320082121041,45.7081730808793));
#28570=CARTESIAN_POINT('Ctrl Pts',(43.0587762231309,43.4277727118381,45.7301972929928));
#28571=CARTESIAN_POINT('Ctrl Pts',(43.1345502781076,43.423543351703,45.7521895769894));
#28572=CARTESIAN_POINT('Ctrl Pts',(43.2093362857701,43.419313991568,45.778013636414));
#28573=CARTESIAN_POINT('Ctrl Pts',(43.2827203614424,43.4150846314329,45.8075595323031));
#28574=CARTESIAN_POINT('Ctrl Pts',(43.3560187397288,43.4108602103136,45.8370709247114));
#28575=CARTESIAN_POINT('Ctrl Pts',(43.4279180062527,43.4066357891943,45.8702953422259));
#28576=CARTESIAN_POINT('Ctrl Pts',(43.498020080816,43.4024113680751,45.9070732590401));
#28577=CARTESIAN_POINT('Ctrl Pts',(43.5680773264276,43.3981896483933,45.9438276570717));
#28578=CARTESIAN_POINT('Ctrl Pts',(43.6363392466317,43.3939679287114,45.9841308267216));
#28579=CARTESIAN_POINT('Ctrl Pts',(43.7024295013073,43.3897462090296,46.0277759166301));
#28580=CARTESIAN_POINT('Ctrl Pts',(43.7684981315458,43.3855258706757,46.0714067260595));
#28581=CARTESIAN_POINT('Ctrl Pts',(43.8323961158317,43.3813055323218,46.1183770260475));
#28582=CARTESIAN_POINT('Ctrl Pts',(43.893774704883,43.3770851939678,46.1684357581696));
#28583=CARTESIAN_POINT('Ctrl Pts',(43.9551523783777,43.3728649185668,46.2184937435884));
#28584=CARTESIAN_POINT('Ctrl Pts',(44.0140103684607,43.3686446431657,46.2716397718904));
#28585=CARTESIAN_POINT('Ctrl Pts',(44.0700329112701,43.3644243677647,46.3275824336683));
#28586=CARTESIAN_POINT('Ctrl Pts',(44.1261114896733,43.360199871105,46.3835810511404));
#28587=CARTESIAN_POINT('Ctrl Pts',(44.1793486224083,43.3559753744454,46.4423815575808));
#28588=CARTESIAN_POINT('Ctrl Pts',(44.2294658038304,43.3517508777858,46.50365601765));
#28589=CARTESIAN_POINT('Ctrl Pts',(44.2796070463803,43.3475243529564,46.5649598954272));
#28590=CARTESIAN_POINT('Ctrl Pts',(44.3266250747688,43.343297828127,46.6287397146439));
#28591=CARTESIAN_POINT('Ctrl Pts',(44.3702836346383,43.3390713032976,46.6946368934368));
#28592=CARTESIAN_POINT('Ctrl Pts',(44.4140220008917,43.3348370525225,46.7606545300633));
#28593=CARTESIAN_POINT('Ctrl Pts',(44.4543883876324,43.3306028017473,46.8287968554796));
#28594=CARTESIAN_POINT('Ctrl Pts',(44.4911916986327,43.3263685509722,46.8986791019554));
#28595=CARTESIAN_POINT('Ctrl Pts',(44.5262923660251,43.3223301907249,46.9653283632178));
#28596=CARTESIAN_POINT('Ctrl Pts',(44.5581522286103,43.3182918304776,47.0335597774958));
#28597=CARTESIAN_POINT('Ctrl Pts',(44.5866470694326,43.3142534702303,47.1030245072234));
#28598=CARTESIAN_POINT('Ctrl Pts',(44.6165329385733,43.3100179699639,47.1758802861161));
#28599=CARTESIAN_POINT('Ctrl Pts',(44.6428304603488,43.3057824696975,47.250369808548));
#28600=CARTESIAN_POINT('Ctrl Pts',(44.6653601119542,43.3015469694311,47.326105346462));
#28601=CARTESIAN_POINT('Ctrl Pts',(44.687857102716,43.2973176092956,47.4017310918857));
#28602=CARTESIAN_POINT('Ctrl Pts',(44.7065969376097,43.2930882491602,47.4785988196821));
#28603=CARTESIAN_POINT('Ctrl Pts',(44.7214481703021,43.2888588890248,47.556300965179));
#28604=CARTESIAN_POINT('Ctrl Pts',(44.7362820598338,43.2846344679051,47.6339123706798));
#28605=CARTESIAN_POINT('Ctrl Pts',(44.747236283483,43.2804100467855,47.7123557989017));
#28606=CARTESIAN_POINT('Ctrl Pts',(44.7542296489309,43.2761856256658,47.791210151122));
#28607=CARTESIAN_POINT('Ctrl Pts',(44.7612185422539,43.2719639059836,47.8700140774744));
#28608=CARTESIAN_POINT('Ctrl Pts',(44.7642515632779,43.2677421863014,47.9492279400133));
#28609=CARTESIAN_POINT('Ctrl Pts',(44.7632990829994,43.2635204666192,48.028423321309));
#28610=CARTESIAN_POINT('Ctrl Pts',(44.7623469143682,43.2593001282649,48.1075927902289));
#28611=CARTESIAN_POINT('Ctrl Pts',(44.7574118394623,43.2550797899105,48.1867433209506));
#28612=CARTESIAN_POINT('Ctrl Pts',(44.7485163350697,43.2508594515562,48.2654457850688));
#28613=CARTESIAN_POINT('Ctrl Pts',(44.7396209633673,43.2466391761548,48.344147075218));
#28614=CARTESIAN_POINT('Ctrl Pts',(44.7267653336476,43.2424189007533,48.4223998458172));
#28615=CARTESIAN_POINT('Ctrl Pts',(44.7100237038394,43.2381986253519,48.4997808805869));
#28616=CARTESIAN_POINT('Ctrl Pts',(44.6932653285012,43.2339741286918,48.5772393144182));
#28617=CARTESIAN_POINT('Ctrl Pts',(44.6726132879773,43.2297496320318,48.6538238107783));
#28618=CARTESIAN_POINT('Ctrl Pts',(44.6481927159089,43.2255251353718,48.7291227283758));
#28619=CARTESIAN_POINT('Ctrl Pts',(44.6237604195877,43.221298610542,48.8044577967868));
#28620=CARTESIAN_POINT('Ctrl Pts',(44.595556154744,43.2170720857122,48.8785056176767));
#28621=CARTESIAN_POINT('Ctrl Pts',(44.5637536871924,43.2128455608824,48.9508735047636));
#28622=CARTESIAN_POINT('Ctrl Pts',(44.5318930857963,43.2086113101068,49.0233736779219));
#28623=CARTESIAN_POINT('Ctrl Pts',(44.4964213492767,43.2043770593313,49.0941873602226));
#28624=CARTESIAN_POINT('Ctrl Pts',(44.4575586966613,43.2001428085558,49.1629456783073));
#28625=CARTESIAN_POINT('Ctrl Pts',(44.4204939596841,43.196104448312,49.2285230077814));
#28626=CARTESIAN_POINT('Ctrl Pts',(44.380345339802,43.1920660880683,49.292230660774));
#28627=CARTESIAN_POINT('Ctrl Pts',(44.3373390188821,43.1880277278245,49.3537754491853));
#28628=CARTESIAN_POINT('Ctrl Pts',(44.2922332648856,43.1837922275583,49.4183246602425));
#28629=CARTESIAN_POINT('Ctrl Pts',(44.2438122213345,43.1795567272921,49.480739811804));
#28630=CARTESIAN_POINT('Ctrl Pts',(44.1923048580973,43.1753212270259,49.5406601625734));
#28631=CARTESIAN_POINT('Ctrl Pts',(44.1408721641878,43.1710918668906,49.6004936478535));
#28632=CARTESIAN_POINT('Ctrl Pts',(44.0863623388966,43.1668625067554,49.6578391614924));
#28633=CARTESIAN_POINT('Ctrl Pts',(44.0290470442044,43.1626331466202,49.7123656644154));
#28634=CARTESIAN_POINT('Ctrl Pts',(43.9717986818932,43.1584087255008,49.7668284916881));
#28635=CARTESIAN_POINT('Ctrl Pts',(43.9117516988982,43.1541843043813,49.8184785282764));
#28636=CARTESIAN_POINT('Ctrl Pts',(43.8492163267107,43.1499598832618,49.8670196783364));
#28637=CARTESIAN_POINT('Ctrl Pts',(43.7867209447117,43.1457381635798,49.9155297872484));
#28638=CARTESIAN_POINT('Ctrl Pts',(43.7217407016284,43.1415164438979,49.960934668518));
#28639=CARTESIAN_POINT('Ctrl Pts',(43.6546198795043,43.1372947242159,50.0029776331384));
#28640=CARTESIAN_POINT('Ctrl Pts',(43.5875210190141,43.1330743858617,50.0450068414881));
#28641=CARTESIAN_POINT('Ctrl Pts',(43.5182833676833,43.1288540475076,50.0836760684711));
#28642=CARTESIAN_POINT('Ctrl Pts',(43.4472799942956,43.1246337091535,50.1187720628818));
#28643=CARTESIAN_POINT('Ctrl Pts',(43.3762776800328,43.1204134337522,50.1538675337815));
#28644=CARTESIAN_POINT('Ctrl Pts',(43.3035101174174,43.116193158351,50.1853896712794));
#28645=CARTESIAN_POINT('Ctrl Pts',(43.2293734161261,43.1119728829497,50.2131719719722));
#28646=CARTESIAN_POINT('Ctrl Pts',(43.1551625608627,43.1077483862899,50.2409820614379));
#28647=CARTESIAN_POINT('Ctrl Pts',(43.0795802718135,43.1035238896301,50.2650446764673));
#28648=CARTESIAN_POINT('Ctrl Pts',(43.0030404470927,43.0992993929703,50.2852423635296));
#28649=CARTESIAN_POINT('Ctrl Pts',(42.9264638758024,43.0950728681406,50.3054497474486));
#28650=CARTESIAN_POINT('Ctrl Pts',(42.8489293129374,43.090846343311,50.3217884100212));
#28651=CARTESIAN_POINT('Ctrl Pts',(42.7708610245089,43.0866198184814,50.3341920532382));
#28652=CARTESIAN_POINT('Ctrl Pts',(42.6926500298663,43.0823855677061,50.3466183698991));
#28653=CARTESIAN_POINT('Ctrl Pts',(42.6139038280005,43.0781513169308,50.3550952433692));
#28654=CARTESIAN_POINT('Ctrl Pts',(42.5350517883784,43.0739170661555,50.3596083266839));
#28655=CARTESIAN_POINT('Ctrl Pts',(42.4598477064768,43.0698787059099,50.3639126197478));
#28656=CARTESIAN_POINT('Ctrl Pts',(42.3845477205658,43.0658403456642,50.3646118016675));
#28657=CARTESIAN_POINT('Ctrl Pts',(42.3095207725316,43.0618019854186,50.3617374854748));
#28658=CARTESIAN_POINT('Ctrl Pts',(42.2308312453366,43.0575664851523,50.3587228542237));
#28659=CARTESIAN_POINT('Ctrl Pts',(42.1521429786395,43.0533309848861,50.3517654633841));
#28660=CARTESIAN_POINT('Ctrl Pts',(42.0738832367456,43.0490954846199,50.3408627250705));
#28661=CARTESIAN_POINT('Ctrl Pts',(41.9957369466373,43.0448661244846,50.3299757922668));
#28662=CARTESIAN_POINT('Ctrl Pts',(41.918018408619,43.0406367643494,50.3151549341235));
#28663=CARTESIAN_POINT('Ctrl Pts',(41.8411530026631,43.0364074042142,50.2964495366691));
#28664=CARTESIAN_POINT('Ctrl Pts',(41.7643773595648,43.0321829830947,50.2777659832406));
#28665=CARTESIAN_POINT('Ctrl Pts',(41.6884533224055,43.0279585619752,50.2552070154485));
#28666=CARTESIAN_POINT('Ctrl Pts',(41.6137977486969,43.0237341408558,50.2288733613523));
#28667=CARTESIAN_POINT('Ctrl Pts',(41.5391899158165,43.0195124211738,50.2025565471302));
#28668=CARTESIAN_POINT('Ctrl Pts',(41.4658493778377,43.0152907014918,50.1724699932682));
#28669=CARTESIAN_POINT('Ctrl Pts',(41.3941782710748,43.0110689818097,50.1387643840596));
#28670=CARTESIAN_POINT('Ctrl Pts',(41.3225306147789,43.0068486434556,50.1050698031764));
#28671=CARTESIAN_POINT('Ctrl Pts',(41.2525517294732,43.0026283051015,50.0677587178443));
#28672=CARTESIAN_POINT('Ctrl Pts',(41.1846227924436,42.9984079667474,50.0270295222942));
#28673=CARTESIAN_POINT('Ctrl Pts',(41.1166948686789,42.9941876913461,49.9863009342829));
#28674=CARTESIAN_POINT('Ctrl Pts',(41.0508172342608,42.9899674159448,49.9421545799041));
#28675=CARTESIAN_POINT('Ctrl Pts',(40.9873442151886,42.9857471405436,49.8948335215894));
#28676=CARTESIAN_POINT('Ctrl Pts',(40.9238077083106,42.9815226438837,49.8474651311925));
#28677=CARTESIAN_POINT('Ctrl Pts',(40.8626809986058,42.9772981472239,49.7969159747142));
#28678=CARTESIAN_POINT('Ctrl Pts',(40.8042867831472,42.9730736505641,49.7434706107248));
#28679=CARTESIAN_POINT('Ctrl Pts',(40.7458645327784,42.9688471257345,49.6899995877559));
#28680=CARTESIAN_POINT('Ctrl Pts',(40.6901777203547,42.9646206009049,49.6336299216627));
#28681=CARTESIAN_POINT('Ctrl Pts',(40.6375116286636,42.9603940760752,49.5746825654093));
#28682=CARTESIAN_POINT('Ctrl Pts',(40.5847492651227,42.9561598252999,49.5156274553649));
#28683=CARTESIAN_POINT('Ctrl Pts',(40.5350189515994,42.9519255745246,49.453985605871));
#28684=CARTESIAN_POINT('Ctrl Pts',(40.488565039521,42.9476913237493,49.3901103671143));
#28685=CARTESIAN_POINT('Ctrl Pts',(40.4442602399847,42.9436529635038,49.329190209439));
#28686=CARTESIAN_POINT('Ctrl Pts',(40.4029355568504,42.9396146032582,49.2662390593534));
#28687=CARTESIAN_POINT('Ctrl Pts',(40.3647639970915,42.9355762430127,49.2015843097199));
#28688=CARTESIAN_POINT('Ctrl Pts',(40.3232516974056,42.9311844491795,49.1312710356526));
#28689=CARTESIAN_POINT('Ctrl Pts',(40.2853206180267,42.9267926553463,49.0586920893796));
#28690=CARTESIAN_POINT('Ctrl Pts',(40.2512151199357,42.9224008615132,48.9842326859574));
#28691=CARTESIAN_POINT('Ctrl Pts',(40.2161405322847,42.9178842771978,48.907657558252));
#28692=CARTESIAN_POINT('Ctrl Pts',(40.1851125221882,42.9133676928824,48.8290938244295));
#28693=CARTESIAN_POINT('Ctrl Pts',(40.1583484050748,42.9088511085669,48.7489917008013));
#28694=CARTESIAN_POINT('Ctrl Pts',(40.1324271131578,42.9044767553981,48.6714120623272));
#28695=CARTESIAN_POINT('Ctrl Pts',(40.1105053531251,42.9001024022292,48.5923899091533));
#28696=CARTESIAN_POINT('Ctrl Pts',(40.0927330828449,42.8957280490603,48.5123571155957));
#28697=CARTESIAN_POINT('Ctrl Pts',(40.0740940202823,42.8911403491716,48.4284209485972));
#28698=CARTESIAN_POINT('Ctrl Pts',(40.0600197140069,42.886552649283,48.3433734694791));
#28699=CARTESIAN_POINT('Ctrl Pts',(40.050624681986,42.8819649493943,48.2577325280336));
#28700=CARTESIAN_POINT('Ctrl Pts',(40.0412296499651,42.8773772495056,48.1720915865882));
#28701=CARTESIAN_POINT('Ctrl Pts',(40.0365140211838,42.872789549617,48.085857708865));
#28702=CARTESIAN_POINT('Ctrl Pts',(40.0365300407225,42.8682018497283,47.9995612600632));
#28703=CARTESIAN_POINT('',(40.0365308527828,42.0744518497637,47.9979922519359));
#28704=CARTESIAN_POINT('Ctrl Pts',(40.0365300407226,42.8682018496837,47.9995612592237));
#28705=CARTESIAN_POINT('Ctrl Pts',(40.0365457119377,42.8637139118291,47.9151413737289));
#28706=CARTESIAN_POINT('Ctrl Pts',(40.0410886773983,42.8592259739746,47.830834979817));
#28707=CARTESIAN_POINT('Ctrl Pts',(40.0500971862548,42.8547380361201,47.7471221503326));
#28708=CARTESIAN_POINT('Ctrl Pts',(40.0591375370619,42.8502342349637,47.6631134250652));
#28709=CARTESIAN_POINT('Ctrl Pts',(40.0726749541952,42.8457304338073,47.5797028312392));
#28710=CARTESIAN_POINT('Ctrl Pts',(40.0905962313369,42.8412266326509,47.4973622833642));
#28711=CARTESIAN_POINT('Ctrl Pts',(40.1085512889131,42.8367143421241,47.4148665289462));
#28712=CARTESIAN_POINT('Ctrl Pts',(40.1309065954803,42.8322020515973,47.3334452030884));
#28713=CARTESIAN_POINT('Ctrl Pts',(40.1574993385981,42.8276897610705,47.253554272226));
#28714=CARTESIAN_POINT('Ctrl Pts',(40.1841701190507,42.8231642290693,47.1734288986327));
#28715=CARTESIAN_POINT('Ctrl Pts',(40.2151030608842,42.8186386970682,47.0948432455739));
#28716=CARTESIAN_POINT('Ctrl Pts',(40.2500872145016,42.814113165067,47.0182335024811));
#28717=CARTESIAN_POINT('Ctrl Pts',(40.2623596416297,42.812525610247,46.9913588351764));
#28718=CARTESIAN_POINT('Ctrl Pts',(40.2751302065365,42.8109380554269,46.9647270873352));
#28719=CARTESIAN_POINT('Ctrl Pts',(40.2883885151456,42.8093505006069,46.9383562848436));
#28720=CARTESIAN_POINT('Ctrl Pts',(40.3237608808337,42.8051150003407,46.8680005783414));
#28721=CARTESIAN_POINT('Ctrl Pts',(40.3627205485394,42.8008795000744,46.7992809094294));
#28722=CARTESIAN_POINT('Ctrl Pts',(40.4050927052958,42.7966439998082,46.7325871523312));
#28723=CARTESIAN_POINT('Ctrl Pts',(40.4474034358743,42.7924146396729,46.6659900800113));
#28724=CARTESIAN_POINT('Ctrl Pts',(40.4931165820223,42.7881852795377,46.601413480092));
#28725=CARTESIAN_POINT('Ctrl Pts',(40.5420108170025,42.7839559194024,46.5392239607783));
#28726=CARTESIAN_POINT('Ctrl Pts',(40.5908479536534,42.7797314982829,46.4771070659295));
#28727=CARTESIAN_POINT('Ctrl Pts',(40.6428585084515,42.7755070771634,46.4173720792295));
#28728=CARTESIAN_POINT('Ctrl Pts',(40.697777968431,42.771282656044,46.3603565643284));
#28729=CARTESIAN_POINT('Ctrl Pts',(40.7526623084538,42.7670609363619,46.3033775097715));
#28730=CARTESIAN_POINT('Ctrl Pts',(40.8104515368487,42.7628392166799,46.2491148124934));
#28731=CARTESIAN_POINT('Ctrl Pts',(40.8708417858123,42.7586174969979,46.1978719255052));
#28732=CARTESIAN_POINT('Ctrl Pts',(40.9312122753554,42.7543971586437,46.1466458049614));
#28733=CARTESIAN_POINT('Ctrl Pts',(40.9941817379733,42.7501768202896,46.0984378361704));
#28734=CARTESIAN_POINT('Ctrl Pts',(41.0594115816624,42.7459564819354,46.0535126166555));
#28735=CARTESIAN_POINT('Ctrl Pts',(41.1246404523477,42.7417362065341,46.0085880672698));
#28736=CARTESIAN_POINT('Ctrl Pts',(41.1921292497807,42.7375159311329,45.966946434947));
#28737=CARTESIAN_POINT('Ctrl Pts',(41.2615098689342,42.7332956557316,45.9288093611727));
#28738=CARTESIAN_POINT('Ctrl Pts',(41.3309598848699,42.7290711590718,45.8906341414402));
#28739=CARTESIAN_POINT('Ctrl Pts',(41.4023050902673,42.7248466624119,45.8559707093128));
#28740=CARTESIAN_POINT('Ctrl Pts',(41.4751527346609,42.7206221657521,45.8249947180076));
#28741=CARTESIAN_POINT('Ctrl Pts',(41.548035353018,42.7163956409224,45.79400385521));
#28742=CARTESIAN_POINT('Ctrl Pts',(41.6224214061022,42.7121691160928,45.7667041218784));
#28743=CARTESIAN_POINT('Ctrl Pts',(41.6979005394215,42.7079425912632,45.7432220338821));
#28744=CARTESIAN_POINT('Ctrl Pts',(41.7735176460661,42.7037083404878,45.7196970214162));
#28745=CARTESIAN_POINT('Ctrl Pts',(41.85023136984,42.6994740897125,45.7000037160322));
#28746=CARTESIAN_POINT('Ctrl Pts',(41.9276188479409,42.6952398389372,45.6842179532436));
#28747=CARTESIAN_POINT('Ctrl Pts',(42.0014261238054,42.6912014786918,45.6691624923672));
#28748=CARTESIAN_POINT('Ctrl Pts',(42.0758458337977,42.6871631184464,45.6576610360458));
#28749=CARTESIAN_POINT('Ctrl Pts',(42.1505083191468,42.683124758201,45.6497352612769));
#28750=CARTESIAN_POINT('Ctrl Pts',(42.2288155917424,42.6788892579347,45.6414225751608));
#28751=CARTESIAN_POINT('Ctrl Pts',(42.3076876106676,42.6746537576685,45.6370119931367));
#28752=CARTESIAN_POINT('Ctrl Pts',(42.3867019084308,42.6704182574022,45.6365674112299));
#28753=CARTESIAN_POINT('Ctrl Pts',(42.4656016605423,42.666188897267,45.6361234738257));
#28754=CARTESIAN_POINT('Ctrl Pts',(42.5446428165234,42.6619595371317,45.6396341217822));
#28755=CARTESIAN_POINT('Ctrl Pts',(42.6233973127031,42.6577301769965,45.6471115450203));
#28756=CARTESIAN_POINT('Ctrl Pts',(42.7020598399593,42.653505755877,45.6545802361783));
#28757=CARTESIAN_POINT('Ctrl Pts',(42.78043590782,42.6492813347575,45.6660064531012));
#28758=CARTESIAN_POINT('Ctrl Pts',(42.8580985165179,42.645056913638,45.681350352023));
#28759=CARTESIAN_POINT('Ctrl Pts',(42.9357114614455,42.640835193956,45.6966844388113));
#28760=CARTESIAN_POINT('Ctrl Pts',(43.0126113935494,42.636613474274,45.7159311444201));
#28761=CARTESIAN_POINT('Ctrl Pts',(43.0883787104353,42.6323917545919,45.7389990729946));
#28762=CARTESIAN_POINT('Ctrl Pts',(43.1641212365924,42.6281714162378,45.7620594538455));
#28763=CARTESIAN_POINT('Ctrl Pts',(43.2387314347309,42.6239510778836,45.7889384384078));
#28764=CARTESIAN_POINT('Ctrl Pts',(43.3118035955149,42.6197307395295,45.8194944063117));
#28765=CARTESIAN_POINT('Ctrl Pts',(43.3848746663147,42.6155104641282,45.8500499184261));
#28766=CARTESIAN_POINT('Ctrl Pts',(43.4564073128616,42.6112901887269,45.8842821225544));
#28767=CARTESIAN_POINT('Ctrl Pts',(43.5260159867585,42.6070699133256,45.9220013381948));
#28768=CARTESIAN_POINT('Ctrl Pts',(43.5956942855454,42.6028454166658,45.9597582818379));
#28769=CARTESIAN_POINT('Ctrl Pts',(43.6634443537622,42.598620920006,46.0010089802159));
#28770=CARTESIAN_POINT('Ctrl Pts',(43.7289059874642,42.5943964233461,46.0455181460597));
#28771=CARTESIAN_POINT('Ctrl Pts',(43.7943990491254,42.5901698985165,46.0900486806377));
#28772=CARTESIAN_POINT('Ctrl Pts',(43.8576011127006,42.5859433736868,46.137840515644));
#28773=CARTESIAN_POINT('Ctrl Pts',(43.9181837765053,42.5817168488572,46.1886169754423));
#28774=CARTESIAN_POINT('Ctrl Pts',(43.9788771833885,42.5774825980819,46.2394862529068));
#28775=CARTESIAN_POINT('Ctrl Pts',(44.036941277607,42.5732483473065,46.2933507370757));
#28776=CARTESIAN_POINT('Ctrl Pts',(44.0920835141889,42.5690140965312,46.3498958148316));
#28777=CARTESIAN_POINT('Ctrl Pts',(44.144674687425,42.5649757362859,46.4038249291412));
#28778=CARTESIAN_POINT('Ctrl Pts',(44.194608164733,42.5609373760405,46.4601918039581));
#28779=CARTESIAN_POINT('Ctrl Pts',(44.2416657329005,42.5568990157952,46.5186972729519));
#28780=CARTESIAN_POINT('Ctrl Pts',(44.2910205032515,42.5526635155289,46.5800587945713));
#28781=CARTESIAN_POINT('Ctrl Pts',(44.3373990175007,42.5484280152627,46.6440062888083));
#28782=CARTESIAN_POINT('Ctrl Pts',(44.3805189859801,42.5441925149964,46.710219015851));
#28783=CARTESIAN_POINT('Ctrl Pts',(44.423576444192,42.5399631548612,46.7763357554562));
#28784=CARTESIAN_POINT('Ctrl Pts',(44.4633844834144,42.5357337947259,46.844710816708));
#28785=CARTESIAN_POINT('Ctrl Pts',(44.4997012727788,42.5315044345906,46.9149907806884));
#28786=CARTESIAN_POINT('Ctrl Pts',(44.5359756516626,42.5272800134711,46.9851886722418));
#28787=CARTESIAN_POINT('Ctrl Pts',(44.5687666682094,42.5230555923516,47.057286631161));
#28788=CARTESIAN_POINT('Ctrl Pts',(44.5978768289048,42.5188311712321,47.1309039835189));
#28789=CARTESIAN_POINT('Ctrl Pts',(44.6269683742027,42.5146094515501,47.2044742589714));
#28790=CARTESIAN_POINT('Ctrl Pts',(44.65238356339,42.5103877318681,47.27956156411));
#28791=CARTESIAN_POINT('Ctrl Pts',(44.6739722616212,42.506166012186,47.3557635571646));
#28792=CARTESIAN_POINT('Ctrl Pts',(44.6955538961266,42.5019456738319,47.4319406172664));
#28793=CARTESIAN_POINT('Ctrl Pts',(44.7133113979149,42.4977253354777,47.5092311898326));
#28794=CARTESIAN_POINT('Ctrl Pts',(44.7271443883942,42.4935049971236,47.5872174465103));
#28795=CARTESIAN_POINT('Ctrl Pts',(44.740977172533,42.4892847217223,47.6652025399025));
#28796=CARTESIAN_POINT('Ctrl Pts',(44.7508854810686,42.485064446321,47.7438828344079));
#28797=CARTESIAN_POINT('Ctrl Pts',(44.7568202622255,42.4808441709197,47.8228314574665));
#28798=CARTESIAN_POINT('Ctrl Pts',(44.7627609795461,42.4766196742598,47.9018590475401));
#28799=CARTESIAN_POINT('Ctrl Pts',(44.7647201947495,42.4723951776,47.9811550331627));
#28800=CARTESIAN_POINT('Ctrl Pts',(44.7627009237643,42.4681706809401,48.060289184297));
#28801=CARTESIAN_POINT('Ctrl Pts',(44.7606806833325,42.4639441561105,48.1394613275303));
#28802=CARTESIAN_POINT('Ctrl Pts',(44.7546781872409,42.4597176312808,48.2184710128488));
#28803=CARTESIAN_POINT('Ctrl Pts',(44.7447484649486,42.4554911064512,48.296892366054));
#28804=CARTESIAN_POINT('Ctrl Pts',(44.7348005914569,42.4512568556758,48.3754570708638));
#28805=CARTESIAN_POINT('Ctrl Pts',(44.7209112292878,42.4470226049005,48.4534308312628));
#28806=CARTESIAN_POINT('Ctrl Pts',(44.703186712563,42.4427883541251,48.5303974056998));
#28807=CARTESIAN_POINT('Ctrl Pts',(44.6862821909592,42.4387499938799,48.603803250302));
#28808=CARTESIAN_POINT('Ctrl Pts',(44.6658896534714,42.4347116336346,48.6762927057238));
#28809=CARTESIAN_POINT('Ctrl Pts',(44.6421426558893,42.4306732733893,48.7475204020907));
#28810=CARTESIAN_POINT('Ctrl Pts',(44.6172364047199,42.426437773123,48.8222252101321));
#28811=CARTESIAN_POINT('Ctrl Pts',(44.5885451487791,42.4222022728568,48.8958258924366));
#28812=CARTESIAN_POINT('Ctrl Pts',(44.5561859229428,42.4179667725905,48.9679115179619));
#28813=CARTESIAN_POINT('Ctrl Pts',(44.5238736077129,42.4137374124553,49.039892642211));
#28814=CARTESIAN_POINT('Ctrl Pts',(44.4879040725767,42.40950805232,49.1103626466809));
#28815=CARTESIAN_POINT('Ctrl Pts',(44.4484437243221,42.4052786921848,49.1789269481972));
#28816=CARTESIAN_POINT('Ctrl Pts',(44.4090294575729,42.4010542710653,49.2474111808247));
#28817=CARTESIAN_POINT('Ctrl Pts',(44.3661327114626,42.3968298499458,49.3139937282349));
#28818=CARTESIAN_POINT('Ctrl Pts',(44.3199668011377,42.3926054288263,49.3783025514846));
#28819=CARTESIAN_POINT('Ctrl Pts',(44.2738304130399,42.3883837091443,49.4425702504574));
#28820=CARTESIAN_POINT('Ctrl Pts',(44.2244292830312,42.3841619894622,49.5045667309079));
#28821=CARTESIAN_POINT('Ctrl Pts',(44.172020570159,42.3799402697802,49.5639480617441));
#28822=CARTESIAN_POINT('Ctrl Pts',(44.1196290051843,42.3757199314261,49.6233099632733));
#28823=CARTESIAN_POINT('Ctrl Pts',(44.0642321217211,42.3714995930719,49.680058062624));
#28824=CARTESIAN_POINT('Ctrl Pts',(44.006127021177,42.3672792547178,49.7338818970003));
#28825=CARTESIAN_POINT('Ctrl Pts',(43.9480227873603,42.3630589793165,49.7877049285108));
#28826=CARTESIAN_POINT('Ctrl Pts',(43.8872107619944,42.3588387039152,49.8386034637785));
#28827=CARTESIAN_POINT('Ctrl Pts',(43.8240234202902,42.3546184285139,49.8863053144613));
#28828=CARTESIAN_POINT('Ctrl Pts',(43.7607728765241,42.3503939318541,49.9340548781075));
#28829=CARTESIAN_POINT('Ctrl Pts',(43.6951426458085,42.3461694351942,49.9786010864343));
#28830=CARTESIAN_POINT('Ctrl Pts',(43.6274961952718,42.3419449385344,50.0197137251337));
#28831=CARTESIAN_POINT('Ctrl Pts',(43.5598172678509,42.3377184137047,50.0608461019034));
#28832=CARTESIAN_POINT('Ctrl Pts',(43.4901206056763,42.3334918888751,50.0985414015462));
#28833=CARTESIAN_POINT('Ctrl Pts',(43.4187941513704,42.3292653640454,50.1326155110646));
#28834=CARTESIAN_POINT('Ctrl Pts',(43.3473373146972,42.3250311132701,50.166751906913));
#28835=CARTESIAN_POINT('Ctrl Pts',(43.2742451670299,42.3207968624948,50.1972537042632));
#28836=CARTESIAN_POINT('Ctrl Pts',(43.1999253050504,42.3165626117194,50.2239851499594));
#28837=CARTESIAN_POINT('Ctrl Pts',(43.1290437271798,42.3125242514741,50.2494799100308));
#28838=CARTESIAN_POINT('Ctrl Pts',(43.0570458714223,42.3084858912288,50.2715453921));
#28839=CARTESIAN_POINT('Ctrl Pts',(42.9842944560811,42.3044475309835,50.2901070781719));
#28840=CARTESIAN_POINT('Ctrl Pts',(42.9079915459072,42.3002120307172,50.3095748872636));
#28841=CARTESIAN_POINT('Ctrl Pts',(42.8305695810991,42.295976530451,50.3252620784841));
#28842=CARTESIAN_POINT('Ctrl Pts',(42.7524374810683,42.2917410301847,50.3370447712524));
#28843=CARTESIAN_POINT('Ctrl Pts',(42.6744186477825,42.2875116700495,50.3488103828562));
#28844=CARTESIAN_POINT('Ctrl Pts',(42.5956921837992,42.2832823099142,50.3566826669339));
#28845=CARTESIAN_POINT('Ctrl Pts',(42.5166799692987,42.2790529497789,50.3605881101252));
#28846=CARTESIAN_POINT('Ctrl Pts',(42.4377600246832,42.2748285286594,50.3644889925686));
#28847=CARTESIAN_POINT('Ctrl Pts',(42.3585554590132,42.27060410754,50.3644322166106));
#28848=CARTESIAN_POINT('Ctrl Pts',(42.2794945691606,42.2663796864205,50.3603959163747));
#28849=CARTESIAN_POINT('Ctrl Pts',(42.2004842372526,42.2621579667384,50.3563621972764));
#28850=CARTESIAN_POINT('Ctrl Pts',(42.1216178662786,42.2579362470564,50.3483540287107));
#28851=CARTESIAN_POINT('Ctrl Pts',(42.0433238327958,42.2537145273744,50.33640162486));
#28852=CARTESIAN_POINT('Ctrl Pts',(41.9650554167722,42.2494941890202,50.3244531317827));
#28853=CARTESIAN_POINT('Ctrl Pts',(41.8873594300161,42.245273850666,50.3085630367748));
#28854=CARTESIAN_POINT('Ctrl Pts',(41.8106577097856,42.2410535123119,50.2888132527283));
#28855=CARTESIAN_POINT('Ctrl Pts',(41.7339571336798,42.2368332369106,50.2690637632804));
#28856=CARTESIAN_POINT('Ctrl Pts',(41.6582512488118,42.2326129615093,50.2454548175639));
#28857=CARTESIAN_POINT('Ctrl Pts',(41.583948839476,42.228392686108,50.2181187849859));
#28858=CARTESIAN_POINT('Ctrl Pts',(41.5095721104213,42.2241681894482,50.1907554100071));
#28859=CARTESIAN_POINT('Ctrl Pts',(41.4366021027103,42.2199436927883,50.1596576635497));
#28860=CARTESIAN_POINT('Ctrl Pts',(41.3654290656604,42.2157191961285,50.1250066876882));
#28861=CARTESIAN_POINT('Ctrl Pts',(41.2942218586215,42.2114926712988,50.0903390759839));
#28862=CARTESIAN_POINT('Ctrl Pts',(41.2248137525836,42.2072661464692,50.0521150632474));
#28863=CARTESIAN_POINT('Ctrl Pts',(41.157569465402,42.2030396216395,50.0105613165478));
#28864=CARTESIAN_POINT('Ctrl Pts',(41.0902022579178,42.1988053708642,49.9689316109924));
#28865=CARTESIAN_POINT('Ctrl Pts',(41.0250071604507,42.1945711200888,49.9239602761392));
#28866=CARTESIAN_POINT('Ctrl Pts',(40.9623188515509,42.1903368693135,49.8759166709356));
#28867=CARTESIAN_POINT('Ctrl Pts',(40.9025307124117,42.1862985090682,49.8300957227703));
#28868=CARTESIAN_POINT('Ctrl Pts',(40.8450227954835,42.1822601488229,49.7814807433587));
#28869=CARTESIAN_POINT('Ctrl Pts',(40.7900540000068,42.1782217885776,49.7303364753729));
#28870=CARTESIAN_POINT('Ctrl Pts',(40.7312006102975,42.173898041127,49.6755778889956));
#28871=CARTESIAN_POINT('Ctrl Pts',(40.675011657768,42.1695742936764,49.617689584426));
#28872=CARTESIAN_POINT('Ctrl Pts',(40.6218435444555,42.1652505462258,49.5569682271985));
#28873=CARTESIAN_POINT('Ctrl Pts',(40.5706245486074,42.1610853052774,49.4984728857247));
#28874=CARTESIAN_POINT('Ctrl Pts',(40.5222091535806,42.156920064329,49.4373489697679));
#28875=CARTESIAN_POINT('Ctrl Pts',(40.4768817937906,42.1527548233806,49.3739020364808));
#28876=CARTESIAN_POINT('Ctrl Pts',(40.4315970956775,42.148593502717,49.3105148188396));
#28877=CARTESIAN_POINT('Ctrl Pts',(40.3893949493629,42.1444321820535,49.2448093115539));
#28878=CARTESIAN_POINT('Ctrl Pts',(40.3505201270085,42.1402708613899,49.1771247559638));
#28879=CARTESIAN_POINT('Ctrl Pts',(40.3116689089882,42.1361120674313,49.1094812976384));
#28880=CARTESIAN_POINT('Ctrl Pts',(40.2761412472426,42.1319532734726,49.0398615943417));
#28881=CARTESIAN_POINT('Ctrl Pts',(40.244138143138,42.127794479514,48.9686331065101));
#28882=CARTESIAN_POINT('Ctrl Pts',(40.2121437854714,42.1236368221524,48.8974240854012));
#28883=CARTESIAN_POINT('Ctrl Pts',(40.1836722700636,42.1194791647908,48.8246075950335));
#28884=CARTESIAN_POINT('Ctrl Pts',(40.1588774918835,42.1153215074292,48.7505733438604));
#28885=CARTESIAN_POINT('Ctrl Pts',(40.134070501267,42.1111618022522,48.6765026278083));
#28886=CARTESIAN_POINT('Ctrl Pts',(40.1129440199525,42.1070020970753,48.6012134126361));
#28887=CARTESIAN_POINT('Ctrl Pts',(40.095602460452,42.1028423918984,48.5251118172591));
#28888=CARTESIAN_POINT('Ctrl Pts',(40.0782556616417,42.0986814299727,48.4489872297263));
#28889=CARTESIAN_POINT('Ctrl Pts',(40.0646961483959,42.094520468047,48.3720502501643));
#28890=CARTESIAN_POINT('Ctrl Pts',(40.054977006387,42.0903595061213,48.2947161351649));
#28891=CARTESIAN_POINT('Ctrl Pts',(40.0452468055504,42.086193809687,48.2172940263222));
#28892=CARTESIAN_POINT('Ctrl Pts',(40.0393657308817,42.0820281132527,48.1394743631729));
#28893=CARTESIAN_POINT('Ctrl Pts',(40.0373348542212,42.0778624168184,48.0616753583057));
#28894=CARTESIAN_POINT('Ctrl Pts',(40.0367806098798,42.0767255611335,48.0404433164714));
#28895=CARTESIAN_POINT('Ctrl Pts',(40.0365128260987,42.0755887054486,48.0192127986881));
#28896=CARTESIAN_POINT('Ctrl Pts',(40.0365308527828,42.0744518497637,47.9979922519359));
#28897=CARTESIAN_POINT('',(40.0365304529153,41.2807018496994,48.001463182638));
#28898=CARTESIAN_POINT('Ctrl Pts',(40.0365308527833,42.0744518497283,47.997992251275));
#28899=CARTESIAN_POINT('Ctrl Pts',(40.0366334841975,42.067979385482,47.8771772419789));
#28900=CARTESIAN_POINT('Ctrl Pts',(40.0460029002097,42.0615069212358,47.7567426871142));
#28901=CARTESIAN_POINT('Ctrl Pts',(40.0644473300431,42.0550344569895,47.6378064512486));
#28902=CARTESIAN_POINT('Ctrl Pts',(40.0673334927678,42.0540216533836,47.6191954487035));
#28903=CARTESIAN_POINT('Ctrl Pts',(40.0704417825611,42.0530088497776,47.600621068999));
#28904=CARTESIAN_POINT('Ctrl Pts',(40.0737713756649,42.0519960461717,47.5820875352133));
#28905=CARTESIAN_POINT('Ctrl Pts',(40.0876955880151,42.0477605459054,47.5045811096588));
#28906=CARTESIAN_POINT('Ctrl Pts',(40.1055241028375,42.0435250456392,47.4276240264088));
#28907=CARTESIAN_POINT('Ctrl Pts',(40.1272000876839,42.0392895453729,47.351639761031));
#28908=CARTESIAN_POINT('Ctrl Pts',(40.1488446492325,42.0350601852377,47.2757656487196));
#28909=CARTESIAN_POINT('Ctrl Pts',(40.17432547699,42.0308308251024,47.2008620012471));
#28910=CARTESIAN_POINT('Ctrl Pts',(40.2035345311768,42.0266014649672,47.1273432031048));
#28911=CARTESIAN_POINT('Ctrl Pts',(40.2327094752443,42.0223770438477,47.0539102596762));
#28912=CARTESIAN_POINT('Ctrl Pts',(40.2656038215422,42.0181526227282,46.9818593857877));
#28913=CARTESIAN_POINT('Ctrl Pts',(40.3020598714922,42.0139282016087,46.9115893890187));
#28914=CARTESIAN_POINT('Ctrl Pts',(40.3384926084873,42.0097064819267,46.8413643285845));
#28915=CARTESIAN_POINT('Ctrl Pts',(40.3784823129429,42.0054847622447,46.7729183004168));
#28916=CARTESIAN_POINT('Ctrl Pts',(40.4218238615273,42.0012630425626,46.7066285892764));
#28917=CARTESIAN_POINT('Ctrl Pts',(40.4651512289501,41.9970427042085,46.6403605678342));
#28918=CARTESIAN_POINT('Ctrl Pts',(40.5118280061515,41.9928223658544,46.5762478549964));
#28919=CARTESIAN_POINT('Ctrl Pts',(40.5616047366716,41.9886020275002,46.5146403477031));
#28920=CARTESIAN_POINT('Ctrl Pts',(40.6113807246949,41.9843817520989,46.4530337593808));
#28921=CARTESIAN_POINT('Ctrl Pts',(40.6642562781117,41.9801614766977,46.3939326665623));
#28922=CARTESIAN_POINT('Ctrl Pts',(40.7199414386359,41.9759412012964,46.3376541661594));
#28923=CARTESIAN_POINT('Ctrl Pts',(40.775682297293,41.9717167046366,46.2813193741454));
#28924=CARTESIAN_POINT('Ctrl Pts',(40.8342380460026,41.9674922079767,46.2278131487776));
#28925=CARTESIAN_POINT('Ctrl Pts',(40.8952820300687,41.9632677113169,46.1774154966461));
#28926=CARTESIAN_POINT('Ctrl Pts',(40.9563553211919,41.9590411864873,46.1269936487335));
#28927=CARTESIAN_POINT('Ctrl Pts',(41.0199188504245,41.9548146616576,46.0796836277557));
#28928=CARTESIAN_POINT('Ctrl Pts',(41.0856151231092,41.950588136828,46.0357233300014));
#28929=CARTESIAN_POINT('Ctrl Pts',(41.1514314863779,41.9463538860527,45.9916826742967));
#28930=CARTESIAN_POINT('Ctrl Pts',(41.2193879796092,41.9421196352774,45.9510042190667));
#28931=CARTESIAN_POINT('Ctrl Pts',(41.2891007154644,41.937885384502,45.9138808230309));
#28932=CARTESIAN_POINT('Ctrl Pts',(41.3555883081961,41.9338470242567,45.8784748788205));
#28933=CARTESIAN_POINT('Ctrl Pts',(41.4236728992671,41.9298086640113,45.8463024497626));
#28934=CARTESIAN_POINT('Ctrl Pts',(41.4930062244249,41.9257703037659,45.8174893512361));
#28935=CARTESIAN_POINT('Ctrl Pts',(41.5657241840231,41.9215348034997,45.7872696880397));
#28936=CARTESIAN_POINT('Ctrl Pts',(41.640092325734,41.9172993032334,45.7606308423139));
#28937=CARTESIAN_POINT('Ctrl Pts',(41.715723748849,41.9130638029672,45.7377541130526));
#28938=CARTESIAN_POINT('Ctrl Pts',(41.7912455304067,41.9088344428319,45.7149105477873));
#28939=CARTESIAN_POINT('Ctrl Pts',(41.868026511167,41.9046050826967,45.6958184032925));
#28940=CARTESIAN_POINT('Ctrl Pts',(41.945659733541,41.9003757225614,45.6806109935645));
#28941=CARTESIAN_POINT('Ctrl Pts',(42.0232022964068,41.8961513014419,45.6654213429381));
#28942=CARTESIAN_POINT('Ctrl Pts',(42.1015946649512,41.8919268803224,45.6541075018368));
#28943=CARTESIAN_POINT('Ctrl Pts',(42.1804161172182,41.8877024592029,45.6467525928364));
#28944=CARTESIAN_POINT('Ctrl Pts',(42.2591871646564,41.8834807395209,45.6394023871612));
#28945=CARTESIAN_POINT('Ctrl Pts',(42.3383862851507,41.8792590198389,45.636006132267));
#28946=CARTESIAN_POINT('Ctrl Pts',(42.417585201652,41.8750373001569,45.6365954215195));
#28947=CARTESIAN_POINT('Ctrl Pts',(42.4967582046205,41.8708169618027,45.6371845179591));
#28948=CARTESIAN_POINT('Ctrl Pts',(42.5759305347451,41.8665966234485,45.6417565656403));
#28949=CARTESIAN_POINT('Ctrl Pts',(42.654672965057,41.8623762850944,45.6502910559456));
#28950=CARTESIAN_POINT('Ctrl Pts',(42.7334142208038,41.8581560096931,45.6588254189458));
#28951=CARTESIAN_POINT('Ctrl Pts',(42.8117251230099,41.8539357342918,45.6713220551797));
#28952=CARTESIAN_POINT('Ctrl Pts',(42.8891821193075,41.8497154588905,45.6877086483209));
#28953=CARTESIAN_POINT('Ctrl Pts',(42.9667165906458,41.8454909622307,45.7041116318728));
#28954=CARTESIAN_POINT('Ctrl Pts',(43.0433949896083,41.8412664655708,45.7244122474451));
#28955=CARTESIAN_POINT('Ctrl Pts',(43.1188051053835,41.837041968911,45.7484872504526));
#28956=CARTESIAN_POINT('Ctrl Pts',(43.1942514253581,41.8328154440813,45.7725738118061));
#28957=CARTESIAN_POINT('Ctrl Pts',(43.2684278091661,41.8285889192517,45.8004382051894));
#28958=CARTESIAN_POINT('Ctrl Pts',(43.3409407777844,41.824362394422,45.8319084674298));
#28959=CARTESIAN_POINT('Ctrl Pts',(43.4135862976784,41.8201281436467,45.8634362562546));
#28960=CARTESIAN_POINT('Ctrl Pts',(43.4845619047036,41.8158938928714,45.8985828762858));
#28961=CARTESIAN_POINT('Ctrl Pts',(43.5534977194812,41.811659642096,45.9371298024229));
#28962=CARTESIAN_POINT('Ctrl Pts',(43.6192443340884,41.8076212818507,45.973893419495));
#28963=CARTESIAN_POINT('Ctrl Pts',(43.683135434209,41.8035829216054,46.0137494611703));
#28964=CARTESIAN_POINT('Ctrl Pts',(43.7448767975816,41.7995445613601,46.0564730924871));
#28965=CARTESIAN_POINT('Ctrl Pts',(43.809632179746,41.7953090610938,46.1012823568481));
#28966=CARTESIAN_POINT('Ctrl Pts',(43.8722687283955,41.7910735608276,46.1494166624567));
#28967=CARTESIAN_POINT('Ctrl Pts',(43.9324246559972,41.7868380605613,46.2006486961708));
#28968=CARTESIAN_POINT('Ctrl Pts',(43.9924933765981,41.782608700426,46.2518064596976));
#28969=CARTESIAN_POINT('Ctrl Pts',(44.0500882630937,41.7783793402908,46.3060527318044));
#28970=CARTESIAN_POINT('Ctrl Pts',(44.1048770340794,41.7741499801555,46.3631173714745));
#28971=CARTESIAN_POINT('Ctrl Pts',(44.1596018231399,41.769925559036,46.4201153714766));
#28972=CARTESIAN_POINT('Ctrl Pts',(44.2115266852493,41.7657011379165,46.4799248618724));
#28973=CARTESIAN_POINT('Ctrl Pts',(44.2603541049907,41.761476716797,46.5422369722948));
#28974=CARTESIAN_POINT('Ctrl Pts',(44.3091503005201,41.757254997115,46.6045092353004));
#28975=CARTESIAN_POINT('Ctrl Pts',(44.3548526963495,41.7530332774329,46.6692805734822));
#28976=CARTESIAN_POINT('Ctrl Pts',(44.3972030273329,41.7488115577509,46.7362078855633));
#28977=CARTESIAN_POINT('Ctrl Pts',(44.4395395014766,41.7445912193968,46.803113299326));
#28978=CARTESIAN_POINT('Ctrl Pts',(44.4785258378359,41.7403708810426,46.8721728899318));
#28979=CARTESIAN_POINT('Ctrl Pts',(44.5139470765968,41.7361505426884,46.9430145704656));
#28980=CARTESIAN_POINT('Ctrl Pts',(44.5493677869951,41.7319302672871,47.0138551942863));
#28981=CARTESIAN_POINT('Ctrl Pts',(44.581223296794,41.7277099918859,47.086477434798));
#28982=CARTESIAN_POINT('Ctrl Pts',(44.6093452878274,41.7234897164846,47.160485950055));
#28983=CARTESIAN_POINT('Ctrl Pts',(44.6374954074031,41.7192652198247,47.2345684910684));
#28984=CARTESIAN_POINT('Ctrl Pts',(44.6619043811873,41.7150407231649,47.310039636938));
#28985=CARTESIAN_POINT('Ctrl Pts',(44.6824528587946,41.710816226505,47.3864860325305));
#28986=CARTESIAN_POINT('Ctrl Pts',(44.7030112016723,41.7065897016754,47.4629691298375));
#28987=CARTESIAN_POINT('Ctrl Pts',(44.7197052571245,41.7023631768457,47.5404279501617));
#28988=CARTESIAN_POINT('Ctrl Pts',(44.7324667822032,41.6981366520161,47.6184385359883));
#28989=CARTESIAN_POINT('Ctrl Pts',(44.7452516349219,41.6939024012407,47.6965917225504));
#28990=CARTESIAN_POINT('Ctrl Pts',(44.7540895403785,41.6896681504654,47.775298222405));
#28991=CARTESIAN_POINT('Ctrl Pts',(44.7589641827196,41.6854338996901,47.8541287363938));
#28992=CARTESIAN_POINT('Ctrl Pts',(44.763613307886,41.6813955394448,47.929312288502));
#28993=CARTESIAN_POINT('Ctrl Pts',(44.7646577996222,41.6773571791995,48.0046082762408));
#28994=CARTESIAN_POINT('Ctrl Pts',(44.7621275787021,41.6733188189542,48.0796476166296));
#28995=CARTESIAN_POINT('Ctrl Pts',(44.7594738403704,41.669083318688,48.1583501411424));
#28996=CARTESIAN_POINT('Ctrl Pts',(44.7528773781285,41.6648478184217,48.2370694862173));
#28997=CARTESIAN_POINT('Ctrl Pts',(44.7423336447328,41.6606123181555,48.3153784039098));
#28998=CARTESIAN_POINT('Ctrl Pts',(44.7318051964039,41.6563829580202,48.3935737985277));
#28999=CARTESIAN_POINT('Ctrl Pts',(44.717340902479,41.652153597885,48.4713594860876));
#29000=CARTESIAN_POINT('Ctrl Pts',(44.6989881977231,41.6479242377497,48.5483098646112));
#29001=CARTESIAN_POINT('Ctrl Pts',(44.6806569251213,41.6436998166302,48.6251703810468));
#29002=CARTESIAN_POINT('Ctrl Pts',(44.6584463735388,41.6394753955107,48.7011970727075));
#29003=CARTESIAN_POINT('Ctrl Pts',(44.6324553583148,41.6352509743912,48.7759726245376));
#29004=CARTESIAN_POINT('Ctrl Pts',(44.6064809638537,41.6310292547092,48.8507003588158));
#29005=CARTESIAN_POINT('Ctrl Pts',(44.5767310577221,41.6268075350272,48.9241780991155));
#29006=CARTESIAN_POINT('Ctrl Pts',(44.5433544784777,41.6225858153452,48.9960030223297));
#29007=CARTESIAN_POINT('Ctrl Pts',(44.5099888199012,41.618365476991,49.0678044447489));
#29008=CARTESIAN_POINT('Ctrl Pts',(44.4729990421105,41.6141451386369,49.1379536986034));
#29009=CARTESIAN_POINT('Ctrl Pts',(44.4325817892143,41.6099248002827,49.206068700802));
#29010=CARTESIAN_POINT('Ctrl Pts',(44.392165139204,41.6057045248814,49.2741826869601));
#29011=CARTESIAN_POINT('Ctrl Pts',(44.3483213563709,41.6014842494801,49.3402620788186));
#29012=CARTESIAN_POINT('Ctrl Pts',(44.3012918756923,41.5972639740789,49.4039514394474));
#29013=CARTESIAN_POINT('Ctrl Pts',(44.254215354577,41.593039477419,49.467704504274));
#29014=CARTESIAN_POINT('Ctrl Pts',(44.2039470497711,41.5888149807592,49.5290623838984));
#29015=CARTESIAN_POINT('Ctrl Pts',(44.1507700370006,41.5845904840993,49.5877010796875));
#29016=CARTESIAN_POINT('Ctrl Pts',(44.0975674940853,41.5803639592697,49.6463679277611));
#29017=CARTESIAN_POINT('Ctrl Pts',(44.0414537941184,41.57613743444,49.7023126595011));
#29018=CARTESIAN_POINT('Ctrl Pts',(43.9827485784147,41.5719109096104,49.7552485232657));
#29019=CARTESIAN_POINT('Ctrl Pts',(43.9239360515447,41.5676766588351,49.8082811520146));
#29020=CARTESIAN_POINT('Ctrl Pts',(43.862522907789,41.5634424080597,49.8582936251212));
#29021=CARTESIAN_POINT('Ctrl Pts',(43.7988613730507,41.5592081572844,49.9050399733041));
#29022=CARTESIAN_POINT('Ctrl Pts',(43.7381450327382,41.5551697970391,49.9496236798754));
#29023=CARTESIAN_POINT('Ctrl Pts',(43.6753840548971,41.5511314367937,49.9912366152817));
#29024=CARTESIAN_POINT('Ctrl Pts',(43.610905035557,41.5470930765484,50.0297042729824));
#29025=CARTESIAN_POINT('Ctrl Pts',(43.5432783536882,41.5428575762821,50.0700498005072));
#29026=CARTESIAN_POINT('Ctrl Pts',(43.4735045451748,41.5386220760159,50.1070884863463));
#29027=CARTESIAN_POINT('Ctrl Pts',(43.4019404775094,41.5343865757496,50.1405853686383));
#29028=CARTESIAN_POINT('Ctrl Pts',(43.3304801550268,41.5301572156144,50.1740336910832));
#29029=CARTESIAN_POINT('Ctrl Pts',(43.2572351487088,41.5259278554791,50.2039502088852));
#29030=CARTESIAN_POINT('Ctrl Pts',(43.1825890635681,41.5216984953438,50.2301445689649));
#29031=CARTESIAN_POINT('Ctrl Pts',(43.1080301495786,41.5174740742243,50.2563083394629));
#29032=CARTESIAN_POINT('Ctrl Pts',(43.0320738487144,41.5132496531048,50.2787584353536));
#29033=CARTESIAN_POINT('Ctrl Pts',(42.9551245929073,41.5090252319853,50.2973521992175));
#29034=CARTESIAN_POINT('Ctrl Pts',(42.8782245446948,41.5048035123033,50.3159340727209));
#29035=CARTESIAN_POINT('Ctrl Pts',(42.8003332568198,41.5005817926213,50.3306643988401));
#29036=CARTESIAN_POINT('Ctrl Pts',(42.7218700352141,41.4963600729392,50.341450431107));
#29037=CARTESIAN_POINT('Ctrl Pts',(42.6434324864251,41.4921397345851,50.3522329342322));
#29038=CARTESIAN_POINT('Ctrl Pts',(42.5644238401186,41.4879193962309,50.3590736422496));
#29039=CARTESIAN_POINT('Ctrl Pts',(42.4852718216873,41.4836990578767,50.3619312346735));
#29040=CARTESIAN_POINT('Ctrl Pts',(42.4061209839307,41.4794787824755,50.3647887844719));
#29041=CARTESIAN_POINT('Ctrl Pts',(42.3268272473944,41.4752585070742,50.3636633211789));
#29042=CARTESIAN_POINT('Ctrl Pts',(42.2478201587803,41.4710382316729,50.3585656100322));
#29043=CARTESIAN_POINT('Ctrl Pts',(42.1687340446719,41.466813735013,50.3534627999867));
#29044=CARTESIAN_POINT('Ctrl Pts',(42.0899356207309,41.4625892383532,50.344379835466));
#29045=CARTESIAN_POINT('Ctrl Pts',(42.0118505204597,41.4583647416933,50.3313795105972));
#29046=CARTESIAN_POINT('Ctrl Pts',(41.933727931736,41.4541382168637,50.3183729443065));
#29047=CARTESIAN_POINT('Ctrl Pts',(41.8563198080603,41.449911692034,50.3014453714602));
#29048=CARTESIAN_POINT('Ctrl Pts',(41.7800402388424,41.4456851672044,50.2807104891777));
#29049=CARTESIAN_POINT('Ctrl Pts',(41.7036212331292,41.441450916429,50.2599377042256));
#29050=CARTESIAN_POINT('Ctrl Pts',(41.6283353514743,41.4372166656537,50.2353438489837));
#29051=CARTESIAN_POINT('Ctrl Pts',(41.5545800121627,41.4329824148784,50.2070920880347));
#29052=CARTESIAN_POINT('Ctrl Pts',(41.4842368402638,41.4289440546331,50.180147347553));
#29053=CARTESIAN_POINT('Ctrl Pts',(41.4152860387921,41.4249056943878,50.1498758476075));
#29054=CARTESIAN_POINT('Ctrl Pts',(41.3480510583184,41.4208673341425,50.1164578580721));
#29055=CARTESIAN_POINT('Ctrl Pts',(41.2775338779776,41.4166318338763,50.0814085075986));
#29056=CARTESIAN_POINT('Ctrl Pts',(41.2086362670648,41.41239633361,50.0427643901465));
#29057=CARTESIAN_POINT('Ctrl Pts',(41.1417488973762,41.4081608333438,50.0006985289258));
#29058=CARTESIAN_POINT('Ctrl Pts',(41.074958493143,41.4039314732085,49.9586936498518));
#29059=CARTESIAN_POINT('Ctrl Pts',(41.0101729369737,41.3997021130732,49.9132771253288));
#29060=CARTESIAN_POINT('Ctrl Pts',(40.9477598481979,41.395472752938,49.8646685985434));
#29061=CARTESIAN_POINT('Ctrl Pts',(40.8854196449697,41.3912483318185,49.8161168364393));
#29062=CARTESIAN_POINT('Ctrl Pts',(40.8254467719094,41.387023910699,49.7643807663975));
#29063=CARTESIAN_POINT('Ctrl Pts',(40.768180002144,41.3827994895795,49.7097233505738));
#29064=CARTESIAN_POINT('Ctrl Pts',(40.7109498533955,41.3785777698975,49.6551008871344));
#29065=CARTESIAN_POINT('Ctrl Pts',(40.656422711875,41.3743560502155,49.5975611089631));
#29066=CARTESIAN_POINT('Ctrl Pts',(40.604903420906,41.3701343305334,49.5374064890669));
#29067=CARTESIAN_POINT('Ctrl Pts',(40.5534009868196,41.3659139921793,49.4772715514945));
#29068=CARTESIAN_POINT('Ctrl Pts',(40.5049047541546,41.3616936538251,49.4145238272755));
#29069=CARTESIAN_POINT('Ctrl Pts',(40.4596808703964,41.357473315471,49.349500691439));
#29070=CARTESIAN_POINT('Ctrl Pts',(40.4144576612224,41.3532530400697,49.284478525523));
#29071=CARTESIAN_POINT('Ctrl Pts',(40.3725069708237,41.3490327646684,49.2171814015387));
#29072=CARTESIAN_POINT('Ctrl Pts',(40.3340521264432,41.3448124892671,49.14797640422));
#29073=CARTESIAN_POINT('Ctrl Pts',(40.2955588182598,41.3405879926073,49.078702185782));
#29074=CARTESIAN_POINT('Ctrl Pts',(40.260568569631,41.3363634959474,49.0075166931521));
#29075=CARTESIAN_POINT('Ctrl Pts',(40.2292588330358,41.3321389992876,48.9348118671405));
#29076=CARTESIAN_POINT('Ctrl Pts',(40.1979340647179,41.3279124744579,48.862072135732));
#29077=CARTESIAN_POINT('Ctrl Pts',(40.1702934924723,41.3236859496283,48.7878120583056));
#29078=CARTESIAN_POINT('Ctrl Pts',(40.146465512677,41.3194594247987,48.7124414048508));
#29079=CARTESIAN_POINT('Ctrl Pts',(40.1225939761335,41.3152251740233,48.6369329763684));
#29080=CARTESIAN_POINT('Ctrl Pts',(40.1025490774193,41.310990923248,48.5603103705151));
#29081=CARTESIAN_POINT('Ctrl Pts',(40.086408590451,41.3067566724726,48.4829960978735));
#29082=CARTESIAN_POINT('Ctrl Pts',(40.0710148161161,41.3027183122273,48.4092586407416));
#29083=CARTESIAN_POINT('Ctrl Pts',(40.0591722004117,41.298679951982,48.3348924576612));
#29084=CARTESIAN_POINT('Ctrl Pts',(40.0509041153203,41.2946415917366,48.260267104108));
#29085=CARTESIAN_POINT('Ctrl Pts',(40.0413907678166,41.2899950110672,48.1744023708484));
#29086=CARTESIAN_POINT('Ctrl Pts',(40.0365840304864,41.2853484303977,48.0880066583314));
#29087=CARTESIAN_POINT('Ctrl Pts',(40.0365304529157,41.2807018497283,48.0014631831762));
#29088=CARTESIAN_POINT('',(40.0365303286314,40.4869518497552,48.0012463629995));
#29089=CARTESIAN_POINT('Ctrl Pts',(40.0365304529153,41.2807018496994,48.001463182638));
#29090=CARTESIAN_POINT('Ctrl Pts',(40.0364822936043,41.2765251727226,47.9236717558034));
#29091=CARTESIAN_POINT('Ctrl Pts',(40.0402790029724,41.2723484957457,47.8457269396662));
#29092=CARTESIAN_POINT('Ctrl Pts',(40.0479396135873,41.2681718187689,47.7680466004383));
#29093=CARTESIAN_POINT('Ctrl Pts',(40.0555893910889,41.2640010481639,47.6904761114504));
#29094=CARTESIAN_POINT('Ctrl Pts',(40.0670921711881,41.2598302775589,47.6131698334982));
#29095=CARTESIAN_POINT('Ctrl Pts',(40.0824149681851,41.2556595069539,47.5365455133376));
#29096=CARTESIAN_POINT('Ctrl Pts',(40.0977257549111,41.2514920054705,47.4599812526333));
#29097=CARTESIAN_POINT('Ctrl Pts',(40.1168505270377,41.247324503987,47.3840983613117));
#29098=CARTESIAN_POINT('Ctrl Pts',(40.1397046532171,41.2431570025036,47.3093080381158));
#29099=CARTESIAN_POINT('Ctrl Pts',(40.1625484484906,41.2389913848841,47.2345515228978));
#29100=CARTESIAN_POINT('Ctrl Pts',(40.189118112592,41.2348257672647,47.1608870572169));
#29101=CARTESIAN_POINT('Ctrl Pts',(40.2192786277662,41.2306601496452,47.0887125933151));
#29102=CARTESIAN_POINT('Ctrl Pts',(40.2494355147339,41.2264950331353,47.0165468117537));
#29103=CARTESIAN_POINT('Ctrl Pts',(40.2831822079519,41.2223299166253,46.9458711212109));
#29104=CARTESIAN_POINT('Ctrl Pts',(40.3203354515176,41.2181648001154,46.877063756625));
#29105=CARTESIAN_POINT('Ctrl Pts',(40.3575222543888,41.2139959213924,46.8081942406048));
#29106=CARTESIAN_POINT('Ctrl Pts',(40.3981215253446,41.2098270426694,46.7411968482197));
#29107=CARTESIAN_POINT('Ctrl Pts',(40.4419042788426,41.2056581639465,46.6764246951212));
#29108=CARTESIAN_POINT('Ctrl Pts',(40.4857054624514,41.2014875303568,46.6116252765389));
#29109=CARTESIAN_POINT('Ctrl Pts',(40.5326925062317,41.197316896767,46.549053348847));
#29110=CARTESIAN_POINT('Ctrl Pts',(40.582594966076,41.1931462631773,46.489030316794));
#29111=CARTESIAN_POINT('Ctrl Pts',(40.6325876920064,41.1889680855353,46.4288987120534));
#29112=CARTESIAN_POINT('Ctrl Pts',(40.6855060416132,41.1847899078932,46.3713255699776));
#29113=CARTESIAN_POINT('Ctrl Pts',(40.7410416825391,41.1806117302511,46.3165963817827));
#29114=CARTESIAN_POINT('Ctrl Pts',(40.7950768881226,41.176546436611,46.2633458405765));
#29115=CARTESIAN_POINT('Ctrl Pts',(40.8515893741545,41.1724811429709,46.2127877225138));
#29116=CARTESIAN_POINT('Ctrl Pts',(40.9102671796561,41.1684158493309,46.1651467184294));
#29117=CARTESIAN_POINT('Ctrl Pts',(40.9714017206828,41.1641803490646,46.1155110700979));
#29118=CARTESIAN_POINT('Ctrl Pts',(41.0351358559068,41.1599448487984,46.0688397875959));
#29119=CARTESIAN_POINT('Ctrl Pts',(41.1011501434374,41.1557093485321,46.0254166284993));
#29120=CARTESIAN_POINT('Ctrl Pts',(41.1670687312047,41.1514799883969,45.9820564192004));
#29121=CARTESIAN_POINT('Ctrl Pts',(41.2352605183376,41.1472506282616,45.9419352383165));
#29122=CARTESIAN_POINT('Ctrl Pts',(41.3053731986432,41.1430212681263,45.9052965349121));
#29123=CARTESIAN_POINT('Ctrl Pts',(41.3754040018746,41.1387968470069,45.868700617917));
#29124=CARTESIAN_POINT('Ctrl Pts',(41.4473508267955,41.1345724258874,45.8355793131379));
#29125=CARTESIAN_POINT('Ctrl Pts',(41.5208339091645,41.1303480047679,45.8061318577396));
#29126=CARTESIAN_POINT('Ctrl Pts',(41.5942700004913,41.1261262850858,45.7767032334325));
#29127=CARTESIAN_POINT('Ctrl Pts',(41.6692399649032,41.1219045654038,45.7509439696526));
#29128=CARTESIAN_POINT('Ctrl Pts',(41.745342153362,41.1176828457218,45.7290060447603));
#29129=CARTESIAN_POINT('Ctrl Pts',(41.8214194415237,41.1134625073676,45.7070752978593));
#29130=CARTESIAN_POINT('Ctrl Pts',(41.8986277674785,41.1092421690135,45.6889635370223));
#29131=CARTESIAN_POINT('Ctrl Pts',(41.976549767592,41.1050218306593,45.6747730558989));
#29132=CARTESIAN_POINT('Ctrl Pts',(42.0544706053783,41.100801555258,45.6605827864486));
#29133=CARTESIAN_POINT('Ctrl Pts',(42.1331046341663,41.0965812798567,45.6503137632214));
#29134=CARTESIAN_POINT('Ctrl Pts',(42.2120252108304,41.0923610044555,45.6440169950663));
#29135=CARTESIAN_POINT('Ctrl Pts',(42.2910247264567,41.0881365077956,45.637713928676));
#29136=CARTESIAN_POINT('Ctrl Pts',(42.3703108935256,41.0839120111358,45.6353910917051));
#29137=CARTESIAN_POINT('Ctrl Pts',(42.4494534726929,41.0796875144759,45.6370474412425));
#29138=CARTESIAN_POINT('Ctrl Pts',(42.5286340480055,41.0754609896463,45.638704585989));
#29139=CARTESIAN_POINT('Ctrl Pts',(42.6076704292831,41.0712344648166,45.6443446895344));
#29140=CARTESIAN_POINT('Ctrl Pts',(42.6861364944463,41.067007939987,45.653914676009));
#29141=CARTESIAN_POINT('Ctrl Pts',(42.7647459929461,41.0627736892116,45.663502156098));
#29142=CARTESIAN_POINT('Ctrl Pts',(42.8427826284677,41.0585394384363,45.6770337934225));
#29143=CARTESIAN_POINT('Ctrl Pts',(42.9198296762005,41.054305187661,45.6944051638154));
#29144=CARTESIAN_POINT('Ctrl Pts',(42.9933122711371,41.0502668274156,45.7109728768119));
#29145=CARTESIAN_POINT('Ctrl Pts',(43.0658944821732,41.0462284671703,45.7310327714717));
#29146=CARTESIAN_POINT('Ctrl Pts',(43.1372303305945,41.042190106925,45.7544528772365));
#29147=CARTESIAN_POINT('Ctrl Pts',(43.212048570332,41.0379546066587,45.7790162787599));
#29148=CARTESIAN_POINT('Ctrl Pts',(43.285780053544,41.0337191063925,45.8073697086495));
#29149=CARTESIAN_POINT('Ctrl Pts',(43.3580133168007,41.0294836061262,45.8393980177431));
#29150=CARTESIAN_POINT('Ctrl Pts',(43.4301418647534,41.0252542459909,45.8713798959546));
#29151=CARTESIAN_POINT('Ctrl Pts',(43.5007760804111,41.0210248858557,45.9070258854392));
#29152=CARTESIAN_POINT('Ctrl Pts',(43.569520621626,41.0167955257204,45.9461713906726));
#29153=CARTESIAN_POINT('Ctrl Pts',(43.6381848834693,41.0125711046009,45.9852711820719));
#29154=CARTESIAN_POINT('Ctrl Pts',(43.7049634503462,41.0083466834814,46.0278621371252));
#29155=CARTESIAN_POINT('Ctrl Pts',(43.7694833089865,41.0041222623619,46.0737326490574));
#29156=CARTESIAN_POINT('Ctrl Pts',(43.8339619083968,40.9999005426799,46.1195738276643));
#29157=CARTESIAN_POINT('Ctrl Pts',(43.8961842849022,40.9956788229979,46.1686901294023));
#29158=CARTESIAN_POINT('Ctrl Pts',(43.955805331725,40.9914571033158,46.220825975157));
#29159=CARTESIAN_POINT('Ctrl Pts',(44.0154068708067,40.9872367649617,46.2729447622951));
#29160=CARTESIAN_POINT('Ctrl Pts',(44.0724084172434,40.9830164266075,46.3280808229195));
#29161=CARTESIAN_POINT('Ctrl Pts',(44.1264981490303,40.9787960882534,46.3859384824937));
#29162=CARTESIAN_POINT('Ctrl Pts',(44.1805870739854,40.9745758128521,46.4437952790316));
#29163=CARTESIAN_POINT('Ctrl Pts',(44.2317639510734,40.9703555374508,46.5043732500526));
#29164=CARTESIAN_POINT('Ctrl Pts',(44.2797550701209,40.9661352620495,46.5673411720669));
#29165=CARTESIAN_POINT('Ctrl Pts',(44.3277941914675,40.9619107653896,46.6303720766722));
#29166=CARTESIAN_POINT('Ctrl Pts',(44.3726409041523,40.9576862687298,46.695797333427));
#29167=CARTESIAN_POINT('Ctrl Pts',(44.4140633294692,40.95346177207,46.7632545347617));
#29168=CARTESIAN_POINT('Ctrl Pts',(44.4555056415842,40.9492352472403,46.8307441221224));
#29169=CARTESIAN_POINT('Ctrl Pts',(44.4935201658159,40.9450087224107,46.9002671850647));
#29170=CARTESIAN_POINT('Ctrl Pts',(44.5279210120423,40.940782197581,46.9714366293666));
#29171=CARTESIAN_POINT('Ctrl Pts',(44.5623847418624,40.9365479468057,47.0427361690267));
#29172=CARTESIAN_POINT('Ctrl Pts',(44.5932214107531,40.9323136960303,47.1156876703405));
#29173=CARTESIAN_POINT('Ctrl Pts',(44.6202933977941,40.928079445255,47.1898841634607));
#29174=CARTESIAN_POINT('Ctrl Pts',(44.6461129446345,40.9240410850097,47.2606480799255));
#29175=CARTESIAN_POINT('Ctrl Pts',(44.6685083686557,40.9200027247644,47.3325439888181));
#29176=CARTESIAN_POINT('Ctrl Pts',(44.6874034892614,40.9159643645191,47.4052095173804));
#29177=CARTESIAN_POINT('Ctrl Pts',(44.7072210101102,40.9117288642529,47.4814223480537));
#29178=CARTESIAN_POINT('Ctrl Pts',(44.7232630846991,40.9074933639866,47.5587715590777));
#29179=CARTESIAN_POINT('Ctrl Pts',(44.7354039584918,40.9032578637204,47.6368488034428));
#29180=CARTESIAN_POINT('Ctrl Pts',(44.7475272318712,40.8990285035851,47.7148128605861));
#29181=CARTESIAN_POINT('Ctrl Pts',(44.7557604637776,40.8947991434498,47.7935023953432));
#29182=CARTESIAN_POINT('Ctrl Pts',(44.7600282069293,40.8905697833146,47.8724958690938));
#29183=CARTESIAN_POINT('Ctrl Pts',(44.7642909662418,40.8863453621951,47.9513970948447));
#29184=CARTESIAN_POINT('Ctrl Pts',(44.7645974140084,40.8821209410756,48.0306010880284));
#29185=CARTESIAN_POINT('Ctrl Pts',(44.7609237204617,40.8778965199561,48.1096796565512));
#29186=CARTESIAN_POINT('Ctrl Pts',(44.7572523761726,40.8736748002741,48.188707655824));
#29187=CARTESIAN_POINT('Ctrl Pts',(44.7496059640198,40.8694530805921,48.2676099220498));
#29188=CARTESIAN_POINT('Ctrl Pts',(44.738012733382,40.86523136091,48.3459579446169));
#29189=CARTESIAN_POINT('Ctrl Pts',(44.7264232959977,40.8610110225559,48.42428033206));
#29190=CARTESIAN_POINT('Ctrl Pts',(44.7108896730341,40.8567906842017,48.5020483719928));
#29191=CARTESIAN_POINT('Ctrl Pts',(44.6914918420243,40.8525703458476,48.5788398559498));
#29192=CARTESIAN_POINT('Ctrl Pts',(44.6720943003632,40.8483500704463,48.655630194443));
#29193=CARTESIAN_POINT('Ctrl Pts',(44.6488327814757,40.844129795045,48.7314435511853));
#29194=CARTESIAN_POINT('Ctrl Pts',(44.6218377787388,40.8399095196437,48.8058705391496));
#29195=CARTESIAN_POINT('Ctrl Pts',(44.5948157747103,40.8356850229839,48.8803719714405));
#29196=CARTESIAN_POINT('Ctrl Pts',(44.5640529874069,40.831460526324,48.9534838225824));
#29197=CARTESIAN_POINT('Ctrl Pts',(44.5297287673595,40.8272360296642,49.0248150166647));
#29198=CARTESIAN_POINT('Ctrl Pts',(44.4953880683438,40.8230095048345,49.0961804566666));
#29199=CARTESIAN_POINT('Ctrl Pts',(44.4574827552199,40.8187829800049,49.1657631238361));
#29200=CARTESIAN_POINT('Ctrl Pts',(44.4162378201187,40.8145564551753,49.2331972646835));
#29201=CARTESIAN_POINT('Ctrl Pts',(44.3749174906589,40.8103222043999,49.3007546728797));
#29202=CARTESIAN_POINT('Ctrl Pts',(44.33024560599,40.8060879536246,49.3661553182307));
#29203=CARTESIAN_POINT('Ctrl Pts',(44.282489987429,40.8018537028492,49.4290632904563));
#29204=CARTESIAN_POINT('Ctrl Pts',(44.2369437026859,40.7978153426039,49.4890609305651));
#29205=CARTESIAN_POINT('Ctrl Pts',(44.1885929592367,40.7937769823586,49.5467911855493));
#29206=CARTESIAN_POINT('Ctrl Pts',(44.1377013096872,40.7897386221133,49.6019939448111));
#29207=CARTESIAN_POINT('Ctrl Pts',(44.0843252901836,40.785503121847,49.6598915288174));
#29208=CARTESIAN_POINT('Ctrl Pts',(44.0279510586162,40.7812676215808,49.715228628654));
#29209=CARTESIAN_POINT('Ctrl Pts',(43.9688540141472,40.7770321213145,49.7676785689696));
#29210=CARTESIAN_POINT('Ctrl Pts',(43.9098426416343,40.7728027611793,49.8200524735201));
#29211=CARTESIAN_POINT('Ctrl Pts',(43.848116642757,40.768573401044,49.8695472212268));
#29212=CARTESIAN_POINT('Ctrl Pts',(43.7839897269887,40.7643440409087,49.9158713100023));
#29213=CARTESIAN_POINT('Ctrl Pts',(43.7199376981628,40.7601196197892,49.9621413018462));
#29214=CARTESIAN_POINT('Ctrl Pts',(43.6534907025532,40.7558951986697,50.0052477192448));
#29215=CARTESIAN_POINT('Ctrl Pts',(43.5849959700272,40.7516707775502,50.0449388724163));
#29216=CARTESIAN_POINT('Ctrl Pts',(43.516545038588,40.7474490578682,50.0846046438456));
#29217=CARTESIAN_POINT('Ctrl Pts',(43.4460493742868,40.7432273381862,50.120859251127));
#29218=CARTESIAN_POINT('Ctrl Pts',(43.3738846492484,40.7390056185041,50.153494632187));
#29219=CARTESIAN_POINT('Ctrl Pts',(43.3017435361867,40.73478528015,50.1861193350957));
#29220=CARTESIAN_POINT('Ctrl Pts',(43.2279348741094,40.7305649417958,50.2151269699477));
#29221=CARTESIAN_POINT('Ctrl Pts',(43.1528570193506,40.7263446034417,50.2403563889066));
#29222=CARTESIAN_POINT('Ctrl Pts',(43.0777802844939,40.7221243280404,50.2655854315298));
#29223=CARTESIAN_POINT('Ctrl Pts',(43.001434839916,40.7179040526391,50.2870362220449));
#29224=CARTESIAN_POINT('Ctrl Pts',(42.9242355874031,40.7136837772378,50.3045970341472));
#29225=CARTESIAN_POINT('Ctrl Pts',(42.8469591176534,40.7094592805779,50.3221754111526));
#29226=CARTESIAN_POINT('Ctrl Pts',(42.7688275927359,40.7052347839181,50.335855932858));
#29227=CARTESIAN_POINT('Ctrl Pts',(42.6902669455783,40.7010102872582,50.3455778693543));
#29228=CARTESIAN_POINT('Ctrl Pts',(42.6116685816595,40.6967837624286,50.3553044733269));
#29229=CARTESIAN_POINT('Ctrl Pts',(42.5326411538339,40.6925572375989,50.3610686718588));
#29230=CARTESIAN_POINT('Ctrl Pts',(42.4536139898798,40.6883307127693,50.3628618201218));
#29231=CARTESIAN_POINT('Ctrl Pts',(42.3744423669193,40.684096461994,50.3646582461997));
#29232=CARTESIAN_POINT('Ctrl Pts',(42.2952714792004,40.6798622112186,50.3624691299369));
#29233=CARTESIAN_POINT('Ctrl Pts',(42.2165287257499,40.6756279604433,50.3563379919751));
#29234=CARTESIAN_POINT('Ctrl Pts',(42.1414288740851,40.671589600198,50.3504905008563));
#29235=CARTESIAN_POINT('Ctrl Pts',(42.0667187686555,40.6675512399527,50.3410577451993));
#29236=CARTESIAN_POINT('Ctrl Pts',(41.9927597494912,40.6635128797074,50.3281206625228));
#29237=CARTESIAN_POINT('Ctrl Pts',(41.9151902840809,40.6592773794411,50.3145520322391));
#29238=CARTESIAN_POINT('Ctrl Pts',(41.8381522505117,40.6550418791749,50.2970766213165));
#29239=CARTESIAN_POINT('Ctrl Pts',(41.7620693805254,40.6508063789087,50.2757493195949));
#29240=CARTESIAN_POINT('Ctrl Pts',(41.6860968065511,40.6465770187734,50.2544529356913));
#29241=CARTESIAN_POINT('Ctrl Pts',(41.6110770945306,40.6423476586382,50.2293158754767));
#29242=CARTESIAN_POINT('Ctrl Pts',(41.5374251200559,40.6381182985029,50.2004442772744));
#29243=CARTESIAN_POINT('Ctrl Pts',(41.4638591558172,40.6338938773834,50.1716063951128));
#29244=CARTESIAN_POINT('Ctrl Pts',(41.3916581898303,40.6296694562639,50.1390428118174));
#29245=CARTESIAN_POINT('Ctrl Pts',(41.3212217486689,40.6254450351445,50.1029093954222));
#29246=CARTESIAN_POINT('Ctrl Pts',(41.2508303502802,40.6212233154624,50.0667990856638));
#29247=CARTESIAN_POINT('Ctrl Pts',(41.1822016536031,40.6170015957804,50.0271236874078));
#29248=CARTESIAN_POINT('Ctrl Pts',(41.1157138801031,40.6127798760984,49.9840865916437));
#29249=CARTESIAN_POINT('Ctrl Pts',(41.0492478611065,40.6085595377442,49.9410635774256));
#29250=CARTESIAN_POINT('Ctrl Pts',(40.9849217680386,40.6043391993901,49.8946813046486));
#29251=CARTESIAN_POINT('Ctrl Pts',(40.923086638139,40.6001188610359,49.8451876225621));
#29252=CARTESIAN_POINT('Ctrl Pts',(40.8612524306058,40.5958985856347,49.7956946787502));
#29253=CARTESIAN_POINT('Ctrl Pts',(40.8019094779762,40.5916783102334,49.74309071222));
#29254=CARTESIAN_POINT('Ctrl Pts',(40.7453762035434,40.5874580348321,49.6876642240385));
#29255=CARTESIAN_POINT('Ctrl Pts',(40.6887863826662,40.5832335381722,49.6321822964567));
#29256=CARTESIAN_POINT('Ctrl Pts',(40.6350121899266,40.5790090415124,49.5738725369367));
#29257=CARTESIAN_POINT('Ctrl Pts',(40.5843351269717,40.5747845448525,49.5130603126614));
#29258=CARTESIAN_POINT('Ctrl Pts',(40.5336337340914,40.5705580200229,49.4522188925963));
#29259=CARTESIAN_POINT('Ctrl Pts',(40.4860327154755,40.5663314951933,49.388872990123));
#29260=CARTESIAN_POINT('Ctrl Pts',(40.4417716043412,40.5621049703636,49.3233790051742));
#29261=CARTESIAN_POINT('Ctrl Pts',(40.3974295853797,40.5578707195883,49.2577652994165));
#29262=CARTESIAN_POINT('Ctrl Pts',(40.3564399171461,40.553636468813,49.1899960675313));
#29263=CARTESIAN_POINT('Ctrl Pts',(40.3189972167955,40.5494022180376,49.1204543083924));
#29264=CARTESIAN_POINT('Ctrl Pts',(40.2832867403507,40.5453638577923,49.0541297824259));
#29265=CARTESIAN_POINT('Ctrl Pts',(40.2508024214045,40.5413254975469,48.9861934463802));
#29266=CARTESIAN_POINT('Ctrl Pts',(40.221671671113,40.5372871373016,48.9169929838709));
#29267=CARTESIAN_POINT('Ctrl Pts',(40.1876925816392,40.5325766577317,48.8362752308537));
#29268=CARTESIAN_POINT('Ctrl Pts',(40.1581660688896,40.5278661781618,48.7535772427311));
#29269=CARTESIAN_POINT('Ctrl Pts',(40.1333014726962,40.5231556985919,48.6693789862394));
#29270=CARTESIAN_POINT('Ctrl Pts',(40.1085164075483,40.5184602858006,48.585450043406));
#29271=CARTESIAN_POINT('Ctrl Pts',(40.0883636356809,40.5137648730092,48.5000306604509));
#29272=CARTESIAN_POINT('Ctrl Pts',(40.073004121357,40.5090694602179,48.4136189329304));
#29273=CARTESIAN_POINT('Ctrl Pts',(40.0577283968686,40.5043996620298,48.3276786021146));
#29274=CARTESIAN_POINT('Ctrl Pts',(40.0471938971035,40.4997298638417,48.2407569881186));
#29275=CARTESIAN_POINT('Ctrl Pts',(40.0415110131285,40.4950600656537,48.1533627715776));
#29276=CARTESIAN_POINT('Ctrl Pts',(40.0382219309356,40.4923573270208,48.1027816295633));
#29277=CARTESIAN_POINT('Ctrl Pts',(40.0365571157034,40.489654588388,48.052042505279));
#29278=CARTESIAN_POINT('Ctrl Pts',(40.0365303286314,40.4869518497552,48.0012463629995));
#29279=CARTESIAN_POINT('',(40.0365308224644,39.6932018496801,47.9980282648923));
#29280=CARTESIAN_POINT('Ctrl Pts',(40.0365303286311,40.4869518497283,48.0012463624935));
#29281=CARTESIAN_POINT('Ctrl Pts',(40.0364879504104,40.4826760072291,47.9208847983668));
#29282=CARTESIAN_POINT('Ctrl Pts',(40.0405485387724,40.4784001647298,47.8405250305544));
#29283=CARTESIAN_POINT('Ctrl Pts',(40.0486851230954,40.4741243222306,47.760607455114));
#29284=CARTESIAN_POINT('Ctrl Pts',(40.0568243739978,40.4698470784217,47.6806636885162));
#29285=CARTESIAN_POINT('Ctrl Pts',(40.0690422298306,40.4655698346129,47.6011628519446));
#29286=CARTESIAN_POINT('Ctrl Pts',(40.0852600030886,40.4612925908041,47.5225388103745));
#29287=CARTESIAN_POINT('Ctrl Pts',(40.1015009109304,40.4570092455254,47.4438026119476));
#29288=CARTESIAN_POINT('Ctrl Pts',(40.1217530396299,40.4527259002467,47.365946150112));
#29289=CARTESIAN_POINT('Ctrl Pts',(40.1458868702053,40.448442554968,47.2893915009043));
#29290=CARTESIAN_POINT('Ctrl Pts',(40.1700380349793,40.4441561331632,47.2127818660826));
#29291=CARTESIAN_POINT('Ctrl Pts',(40.1980762971258,40.4398697113585,47.1374763301334));
#29292=CARTESIAN_POINT('Ctrl Pts',(40.2298235847538,40.4355832895538,47.0638778030572));
#29293=CARTESIAN_POINT('Ctrl Pts',(40.2616371863975,40.4312879142332,46.9901255427255));
#29294=CARTESIAN_POINT('Ctrl Pts',(40.297175095069,40.4269925389126,46.9180878228388));
#29295=CARTESIAN_POINT('Ctrl Pts',(40.3362127465961,40.422697163592,46.8481438398883));
#29296=CARTESIAN_POINT('Ctrl Pts',(40.371462524921,40.4188185740266,46.7849866109636));
#29297=CARTESIAN_POINT('Ctrl Pts',(40.4095651002173,40.4149399844611,46.7235363621325));
#29298=CARTESIAN_POINT('Ctrl Pts',(40.4503260771266,40.4110613948956,46.6640501374051));
#29299=CARTESIAN_POINT('Ctrl Pts',(40.4948379094919,40.4068258946294,46.5990899459699));
#29300=CARTESIAN_POINT('Ctrl Pts',(40.5426844648708,40.4025903943631,46.5362333175087));
#29301=CARTESIAN_POINT('Ctrl Pts',(40.5936400916276,40.3983548940969,46.4758430781823));
#29302=CARTESIAN_POINT('Ctrl Pts',(40.6445218488996,40.3941255339616,46.4155403855344));
#29303=CARTESIAN_POINT('Ctrl Pts',(40.6985034269968,40.3898961738264,46.3576973374298));
#29304=CARTESIAN_POINT('Ctrl Pts',(40.755316211548,40.3856668136911,46.3026474506151));
#29305=CARTESIAN_POINT('Ctrl Pts',(40.8120626505459,40.3814423925716,46.2476618506548));
#29306=CARTESIAN_POINT('Ctrl Pts',(40.8716333905205,40.3772179714521,46.1954632550286));
#29307=CARTESIAN_POINT('Ctrl Pts',(40.9337209287244,40.3729935503327,46.1463505924692));
#29308=CARTESIAN_POINT('Ctrl Pts',(40.9957687631211,40.3687718306506,46.0972693365293));
#29309=CARTESIAN_POINT('Ctrl Pts',(41.0603298342292,40.3645501109686,46.051270387283));
#29310=CARTESIAN_POINT('Ctrl Pts',(41.127062228754,40.3603283912866,46.0086135805838));
#29311=CARTESIAN_POINT('Ctrl Pts',(41.1937727887366,40.3561080529324,45.9659707310018));
#29312=CARTESIAN_POINT('Ctrl Pts',(41.2626528662615,40.3518877145782,45.9266681051667));
#29313=CARTESIAN_POINT('Ctrl Pts',(41.3333313641073,40.3476673762241,45.8909223669806));
#29314=CARTESIAN_POINT('Ctrl Pts',(41.404008807674,40.3434471008228,45.8551771619974));
#29315=CARTESIAN_POINT('Ctrl Pts',(41.4764841988021,40.3392268254215,45.8229889498333));
#29316=CARTESIAN_POINT('Ctrl Pts',(41.5503629715907,40.3350065500202,45.7945278598777));
#29317=CARTESIAN_POINT('Ctrl Pts',(41.624315640363,40.3307820533604,45.7660383022018));
#29318=CARTESIAN_POINT('Ctrl Pts',(41.699674055859,40.3265575567006,45.7412834829944));
#29319=CARTESIAN_POINT('Ctrl Pts',(41.7760254146192,40.3223330600407,45.7203846469856));
#29320=CARTESIAN_POINT('Ctrl Pts',(41.852413429467,40.3181065352111,45.6994757775004));
#29321=CARTESIAN_POINT('Ctrl Pts',(41.9297948782545,40.3138800103814,45.682426680252));
#29322=CARTESIAN_POINT('Ctrl Pts',(42.0077461208794,40.3096534855518,45.6693075416918));
#29323=CARTESIAN_POINT('Ctrl Pts',(42.0858398557624,40.3054192347765,45.6561644217861));
#29324=CARTESIAN_POINT('Ctrl Pts',(42.1645049983709,40.3011849840011,45.6469656702076));
#29325=CARTESIAN_POINT('Ctrl Pts',(42.2433123288832,40.2969507332258,45.6417295713553));
#29326=CARTESIAN_POINT('Ctrl Pts',(42.3184737700608,40.2929123729805,45.6367357118586));
#29327=CARTESIAN_POINT('Ctrl Pts',(42.3937641761254,40.2888740127351,45.6353459322716));
#29328=CARTESIAN_POINT('Ctrl Pts',(42.4688143307643,40.2848356524898,45.6375320047075));
#29329=CARTESIAN_POINT('Ctrl Pts',(42.547528197444,40.2806001522236,45.6398247943107));
#29330=CARTESIAN_POINT('Ctrl Pts',(42.6262769653922,40.2763646519573,45.6460601892281));
#29331=CARTESIAN_POINT('Ctrl Pts',(42.7046334120102,40.2721291516911,45.6562446959661));
#29332=CARTESIAN_POINT('Ctrl Pts',(42.7828762666518,40.2678997915558,45.6664144384021));
#29333=CARTESIAN_POINT('Ctrl Pts',(42.8607274678836,40.2636704314206,45.6805218639176));
#29334=CARTESIAN_POINT('Ctrl Pts',(42.9377612006724,40.2594410712853,45.6985214900088));
#29335=CARTESIAN_POINT('Ctrl Pts',(43.0147049740326,40.2552166501658,45.7165000962686));
#29336=CARTESIAN_POINT('Ctrl Pts',(43.0908327213179,40.2509922290463,45.7383617645431));
#29337=CARTESIAN_POINT('Ctrl Pts',(43.1657266787048,40.2467678079268,45.7640095942917));
#29338=CARTESIAN_POINT('Ctrl Pts',(43.2405727428216,40.2425460882448,45.7896410227379));
#29339=CARTESIAN_POINT('Ctrl Pts',(43.3141861401709,40.2383243685628,45.8190536554844));
#29340=CARTESIAN_POINT('Ctrl Pts',(43.3861633693248,40.2341026488807,45.8521005028396));
#29341=CARTESIAN_POINT('Ctrl Pts',(43.45811704785,40.2298823105266,45.8851365374136));
#29342=CARTESIAN_POINT('Ctrl Pts',(43.5284351949817,40.2256619721724,45.9218042297505));
#29343=CARTESIAN_POINT('Ctrl Pts',(43.5967348298591,40.2214416338183,45.9619086899989));
#29344=CARTESIAN_POINT('Ctrl Pts',(43.6650334459419,40.217221358417,46.0020125520272));
#29345=CARTESIAN_POINT('Ctrl Pts',(43.7313132055605,40.2130010830157,46.0455528412591));
#29346=CARTESIAN_POINT('Ctrl Pts',(43.7952175683292,40.2087808076144,46.0922897552496));
#29347=CARTESIAN_POINT('Ctrl Pts',(43.8591858503478,40.2045563109546,46.1390734170419));
#29348=CARTESIAN_POINT('Ctrl Pts',(43.9207736095071,40.2003318142947,46.1890598130093));
#29349=CARTESIAN_POINT('Ctrl Pts',(43.9796555524277,40.1961073176349,46.2419673562234));
#29350=CARTESIAN_POINT('Ctrl Pts',(44.0385657644152,40.1918807928052,46.2949003002105));
#29351=CARTESIAN_POINT('Ctrl Pts',(44.0947672389277,40.1876542679756,46.3507568539537));
#29352=CARTESIAN_POINT('Ctrl Pts',(44.1479717615001,40.1834277431459,46.4092186945095));
#29353=CARTESIAN_POINT('Ctrl Pts',(44.2012735401561,40.1791934923706,46.4677874013498));
#29354=CARTESIAN_POINT('Ctrl Pts',(44.2515671210607,40.1749592415953,46.5289705478201));
#29355=CARTESIAN_POINT('Ctrl Pts',(44.2986049222509,40.1707249908199,46.5924170397079));
#29356=CARTESIAN_POINT('Ctrl Pts',(44.3434665982432,40.1666866305746,46.6529282857674));
#29357=CARTESIAN_POINT('Ctrl Pts',(44.385366910784,40.1626482703293,46.7154977714741));
#29358=CARTESIAN_POINT('Ctrl Pts',(44.4241298574355,40.158609910084,46.7797997045));
#29359=CARTESIAN_POINT('Ctrl Pts',(44.4647850889873,40.1543744098177,46.8472406552591));
#29360=CARTESIAN_POINT('Ctrl Pts',(44.5021433601042,40.1501389095515,46.916843874885));
#29361=CARTESIAN_POINT('Ctrl Pts',(44.5359680748416,40.1459034092852,46.9882535771461));
#29362=CARTESIAN_POINT('Ctrl Pts',(44.569743754479,40.14167404915,47.0595597580053));
#29363=CARTESIAN_POINT('Ctrl Pts',(44.5999958509682,40.1374446890147,47.1326668003879));
#29364=CARTESIAN_POINT('Ctrl Pts',(44.6265322540626,40.1332153288794,47.2071919762523));
#29365=CARTESIAN_POINT('Ctrl Pts',(44.65303766814,40.1289909077599,47.2816301221625));
#29366=CARTESIAN_POINT('Ctrl Pts',(44.6758358549175,40.1247664866405,47.3574826707428));
#29367=CARTESIAN_POINT('Ctrl Pts',(44.6947823037968,40.120542065521,47.4343458485249));
#29368=CARTESIAN_POINT('Ctrl Pts',(44.7137166367802,40.1163203458389,47.5111598737575));
#29369=CARTESIAN_POINT('Ctrl Pts',(44.7288040085917,40.1120986261569,47.5889827909877));
#29370=CARTESIAN_POINT('Ctrl Pts',(44.739949750849,40.1078769064749,47.6673957240175));
#29371=CARTESIAN_POINT('Ctrl Pts',(44.7510918462691,40.1036565681207,47.7457830006848));
#29372=CARTESIAN_POINT('Ctrl Pts',(44.7582948070186,40.0994362297666,47.8247594454883));
#29373=CARTESIAN_POINT('Ctrl Pts',(44.7615153515461,40.0952158914124,47.903897527024));
#29374=CARTESIAN_POINT('Ctrl Pts',(44.7647358480343,40.0909956160111,47.9830344280927));
#29375=CARTESIAN_POINT('Ctrl Pts',(44.7639740286308,40.0867753406098,48.0623324920834));
#29376=CARTESIAN_POINT('Ctrl Pts',(44.759238688608,40.0825550652085,48.141362127443));
#29377=CARTESIAN_POINT('Ctrl Pts',(44.754498612142,40.0783305685487,48.220470810849));
#29378=CARTESIAN_POINT('Ctrl Pts',(44.7457771037386,40.0741060718888,48.2993100596483));
#29379=CARTESIAN_POINT('Ctrl Pts',(44.733135004958,40.069881575229,48.3774539568475));
#29380=CARTESIAN_POINT('Ctrl Pts',(44.7204868367387,40.0656550503993,48.4556353707275));
#29381=CARTESIAN_POINT('Ctrl Pts',(44.7039144267388,40.0614285255697,48.5331203083622));
#29382=CARTESIAN_POINT('Ctrl Pts',(44.683529571915,40.05720200074,48.6094941632941));
#29383=CARTESIAN_POINT('Ctrl Pts',(44.6631074542601,40.0529677499647,48.6860076270723));
#29384=CARTESIAN_POINT('Ctrl Pts',(44.6388591101169,40.0487334991894,48.761405501701));
#29385=CARTESIAN_POINT('Ctrl Pts',(44.6109458798371,40.044499248414,48.8352896248197));
#29386=CARTESIAN_POINT('Ctrl Pts',(44.5843240084693,40.0404608881687,48.9057556225588));
#29387=CARTESIAN_POINT('Ctrl Pts',(44.554369027367,40.0364225279234,48.9748445206523));
#29388=CARTESIAN_POINT('Ctrl Pts',(44.5212597212008,40.0323841676781,49.0422320452333));
#29389=CARTESIAN_POINT('Ctrl Pts',(44.4865341230461,40.0281486674118,49.1129092164035));
#29390=CARTESIAN_POINT('Ctrl Pts',(44.4482063685516,40.0239131671456,49.1819833203683));
#29391=CARTESIAN_POINT('Ctrl Pts',(44.4064476875312,40.0196776668794,49.2490628959746));
#29392=CARTESIAN_POINT('Ctrl Pts',(44.3647495433436,40.0154483067441,49.3160452274883));
#29393=CARTESIAN_POINT('Ctrl Pts',(44.3196305955762,40.0112189466088,49.3810383774373));
#29394=CARTESIAN_POINT('Ctrl Pts',(44.2713087992454,40.0069895864736,49.4436737230991));
#29395=CARTESIAN_POINT('Ctrl Pts',(44.2230434327543,40.0027651653541,49.5062359236632));
#29396=CARTESIAN_POINT('Ctrl Pts',(44.1715829355024,39.9985407442346,49.5664454218263));
#29397=CARTESIAN_POINT('Ctrl Pts',(44.1171887133054,39.9943163231151,49.6239622421093));
#29398=CARTESIAN_POINT('Ctrl Pts',(44.0628292751853,39.9900946034331,49.6814422814729));
#29399=CARTESIAN_POINT('Ctrl Pts',(44.0055401573259,39.985872883751,49.7362327205046));
#29400=CARTESIAN_POINT('Ctrl Pts',(43.9456224315768,39.981651164069,49.7880273319797));
#29401=CARTESIAN_POINT('Ctrl Pts',(43.8857243106408,39.9774308257149,49.8398049964887));
#29402=CARTESIAN_POINT('Ctrl Pts',(43.8231996444346,39.9732104873607,49.8885884731295));
#29403=CARTESIAN_POINT('Ctrl Pts',(43.7583845839174,39.9689901490066,49.9341100700518));
#29404=CARTESIAN_POINT('Ctrl Pts',(43.6935704902169,39.9647698736053,49.9796309879491));
#29405=CARTESIAN_POINT('Ctrl Pts',(43.626466454971,39.960549598204,50.0218898541813));
#29406=CARTESIAN_POINT('Ctrl Pts',(43.5574385349003,39.9563293228027,50.060661660445));
#29407=CARTESIAN_POINT('Ctrl Pts',(43.4883415708289,39.9521048261428,50.0994722475472));
#29408=CARTESIAN_POINT('Ctrl Pts',(43.4173172880305,39.947880329483,50.1347885768163));
#29409=CARTESIAN_POINT('Ctrl Pts',(43.344756809417,39.9436558328232,50.1664314002433));
#29410=CARTESIAN_POINT('Ctrl Pts',(43.2721614947074,39.9394293079935,50.1980894153071));
#29411=CARTESIAN_POINT('Ctrl Pts',(43.1980289546627,39.9352027831639,50.2260702451727));
#29412=CARTESIAN_POINT('Ctrl Pts',(43.1227683661523,39.9309762583342,50.2502436156536));
#29413=CARTESIAN_POINT('Ctrl Pts',(43.0473702038093,39.9267420075589,50.2744611742452));
#29414=CARTESIAN_POINT('Ctrl Pts',(42.9708403272855,39.9225077567836,50.2948572447362));
#29415=CARTESIAN_POINT('Ctrl Pts',(42.8936008860584,39.9182735060082,50.3113521164423));
#29416=CARTESIAN_POINT('Ctrl Pts',(42.8199347983912,39.9142351457629,50.3270838804978));
#29417=CARTESIAN_POINT('Ctrl Pts',(42.7456237061773,39.9101967855176,50.3392674065297));
#29418=CARTESIAN_POINT('Ctrl Pts',(42.6710370538251,39.9061584252723,50.347877628062));
#29419=CARTESIAN_POINT('Ctrl Pts',(42.5928093161525,39.9019229250061,50.3569081734757));
#29420=CARTESIAN_POINT('Ctrl Pts',(42.5139810670693,39.8976874247398,50.362041958593));
#29421=CARTESIAN_POINT('Ctrl Pts',(42.4349741702642,39.8934519244736,50.3632112153412));
#29422=CARTESIAN_POINT('Ctrl Pts',(42.3560818083822,39.8892225643383,50.3643787770382));
#29423=CARTESIAN_POINT('Ctrl Pts',(42.2770117784023,39.8849932042031,50.3615932166178));
#29424=CARTESIAN_POINT('Ctrl Pts',(42.198192014189,39.8807638440678,50.3548384186103));
#29425=CARTESIAN_POINT('Ctrl Pts',(42.1194642951185,39.8765394229483,50.3480915088064));
#29426=CARTESIAN_POINT('Ctrl Pts',(42.0409867262507,39.8723150018288,50.3373846123811));
#29427=CARTESIAN_POINT('Ctrl Pts',(41.9631866548269,39.8680905807093,50.3227536551212));
#29428=CARTESIAN_POINT('Ctrl Pts',(41.8854363350783,39.8638688610273,50.3081320540819));
#29429=CARTESIAN_POINT('Ctrl Pts',(41.8083631128912,39.8596471413453,50.2895914592671));
#29430=CARTESIAN_POINT('Ctrl Pts',(41.7323874112646,39.8554254216633,50.2672194142301));
#29431=CARTESIAN_POINT('Ctrl Pts',(41.6564365685492,39.8512050833091,50.2448546892266));
#29432=CARTESIAN_POINT('Ctrl Pts',(41.5815829832299,39.846984744955,50.2186611357793));
#29433=CARTESIAN_POINT('Ctrl Pts',(41.5082336464741,39.8427644066008,50.1887766472665));
#29434=CARTESIAN_POINT('Ctrl Pts',(41.4348854038371,39.8385441311995,50.1588926045271));
#29435=CARTESIAN_POINT('Ctrl Pts',(41.3630417993178,39.8343238557983,50.1253179144891));
#29436=CARTESIAN_POINT('Ctrl Pts',(41.2930901047849,39.830103580397,50.0882387135514));
#29437=CARTESIAN_POINT('Ctrl Pts',(41.2230684422614,39.8258790837371,50.0511224247748));
#29438=CARTESIAN_POINT('Ctrl Pts',(41.1549428856186,39.8216545870773,50.0104948431069));
#29439=CARTESIAN_POINT('Ctrl Pts',(41.0890757816296,39.8174300904174,49.9665879422467));
#29440=CARTESIAN_POINT('Ctrl Pts',(41.0231770550162,39.8132035655878,49.9226599617981));
#29441=CARTESIAN_POINT('Ctrl Pts',(40.9595393185366,39.8089770407581,49.8754498058017));
#29442=CARTESIAN_POINT('Ctrl Pts',(40.8984934976422,39.8047505159285,49.8252311262625));
#29443=CARTESIAN_POINT('Ctrl Pts',(40.8373360870338,39.8005162651532,49.7749206486607));
#29444=CARTESIAN_POINT('Ctrl Pts',(40.7787804074337,39.7962820143778,49.7215909751311));
#29445=CARTESIAN_POINT('Ctrl Pts',(40.7231218770389,39.7920477636025,49.6655540224305));
#29446=CARTESIAN_POINT('Ctrl Pts',(40.6700382954596,39.7880094033571,49.6121095256205));
#29447=CARTESIAN_POINT('Ctrl Pts',(40.6195899396743,39.7839710431118,49.556202995311));
#29448=CARTESIAN_POINT('Ctrl Pts',(40.5719977575736,39.7799326828665,49.4981315838684));
#29449=CARTESIAN_POINT('Ctrl Pts',(40.5222903575728,39.7757148391114,49.4374792088401));
#29450=CARTESIAN_POINT('Ctrl Pts',(40.4755045721295,39.7714969953564,49.3742277636628));
#29451=CARTESIAN_POINT('Ctrl Pts',(40.4319254715984,39.7672791516013,49.3086913660436));
#29452=CARTESIAN_POINT('Ctrl Pts',(40.3884068159339,39.7630671580589,49.2432458683916));
#29453=CARTESIAN_POINT('Ctrl Pts',(40.3480862789779,39.7588551645164,49.1755220970716));
#29454=CARTESIAN_POINT('Ctrl Pts',(40.3112091156363,39.754643170974,49.1058675699644));
#29455=CARTESIAN_POINT('Ctrl Pts',(40.2743713555646,39.750435677949,49.0362874687588));
#29456=CARTESIAN_POINT('Ctrl Pts',(40.2409698857243,39.7462281849241,48.9647811226784));
#29457=CARTESIAN_POINT('Ctrl Pts',(40.2112061406572,39.7420206918991,48.8917241065504));
#29458=CARTESIAN_POINT('Ctrl Pts',(40.181461551302,39.7378159067835,48.8187141093428));
#29459=CARTESIAN_POINT('Ctrl Pts',(40.1553502204571,39.733611121668,48.7441558588768));
#29460=CARTESIAN_POINT('Ctrl Pts',(40.1330265412458,39.7294063365524,48.6684472890242));
#29461=CARTESIAN_POINT('Ctrl Pts',(40.1107120521572,39.7252032824459,48.5927698865721));
#29462=CARTESIAN_POINT('Ctrl Pts',(40.0921822489825,39.7210002283394,48.5159435595929));
#29463=CARTESIAN_POINT('Ctrl Pts',(40.0775419483511,39.7167971742329,48.438382298036));
#29464=CARTESIAN_POINT('Ctrl Pts',(40.0628968075301,39.7125927305662,48.3607953941631));
#29465=CARTESIAN_POINT('Ctrl Pts',(40.0521438325292,39.7083882868995,48.2824735346466));
#29466=CARTESIAN_POINT('Ctrl Pts',(40.0453366784163,39.7041838432328,48.2038408273345));
#29467=CARTESIAN_POINT('Ctrl Pts',(40.0394099234416,39.7005231787313,48.1353780334109));
#29468=CARTESIAN_POINT('Ctrl Pts',(40.0364735495153,39.6968625142298,48.0666799369991));
#29469=CARTESIAN_POINT('Ctrl Pts',(40.0365308224637,39.6932018497283,47.9980282657969));
#29470=CARTESIAN_POINT('',(40.0365300273278,38.8994518497758,47.9996405879596));
#29471=CARTESIAN_POINT('Ctrl Pts',(40.0365308224644,39.6932018496801,47.9980282648923));
#29472=CARTESIAN_POINT('Ctrl Pts',(40.036609302553,39.6881857094131,47.9039561607262));
#29473=CARTESIAN_POINT('Ctrl Pts',(40.0423081124997,39.6831695691462,47.8101261109713));
#29474=CARTESIAN_POINT('Ctrl Pts',(40.0535177843081,39.6781534288793,47.717136689651));
#29475=CARTESIAN_POINT('Ctrl Pts',(40.064867614996,39.6730745698628,47.6229845854869));
#29476=CARTESIAN_POINT('Ctrl Pts',(40.0818668921383,39.6679957108462,47.529694318329));
#29477=CARTESIAN_POINT('Ctrl Pts',(40.1043529074695,39.6629168518297,47.4378657923091));
#29478=CARTESIAN_POINT('Ctrl Pts',(40.117944819063,39.6598468813734,47.3823590611679));
#29479=CARTESIAN_POINT('Ctrl Pts',(40.1335404969883,39.656776910917,47.3273859930675));
#29480=CARTESIAN_POINT('Ctrl Pts',(40.1510956352582,39.6537069404606,47.273075245197));
#29481=CARTESIAN_POINT('Ctrl Pts',(40.175315670556,39.6494714401943,47.1981451472256));
#29482=CARTESIAN_POINT('Ctrl Pts',(40.2033306781086,39.6452359399281,47.1242844137133));
#29483=CARTESIAN_POINT('Ctrl Pts',(40.2350273968893,39.6410004396618,47.0519050318242));
#29484=CARTESIAN_POINT('Ctrl Pts',(40.2666781654886,39.6367710795266,46.979630577065));
#29485=CARTESIAN_POINT('Ctrl Pts',(40.3019998596699,39.6325417193913,46.9088336356899));
#29486=CARTESIAN_POINT('Ctrl Pts',(40.3408296986338,39.6283123592561,46.8399103005063));
#29487=CARTESIAN_POINT('Ctrl Pts',(40.3796141923963,39.6240879381366,46.7710674534884));
#29488=CARTESIAN_POINT('Ctrl Pts',(40.4218984606851,39.6198635170171,46.704094271529));
#29489=CARTESIAN_POINT('Ctrl Pts',(40.4674726095466,39.6156390958976,46.6393647343806));
#29490=CARTESIAN_POINT('Ctrl Pts',(40.5130176146013,39.6114173762155,46.5746765905477));
#29491=CARTESIAN_POINT('Ctrl Pts',(40.5618480551299,39.6071956565335,46.5122296265529));
#29492=CARTESIAN_POINT('Ctrl Pts',(40.613709937326,39.6029739368515,46.4523701176017));
#29493=CARTESIAN_POINT('Ctrl Pts',(40.6655548505453,39.5987535984973,46.3925301944152));
#29494=CARTESIAN_POINT('Ctrl Pts',(40.7204289287941,39.5945332601431,46.3352763996614));
#29495=CARTESIAN_POINT('Ctrl Pts',(40.7780379306252,39.590312921789,46.2809219079957));
#29496=CARTESIAN_POINT('Ctrl Pts',(40.8356460731289,39.5860926463877,46.2265682271113));
#29497=CARTESIAN_POINT('Ctrl Pts',(40.8959887158222,39.5818723709864,46.1751140844765));
#29498=CARTESIAN_POINT('Ctrl Pts',(40.9587358939018,39.5776520955851,46.1268347063399));
#29499=CARTESIAN_POINT('Ctrl Pts',(41.0215458337771,39.5734275989253,46.0785070375779));
#29500=CARTESIAN_POINT('Ctrl Pts',(41.0867647406477,39.5692031022654,46.0333607636821));
#29501=CARTESIAN_POINT('Ctrl Pts',(41.1540312741243,39.5649786056056,45.9916294228804));
#29502=CARTESIAN_POINT('Ctrl Pts',(41.2213301020876,39.5607520807759,45.9498780469712));
#29503=CARTESIAN_POINT('Ctrl Pts',(41.2906781036953,39.5565255559463,45.9115450976135));
#29504=CARTESIAN_POINT('Ctrl Pts',(41.3616890412668,39.5522990311166,45.8768182381448));
#29505=CARTESIAN_POINT('Ctrl Pts',(41.4328297844515,39.5480647803413,45.8420278991413));
#29506=CARTESIAN_POINT('Ctrl Pts',(41.5056391052079,39.5438305295659,45.8108570072194));
#29507=CARTESIAN_POINT('Ctrl Pts',(41.579710669082,39.5395962787906,45.78344504817));
#29508=CARTESIAN_POINT('Ctrl Pts',(41.6503554359434,39.5355579185453,45.7573012575576));
#29509=CARTESIAN_POINT('Ctrl Pts',(41.7221478859671,39.5315195583,45.7345763625703));
#29510=CARTESIAN_POINT('Ctrl Pts',(41.7947259995611,39.5274811980547,45.7153482048039));
#29511=CARTESIAN_POINT('Ctrl Pts',(41.8708471479427,39.5232456977884,45.6951813889697));
#29512=CARTESIAN_POINT('Ctrl Pts',(41.9481219784927,39.5190101975222,45.6787847683847));
#29513=CARTESIAN_POINT('Ctrl Pts',(42.0261427251915,39.5147746972559,45.6662859688958));
#29514=CARTESIAN_POINT('Ctrl Pts',(42.1040503665722,39.5105453371207,45.6538052886988));
#29515=CARTESIAN_POINT('Ctrl Pts',(42.1827013172257,39.5063159769854,45.6452112821123));
#29516=CARTESIAN_POINT('Ctrl Pts',(42.261674388957,39.5020866168502,45.6405813287529));
#29517=CARTESIAN_POINT('Ctrl Pts',(42.340555236514,39.4978621957307,45.6359567822191));
#29518=CARTESIAN_POINT('Ctrl Pts',(42.4197569915148,39.4936377746112,45.6352871171725));
#29519=CARTESIAN_POINT('Ctrl Pts',(42.4988515756488,39.4894133534917,45.6385981267705));
#29520=CARTESIAN_POINT('Ctrl Pts',(42.5778955802913,39.4851916338097,45.6419070190404));
#29521=CARTESIAN_POINT('Ctrl Pts',(42.6568320824179,39.4809699141276,45.6491915139728));
#29522=CARTESIAN_POINT('Ctrl Pts',(42.7352324463743,39.4767481944456,45.6604253275867));
#29523=CARTESIAN_POINT('Ctrl Pts',(42.8136071580807,39.4725278560914,45.6716554655468));
#29524=CARTESIAN_POINT('Ctrl Pts',(42.8914456156923,39.4683075177373,45.6868322897868));
#29525=CARTESIAN_POINT('Ctrl Pts',(42.9683252484153,39.4640871793831,45.7058777598145));
#29526=CARTESIAN_POINT('Ctrl Pts',(43.0452037343597,39.4598669039819,45.7249229457496));
#29527=CARTESIAN_POINT('Ctrl Pts',(43.1211229685864,39.4556466285806,45.7478365486077));
#29528=CARTESIAN_POINT('Ctrl Pts',(43.1956729699453,39.4514263531793,45.7744899537862));
#29529=CARTESIAN_POINT('Ctrl Pts',(43.2702975386727,39.4472018565194,45.8011700185791));
#29530=CARTESIAN_POINT('Ctrl Pts',(43.3435496956695,39.4429773598596,45.8315971997728));
#29531=CARTESIAN_POINT('Ctrl Pts',(43.4150375466559,39.4387528631998,45.8655939421519));
#29532=CARTESIAN_POINT('Ctrl Pts',(43.4865597187727,39.4345263383701,45.8996070062781));
#29533=CARTESIAN_POINT('Ctrl Pts',(43.5563154837181,39.4302998135405,45.9371928226232));
#29534=CARTESIAN_POINT('Ctrl Pts',(43.6239380600601,39.4260732887108,45.978128078726));
#29535=CARTESIAN_POINT('Ctrl Pts',(43.6916842482046,39.4218390379355,46.0191381631046));
#29536=CARTESIAN_POINT('Ctrl Pts',(43.7572890660339,39.4176047871602,46.0635096581189));
#29537=CARTESIAN_POINT('Ctrl Pts',(43.8204153786014,39.4133705363848,46.1109762857146));
#29538=CARTESIAN_POINT('Ctrl Pts',(43.8806212579013,39.4093321761395,46.1562469491759));
#29539=CARTESIAN_POINT('Ctrl Pts',(43.9385726368473,39.4052938158942,46.2043324398239));
#29540=CARTESIAN_POINT('Ctrl Pts',(43.9940081989544,39.4012554556489,46.2549704006619));
#29541=CARTESIAN_POINT('Ctrl Pts',(44.0521499505075,39.3970199553827,46.3080803471707));
#29542=CARTESIAN_POINT('Ctrl Pts',(44.1077449942743,39.3927844551164,46.3642002163054));
#29543=CARTESIAN_POINT('Ctrl Pts',(44.1604653953895,39.3885489548502,46.4230561098961));
#29544=CARTESIAN_POINT('Ctrl Pts',(44.2131093686571,39.3843195947149,46.4818266811225));
#29545=CARTESIAN_POINT('Ctrl Pts',(44.2628866643237,39.3800902345796,46.5433250536541));
#29546=CARTESIAN_POINT('Ctrl Pts',(44.3095043447309,39.3758608744444,46.6072388581118));
#29547=CARTESIAN_POINT('Ctrl Pts',(44.3560675853526,39.3716364533249,46.671078024497));
#29548=CARTESIAN_POINT('Ctrl Pts',(44.3994782678398,39.3674120322054,46.7373266402747));
#29549=CARTESIAN_POINT('Ctrl Pts',(44.4394831127008,39.3631876110859,46.8056386334496));
#29550=CARTESIAN_POINT('Ctrl Pts',(44.4794623752197,39.3589658914038,46.8739069423962));
#29551=CARTESIAN_POINT('Ctrl Pts',(44.5160398863722,39.3547441717218,46.9442356059145));
#29552=CARTESIAN_POINT('Ctrl Pts',(44.549005863483,39.3505224520398,47.0162499099793));
#29553=CARTESIAN_POINT('Ctrl Pts',(44.5819610542729,39.3463021136856,47.0882406512845));
#29554=CARTESIAN_POINT('Ctrl Pts',(44.6113068622305,39.3420817753315,47.1619155115332));
#29555=CARTESIAN_POINT('Ctrl Pts',(44.636880314397,39.3378614369773,47.2368768775859));
#29556=CARTESIAN_POINT('Ctrl Pts',(44.662453385096,39.333641161576,47.3118371254739));
#29557=CARTESIAN_POINT('Ctrl Pts',(44.6842540615746,39.3294208861747,47.3880833963766));
#29558=CARTESIAN_POINT('Ctrl Pts',(44.7021687160105,39.3252006107735,47.4652013052347));
#29559=CARTESIAN_POINT('Ctrl Pts',(44.7201012892742,39.3209761141136,47.5423963499672));
#29560=CARTESIAN_POINT('Ctrl Pts',(44.7341399694105,39.3167516174537,47.6204643159974));
#29561=CARTESIAN_POINT('Ctrl Pts',(44.744222073869,39.3125271207939,47.6989795533768));
#29562=CARTESIAN_POINT('Ctrl Pts',(44.7543090187195,39.3083005959643,47.7775324857163));
#29563=CARTESIAN_POINT('Ctrl Pts',(44.7604355674331,39.3040740711346,47.8565326485915));
#29564=CARTESIAN_POINT('Ctrl Pts',(44.7625911064243,39.299847546305,47.9355507583827));
#29565=CARTESIAN_POINT('Ctrl Pts',(44.7647505856684,39.2956132955296,48.0147133106296));
#29566=CARTESIAN_POINT('Ctrl Pts',(44.7629245611091,39.2913790447543,48.0938934048865));
#29567=CARTESIAN_POINT('Ctrl Pts',(44.7571545929269,39.2871447939789,48.1726634470399));
#29568=CARTESIAN_POINT('Ctrl Pts',(44.751651562672,39.2831064337336,48.2477893249418));
#29569=CARTESIAN_POINT('Ctrl Pts',(44.7425615182468,39.2790680734883,48.322541902322));
#29570=CARTESIAN_POINT('Ctrl Pts',(44.7299637392547,39.275029713243,48.3965594717799));
#29571=CARTESIAN_POINT('Ctrl Pts',(44.7167509763921,39.2707942129767,48.4741903457243));
#29572=CARTESIAN_POINT('Ctrl Pts',(44.6996290368853,39.2665587127105,48.5513077094673));
#29573=CARTESIAN_POINT('Ctrl Pts',(44.6786508668115,39.2623232124442,48.6274875840041));
#29574=CARTESIAN_POINT('Ctrl Pts',(44.6577031084255,39.258093852309,48.7035570219033));
#29575=CARTESIAN_POINT('Ctrl Pts',(44.6329103443977,39.2538644921737,48.7786912207728));
#29576=CARTESIAN_POINT('Ctrl Pts',(44.6043768093628,39.2496351320385,48.8524748226449));
#29577=CARTESIAN_POINT('Ctrl Pts',(44.5758765955811,39.245410710919,48.9261722605674));
#29578=CARTESIAN_POINT('Ctrl Pts',(44.5436444601154,39.2411862897995,48.9985218002329));
#29579=CARTESIAN_POINT('Ctrl Pts',(44.5078344371775,39.23696186868,49.0691232044758));
#29580=CARTESIAN_POINT('Ctrl Pts',(44.4720473140723,39.232740148998,49.1396794604553));
#29581=CARTESIAN_POINT('Ctrl Pts',(44.4326870564077,39.2285184293159,49.2084893823486));
#29582=CARTESIAN_POINT('Ctrl Pts',(44.389955318554,39.2242967096339,49.2751738199394));
#29583=CARTESIAN_POINT('Ctrl Pts',(44.3472375623345,39.2200763712797,49.3418364386792));
#29584=CARTESIAN_POINT('Ctrl Pts',(44.3011507694226,39.2158560329256,49.4063745591698));
#29585=CARTESIAN_POINT('Ctrl Pts',(44.2519411766446,39.2116356945714,49.4684360112542));
#29586=CARTESIAN_POINT('Ctrl Pts',(44.2027323179038,39.2074154191702,49.5304965375961));
#29587=CARTESIAN_POINT('Ctrl Pts',(44.1504010445462,39.2031951437689,49.5900801020268));
#29588=CARTESIAN_POINT('Ctrl Pts',(44.0952343943522,39.1989748683676,49.6468669615683));
#29589=CARTESIAN_POINT('Ctrl Pts',(44.0400125646563,39.1947503717077,49.7037106211985));
#29590=CARTESIAN_POINT('Ctrl Pts',(43.9819500206073,39.1905258750479,49.7577516504136));
#29591=CARTESIAN_POINT('Ctrl Pts',(43.9213708350321,39.1863013783881,49.8087070584298));
#29592=CARTESIAN_POINT('Ctrl Pts',(43.8607625655483,39.1820748535584,49.8596869300041));
#29593=CARTESIAN_POINT('Ctrl Pts',(43.7976356220278,39.1778483287288,49.9075779451866));
#29594=CARTESIAN_POINT('Ctrl Pts',(43.7323453021837,39.1736218038991,49.9521389388692));
#29595=CARTESIAN_POINT('Ctrl Pts',(43.6669356338237,39.1693875531238,49.9967813885543));
#29596=CARTESIAN_POINT('Ctrl Pts',(43.5993550885029,39.1651533023485,50.0380814077597));
#29597=CARTESIAN_POINT('Ctrl Pts',(43.5299857685759,39.1609190515731,50.0758426249877));
#29598=CARTESIAN_POINT('Ctrl Pts',(43.4638257042102,39.1568806913278,50.111856882659));
#29599=CARTESIAN_POINT('Ctrl Pts',(43.3960390519226,39.1528423310825,50.1446524083331));
#29600=CARTESIAN_POINT('Ctrl Pts',(43.3269729073796,39.1488039708372,50.1741001977564));
#29601=CARTESIAN_POINT('Ctrl Pts',(43.2545351713106,39.144568470571,50.2049855354594));
#29602=CARTESIAN_POINT('Ctrl Pts',(43.180414480439,39.1403329703047,50.2323053412393));
#29603=CARTESIAN_POINT('Ctrl Pts',(43.1049960563844,39.1360974700385,50.2558747751997));
#29604=CARTESIAN_POINT('Ctrl Pts',(43.0296869651061,39.1318681099032,50.2794100409622));
#29605=CARTESIAN_POINT('Ctrl Pts',(42.9530843207721,39.1276387497679,50.2992055927087));
#29606=CARTESIAN_POINT('Ctrl Pts',(42.8755938411415,39.1234093896327,50.3151243895671));
#29607=CARTESIAN_POINT('Ctrl Pts',(42.7981938543251,39.1191849685132,50.3310245965712));
#29608=CARTESIAN_POINT('Ctrl Pts',(42.7199085499042,39.1149605473937,50.3430569512118));
#29609=CARTESIAN_POINT('Ctrl Pts',(42.6411578697656,39.1107361262742,50.3511344756841));
#29610=CARTESIAN_POINT('Ctrl Pts',(42.5624575491984,39.1065144065922,50.359206834732));
#29611=CARTESIAN_POINT('Ctrl Pts',(42.4832929092245,39.1022926869101,50.3633293354524));
#29612=CARTESIAN_POINT('Ctrl Pts',(42.4040919191154,39.0980709672281,50.3634664577899));
#29613=CARTESIAN_POINT('Ctrl Pts',(42.3249168432175,39.0938506288739,50.3636035352616));
#29614=CARTESIAN_POINT('Ctrl Pts',(42.2457059097968,39.0896302905198,50.3597578228464));
#29615=CARTESIAN_POINT('Ctrl Pts',(42.1668885158669,39.0854099521656,50.3519458915684));
#29616=CARTESIAN_POINT('Ctrl Pts',(42.0880722976202,39.0811896767643,50.3441340768174));
#29617=CARTESIAN_POINT('Ctrl Pts',(42.0096500741269,39.076969401363,50.3323562084255));
#29618=CARTESIAN_POINT('Ctrl Pts',(41.9320460432017,39.0727491259617,50.3166807149922));
#29619=CARTESIAN_POINT('Ctrl Pts',(41.8543643901669,39.0685246293019,50.3009895424137));
#29620=CARTESIAN_POINT('Ctrl Pts',(41.7775030256827,39.0643001326421,50.2813930501334));
#29621=CARTESIAN_POINT('Ctrl Pts',(41.701875273582,39.0600756359822,50.2580106968887));
#29622=CARTESIAN_POINT('Ctrl Pts',(41.6262112127954,39.0558491111526,50.2346171178374));
#29623=CARTESIAN_POINT('Ctrl Pts',(41.5517823857096,39.0516225863229,50.2074342182114));
#29624=CARTESIAN_POINT('Ctrl Pts',(41.4789838319879,39.0473960614933,50.1766303450886));
#29625=CARTESIAN_POINT('Ctrl Pts',(41.4060522049507,39.0431618107179,50.1457701635183));
#29626=CARTESIAN_POINT('Ctrl Pts',(41.3347572297971,39.0389275599426,50.1112759870524));
#29627=CARTESIAN_POINT('Ctrl Pts',(41.26547077459,39.0346933091672,50.0733629391861));
#29628=CARTESIAN_POINT('Ctrl Pts',(41.1993897413464,39.0306549489219,50.037203875067));
#29629=CARTESIAN_POINT('Ctrl Pts',(41.1351357818285,39.0266165886766,49.9979354982365));
#29630=CARTESIAN_POINT('Ctrl Pts',(41.0730051680361,39.0225782284313,49.9557799356883));
#29631=CARTESIAN_POINT('Ctrl Pts',(41.0081093410906,39.0183601351013,49.9117481786377));
#29632=CARTESIAN_POINT('Ctrl Pts',(40.9452791040872,39.0141420417714,49.8643957276567));
#29633=CARTESIAN_POINT('Ctrl Pts',(40.8848766116523,39.0099239484414,49.8139436482377));
#29634=CARTESIAN_POINT('Ctrl Pts',(40.8245618272495,39.0057119800353,49.7635648282558));
#29635=CARTESIAN_POINT('Ctrl Pts',(40.7666681488711,39.0015000116292,49.7100956167142));
#29636=CARTESIAN_POINT('Ctrl Pts',(40.7115287850674,38.9972880432231,49.6538002894074));
#29637=CARTESIAN_POINT('Ctrl Pts',(40.6564533472651,38.9930809579763,49.5975702282721));
#29638=CARTESIAN_POINT('Ctrl Pts',(40.6041262095551,38.9888738727295,49.5385208975658));
#29639=CARTESIAN_POINT('Ctrl Pts',(40.5548462813506,38.9846667874827,49.4769557188536));
#29640=CARTESIAN_POINT('Ctrl Pts',(40.5055972915353,38.9804623434824,49.415429191323));
#29641=CARTESIAN_POINT('Ctrl Pts',(40.4593920102545,38.9762578994822,49.3513903188447));
#29642=CARTESIAN_POINT('Ctrl Pts',(40.4164904665994,38.9720534554819,49.2851771752599));
#29643=CARTESIAN_POINT('Ctrl Pts',(40.3736021703791,38.9678503097589,49.2189844774265));
#29644=CARTESIAN_POINT('Ctrl Pts',(40.3340158437539,38.9636471640359,49.150619238736));
#29645=CARTESIAN_POINT('Ctrl Pts',(40.2979484921268,38.9594440183129,49.0804489340769));
#29646=CARTESIAN_POINT('Ctrl Pts',(40.2618807714525,38.9552408295826,49.0102779114236));
#29647=CARTESIAN_POINT('Ctrl Pts',(40.229332312171,38.9510376408523,48.9383022082623));
#29648=CARTESIAN_POINT('Ctrl Pts',(40.2004736799548,38.946834452122,48.8649129484107));
#29649=CARTESIAN_POINT('Ctrl Pts',(40.1715861759055,38.9426270582803,48.7914502657284));
#29650=CARTESIAN_POINT('Ctrl Pts',(40.146396043925,38.9384196644386,48.7165716442099));
#29651=CARTESIAN_POINT('Ctrl Pts',(40.1250250095019,38.9342122705969,48.6406865329537));
#29652=CARTESIAN_POINT('Ctrl Pts',(40.1036429612815,38.9300027084286,48.5647623134718));
#29653=CARTESIAN_POINT('Ctrl Pts',(40.0860840344984,38.9257931462603,48.487831033692));
#29654=CARTESIAN_POINT('Ctrl Pts',(40.0724189301043,38.9215835840919,48.4103130560477));
#29655=CARTESIAN_POINT('Ctrl Pts',(40.0587299728202,38.9173666739941,48.3326597682189));
#29656=CARTESIAN_POINT('Ctrl Pts',(40.0489484706961,38.9131497638963,48.2544182077444));
#29657=CARTESIAN_POINT('Ctrl Pts',(40.043093244688,38.9089328537985,48.1760141689309));
#29658=CARTESIAN_POINT('Ctrl Pts',(40.0387050852656,38.9057725191242,48.1172547937692));
#29659=CARTESIAN_POINT('Ctrl Pts',(40.0365210911557,38.90261218445,48.0584042686917));
#29660=CARTESIAN_POINT('Ctrl Pts',(40.0365300273278,38.8994518497758,47.9996405879596));
#29661=CARTESIAN_POINT('',(40.0365309862254,38.105701849771,48.0021591264912));
#29662=CARTESIAN_POINT('Ctrl Pts',(40.036530027328,38.8994518497283,47.9996405870764));
#29663=CARTESIAN_POINT('Ctrl Pts',(40.0365329485919,38.898418728494,47.9804305942669));
#29664=CARTESIAN_POINT('Ctrl Pts',(40.0367700699565,38.8973856072597,47.9612226144579));
#29665=CARTESIAN_POINT('Ctrl Pts',(40.0372412719132,38.8963524860254,47.9420204022983));
#29666=CARTESIAN_POINT('Ctrl Pts',(40.0391730645693,38.8921169857592,47.8632968488409));
#29667=CARTESIAN_POINT('Ctrl Pts',(40.045047261029,38.8878814854929,47.7845203141424));
#29668=CARTESIAN_POINT('Ctrl Pts',(40.0548723269245,38.8836459852267,47.7061179864713));
#29669=CARTESIAN_POINT('Ctrl Pts',(40.0646831495931,38.8794166250914,47.6278293172895));
#29670=CARTESIAN_POINT('Ctrl Pts',(40.0784334100136,38.8751872649562,47.5499142396325));
#29671=CARTESIAN_POINT('Ctrl Pts',(40.0960795788996,38.8709579048209,47.4727987726337));
#29672=CARTESIAN_POINT('Ctrl Pts',(40.1137051407189,38.8667334837014,47.395773360512));
#29673=CARTESIAN_POINT('Ctrl Pts',(40.1352174659245,38.8625090625819,47.319546158604));
#29674=CARTESIAN_POINT('Ctrl Pts',(40.1605215708118,38.8582846414625,47.2445353707149));
#29675=CARTESIAN_POINT('Ctrl Pts',(40.1858094942024,38.8540629217804,47.1695725508068));
#29676=CARTESIAN_POINT('Ctrl Pts',(40.2148842350025,38.8498412020984,47.0958250445317));
#29677=CARTESIAN_POINT('Ctrl Pts',(40.247600655478,38.8456194824164,47.0236970231525));
#29678=CARTESIAN_POINT('Ctrl Pts',(40.2803063712865,38.8413991440622,46.9515926017407));
#29679=CARTESIAN_POINT('Ctrl Pts',(40.316651207031,38.837178805708,46.8811070401549));
#29680=CARTESIAN_POINT('Ctrl Pts',(40.3564420312162,38.8329584673539,46.8126242089717));
#29681=CARTESIAN_POINT('Ctrl Pts',(40.3962322618597,38.8287381919526,46.7441423993157));
#29682=CARTESIAN_POINT('Ctrl Pts',(40.439468141818,38.8245179165513,46.677663665831));
#29683=CARTESIAN_POINT('Ctrl Pts',(40.4859115062213,38.82029764115,46.6135456448609));
#29684=CARTESIAN_POINT('Ctrl Pts',(40.5324013248086,38.8160731444902,46.5493634909329));
#29685=CARTESIAN_POINT('Ctrl Pts',(40.5821047607004,38.8118486478303,46.4875471474579));
#29686=CARTESIAN_POINT('Ctrl Pts',(40.6347417216878,38.8076241511705,46.4284231957203));
#29687=CARTESIAN_POINT('Ctrl Pts',(40.6874039535424,38.8033976263408,46.3692708587281));
#29688=CARTESIAN_POINT('Ctrl Pts',(40.7430021863726,38.7991711015112,46.312813823386));
#29689=CARTESIAN_POINT('Ctrl Pts',(40.8012194223008,38.7949445766815,46.2593417609215));
#29690=CARTESIAN_POINT('Ctrl Pts',(40.8595430773846,38.7907103259062,46.2057719533195));
#29691=CARTESIAN_POINT('Ctrl Pts',(40.9204949398595,38.7864760751308,46.1551983223142));
#29692=CARTESIAN_POINT('Ctrl Pts',(40.9837250545877,38.7822418243555,46.1078700573435));
#29693=CARTESIAN_POINT('Ctrl Pts',(41.0440299338148,38.7782034641102,46.0627313553918));
#29694=CARTESIAN_POINT('Ctrl Pts',(41.106406611522,38.7741651038649,46.0205445468993));
#29695=CARTESIAN_POINT('Ctrl Pts',(41.1705301059344,38.7701267436196,45.9814871264997));
#29696=CARTESIAN_POINT('Ctrl Pts',(41.2377839072695,38.7658912433533,45.9405230459192));
#29697=CARTESIAN_POINT('Ctrl Pts',(41.3072150742202,38.7616557430871,45.9028459751863));
#29698=CARTESIAN_POINT('Ctrl Pts',(41.378468909298,38.7574202428208,45.8686941393528));
#29699=CARTESIAN_POINT('Ctrl Pts',(41.4496194489317,38.7531908826856,45.8345918128411));
#29700=CARTESIAN_POINT('Ctrl Pts',(41.5225869899038,38.7489615225503,45.8040047738802));
#29701=CARTESIAN_POINT('Ctrl Pts',(41.596989689193,38.7447321624151,45.777126885844));
#29702=CARTESIAN_POINT('Ctrl Pts',(41.6713055015552,38.7405077412956,45.7502803856084));
#29703=CARTESIAN_POINT('Ctrl Pts',(41.7470527026375,38.7362833201761,45.7271345874006));
#29704=CARTESIAN_POINT('Ctrl Pts',(41.8238281859263,38.7320588990566,45.7078358519585));
#29705=CARTESIAN_POINT('Ctrl Pts',(41.9005545727447,38.7278371793746,45.6885494576929));
#29706=CARTESIAN_POINT('Ctrl Pts',(41.9783074826781,38.7236154596925,45.6731053574836));
#29707=CARTESIAN_POINT('Ctrl Pts',(42.0566684780718,38.7193937400105,45.661600139636));
#29708=CARTESIAN_POINT('Ctrl Pts',(42.1350038340967,38.7151734016563,45.6500986862444));
#29709=CARTESIAN_POINT('Ctrl Pts',(42.2139464164861,38.7109530633022,45.6425336242445));
#29710=CARTESIAN_POINT('Ctrl Pts',(42.2930688968157,38.706732724948,45.6389501953428));
#29711=CARTESIAN_POINT('Ctrl Pts',(42.3721901969113,38.7025124495467,45.6353668198935));
#29712=CARTESIAN_POINT('Ctrl Pts',(42.4514909206817,38.6982921741455,45.635764979386));
#29713=CARTESIAN_POINT('Ctrl Pts',(42.5305414407572,38.6940718987442,45.6401378486986));
#29714=CARTESIAN_POINT('Ctrl Pts',(42.6096710297683,38.6898474020843,45.6445150918991));
#29715=CARTESIAN_POINT('Ctrl Pts',(42.6885494454001,38.6856229054245,45.6528749607679));
#29716=CARTESIAN_POINT('Ctrl Pts',(42.7667504961249,38.6813984087646,45.6651585675913));
#29717=CARTESIAN_POINT('Ctrl Pts',(42.8449890909696,38.677171883935,45.6774480717423));
#29718=CARTESIAN_POINT('Ctrl Pts',(42.9225492130191,38.6729453591054,45.6936649703704));
#29719=CARTESIAN_POINT('Ctrl Pts',(42.9990157474873,38.6687188342757,45.7136993690325));
#29720=CARTESIAN_POINT('Ctrl Pts',(43.075622060217,38.6644845835004,45.7337703899037));
#29721=CARTESIAN_POINT('Ctrl Pts',(43.1511303421672,38.660250332725,45.7576727129945));
#29722=CARTESIAN_POINT('Ctrl Pts',(43.2251416952759,38.6560160819497,45.7852468255769));
#29723=CARTESIAN_POINT('Ctrl Pts',(43.2957290369222,38.6519777217044,45.8115452679603));
#29724=CARTESIAN_POINT('Ctrl Pts',(43.3649545786653,38.6479393614591,45.8411831002522));
#29725=CARTESIAN_POINT('Ctrl Pts',(43.4324932301622,38.6439010012138,45.8739830267448));
#29726=CARTESIAN_POINT('Ctrl Pts',(43.5033289057883,38.6396655009475,45.9083841422852));
#29727=CARTESIAN_POINT('Ctrl Pts',(43.5725780501447,38.6354300006813,45.9463947277719));
#29728=CARTESIAN_POINT('Ctrl Pts',(43.6398484209544,38.631194500415,45.9878453503876));
#29729=CARTESIAN_POINT('Ctrl Pts',(43.7070212710787,38.6269651402798,46.0292358827573));
#29730=CARTESIAN_POINT('Ctrl Pts',(43.7722206479711,38.6227357801445,46.0740563048966));
#29731=CARTESIAN_POINT('Ctrl Pts',(43.8350769332684,38.6185064200093,46.1220903545429));
#29732=CARTESIAN_POINT('Ctrl Pts',(43.8978598154564,38.6142819988898,46.170068310378));
#29733=CARTESIAN_POINT('Ctrl Pts',(43.9583046724889,38.6100575777703,46.2212521526019));
#29734=CARTESIAN_POINT('Ctrl Pts',(44.0160703336841,38.6058331566508,46.2753820372366));
#29735=CARTESIAN_POINT('Ctrl Pts',(44.0737990548309,38.6016114369688,46.3294773068332));
#29736=CARTESIAN_POINT('Ctrl Pts',(44.1288516391055,38.5973897172867,46.386514559564));
#29737=CARTESIAN_POINT('Ctrl Pts',(44.1809204818222,38.5931679976047,46.4461941310684));
#29738=CARTESIAN_POINT('Ctrl Pts',(44.2329722878454,38.5889476592505,46.5058541756828));
#29739=CARTESIAN_POINT('Ctrl Pts',(44.2820419825228,38.5847273208964,46.5681544689535));
#29740=CARTESIAN_POINT('Ctrl Pts',(44.3278603352689,38.5805069825422,46.6327600910605));
#29741=CARTESIAN_POINT('Ctrl Pts',(44.3736780045635,38.5762867071409,46.6973647494748));
#29742=CARTESIAN_POINT('Ctrl Pts',(44.4162441579054,38.5720664317396,46.7642742847531));
#29743=CARTESIAN_POINT('Ctrl Pts',(44.4553321106632,38.5678461563383,46.8331236758864));
#29744=CARTESIAN_POINT('Ctrl Pts',(44.4944591604796,38.5636216596785,46.90204193245));
#29745=CARTESIAN_POINT('Ctrl Pts',(44.5301008276703,38.5593971630187,46.9729035117433));
#29746=CARTESIAN_POINT('Ctrl Pts',(44.5620760724659,38.5551726663588,47.045318116978));
#29747=CARTESIAN_POINT('Ctrl Pts',(44.5940666684929,38.5509461415292,47.1177674882754));
#29748=CARTESIAN_POINT('Ctrl Pts',(44.6223871675287,38.5467196166995,47.1917709318967));
#29749=CARTESIAN_POINT('Ctrl Pts',(44.646905420318,38.5424930918699,47.2669198726976));
#29750=CARTESIAN_POINT('Ctrl Pts',(44.6714684916514,38.5382588410945,47.3422061832428));
#29751=CARTESIAN_POINT('Ctrl Pts',(44.6922153049804,38.5340245903192,47.4186417209783));
#29752=CARTESIAN_POINT('Ctrl Pts',(44.7090642145296,38.5297903395438,47.4958047064096));
#29753=CARTESIAN_POINT('Ctrl Pts',(44.7251336374596,38.5257519792985,47.5693978753808));
#29754=CARTESIAN_POINT('Ctrl Pts',(44.737657817594,38.5217136190532,47.6436523139323));
#29755=CARTESIAN_POINT('Ctrl Pts',(44.7466099944902,38.5176752588079,47.7181986964925));
#29756=CARTESIAN_POINT('Ctrl Pts',(44.7559991884512,38.5134397585416,47.7963841985283));
#29757=CARTESIAN_POINT('Ctrl Pts',(44.7614944169681,38.5092042582754,47.8751880757596));
#29758=CARTESIAN_POINT('Ctrl Pts',(44.7630259780619,38.5049687580091,47.9541887797103));
#29759=CARTESIAN_POINT('Ctrl Pts',(44.7645553188783,38.5007393978739,48.0330749577161));
#29760=CARTESIAN_POINT('Ctrl Pts',(44.7621323939109,38.4965100377386,48.1121569305197));
#29761=CARTESIAN_POINT('Ctrl Pts',(44.7557391254035,38.4922806776033,48.1910068426604));
#29762=CARTESIAN_POINT('Ctrl Pts',(44.7493533229083,38.4880562564838,48.2697646744515));
#29763=CARTESIAN_POINT('Ctrl Pts',(44.7390064282714,38.4838318353643,48.3482905187185));
#29764=CARTESIAN_POINT('Ctrl Pts',(44.7247324071361,38.4796074142449,48.426156867962));
#29765=CARTESIAN_POINT('Ctrl Pts',(44.7104675139676,38.4753856945628,48.503973423147));
#29766=CARTESIAN_POINT('Ctrl Pts',(44.6922805631403,38.4711639748808,48.58113085995));
#29767=CARTESIAN_POINT('Ctrl Pts',(44.6702571692749,38.4669422551988,48.6572083583279));
#29768=CARTESIAN_POINT('Ctrl Pts',(44.6482409813659,38.4627219168446,48.7332609644872));
#29769=CARTESIAN_POINT('Ctrl Pts',(44.6223909733764,38.4585015784904,48.80823388336));
#29770=CARTESIAN_POINT('Ctrl Pts',(44.5928431708198,38.4542812401363,48.8817194956952));
#29771=CARTESIAN_POINT('Ctrl Pts',(44.5632958090143,38.450060964735,48.9552040118788));
#29772=CARTESIAN_POINT('Ctrl Pts',(44.530050938619,38.4458406893337,49.027200830655));
#29773=CARTESIAN_POINT('Ctrl Pts',(44.4932929180909,38.4416204139324,49.097321830627));
#29774=CARTESIAN_POINT('Ctrl Pts',(44.456498130979,38.4373959172726,49.1675129679343));
#29775=CARTESIAN_POINT('Ctrl Pts',(44.4161833925721,38.4331714206127,49.2358241216887));
#29776=CARTESIAN_POINT('Ctrl Pts',(44.3725790124487,38.4289469239529,49.3018918851222));
#29777=CARTESIAN_POINT('Ctrl Pts',(44.3289536979764,38.4247203991233,49.3679913675161));
#29778=CARTESIAN_POINT('Ctrl Pts',(44.2820358738255,38.4204938742936,49.4318449352347));
#29779=CARTESIAN_POINT('Ctrl Pts',(44.2320976715372,38.416267349464,49.4931204113694));
#29780=CARTESIAN_POINT('Ctrl Pts',(44.1820681838893,38.4120330986886,49.5545078970203));
#29781=CARTESIAN_POINT('Ctrl Pts',(44.1290076008186,38.4077988479133,49.6133075247097));
#29782=CARTESIAN_POINT('Ctrl Pts',(44.0732264810481,38.403564597138,49.6692224489323));
#29783=CARTESIAN_POINT('Ctrl Pts',(44.0200259814856,38.3995262368926,49.7225505627076));
#29784=CARTESIAN_POINT('Ctrl Pts',(43.9643513894669,38.3954878766473,49.7732547690044));
#29785=CARTESIAN_POINT('Ctrl Pts',(43.9064988409918,38.391449516402,49.8211127595485));
#29786=CARTESIAN_POINT('Ctrl Pts',(43.8458221134131,38.3872140161358,49.8713070263742));
#29787=CARTESIAN_POINT('Ctrl Pts',(43.7825187127748,38.3829785158695,49.9185608946895));
#29788=CARTESIAN_POINT('Ctrl Pts',(43.7169054649991,38.3787430156033,49.9625876890359));
#29789=CARTESIAN_POINT('Ctrl Pts',(43.6513873356063,38.374513655468,50.0065506585052));
#29790=CARTESIAN_POINT('Ctrl Pts',(43.583566395141,38.3702842953327,50.0472955848435));
#29791=CARTESIAN_POINT('Ctrl Pts',(43.5137927021419,38.3660549351975,50.0845757979876));
#29792=CARTESIAN_POINT('Ctrl Pts',(43.4441004903501,38.361830514078,50.1218124755719));
#29793=CARTESIAN_POINT('Ctrl Pts',(43.3724604694405,38.3576060929585,50.1555922602152));
#29794=CARTESIAN_POINT('Ctrl Pts',(43.2992505603425,38.353381671839,50.1857124400579));
#29795=CARTESIAN_POINT('Ctrl Pts',(43.2260874675976,38.349159952157,50.2158133586149));
#29796=CARTESIAN_POINT('Ctrl Pts',(43.1513569120975,38.344938232475,50.2422591391675));
#29797=CARTESIAN_POINT('Ctrl Pts',(43.0754591320902,38.3407165127929,50.2648941259529));
#29798=CARTESIAN_POINT('Ctrl Pts',(42.9995861854986,38.3364961744388,50.2875217066714));
#29799=CARTESIAN_POINT('Ctrl Pts',(42.9225472221832,38.3322758360846,50.3063408354675));
#29800=CARTESIAN_POINT('Ctrl Pts',(42.8447586500196,38.3280554977305,50.3212453950698));
#29801=CARTESIAN_POINT('Ctrl Pts',(42.7669712381927,38.3238352223292,50.3361497323476));
#29802=CARTESIAN_POINT('Ctrl Pts',(42.6884347009615,38.3196149469279,50.3471395294893));
#29803=CARTESIAN_POINT('Ctrl Pts',(42.60957519567,38.3153946715266,50.3541598667592));
#29804=CARTESIAN_POINT('Ctrl Pts',(42.5306368125019,38.3111701748668,50.3611872260019));
#29805=CARTESIAN_POINT('Ctrl Pts',(42.4513752845733,38.3069456782069,50.3642371523107));
#29806=CARTESIAN_POINT('Ctrl Pts',(42.3722208426973,38.3027211815471,50.3633067425367));
#29807=CARTESIAN_POINT('Ctrl Pts',(42.2930283989807,38.2984946567174,50.3623758860755));
#29808=CARTESIAN_POINT('Ctrl Pts',(42.2139436128266,38.2942681318878,50.3574609158405));
#29809=CARTESIAN_POINT('Ctrl Pts',(42.1353930751858,38.2900416070581,50.3486109972152));
#29810=CARTESIAN_POINT('Ctrl Pts',(42.0566989497956,38.2858073562828,50.3397449012355));
#29811=CARTESIAN_POINT('Ctrl Pts',(41.9785414887562,38.2815731055075,50.3269295598006));
#29812=CARTESIAN_POINT('Ctrl Pts',(41.9013383570951,38.2773388547321,50.3102655706207));
#29813=CARTESIAN_POINT('Ctrl Pts',(41.8277068991924,38.2733004944868,50.2943725130285));
#29814=CARTESIAN_POINT('Ctrl Pts',(41.7549437581605,38.2692621342415,50.2749791626272));
#29815=CARTESIAN_POINT('Ctrl Pts',(41.6833961085529,38.2652237739962,50.2522143112197));
#29816=CARTESIAN_POINT('Ctrl Pts',(41.6083557281623,38.2609882737299,50.2283381515063));
#29817=CARTESIAN_POINT('Ctrl Pts',(41.5343672976752,38.2567527734637,50.2006621554591));
#29818=CARTESIAN_POINT('Ctrl Pts',(41.4618433193258,38.2525172731974,50.169297693588));
#29819=CARTESIAN_POINT('Ctrl Pts',(41.389424477725,38.2482879130622,50.1379787002312));
#29820=CARTESIAN_POINT('Ctrl Pts',(41.3184662995248,38.2440585529269,50.1029820441847));
#29821=CARTESIAN_POINT('Ctrl Pts',(41.2493656198619,38.2398291927916,50.0644686880997));
#29822=CARTESIAN_POINT('Ctrl Pts',(41.1803456354663,38.2356047716721,50.0260003076297));
#29823=CARTESIAN_POINT('Ctrl Pts',(41.1131792469015,38.2313803505526,49.9840236153632));
#29824=CARTESIAN_POINT('Ctrl Pts',(41.0482413925371,38.2271559294332,49.938746788018));
#29825=CARTESIAN_POINT('Ctrl Pts',(40.9833450647032,38.2229342097511,49.893498914348));
#29826=CARTESIAN_POINT('Ctrl Pts',(40.9206748265075,38.2187124900691,49.8449553619555));
#29827=CARTESIAN_POINT('Ctrl Pts',(40.8605781143012,38.214490770387,49.7933685339973));
#29828=CARTESIAN_POINT('Ctrl Pts',(40.8005010654714,38.2102704320329,49.7417985850194));
#29829=CARTESIAN_POINT('Ctrl Pts',(40.7429962264743,38.2060500936787,49.6871876431736));
#29830=CARTESIAN_POINT('Ctrl Pts',(40.6883781180301,38.2018297553246,49.6298285106298));
#29831=CARTESIAN_POINT('Ctrl Pts',(40.6337608242993,38.1976094799233,49.5724702336861));
#29832=CARTESIAN_POINT('Ctrl Pts',(40.5820304982221,38.193389204522,49.5123641883541));
#29833=CARTESIAN_POINT('Ctrl Pts',(40.533463876334,38.1891689291207,49.4498390738112));
#29834=CARTESIAN_POINT('Ctrl Pts',(40.4848486765098,38.1849444324608,49.3872514195879));
#29835=CARTESIAN_POINT('Ctrl Pts',(40.4394037908502,38.180719935801,49.3222402341853));
#29836=CARTESIAN_POINT('Ctrl Pts',(40.3973644121932,38.1764954391412,49.2551657832133));
#29837=CARTESIAN_POINT('Ctrl Pts',(40.3553048505404,38.1722689143115,49.1880591299729));
#29838=CARTESIAN_POINT('Ctrl Pts',(40.3166542822164,38.1680423894819,49.1188876481202));
#29839=CARTESIAN_POINT('Ctrl Pts',(40.2816021398275,38.1638158646522,49.0480367106721));
#29840=CARTESIAN_POINT('Ctrl Pts',(40.2464859232974,38.1595816138769,48.9770562600856));
#29841=CARTESIAN_POINT('Ctrl Pts',(40.2149814638827,38.1553473631015,48.9043906511003));
#29842=CARTESIAN_POINT('Ctrl Pts',(40.1872301093111,38.1511131123262,48.8304455742315));
#29843=CARTESIAN_POINT('Ctrl Pts',(40.1607626247427,38.1470747520809,48.7599214426659));
#29844=CARTESIAN_POINT('Ctrl Pts',(40.1377087367046,38.1430363918356,48.6882339613397));
#29845=CARTESIAN_POINT('Ctrl Pts',(40.1181479461546,38.1389980315903,48.6157447890655));
#29846=CARTESIAN_POINT('Ctrl Pts',(40.091268239247,38.1334486679537,48.516132879224));
#29847=CARTESIAN_POINT('Ctrl Pts',(40.0708982267616,38.1278993043172,48.4146948253093));
#29848=CARTESIAN_POINT('Ctrl Pts',(40.0572375947585,38.1223499406806,48.3121774391067));
#29849=CARTESIAN_POINT('Ctrl Pts',(40.0435769627555,38.1168005770441,48.2096600529041));
#29850=CARTESIAN_POINT('Ctrl Pts',(40.0366259066926,38.1112512134075,48.1060629894526));
#29851=CARTESIAN_POINT('Ctrl Pts',(40.0365309862254,38.105701849771,48.0021591264911));
#29852=CARTESIAN_POINT('',(40.036530095277,37.3119518496952,47.9993289049744));
#29853=CARTESIAN_POINT('Ctrl Pts',(40.0365309862246,38.1057018497283,48.0021591256915));
#29854=CARTESIAN_POINT('Ctrl Pts',(40.0364594804506,38.1015213847461,47.923885923739));
#29855=CARTESIAN_POINT('Ctrl Pts',(40.0402806015298,38.0973409197639,47.8455205042509));
#29856=CARTESIAN_POINT('Ctrl Pts',(40.0479951025618,38.0931604547817,47.7674846170108));
#29857=CARTESIAN_POINT('Ctrl Pts',(40.0557053122759,38.0889823152518,47.6894921385139));
#29858=CARTESIAN_POINT('Ctrl Pts',(40.0673045584702,38.0848041757218,47.6118293051813));
#29859=CARTESIAN_POINT('Ctrl Pts',(40.0827415695637,38.0806260361919,47.5349152685025));
#29860=CARTESIAN_POINT('Ctrl Pts',(40.09817505423,38.0764488511152,47.4580188020482));
#29861=CARTESIAN_POINT('Ctrl Pts',(40.1174444687557,38.0722716660385,47.3818712629778));
#29862=CARTESIAN_POINT('Ctrl Pts',(40.14044727168,38.0680944809618,47.3068824711193));
#29863=CARTESIAN_POINT('Ctrl Pts',(40.163452360777,38.0639168807284,47.2318862263725));
#29864=CARTESIAN_POINT('Ctrl Pts',(40.1901914315531,38.0597392804951,47.1580494154471));
#29865=CARTESIAN_POINT('Ctrl Pts',(40.2205123195484,38.0555616802617,47.0857659535656));
#29866=CARTESIAN_POINT('Ctrl Pts',(40.2508654090067,38.0513796433233,47.0134057250268));
#29867=CARTESIAN_POINT('Ctrl Pts',(40.2848077193831,38.0471976063848,46.9426025802068));
#29868=CARTESIAN_POINT('Ctrl Pts',(40.3221395781701,38.0430155694463,46.8737289365819));
#29869=CARTESIAN_POINT('Ctrl Pts',(40.3594942267784,38.0388309795175,46.8048132479564));
#29870=CARTESIAN_POINT('Ctrl Pts',(40.4002422894582,38.0346463895887,46.7378298124712));
#29871=CARTESIAN_POINT('Ctrl Pts',(40.4441403040548,38.0304617996599,46.6731227296102));
#29872=CARTESIAN_POINT('Ctrl Pts',(40.488111138022,38.0262702682053,46.608308308659));
#29873=CARTESIAN_POINT('Ctrl Pts',(40.5352420593665,38.0220787367506,46.5457781553767));
#29874=CARTESIAN_POINT('Ctrl Pts',(40.5852493227092,38.0178872052959,46.4858433303741));
#29875=CARTESIAN_POINT('Ctrl Pts',(40.605590571862,38.0161822332588,46.4614638877329));
#29876=CARTESIAN_POINT('Ctrl Pts',(40.626407314884,38.0144772612217,46.4375134349776));
#29877=CARTESIAN_POINT('Ctrl Pts',(40.6476788097917,38.0127722891846,46.4140110696329));
#29878=CARTESIAN_POINT('Ctrl Pts',(40.7005215663789,38.0085367889183,46.3556263732812));
#29879=CARTESIAN_POINT('Ctrl Pts',(40.7563858928542,38.0043012886521,46.2997745547736));
#29880=CARTESIAN_POINT('Ctrl Pts',(40.8149993977995,38.0000657883858,46.2467848015933));
#29881=CARTESIAN_POINT('Ctrl Pts',(40.8735279317674,37.9958364282506,46.1938718667355));
#29882=CARTESIAN_POINT('Ctrl Pts',(40.9347973846144,37.9916070681153,46.1438130699485));
#29883=CARTESIAN_POINT('Ctrl Pts',(40.9984967336247,37.98737770798,46.0969027783008));
#29884=CARTESIAN_POINT('Ctrl Pts',(41.062121695002,37.9831532868605,46.0500472681478));
#29885=CARTESIAN_POINT('Ctrl Pts',(41.1281705377089,37.9789288657411,46.0063332335187));
#29886=CARTESIAN_POINT('Ctrl Pts',(41.1962983549,37.9747044446216,45.9660155382886));
#29887=CARTESIAN_POINT('Ctrl Pts',(41.2643826056398,37.9704827249395,45.9257236254625));
#29888=CARTESIAN_POINT('Ctrl Pts',(41.334542789331,37.9662610052575,45.8888239796809));
#29889=CARTESIAN_POINT('Ctrl Pts',(41.406405157928,37.9620392855754,45.8555280998092));
#29890=CARTESIAN_POINT('Ctrl Pts',(41.478244013478,37.9578189472213,45.8222431142011));
#29891=CARTESIAN_POINT('Ctrl Pts',(41.5517835224818,37.9535986088671,45.7925597502938));
#29892=CARTESIAN_POINT('Ctrl Pts',(41.6266268233561,37.949378270513,45.7666428027412));
#29893=CARTESIAN_POINT('Ctrl Pts',(41.7014690078267,37.9451579951117,45.7407262417799));
#29894=CARTESIAN_POINT('Ctrl Pts',(41.77761450156,37.9409377197104,45.7185761378162));
#29895=CARTESIAN_POINT('Ctrl Pts',(41.8546494449382,37.9367174443091,45.7003080178003));
#29896=CARTESIAN_POINT('Ctrl Pts',(41.931761441206,37.9324929476493,45.6820216254086));
#29897=CARTESIAN_POINT('Ctrl Pts',(42.0097642065436,37.9282684509894,45.6676250820813));
#29898=CARTESIAN_POINT('Ctrl Pts',(42.088232382933,37.9240439543296,45.657183021692));
#29899=CARTESIAN_POINT('Ctrl Pts',(42.1667382316886,37.9198174294999,45.6467359480968));
#29900=CARTESIAN_POINT('Ctrl Pts',(42.2457094682034,37.9155909046703,45.6402471780457));
#29901=CARTESIAN_POINT('Ctrl Pts',(42.3247168620443,37.9113643798406,45.6377292936584));
#29902=CARTESIAN_POINT('Ctrl Pts',(42.4038686787525,37.9071301290653,45.6352068066629));
#29903=CARTESIAN_POINT('Ctrl Pts',(42.4830563143533,37.9028958782899,45.6366697011167));
#29904=CARTESIAN_POINT('Ctrl Pts',(42.5618519886392,37.8986616275146,45.6420783781742));
#29905=CARTESIAN_POINT('Ctrl Pts',(42.6370023128456,37.8946232672693,45.647236831834));
#29906=CARTESIAN_POINT('Ctrl Pts',(42.7117957900945,37.890584907024,45.6559839738596));
#29907=CARTESIAN_POINT('Ctrl Pts',(42.7858703532216,37.8865465467787,45.66824218423));
#29908=CARTESIAN_POINT('Ctrl Pts',(42.8635610030867,37.8823110465124,45.6810988018009));
#29909=CARTESIAN_POINT('Ctrl Pts',(42.9407560751894,37.8780755462462,45.6978669098096));
#29910=CARTESIAN_POINT('Ctrl Pts',(43.0170313521786,37.8738400459799,45.7184955070549));
#29911=CARTESIAN_POINT('Ctrl Pts',(43.0931960542268,37.8696106858446,45.739094199382));
#29912=CARTESIAN_POINT('Ctrl Pts',(43.1684431598382,37.8653813257094,45.7635421458197));
#29913=CARTESIAN_POINT('Ctrl Pts',(43.2423568374042,37.8611519655741,45.7917370176135));
#29914=CARTESIAN_POINT('Ctrl Pts',(43.3161841991192,37.8569275444546,45.8198989636427));
#29915=CARTESIAN_POINT('Ctrl Pts',(43.3886807909189,37.8527031233351,45.8517989734217));
#29916=CARTESIAN_POINT('Ctrl Pts',(43.459445673463,37.8484787022157,45.887284849801));
#29917=CARTESIAN_POINT('Ctrl Pts',(43.5301653032023,37.8442569825336,45.922748033633));
#29918=CARTESIAN_POINT('Ctrl Pts',(43.5991550032072,37.8400352628516,45.9617923229416));
#29919=CARTESIAN_POINT('Ctrl Pts',(43.6660347024841,37.8358135431696,46.0042178042166));
#29920=CARTESIAN_POINT('Ctrl Pts',(43.7328925190213,37.8315932048154,46.0466294040632));
#29921=CARTESIAN_POINT('Ctrl Pts',(43.797641309668,37.8273728664612,46.0924197478833));
#29922=CARTESIAN_POINT('Ctrl Pts',(43.8599277787561,37.8231525281071,46.1413442164521));
#29923=CARTESIAN_POINT('Ctrl Pts',(43.9222133187453,37.8189322527058,46.1902679552368));
#29924=CARTESIAN_POINT('Ctrl Pts',(43.9820362419074,37.8147119773045,46.2423254348709));
#29925=CARTESIAN_POINT('Ctrl Pts',(44.0390754923038,37.8104917019032,46.2972310868972));
#29926=CARTESIAN_POINT('Ctrl Pts',(44.0961717952384,37.8062672052434,46.3521916573664));
#29927=CARTESIAN_POINT('Ctrl Pts',(44.1504785244211,37.8020427085835,46.4100057648622));
#29928=CARTESIAN_POINT('Ctrl Pts',(44.2017112058828,37.7978182119237,46.4703506377289));
#29929=CARTESIAN_POINT('Ctrl Pts',(44.2529684840208,37.7935916870941,46.5307244820112));
#29930=CARTESIAN_POINT('Ctrl Pts',(44.3011484885996,37.7893651622644,46.5936311389899));
#29931=CARTESIAN_POINT('Ctrl Pts',(44.3460084276921,37.7851386374348,46.6587164206436));
#29932=CARTESIAN_POINT('Ctrl Pts',(44.3909503692494,37.7809043866594,46.7239206760101));
#29933=CARTESIAN_POINT('Ctrl Pts',(44.4325598708682,37.7766701358841,46.7913111135161));
#29934=CARTESIAN_POINT('Ctrl Pts',(44.4706388108378,37.7724358851088,46.8605065353622));
#29935=CARTESIAN_POINT('Ctrl Pts',(44.5069560923395,37.7683975248634,46.9265007467512));
#29936=CARTESIAN_POINT('Ctrl Pts',(44.540062135037,37.7643591646181,46.9941362896968));
#29937=CARTESIAN_POINT('Ctrl Pts',(44.5698263442917,37.7603208043728,47.0630666637813));
#29938=CARTESIAN_POINT('Ctrl Pts',(44.601043548445,37.7560853041066,47.1353620015057));
#29939=CARTESIAN_POINT('Ctrl Pts',(44.628702976007,37.7518498038403,47.2093566274597));
#29940=CARTESIAN_POINT('Ctrl Pts',(44.6526180224422,37.7476143035741,47.2846661717293));
#29941=CARTESIAN_POINT('Ctrl Pts',(44.6764983996511,37.7433849434388,47.3598665410639));
#29942=CARTESIAN_POINT('Ctrl Pts',(44.6966450342552,37.7391555833035,47.4363775997551));
#29943=CARTESIAN_POINT('Ctrl Pts',(44.7129190262478,37.7349262231683,47.513794262764));
#29944=CARTESIAN_POINT('Ctrl Pts',(44.7291740135917,37.7307018020488,47.5911205191612));
#29945=CARTESIAN_POINT('Ctrl Pts',(44.7415652492095,37.7264773809293,47.6693498213845));
#29946=CARTESIAN_POINT('Ctrl Pts',(44.7500038304048,37.7222529598098,47.7480626308332));
#29947=CARTESIAN_POINT('Ctrl Pts',(44.758437015287,37.7180312401278,47.826725104928));
#29948=CARTESIAN_POINT('Ctrl Pts',(44.7629225126911,37.7138095204457,47.9058700071481));
#29949=CARTESIAN_POINT('Ctrl Pts',(44.7634228403172,37.7095878007637,47.985069535613));
#29950=CARTESIAN_POINT('Ctrl Pts',(44.7639230042384,37.7053674624096,48.0642431503449));
#29951=CARTESIAN_POINT('Ctrl Pts',(44.760440584591,37.7011471240554,48.1434708868438));
#29952=CARTESIAN_POINT('Ctrl Pts',(44.7529901830593,37.6969267857013,48.2223232766187));
#29953=CARTESIAN_POINT('Ctrl Pts',(44.7455398926619,37.6927065103,48.3011744901884));
#29954=CARTESIAN_POINT('Ctrl Pts',(44.7341217835124,37.6884862348987,48.3796499010185));
#29955=CARTESIAN_POINT('Ctrl Pts',(44.7188023381678,37.6842659594974,48.457325001949));
#29956=CARTESIAN_POINT('Ctrl Pts',(44.7034675698091,37.6800414628376,48.5350777960756));
#29957=CARTESIAN_POINT('Ctrl Pts',(44.6842237610639,37.6758169661777,48.612028219629));
#29958=CARTESIAN_POINT('Ctrl Pts',(44.6611884739575,37.6715924695179,48.6877624052983));
#29959=CARTESIAN_POINT('Ctrl Pts',(44.6381421276701,37.6673659446882,48.7635329507519));
#29960=CARTESIAN_POINT('Ctrl Pts',(44.6113008360124,37.6631394198586,48.8380856528865));
#29961=CARTESIAN_POINT('Ctrl Pts',(44.580831132685,37.6589128950289,48.9110247041722));
#29962=CARTESIAN_POINT('Ctrl Pts',(44.5503057317613,37.6546786442536,48.9840970855984));
#29963=CARTESIAN_POINT('Ctrl Pts',(44.516138868655,37.6504443934783,49.0555494974379));
#29964=CARTESIAN_POINT('Ctrl Pts',(44.4785439592545,37.6462101427029,49.1250090890062));
#29965=CARTESIAN_POINT('Ctrl Pts',(44.4426883154572,37.6421717824576,49.191255248747));
#29966=CARTESIAN_POINT('Ctrl Pts',(44.4037150128913,37.6381334222123,49.2556886129284));
#29967=CARTESIAN_POINT('Ctrl Pts',(44.3618448175453,37.634095061967,49.3180118940172));
#29968=CARTESIAN_POINT('Ctrl Pts',(44.3179306512096,37.6298595617007,49.3833776012869));
#29969=CARTESIAN_POINT('Ctrl Pts',(44.2706626089232,37.6256240614345,49.4466704190592));
#29970=CARTESIAN_POINT('Ctrl Pts',(44.2202630051063,37.6213885611682,49.5075254668301));
#29971=CARTESIAN_POINT('Ctrl Pts',(44.1699364647174,37.6171592010329,49.568292294098));
#29972=CARTESIAN_POINT('Ctrl Pts',(44.1164876748209,37.6129298408977,49.6266280108294));
#29973=CARTESIAN_POINT('Ctrl Pts',(44.0601821795825,37.6087004807624,49.6821966506615));
#29974=CARTESIAN_POINT('Ctrl Pts',(44.0039424374888,37.6044760596429,49.7377003978432));
#29975=CARTESIAN_POINT('Ctrl Pts',(43.9448529517098,37.6002516385234,49.7904431614876));
#29976=CARTESIAN_POINT('Ctrl Pts',(43.8832184703814,37.5960272174039,49.8401232051196));
#29977=CARTESIAN_POINT('Ctrl Pts',(43.8216234031389,37.5918054977219,49.8897714793027));
#29978=CARTESIAN_POINT('Ctrl Pts',(43.7574869349752,37.5875837780398,49.9363606270291));
#29979=CARTESIAN_POINT('Ctrl Pts',(43.6911485816734,37.5833620583578,49.9796276874561));
#29980=CARTESIAN_POINT('Ctrl Pts',(43.6248319339853,37.5791417200037,50.0228805910937));
#29981=CARTESIAN_POINT('Ctrl Pts',(43.5563152245564,37.5749213816495,50.0628133095885));
#29982=CARTESIAN_POINT('Ctrl Pts',(43.4859675478282,37.5707010432953,50.0992057845681));
#29983=CARTESIAN_POINT('Ctrl Pts',(43.4156209204442,37.566480767894,50.1355977166977));
#29984=CARTESIAN_POINT('Ctrl Pts',(43.343443797536,37.5622604924928,50.1684492958105));
#29985=CARTESIAN_POINT('Ctrl Pts',(43.2698291680371,37.5580402170915,50.1975867808421));
#29986=CARTESIAN_POINT('Ctrl Pts',(43.1961409067595,37.5538157204316,50.2267534101466));
#29987=CARTESIAN_POINT('Ctrl Pts',(43.1210127040735,37.5495912237718,50.2521983511218));
#29988=CARTESIAN_POINT('Ctrl Pts',(43.0448562340585,37.5453667271119,50.2737965780377));
#29989=CARTESIAN_POINT('Ctrl Pts',(42.9686632015215,37.5411402022823,50.2954051742058));
#29990=CARTESIAN_POINT('Ctrl Pts',(42.8914413762488,37.5369136774526,50.3131632719361));
#29991=CARTESIAN_POINT('Ctrl Pts',(42.8136137367968,37.532687152623,50.3269968022395));
#29992=CARTESIAN_POINT('Ctrl Pts',(42.735643831029,37.5284529018477,50.3408556197726));
#29993=CARTESIAN_POINT('Ctrl Pts',(42.6570663651013,37.5242186510723,50.3507754756478));
#29994=CARTESIAN_POINT('Ctrl Pts',(42.5783103730831,37.519984400297,50.3567341495703));
#29995=CARTESIAN_POINT('Ctrl Pts',(42.5031978953109,37.5159460400517,50.3624171554101));
#29996=CARTESIAN_POINT('Ctrl Pts',(42.4279234026227,37.5119076798064,50.3644974157545));
#29997=CARTESIAN_POINT('Ctrl Pts',(42.3528563546987,37.5078693195611,50.3629997709707));
#29998=CARTESIAN_POINT('Ctrl Pts',(42.2741247700564,37.5036338192948,50.3614290158881));
#29999=CARTESIAN_POINT('Ctrl Pts',(42.1953221253149,37.4993983190286,50.3559161414232));
#30000=CARTESIAN_POINT('Ctrl Pts',(42.1168755654281,37.4951628187624,50.346450722996));
#30001=CARTESIAN_POINT('Ctrl Pts',(42.0385427281531,37.4909334586271,50.336999026421));
#30002=CARTESIAN_POINT('Ctrl Pts',(41.9605654126611,37.4867040984918,50.3236062202699));
#30003=CARTESIAN_POINT('Ctrl Pts',(41.8833698332261,37.4824747383566,50.3063138796962));
#30004=CARTESIAN_POINT('Ctrl Pts',(41.8062644022232,37.4782503172371,50.289041732991));
#30005=CARTESIAN_POINT('Ctrl Pts',(41.7299393487857,37.4740258961176,50.2678792032686));
#30006=CARTESIAN_POINT('Ctrl Pts',(41.6548133079061,37.4698014749981,50.2429193553996));
#30007=CARTESIAN_POINT('Ctrl Pts',(41.5797353087096,37.4655797553161,50.2179754688815));
#30008=CARTESIAN_POINT('Ctrl Pts',(41.5058552444528,37.461358035634,50.189239231483));
#30009=CARTESIAN_POINT('Ctrl Pts',(41.4335779477341,37.457136315952,50.1568539259287));
#30010=CARTESIAN_POINT('Ctrl Pts',(41.361324299825,37.4529159775978,50.1244792167022));
#30011=CARTESIAN_POINT('Ctrl Pts',(41.2906728061292,37.4486956392437,50.0884580018988));
#30012=CARTESIAN_POINT('Ctrl Pts',(41.2220082188658,37.4444753008895,50.0489816505963));
#30013=CARTESIAN_POINT('Ctrl Pts',(41.153344655841,37.4402550254882,50.0095058881447));
#30014=CARTESIAN_POINT('Ctrl Pts',(41.0866683465688,37.436034750087,49.9665753267307));
#30015=CARTESIAN_POINT('Ctrl Pts',(41.0223380158291,37.4318144746857,49.92042648864));
#30016=CARTESIAN_POINT('Ctrl Pts',(40.957943339772,37.4275899780258,49.8742314909603));
#30017=CARTESIAN_POINT('Ctrl Pts',(40.8958997120076,37.423365481366,49.8248120604304));
#30018=CARTESIAN_POINT('Ctrl Pts',(40.8365349948571,37.4191409847061,49.7724467886494));
#30019=CARTESIAN_POINT('Ctrl Pts',(40.7771417768612,37.4149144598765,49.7200563764384));
#30020=CARTESIAN_POINT('Ctrl Pts',(40.7204303680073,37.4106879350469,49.6647176337779));
#30021=CARTESIAN_POINT('Ctrl Pts',(40.666691890193,37.4064614102172,49.6067462268128));
#30022=CARTESIAN_POINT('Ctrl Pts',(40.6128551802427,37.4022271594419,49.5486688500592));
#30023=CARTESIAN_POINT('Ctrl Pts',(40.5620025627237,37.3979929086665,49.4879495534256));
#30024=CARTESIAN_POINT('Ctrl Pts',(40.5143848293078,37.3937586578912,49.4249371456156));
#30025=CARTESIAN_POINT('Ctrl Pts',(40.4689700506842,37.3897202976459,49.3648399014603));
#30026=CARTESIAN_POINT('Ctrl Pts',(40.4264976334479,37.3856819374006,49.3026573435625));
#30027=CARTESIAN_POINT('Ctrl Pts',(40.3871465606955,37.3816435771553,49.2387136363099));
#30028=CARTESIAN_POINT('Ctrl Pts',(40.3446380882119,37.3772811922606,49.1696392977945));
#30029=CARTESIAN_POINT('Ctrl Pts',(40.3056184800292,37.3729188073658,49.0982601812154));
#30030=CARTESIAN_POINT('Ctrl Pts',(40.2703369551552,37.3685564224711,49.0249515873066));
#30031=CARTESIAN_POINT('Ctrl Pts',(40.2351169695126,37.3642016465959,48.9517708607319));
#30032=CARTESIAN_POINT('Ctrl Pts',(40.2036222892192,37.3598468707208,48.8766677337123));
#30033=CARTESIAN_POINT('Ctrl Pts',(40.1760577304954,37.3554920948456,48.8000445130183));
#30034=CARTESIAN_POINT('Ctrl Pts',(40.1485459309493,37.3511456541082,48.7235679508708));
#30035=CARTESIAN_POINT('Ctrl Pts',(40.1249494227624,37.3467992133708,48.6455774906775));
#30036=CARTESIAN_POINT('Ctrl Pts',(40.1054254988952,37.3424527726335,48.5664965134752));
#30037=CARTESIAN_POINT('Ctrl Pts',(40.0859237581091,37.3381112703218,48.4875053880746));
#30038=CARTESIAN_POINT('Ctrl Pts',(40.0704855060544,37.3337697680101,48.4074266254418));
#30039=CARTESIAN_POINT('Ctrl Pts',(40.0592185511532,37.3294282656984,48.3266996321309));
#30040=CARTESIAN_POINT('Ctrl Pts',(40.0479640197821,37.3250915505528,48.246061652599));
#30041=CARTESIAN_POINT('Ctrl Pts',(40.040871690593,37.3207548354073,48.1647772909337));
#30042=CARTESIAN_POINT('Ctrl Pts',(40.0379982524025,37.3164181202617,48.0832957696788));
#30043=CARTESIAN_POINT('Ctrl Pts',(40.0370118258954,37.3149293634172,48.0553238673531));
#30044=CARTESIAN_POINT('Ctrl Pts',(40.0365221448597,37.3134406065728,48.027328798736));
#30045=CARTESIAN_POINT('Ctrl Pts',(40.0365300952768,37.3119518497283,47.9993289055974));
#30046=CARTESIAN_POINT('',(40.0365307594277,36.5182018497731,47.9981053315523));
#30047=CARTESIAN_POINT('Ctrl Pts',(40.036530095277,37.3119518496952,47.9993289049744));
#30048=CARTESIAN_POINT('Ctrl Pts',(40.0365552543786,37.307240681783,47.9107233018587));
#30049=CARTESIAN_POINT('Ctrl Pts',(40.0415680366451,37.3025295138709,47.8222574099801));
#30050=CARTESIAN_POINT('Ctrl Pts',(40.0514920247457,37.2978183459587,47.7344802623775));
#30051=CARTESIAN_POINT('Ctrl Pts',(40.0610728789532,37.293270072376,47.6497381158331));
#30052=CARTESIAN_POINT('Ctrl Pts',(40.0752307320124,37.2887217987933,47.5656381757661));
#30053=CARTESIAN_POINT('Ctrl Pts',(40.0938452749518,37.2841735252106,47.4826598555709));
#30054=CARTESIAN_POINT('Ctrl Pts',(40.1134598248503,37.2793809101337,47.3952237897344));
#30055=CARTESIAN_POINT('Ctrl Pts',(40.1380230555135,37.2745882950568,47.309033667321));
#30056=CARTESIAN_POINT('Ctrl Pts',(40.1673362679649,37.26979567998,47.2246271216022));
#30057=CARTESIAN_POINT('Ctrl Pts',(40.1966494804162,37.2650030649031,47.1402205758833));
#30058=CARTESIAN_POINT('Ctrl Pts',(40.2307124154202,37.2602104498262,47.0575979838451));
#30059=CARTESIAN_POINT('Ctrl Pts',(40.2692704858121,37.2554178347493,46.9772672987195));
#30060=CARTESIAN_POINT('Ctrl Pts',(40.3033463952669,37.2511823344831,46.9062746083447));
#30061=CARTESIAN_POINT('Ctrl Pts',(40.3410390123655,37.2469468342168,46.8368518799383));
#30062=CARTESIAN_POINT('Ctrl Pts',(40.3821807048506,37.2427113339506,46.7693921286524));
#30063=CARTESIAN_POINT('Ctrl Pts',(40.4232627549404,37.2384819738153,46.7020301725934));
#30064=CARTESIAN_POINT('Ctrl Pts',(40.4677837088575,37.23425261368,46.6366259399305));
#30065=CARTESIAN_POINT('Ctrl Pts',(40.515529001641,37.2300232535448,46.5735500368944));
#30066=CARTESIAN_POINT('Ctrl Pts',(40.5632185378215,37.2257988324253,46.5105477934356));
#30067=CARTESIAN_POINT('Ctrl Pts',(40.6141246485976,37.2215744113058,46.4498688487173));
#30068=CARTESIAN_POINT('Ctrl Pts',(40.6679890572934,37.2173499901863,46.3918555614484));
#30069=CARTESIAN_POINT('Ctrl Pts',(40.721819020718,37.2131282705043,46.3338793725801));
#30070=CARTESIAN_POINT('Ctrl Pts',(40.7786032088003,37.2089065508222,46.2785658008439));
#30071=CARTESIAN_POINT('Ctrl Pts',(40.8380433709711,37.2046848311402,46.2262238219176));
#30072=CARTESIAN_POINT('Ctrl Pts',(40.8974640845854,37.2004644927861,46.1738989690537));
#30073=CARTESIAN_POINT('Ctrl Pts',(40.9595386947168,37.1962441544319,46.124544088298));
#30074=CARTESIAN_POINT('Ctrl Pts',(41.0239335197275,37.1920238160778,46.0784299433093));
#30075=CARTESIAN_POINT('Ctrl Pts',(41.0883273841898,37.1878035406765,46.0323164861843));
#30076=CARTESIAN_POINT('Ctrl Pts',(41.1550410123622,37.1835832652752,45.9894439409183));
#30077=CARTESIAN_POINT('Ctrl Pts',(41.2237104266237,37.1793629898739,45.9500406637043));
#30078=CARTESIAN_POINT('Ctrl Pts',(41.2924485262967,37.175138493214,45.9105979740336));
#30079=CARTESIAN_POINT('Ctrl Pts',(41.363145911833,37.1709139965542,45.8746317184821));
#30080=CARTESIAN_POINT('Ctrl Pts',(41.4354131207765,37.1666894998944,45.8423247247721));
#30081=CARTESIAN_POINT('Ctrl Pts',(41.507715025018,37.1624629750647,45.8100022205589));
#30082=CARTESIAN_POINT('Ctrl Pts',(41.5815878158893,37.1582364502351,45.7813426479462));
#30083=CARTESIAN_POINT('Ctrl Pts',(41.6566235285636,37.1540099254054,45.7564800284787));
#30084=CARTESIAN_POINT('Ctrl Pts',(41.7317964040052,37.1497756746301,45.7315719609764));
#30085=CARTESIAN_POINT('Ctrl Pts',(41.8081359954775,37.1455414238548,45.7104748411244));
#30086=CARTESIAN_POINT('Ctrl Pts',(41.8852209023398,37.1413071730794,45.6932722480726));
#30087=CARTESIAN_POINT('Ctrl Pts',(41.9587396049162,37.1372688128341,45.6768655042157));
#30088=CARTESIAN_POINT('Ctrl Pts',(42.0329358281995,37.1332304525888,45.6640009333683));
#30089=CARTESIAN_POINT('Ctrl Pts',(42.1074403732221,37.1291920923435,45.6547069893765));
#30090=CARTESIAN_POINT('Ctrl Pts',(42.1855819953439,37.1249565920773,45.6449593443273));
#30091=CARTESIAN_POINT('Ctrl Pts',(42.2643598434414,37.120721091811,45.6391027879781));
#30092=CARTESIAN_POINT('Ctrl Pts',(42.3433526931166,37.1164855915448,45.637208954748));
#30093=CARTESIAN_POINT('Ctrl Pts',(42.4222310282329,37.1122562314095,45.6353178669751));
#30094=CARTESIAN_POINT('Ctrl Pts',(42.5013232807296,37.1080268712743,45.6373781055342));
#30095=CARTESIAN_POINT('Ctrl Pts',(42.5802016825473,37.103797511139,45.6434097100881));
#30096=CARTESIAN_POINT('Ctrl Pts',(42.6589879707454,37.0995730900195,45.6494342709783));
#30097=CARTESIAN_POINT('Ctrl Pts',(42.7375604389768,37.0953486689,45.6594209462268));
#30098=CARTESIAN_POINT('Ctrl Pts',(42.8154914284748,37.0911242477805,45.6733377310482));
#30099=CARTESIAN_POINT('Ctrl Pts',(42.8933725825779,37.0869025280985,45.6872456163487));
#30100=CARTESIAN_POINT('Ctrl Pts',(42.9706126113401,37.0826808084164,45.7050785407085));
#30101=CARTESIAN_POINT('Ctrl Pts',(43.0467903065244,37.0784590887344,45.7267528202402));
#30102=CARTESIAN_POINT('Ctrl Pts',(43.1229430767061,37.0742387503803,45.748420008044));
#30103=CARTESIAN_POINT('Ctrl Pts',(43.1980337524171,37.0700184120261,45.7739259269379));
#30104=CARTESIAN_POINT('Ctrl Pts',(43.2716540948951,37.0657980736719,45.8031364221344));
#30105=CARTESIAN_POINT('Ctrl Pts',(43.3452733392119,37.0615777982707,45.8323464816112));
#30106=CARTESIAN_POINT('Ctrl Pts',(43.4174218581185,37.0573575228694,45.8652608332087));
#30107=CARTESIAN_POINT('Ctrl Pts',(43.4877106888523,37.0531372474681,45.9016969002891));
#30108=CARTESIAN_POINT('Ctrl Pts',(43.5580698247914,37.0489127508082,45.9381694119248));
#30109=CARTESIAN_POINT('Ctrl Pts',(43.6265651390422,37.0446882541484,45.9781704592332));
#30110=CARTESIAN_POINT('Ctrl Pts',(43.6928321724845,37.0404637574885,46.0214714015994));
#30111=CARTESIAN_POINT('Ctrl Pts',(43.7591310205564,37.0362372326589,46.0647931326349));
#30112=CARTESIAN_POINT('Ctrl Pts',(43.8231990766439,37.0320107078292,46.1114176382367));
#30113=CARTESIAN_POINT('Ctrl Pts',(43.8847029193674,37.0277841829996,46.1610743130507));
#30114=CARTESIAN_POINT('Ctrl Pts',(43.9463191890535,37.0235499322242,46.2108217586015));
#30115=CARTESIAN_POINT('Ctrl Pts',(44.0053615282488,37.0193156814489,46.2636121353245));
#30116=CARTESIAN_POINT('Ctrl Pts',(44.0615316703824,37.0150814306736,46.3191362490624));
#30117=CARTESIAN_POINT('Ctrl Pts',(44.1151031948386,37.0110430704283,46.372091632546));
#30118=CARTESIAN_POINT('Ctrl Pts',(44.1660621853139,37.007004710183,46.4275331154113));
#30119=CARTESIAN_POINT('Ctrl Pts',(44.2141849778257,37.0029663499377,46.485165584253));
#30120=CARTESIAN_POINT('Ctrl Pts',(44.2646569734169,36.9987308496714,46.5456114886044));
#30121=CARTESIAN_POINT('Ctrl Pts',(44.3122006470405,36.9944953494052,46.6086975227285));
#30122=CARTESIAN_POINT('Ctrl Pts',(44.3565278733249,36.9902598491389,46.6741081786954));
#30123=CARTESIAN_POINT('Ctrl Pts',(44.4007908392012,36.9860304890037,46.7394240099732));
#30124=CARTESIAN_POINT('Ctrl Pts',(44.4418463562146,36.9818011288684,46.8070573856887));
#30125=CARTESIAN_POINT('Ctrl Pts',(44.479446151567,36.9775717687331,46.8766593821849));
#30126=CARTESIAN_POINT('Ctrl Pts',(44.5170020381539,36.9733473476137,46.9461800979797));
#30127=CARTESIAN_POINT('Ctrl Pts',(44.5511100005808,36.9691229264942,47.0176644553284));
#30128=CARTESIAN_POINT('Ctrl Pts',(44.5815655960173,36.9648985053747,47.090735466889));
#30129=CARTESIAN_POINT('Ctrl Pts',(44.6120017156763,36.9606767856926,47.1637597509189));
#30130=CARTESIAN_POINT('Ctrl Pts',(44.6387899239713,36.9564550660106,47.2383682432688));
#30131=CARTESIAN_POINT('Ctrl Pts',(44.6617727313293,36.9522333463286,47.3141614237189));
#30132=CARTESIAN_POINT('Ctrl Pts',(44.6847480188151,36.9480130079744,47.3899298049779));
#30133=CARTESIAN_POINT('Ctrl Pts',(44.7039202416452,36.9437926696203,47.4668816558271));
#30134=CARTESIAN_POINT('Ctrl Pts',(44.7191813740651,36.9395723312661,47.5446010594111));
#30135=CARTESIAN_POINT('Ctrl Pts',(44.7344422788416,36.9353520558648,47.6223193036901));
#30136=CARTESIAN_POINT('Ctrl Pts',(44.7457921200483,36.9311317804635,47.700804617132));
#30137=CARTESIAN_POINT('Ctrl Pts',(44.7531740242177,36.9269115050623,47.7796310987295));
#30138=CARTESIAN_POINT('Ctrl Pts',(44.7605633120109,36.9226870084024,47.8585364251721));
#30139=CARTESIAN_POINT('Ctrl Pts',(44.7639766905991,36.9184625117426,47.9377831330323));
#30140=CARTESIAN_POINT('Ctrl Pts',(44.7634092838742,36.9142380150827,48.0169410093344));
#30141=CARTESIAN_POINT('Ctrl Pts',(44.7628416047388,36.9100114902531,48.0961368891259));
#30142=CARTESIAN_POINT('Ctrl Pts',(44.7582893600182,36.9057849654234,48.1752433831794));
#30143=CARTESIAN_POINT('Ctrl Pts',(44.7497997582814,36.9015584405938,48.2538336795631));
#30144=CARTESIAN_POINT('Ctrl Pts',(44.7412946378373,36.8973241898184,48.3325676363738));
#30145=CARTESIAN_POINT('Ctrl Pts',(44.7288378523836,36.8930899390431,48.4107830452673));
#30146=CARTESIAN_POINT('Ctrl Pts',(44.7125280832083,36.8888556882678,48.4880617842782));
#30147=CARTESIAN_POINT('Ctrl Pts',(44.6969728582246,36.8848173280225,48.5617653516834));
#30148=CARTESIAN_POINT('Ctrl Pts',(44.6779133952358,36.8807789677771,48.634616663293));
#30149=CARTESIAN_POINT('Ctrl Pts',(44.6554768925876,36.8767406075318,48.7062679575795));
#30150=CARTESIAN_POINT('Ctrl Pts',(44.6319451105851,36.8725051072656,48.7814170422553));
#30151=CARTESIAN_POINT('Ctrl Pts',(44.6046087080825,36.8682696069993,48.8555316137063));
#30152=CARTESIAN_POINT('Ctrl Pts',(44.5735771627301,36.8640341067331,48.9281986633033));
#30153=CARTESIAN_POINT('Ctrl Pts',(44.5425906032687,36.8598047465978,49.0007603687438));
#30154=CARTESIAN_POINT('Ctrl Pts',(44.507919721353,36.8555753864625,49.0718782914855));
#30155=CARTESIAN_POINT('Ctrl Pts',(44.4697236581007,36.8513460263273,49.1411548624084));
#30156=CARTESIAN_POINT('Ctrl Pts',(44.4315721999312,36.8471216052078,49.2103505326594));
#30157=CARTESIAN_POINT('Ctrl Pts',(44.3899039664761,36.8428971840883,49.2777087152894));
#30158=CARTESIAN_POINT('Ctrl Pts',(44.3449254128398,36.8386727629688,49.3428535211965));
#30159=CARTESIAN_POINT('Ctrl Pts',(44.2999756221384,36.8344510432868,49.4079566682316));
#30160=CARTESIAN_POINT('Ctrl Pts',(44.2517199787753,36.8302293236047,49.470848862644));
#30161=CARTESIAN_POINT('Ctrl Pts',(44.2004092899499,36.8260076039227,49.5311815142438));
#30162=CARTESIAN_POINT('Ctrl Pts',(44.1491153897534,36.8217872655686,49.5914944252687));
#30163=CARTESIAN_POINT('Ctrl Pts',(44.0947687328041,36.8175669272144,49.6492490991557));
#30164=CARTESIAN_POINT('Ctrl Pts',(44.0376606758367,36.8133465888603,49.7041296757343));
#30165=CARTESIAN_POINT('Ctrl Pts',(43.9805534707242,36.809126313459,49.7590094336843));
#30166=CARTESIAN_POINT('Ctrl Pts',(43.9206852868116,36.8049060380577,49.8110148552911));
#30167=CARTESIAN_POINT('Ctrl Pts',(43.8583835507378,36.8006857626564,49.8598676995522));
#30168=CARTESIAN_POINT('Ctrl Pts',(43.796019498414,36.7964612659966,49.9087694080384));
#30169=CARTESIAN_POINT('Ctrl Pts',(43.7312174016947,36.7922367693367,49.9545119497349));
#30170=CARTESIAN_POINT('Ctrl Pts',(43.6643364438341,36.7880122726769,49.9968584821396));
#30171=CARTESIAN_POINT('Ctrl Pts',(43.5974233766006,36.7837857478472,50.0392253450038));
#30172=CARTESIAN_POINT('Ctrl Pts',(43.5284298692115,36.7795592230176,50.0781927194547));
#30173=CARTESIAN_POINT('Ctrl Pts',(43.4577404219148,36.7753326981879,50.1135694076012));
#30174=CARTESIAN_POINT('Ctrl Pts',(43.3869217566782,36.7710984474126,50.1490107631476));
#30175=CARTESIAN_POINT('Ctrl Pts',(43.3144013876554,36.7668641966373,50.1808481275017));
#30176=CARTESIAN_POINT('Ctrl Pts',(43.2405843528913,36.7626299458619,50.2089382939716));
#30177=CARTESIAN_POINT('Ctrl Pts',(43.1701823397762,36.7585915856166,50.2357289158727));
#30178=CARTESIAN_POINT('Ctrl Pts',(43.098601334768,36.7545532253713,50.2591113121279));
#30179=CARTESIAN_POINT('Ctrl Pts',(43.0262026282942,36.750514865126,50.2790043240892));
#30180=CARTESIAN_POINT('Ctrl Pts',(42.9502696451231,36.7462793648597,50.2998684502049));
#30181=CARTESIAN_POINT('Ctrl Pts',(42.873148449299,36.7420438645935,50.3169731208476));
#30182=CARTESIAN_POINT('Ctrl Pts',(42.7952456191475,36.7378083643272,50.3301869756405));
#30183=CARTESIAN_POINT('Ctrl Pts',(42.7174557233725,36.733579004192,50.3433816745383));
#30184=CARTESIAN_POINT('Ctrl Pts',(42.6388869022777,36.7293496440567,50.3526966806937));
#30185=CARTESIAN_POINT('Ctrl Pts',(42.5599596166417,36.7251202839215,50.358050754743));
#30186=CARTESIAN_POINT('Ctrl Pts',(42.4811245017114,36.720895862802,50.3633985763438));
#30187=CARTESIAN_POINT('Ctrl Pts',(42.4019322199432,36.7166714416825,50.3647946260616));
#30188=CARTESIAN_POINT('Ctrl Pts',(42.3228105950758,36.712447020563,50.3622091856285));
#30189=CARTESIAN_POINT('Ctrl Pts',(42.243739566992,36.7082253008809,50.3596253985356));
#30190=CARTESIAN_POINT('Ctrl Pts',(42.1647395739628,36.7040035811989,50.3530651900187));
#30191=CARTESIAN_POINT('Ctrl Pts',(42.0862394746819,36.6997818615169,50.3425509116457));
#30192=CARTESIAN_POINT('Ctrl Pts',(42.007765060284,36.6955615231627,50.3320400734978));
#30193=CARTESIAN_POINT('Ctrl Pts',(41.9297906796978,36.6913411848086,50.3175777967216));
#30194=CARTESIAN_POINT('Ctrl Pts',(41.8527396017054,36.6871208464544,50.2992382428445));
#30195=CARTESIAN_POINT('Ctrl Pts',(41.775689673049,36.6829005710531,50.2808989625301));
#30196=CARTESIAN_POINT('Ctrl Pts',(41.6995634758968,36.6786802956518,50.2586826300551));
#30197=CARTESIAN_POINT('Ctrl Pts',(41.6247721537662,36.6744600202505,50.232714094398));
#30198=CARTESIAN_POINT('Ctrl Pts',(41.5499060228899,36.6702355235907,50.2067195841557));
#30199=CARTESIAN_POINT('Ctrl Pts',(41.4763778786821,36.6660110269308,50.1769655278032));
#30200=CARTESIAN_POINT('Ctrl Pts',(41.4045812274179,36.661786530271,50.1436258787604));
#30201=CARTESIAN_POINT('Ctrl Pts',(41.3327501067692,36.6575600054413,50.1102702234393));
#30202=CARTESIAN_POINT('Ctrl Pts',(41.2626525508697,36.6533334806117,50.0733257652574));
#30203=CARTESIAN_POINT('Ctrl Pts',(41.1946573738737,36.649106955782,50.0330124432829));
#30204=CARTESIAN_POINT('Ctrl Pts',(41.1265379039738,36.6448727050067,49.9926254299073));
#30205=CARTESIAN_POINT('Ctrl Pts',(41.0605288845522,36.6406384542314,49.9488575073244));
#30206=CARTESIAN_POINT('Ctrl Pts',(40.9969698785914,36.636404203456,49.9019718502964));
#30207=CARTESIAN_POINT('Ctrl Pts',(40.9363513237343,36.6323658432107,49.8572552797712));
#30208=CARTESIAN_POINT('Ctrl Pts',(40.8779613577221,36.6283274829654,49.809703322906));
#30209=CARTESIAN_POINT('Ctrl Pts',(40.8220636923022,36.6242891227201,49.7595759289525));
#30210=CARTESIAN_POINT('Ctrl Pts',(40.7643098066972,36.6201166587381,49.7077839309448));
#30211=CARTESIAN_POINT('Ctrl Pts',(40.7089831080756,36.6159441947562,49.6530326374279));
#30212=CARTESIAN_POINT('Ctrl Pts',(40.6564092697084,36.6117717307743,49.5955819647205));
#30213=CARTESIAN_POINT('Ctrl Pts',(40.6039242673574,36.6076063171636,49.538228368602));
#30214=CARTESIAN_POINT('Ctrl Pts',(40.5541832096105,36.6034409035529,49.4781848075652));
#30215=CARTESIAN_POINT('Ctrl Pts',(40.5074774148454,36.5992754899422,49.4157502271163));
#30216=CARTESIAN_POINT('Ctrl Pts',(40.4608158950588,36.595114024955,49.3533748318224));
#30217=CARTESIAN_POINT('Ctrl Pts',(40.4171842214425,36.5909525599677,49.2886132972042));
#30218=CARTESIAN_POINT('Ctrl Pts',(40.3768348452745,36.5867910949805,49.2217991641856));
#30219=CARTESIAN_POINT('Ctrl Pts',(40.3365102421364,36.5826321849794,49.1550260525821));
#30220=CARTESIAN_POINT('Ctrl Pts',(40.2994641884032,36.5784732749783,49.0862032564411));
#30221=CARTESIAN_POINT('Ctrl Pts',(40.2659060323137,36.5743143649772,49.0156935453103));
#30222=CARTESIAN_POINT('Ctrl Pts',(40.2323572752878,36.5701566198154,48.9452035827395));
#30223=CARTESIAN_POINT('Ctrl Pts',(40.2022946835431,36.5659988746537,48.8730280809267));
#30224=CARTESIAN_POINT('Ctrl Pts',(40.1758810270027,36.5618411294919,48.7995531469849));
#30225=CARTESIAN_POINT('Ctrl Pts',(40.1494532345774,36.5576811592157,48.726038891217));
#30226=CARTESIAN_POINT('Ctrl Pts',(40.1266784446724,36.5535211889395,48.6512242699834));
#30227=CARTESIAN_POINT('Ctrl Pts',(40.1076703512129,36.5493612186634,48.5755130078388));
#30228=CARTESIAN_POINT('Ctrl Pts',(40.0886566805686,36.5452000278059,48.4997795311728));
#30229=CARTESIAN_POINT('Ctrl Pts',(40.0734120047945,36.5410388369485,48.4231493647047));
#30230=CARTESIAN_POINT('Ctrl Pts',(40.0619989009569,36.536877646091,48.3460365613242));
#30231=CARTESIAN_POINT('Ctrl Pts',(40.0505713886998,36.5327112019577,48.2688264072465));
#30232=CARTESIAN_POINT('Ctrl Pts',(40.0429851519426,36.5285447578243,48.1911328822445));
#30233=CARTESIAN_POINT('Ctrl Pts',(40.0392508194379,36.524378313691,48.1133743682477));
#30234=CARTESIAN_POINT('Ctrl Pts',(40.0374055232866,36.5223194923851,48.0749505036252));
#30235=CARTESIAN_POINT('Ctrl Pts',(40.0364999718189,36.5202606710791,48.0365107667864));
#30236=CARTESIAN_POINT('Ctrl Pts',(40.0365307594277,36.5182018497731,47.9981053315523));
#30237=CARTESIAN_POINT('',(40.0365305727061,35.7244518497007,48.0016453409487));
#30238=CARTESIAN_POINT('Ctrl Pts',(40.0365307594284,36.5182018497283,47.9981053307162));
#30239=CARTESIAN_POINT('Ctrl Pts',(40.0366311430135,36.5114890265903,47.8728837325548));
#30240=CARTESIAN_POINT('Ctrl Pts',(40.0466856383398,36.5047762034523,47.7480505508952));
#30241=CARTESIAN_POINT('Ctrl Pts',(40.0664971456614,36.4980633803143,47.624826880369));
#30242=CARTESIAN_POINT('Ctrl Pts',(40.0789973475601,36.4938278800481,47.5470780884537));
#30243=CARTESIAN_POINT('Ctrl Pts',(40.0954112714295,36.4895923797818,47.4698069314393));
#30244=CARTESIAN_POINT('Ctrl Pts',(40.1156898620174,36.4853568795156,47.3934378561022));
#30245=CARTESIAN_POINT('Ctrl Pts',(40.1359390550856,36.4811275193803,47.317179491684));
#30246=CARTESIAN_POINT('Ctrl Pts',(40.1600416697815,36.4768981592451,47.2418210618124));
#30247=CARTESIAN_POINT('Ctrl Pts',(40.187897285383,36.4726687991098,47.1677788629914));
#30248=CARTESIAN_POINT('Ctrl Pts',(40.2157203714007,36.4684443779903,47.0938231301076));
#30249=CARTESIAN_POINT('Ctrl Pts',(40.2472875846211,36.4642199568709,47.0211810108107));
#30250=CARTESIAN_POINT('Ctrl Pts',(40.2824485681572,36.4599955357514,46.9502541381837));
#30251=CARTESIAN_POINT('Ctrl Pts',(40.3175870669089,36.4557738160693,46.8793726219511));
#30252=CARTESIAN_POINT('Ctrl Pts',(40.3563145667419,36.4515520963873,46.81020459472));
#30253=CARTESIAN_POINT('Ctrl Pts',(40.3984328992107,36.4473303767053,46.7431310402679));
#30254=CARTESIAN_POINT('Ctrl Pts',(40.4405374507487,36.4431100383511,46.6760794319842));
#30255=CARTESIAN_POINT('Ctrl Pts',(40.4860303824847,36.438889699997,46.6111213328787));
#30256=CARTESIAN_POINT('Ctrl Pts',(40.53466869794,36.4346693616428,46.5486111567003));
#30257=CARTESIAN_POINT('Ctrl Pts',(40.5833062878795,36.4304490862415,46.4861019129577));
#30258=CARTESIAN_POINT('Ctrl Pts',(40.635088878997,36.4262288108403,46.4260408891683));
#30259=CARTESIAN_POINT('Ctrl Pts',(40.6897323781643,36.422008535439,46.3687504474789));
#30260=CARTESIAN_POINT('Ctrl Pts',(40.7444305335605,36.4177840387791,46.3114027020014));
#30261=CARTESIAN_POINT('Ctrl Pts',(40.8019949886455,36.4135595421193,46.2568314149466));
#30262=CARTESIAN_POINT('Ctrl Pts',(40.862104279723,36.4093350454594,46.2053225374866));
#30263=CARTESIAN_POINT('Ctrl Pts',(40.922242429114,36.4051085206298,46.1537889307491));
#30264=CARTESIAN_POINT('Ctrl Pts',(40.9849274765946,36.4008819958001,46.1053209500218));
#30265=CARTESIAN_POINT('Ctrl Pts',(41.0498063512841,36.3966554709705,46.0601630089445));
#30266=CARTESIAN_POINT('Ctrl Pts',(41.1148038223814,36.3924212201952,46.0149225206649));
#30267=CARTESIAN_POINT('Ctrl Pts',(41.1820027348204,36.3881869694198,45.9730044116997));
#30268=CARTESIAN_POINT('Ctrl Pts',(41.2510228033739,36.3839527186445,45.9346085498063));
#30269=CARTESIAN_POINT('Ctrl Pts',(41.3168497738978,36.3799143583991,45.897989008243));
#30270=CARTESIAN_POINT('Ctrl Pts',(41.3843327850954,36.3758759981537,45.8645731447572));
#30271=CARTESIAN_POINT('Ctrl Pts',(41.4531259390844,36.3718376379084,45.8344931416259));
#30272=CARTESIAN_POINT('Ctrl Pts',(41.5252773580597,36.3676021376421,45.8029447275344));
#30273=CARTESIAN_POINT('Ctrl Pts',(41.5991443629551,36.3633666373759,45.774946259881));
#30274=CARTESIAN_POINT('Ctrl Pts',(41.6743434436451,36.3591311371096,45.7506861039154));
#30275=CARTESIAN_POINT('Ctrl Pts',(41.7494335095372,36.3549017769743,45.7264611174755));
#30276=CARTESIAN_POINT('Ctrl Pts',(41.8258513735225,36.3506724168391,45.7059638237071));
#30277=CARTESIAN_POINT('Ctrl Pts',(41.9031925918014,36.3464430567038,45.6893349788299));
#30278=CARTESIAN_POINT('Ctrl Pts',(41.9804434915723,36.3422186355843,45.672725552996));
#30279=CARTESIAN_POINT('Ctrl Pts',(42.0586151463996,36.3379942144648,45.6599756969946));
#30280=CARTESIAN_POINT('Ctrl Pts',(42.1372884297915,36.3337697933454,45.6511762365434));
#30281=CARTESIAN_POINT('Ctrl Pts',(42.2159114031058,36.3295480736633,45.6423824031808));
#30282=CARTESIAN_POINT('Ctrl Pts',(42.2950349031182,36.3253263539813,45.6375340034249));
#30283=CARTESIAN_POINT('Ctrl Pts',(42.3742313043362,36.3211046342993,45.6366704810324));
#30284=CARTESIAN_POINT('Ctrl Pts',(42.4534017928445,36.3168842959451,45.6358072411805));
#30285=CARTESIAN_POINT('Ctrl Pts',(42.5326446662259,36.3126639575909,45.6389262948231));
#30286=CARTESIAN_POINT('Ctrl Pts',(42.6115303935436,36.3084436192368,45.6460150099231));
#30287=CARTESIAN_POINT('Ctrl Pts',(42.6904149441587,36.3042233438355,45.653103619284));
#30288=CARTESIAN_POINT('Ctrl Pts',(42.7689418919513,36.3000030684342,45.6641617290631));
#30289=CARTESIAN_POINT('Ctrl Pts',(42.8466864293436,36.2957827930329,45.6791248041439));
#30290=CARTESIAN_POINT('Ctrl Pts',(42.9245087293847,36.2915582963731,45.6941028457856));
#30291=CARTESIAN_POINT('Ctrl Pts',(43.0015465937044,36.2873337997132,45.7129935662894));
#30292=CARTESIAN_POINT('Ctrl Pts',(43.0773856202172,36.2831093030534,45.7356813028147));
#30293=CARTESIAN_POINT('Ctrl Pts',(43.1532610568484,36.2788827782238,45.758379931663));
#30294=CARTESIAN_POINT('Ctrl Pts',(43.2279360661542,36.2746562533941,45.7848790508678));
#30295=CARTESIAN_POINT('Ctrl Pts',(43.3010140810621,36.2704297285645,45.8150139436079));
#30296=CARTESIAN_POINT('Ctrl Pts',(43.3742256801313,36.2661954777891,45.8452039219217));
#30297=CARTESIAN_POINT('Ctrl Pts',(43.4458340259795,36.2619612270138,45.8790427531237));
#30298=CARTESIAN_POINT('Ctrl Pts',(43.5154652931418,36.2577269762384,45.9163187334201));
#30299=CARTESIAN_POINT('Ctrl Pts',(43.5818751861916,36.2536886159932,45.9518702028346));
#30300=CARTESIAN_POINT('Ctrl Pts',(43.6464865999726,36.2496502557479,45.9905476115089));
#30301=CARTESIAN_POINT('Ctrl Pts',(43.7090012376697,36.2456118955026,46.0321315591028));
#30302=CARTESIAN_POINT('Ctrl Pts',(43.7745676429749,36.2413763952364,46.0757455039735));
#30303=CARTESIAN_POINT('Ctrl Pts',(43.838076561073,36.2371408949701,46.1227227955636));
#30304=CARTESIAN_POINT('Ctrl Pts',(43.8991620957885,36.2329053947038,46.172842795091));
#30305=CARTESIAN_POINT('Ctrl Pts',(43.9601590758679,36.2286760345686,46.2228901365277));
#30306=CARTESIAN_POINT('Ctrl Pts',(44.0187392892554,36.2244466744333,46.2760708434371));
#30307=CARTESIAN_POINT('Ctrl Pts',(44.0745655553659,36.2202173142981,46.3321209151494));
#30308=CARTESIAN_POINT('Ctrl Pts',(44.130326627972,36.2159928931786,46.3881055319988));
#30309=CARTESIAN_POINT('Ctrl Pts',(44.1833398146736,36.2117684720591,46.4469525241243));
#30310=CARTESIAN_POINT('Ctrl Pts',(44.2333019846281,36.2075440509396,46.5083585303235));
#30311=CARTESIAN_POINT('Ctrl Pts',(44.2832322047192,36.2033223312575,46.5697252685423));
#30312=CARTESIAN_POINT('Ctrl Pts',(44.3301149850966,36.1991006115755,46.6336474097649));
#30313=CARTESIAN_POINT('Ctrl Pts',(44.3736858107019,36.1948788918935,46.6997866476867));
#30314=CARTESIAN_POINT('Ctrl Pts',(44.4172423801271,36.1906585535393,46.7659042451443));
#30315=CARTESIAN_POINT('Ctrl Pts',(44.4574888885549,36.1864382151852,46.8342371072001));
#30316=CARTESIAN_POINT('Ctrl Pts',(44.4942035873017,36.182217876831,46.904417152456));
#30317=CARTESIAN_POINT('Ctrl Pts',(44.5309177383921,36.1779976014297,46.9745961508681));
#30318=CARTESIAN_POINT('Ctrl Pts',(44.5640999681374,36.1737773260284,47.0466218612126));
#30319=CARTESIAN_POINT('Ctrl Pts',(44.5935747350978,36.1695570506271,47.1201020954449));
#30320=CARTESIAN_POINT('Ctrl Pts',(44.6230789836917,36.1653325539673,47.1936558270296));
#30321=CARTESIAN_POINT('Ctrl Pts',(44.6488681864982,36.1611080573074,47.2686665521205));
#30322=CARTESIAN_POINT('Ctrl Pts',(44.6708154312115,36.1568835606476,47.344723174321));
#30323=CARTESIAN_POINT('Ctrl Pts',(44.6927732127395,36.1526570358179,47.420816311107));
#30324=CARTESIAN_POINT('Ctrl Pts',(44.710885254245,36.1484305109883,47.4979558877583));
#30325=CARTESIAN_POINT('Ctrl Pts',(44.7250755477863,36.1442039861587,47.5757192698385));
#30326=CARTESIAN_POINT('Ctrl Pts',(44.7392917807084,36.1399697353833,47.653624800774));
#30327=CARTESIAN_POINT('Ctrl Pts',(44.7495718795936,36.135735484608,47.7321559491111));
#30328=CARTESIAN_POINT('Ctrl Pts',(44.7558916568792,36.1315012338326,47.810883787191));
#30329=CARTESIAN_POINT('Ctrl Pts',(44.7619190602389,36.1274628735873,47.8859694135201));
#30330=CARTESIAN_POINT('Ctrl Pts',(44.7643444989689,36.123424513342,47.9612335748426));
#30331=CARTESIAN_POINT('Ctrl Pts',(44.7631911188751,36.1193861530967,48.0363067014481));
#30332=CARTESIAN_POINT('Ctrl Pts',(44.7619814343997,36.1151506528304,48.1150446615137));
#30333=CARTESIAN_POINT('Ctrl Pts',(44.7568299978679,36.1109151525642,48.1938717590423));
#30334=CARTESIAN_POINT('Ctrl Pts',(44.747724425971,36.1066796522979,48.2723609013776));
#30335=CARTESIAN_POINT('Ctrl Pts',(44.7386320542631,36.1024502921627,48.3507362593697));
#30336=CARTESIAN_POINT('Ctrl Pts',(44.7255969840385,36.0982209320274,48.4287741727973));
#30337=CARTESIAN_POINT('Ctrl Pts',(44.708658835443,36.0939915718922,48.5060482412094));
#30338=CARTESIAN_POINT('Ctrl Pts',(44.6917404670933,36.0897671507727,48.5832320695306));
#30339=CARTESIAN_POINT('Ctrl Pts',(44.6709281779119,36.0855427296532,48.6596533693462));
#30340=CARTESIAN_POINT('Ctrl Pts',(44.6463131119784,36.0813183085337,48.7348930832808));
#30341=CARTESIAN_POINT('Ctrl Pts',(44.6217137869143,36.0770965888517,48.8100846828406));
#30342=CARTESIAN_POINT('Ctrl Pts',(44.5933166572539,36.0728748691697,48.8840957513468));
#30343=CARTESIAN_POINT('Ctrl Pts',(44.5612631476989,36.0686531494876,48.9565208033799));
#30344=CARTESIAN_POINT('Ctrl Pts',(44.5292201259095,36.0644328111335,49.0289221582586));
#30345=CARTESIAN_POINT('Ctrl Pts',(44.4935232895901,36.0602124727793,49.0997380982307));
#30346=CARTESIAN_POINT('Ctrl Pts',(44.4543622413764,36.0559921344252,49.1685829975261));
#30347=CARTESIAN_POINT('Ctrl Pts',(44.4152017773102,36.0517718590239,49.2374268698934));
#30348=CARTESIAN_POINT('Ctrl Pts',(44.37257743729,36.0475515836226,49.3042993527195));
#30349=CARTESIAN_POINT('Ctrl Pts',(44.3267240960435,36.0433313082214,49.3688406403324));
#30350=CARTESIAN_POINT('Ctrl Pts',(44.2808248907736,36.0391068115615,49.4334464842685));
#30351=CARTESIAN_POINT('Ctrl Pts',(44.2316905049191,36.0348823149017,49.4957160915161));
#30352=CARTESIAN_POINT('Ctrl Pts',(44.1795980236105,36.0306578182418,49.5553203256119));
#30353=CARTESIAN_POINT('Ctrl Pts',(44.1274805328378,36.0264312934122,49.6149531755447));
#30354=CARTESIAN_POINT('Ctrl Pts',(44.0724024441464,36.0222047685826,49.6719177652434));
#30355=CARTESIAN_POINT('Ctrl Pts',(44.0146780853099,36.0179782437529,49.7259215282625));
#30356=CARTESIAN_POINT('Ctrl Pts',(43.9568482082806,36.0137439929776,49.78002400835));
#30357=CARTESIAN_POINT('Ctrl Pts',(43.8963627544433,36.0095097422022,49.8311545429287));
#30358=CARTESIAN_POINT('Ctrl Pts',(43.8335693787318,36.0052754914269,49.8790607433669));
#30359=CARTESIAN_POINT('Ctrl Pts',(43.7736810335206,36.0012371311816,49.9247506435688));
#30360=CARTESIAN_POINT('Ctrl Pts',(43.7116939031599,35.9971987709362,49.9675077763346));
#30361=CARTESIAN_POINT('Ctrl Pts',(43.6479313278327,35.9931604106909,50.0071516738687));
#30362=CARTESIAN_POINT('Ctrl Pts',(43.5810560645158,35.9889249104246,50.0487308615488));
#30363=CARTESIAN_POINT('Ctrl Pts',(43.5119733797754,35.9846894101584,50.0870431477272));
#30364=CARTESIAN_POINT('Ctrl Pts',(43.4410357712582,35.9804539098921,50.1218470642016));
#30365=CARTESIAN_POINT('Ctrl Pts',(43.3702009997569,35.9762245497569,50.1566005260443));
#30366=CARTESIAN_POINT('Ctrl Pts',(43.297517062263,35.9719951896216,50.1878555131392));
#30367=CARTESIAN_POINT('Ctrl Pts',(43.2233640076852,35.9677658294863,50.2154146681262));
#30368=CARTESIAN_POINT('Ctrl Pts',(43.1492975485011,35.9635414083668,50.2429416397339));
#30369=CARTESIAN_POINT('Ctrl Pts',(43.073765819162,35.9593169872473,50.2667811932017));
#30370=CARTESIAN_POINT('Ctrl Pts',(42.9971705668534,35.9550925661278,50.2867832767851));
#30371=CARTESIAN_POINT('Ctrl Pts',(42.9206242957608,35.9508708464458,50.3067725694141));
#30372=CARTESIAN_POINT('Ctrl Pts',(42.8430163044532,35.9466491267638,50.322929144534));
#30373=CARTESIAN_POINT('Ctrl Pts',(42.764764127109,35.9424274070817,50.3351525801271));
#30374=CARTESIAN_POINT('Ctrl Pts',(42.6865375535287,35.9382070687276,50.3473720162666));
#30375=CARTESIAN_POINT('Ctrl Pts',(42.6076676758178,35.9339867303734,50.3556607958653));
#30376=CARTESIAN_POINT('Ctrl Pts',(42.5285813894844,35.9297663920192,50.3599697598017));
#30377=CARTESIAN_POINT('Ctrl Pts',(42.4494962828452,35.9255461166179,50.3642786594632));
#30378=CARTESIAN_POINT('Ctrl Pts',(42.3701952427293,35.9213258412166,50.3646078372648));
#30379=CARTESIAN_POINT('Ctrl Pts',(42.2911079410338,35.9171055658154,50.3609601776384));
#30380=CARTESIAN_POINT('Ctrl Pts',(42.2119415336124,35.9128810691555,50.3573088695025));
#30381=CARTESIAN_POINT('Ctrl Pts',(42.1329897616534,35.9086565724957,50.3496727995296));
#30382=CARTESIAN_POINT('Ctrl Pts',(42.0546793388577,35.9044320758358,50.3381069440657));
#30383=CARTESIAN_POINT('Ctrl Pts',(41.9763313194327,35.9002055510062,50.3265355358649));
#30384=CARTESIAN_POINT('Ctrl Pts',(41.8986257234762,35.8959790261765,50.3110306756431));
#30385=CARTESIAN_POINT('Ctrl Pts',(41.8219786562303,35.8917525013469,50.2916984459232));
#30386=CARTESIAN_POINT('Ctrl Pts',(41.7451914807151,35.8875182505715,50.2723308775354));
#30387=CARTESIAN_POINT('Ctrl Pts',(41.6694671503326,35.8832839997962,50.2491220972927));
#30388=CARTESIAN_POINT('Ctrl Pts',(41.5952060093662,35.8790497490208,50.2222279526502));
#30389=CARTESIAN_POINT('Ctrl Pts',(41.5243804358801,35.8750113887755,50.1965780206273));
#30390=CARTESIAN_POINT('Ctrl Pts',(41.4548859772165,35.8709730285303,50.1675763491656));
#30391=CARTESIAN_POINT('Ctrl Pts',(41.3870493361438,35.866934668285,50.1353972448922));
#30392=CARTESIAN_POINT('Ctrl Pts',(41.3159011240294,35.8626991680187,50.1016472581552));
#30393=CARTESIAN_POINT('Ctrl Pts',(41.2463062715651,35.8584636677525,50.0642734021379));
#30394=CARTESIAN_POINT('Ctrl Pts',(41.1786585585128,35.8542281674862,50.0234415050122));
#30395=CARTESIAN_POINT('Ctrl Pts',(41.1111089131723,35.849998807351,49.9826688011768));
#30396=CARTESIAN_POINT('Ctrl Pts',(41.0455012002203,35.8457694472157,49.9384482517782));
#30397=CARTESIAN_POINT('Ctrl Pts',(40.9822070059609,35.8415400870805,49.8909927199632));
#30398=CARTESIAN_POINT('Ctrl Pts',(40.9189867261978,35.837315665961,49.8435926063704));
#30399=CARTESIAN_POINT('Ctrl Pts',(40.8580749698998,35.8330912448415,49.7929652976213));
#30400=CARTESIAN_POINT('Ctrl Pts',(40.7998152766036,35.828866823722,49.7393674976579));
#30401=CARTESIAN_POINT('Ctrl Pts',(40.7415928392801,35.82464510404,49.6858039724745));
#30402=CARTESIAN_POINT('Ctrl Pts',(40.6860194433523,35.820423384358,49.6292740432384));
#30403=CARTESIAN_POINT('Ctrl Pts',(40.6334054289925,35.8162016646759,49.5700745404556));
#30404=CARTESIAN_POINT('Ctrl Pts',(40.5808086297038,35.8119813263218,49.5108944074863));
#30405=CARTESIAN_POINT('Ctrl Pts',(40.5311696008259,35.8077609879676,49.4490467859523));
#30406=CARTESIAN_POINT('Ctrl Pts',(40.4847606333963,35.8035406496135,49.384864112291));
#30407=CARTESIAN_POINT('Ctrl Pts',(40.4383523582283,35.7993203742122,49.3206823960135));
#30408=CARTESIAN_POINT('Ctrl Pts',(40.3951743226679,35.7951000988109,49.2541660779658));
#30409=CARTESIAN_POINT('Ctrl Pts',(40.3554565496667,35.7908798234096,49.185678084726));
#30410=CARTESIAN_POINT('Ctrl Pts',(40.3156990496398,35.7866553267498,49.1171215875377));
#30411=CARTESIAN_POINT('Ctrl Pts',(40.2794089621146,35.78243083009,49.0465898825571));
#30412=CARTESIAN_POINT('Ctrl Pts',(40.2467708989212,35.7782063334301,48.974471589718));
#30413=CARTESIAN_POINT('Ctrl Pts',(40.2141171662791,35.7739798086005,48.902318673075));
#30414=CARTESIAN_POINT('Ctrl Pts',(40.1851191228135,35.7697532837708,48.828578088533));
#30415=CARTESIAN_POINT('Ctrl Pts',(40.1599126595402,35.7655267589412,48.753657182021));
#30416=CARTESIAN_POINT('Ctrl Pts',(40.1346601196971,35.7612925081659,48.6785993226037));
#30417=CARTESIAN_POINT('Ctrl Pts',(40.1132131370043,35.7570582573905,48.6023572828514));
#30418=CARTESIAN_POINT('Ctrl Pts',(40.0956572222283,35.7528240066152,48.5253520756895));
#30419=CARTESIAN_POINT('Ctrl Pts',(40.0789135024857,35.7487856463698,48.4519093856397));
#30420=CARTESIAN_POINT('Ctrl Pts',(40.0657088114729,35.7447472861245,48.3777729380046));
#30421=CARTESIAN_POINT('Ctrl Pts',(40.0560732958414,35.7407089258792,48.3033117973838));
#30422=CARTESIAN_POINT('Ctrl Pts',(40.0431435172632,35.7352899004955,48.2033933189411));
#30423=CARTESIAN_POINT('Ctrl Pts',(40.0366008742664,35.7298708751119,48.1026308155814));
#30424=CARTESIAN_POINT('Ctrl Pts',(40.0365305727064,35.7244518497283,48.0016453414631));
#30425=CARTESIAN_POINT('',(40.0365302293311,34.930701849776,48.0010411697219));
#30426=CARTESIAN_POINT('Ctrl Pts',(40.0365305727061,35.7244518497007,48.0016453409487));
#30427=CARTESIAN_POINT('Ctrl Pts',(40.0364764503775,35.7202799598572,47.923900683194));
#30428=CARTESIAN_POINT('Ctrl Pts',(40.0402625742032,35.7161080700138,47.8460064445692));
#30429=CARTESIAN_POINT('Ctrl Pts',(40.0479067550704,35.7119361801703,47.7683800352804));
#30430=CARTESIAN_POINT('Ctrl Pts',(40.0555407043263,35.7077698743334,47.6908575276738));
#30431=CARTESIAN_POINT('Ctrl Pts',(40.0670224088016,35.7036035684964,47.613602615599));
#30432=CARTESIAN_POINT('Ctrl Pts',(40.0823176524898,35.6994372626595,47.537032423447));
#30433=CARTESIAN_POINT('Ctrl Pts',(40.0976016605286,35.6952740173263,47.4605184785728));
#30434=CARTESIAN_POINT('Ctrl Pts',(40.116693558554,35.6911107719931,47.3846887289259));
#30435=CARTESIAN_POINT('Ctrl Pts',(40.1395075048344,35.6869475266599,47.3099535376514));
#30436=CARTESIAN_POINT('Ctrl Pts',(40.1623122877722,35.6827859535163,47.2352483641628));
#30437=CARTESIAN_POINT('Ctrl Pts',(40.1888360119416,35.6786243803726,47.161637339074));
#30438=CARTESIAN_POINT('Ctrl Pts',(40.2189425039841,35.674462807229,47.0895173587745));
#30439=CARTESIAN_POINT('Ctrl Pts',(40.2490469258089,35.6703015202483,47.0174023376734));
#30440=CARTESIAN_POINT('Ctrl Pts',(40.2827334384652,35.6661402332677,46.9467786036397));
#30441=CARTESIAN_POINT('Ctrl Pts',(40.3198177222954,35.661978946287,46.8780231141313));
#30442=CARTESIAN_POINT('Ctrl Pts',(40.3569366995747,35.6578137662987,46.8092033018202));
#30443=CARTESIAN_POINT('Ctrl Pts',(40.3974595657716,35.6536485863105,46.7422556511874));
#30444=CARTESIAN_POINT('Ctrl Pts',(40.4411564144341,35.6494834063222,46.6775317591006));
#30445=CARTESIAN_POINT('Ctrl Pts',(40.4848737671885,35.6453162718857,46.6127774962969));
#30446=CARTESIAN_POINT('Ctrl Pts',(40.5317677753964,35.6411491374491,46.5502494556462));
#30447=CARTESIAN_POINT('Ctrl Pts',(40.58156725145,35.6369820030125,46.4902673150849));
#30448=CARTESIAN_POINT('Ctrl Pts',(40.6314538750544,35.6328075762189,46.4301802076233));
#30449=CARTESIAN_POINT('Ctrl Pts',(40.684255791651,35.6286331494253,46.3726482531046));
#30450=CARTESIAN_POINT('Ctrl Pts',(40.7396642417081,35.6244587226317,46.3179549320434));
#30451=CARTESIAN_POINT('Ctrl Pts',(40.7838003742899,35.6211335429122,46.2743884423254));
#30452=CARTESIAN_POINT('Ctrl Pts',(40.8295895906978,35.6178083631928,46.2326223958576));
#30453=CARTESIAN_POINT('Ctrl Pts',(40.8768618671674,35.6144831834733,46.1927809570473));
#30454=CARTESIAN_POINT('Ctrl Pts',(40.9370756770865,35.610247683207,46.1420322941396));
#30455=CARTESIAN_POINT('Ctrl Pts',(40.9999430179682,35.6060121829408,46.0941998150729));
#30456=CARTESIAN_POINT('Ctrl Pts',(41.0651497065104,35.6017766826745,46.0495730890724));
#30457=CARTESIAN_POINT('Ctrl Pts',(41.1302618660514,35.5975473225392,46.0050110576596));
#30458=CARTESIAN_POINT('Ctrl Pts',(41.1977062546563,35.5933179624039,45.9636458133875));
#30459=CARTESIAN_POINT('Ctrl Pts',(41.2671350908877,35.5890886022687,45.9257272265678));
#30460=CARTESIAN_POINT('Ctrl Pts',(41.3364828486331,35.5848641811492,45.8878529207959));
#30461=CARTESIAN_POINT('Ctrl Pts',(41.4078100390722,35.5806397600296,45.8534174978916));
#30462=CARTESIAN_POINT('Ctrl Pts',(41.4807406163786,35.5764153389101,45.8226271273564));
#30463=CARTESIAN_POINT('Ctrl Pts',(41.5536245559595,35.5721936192281,45.7918564466812));
#30464=CARTESIAN_POINT('Ctrl Pts',(41.6281094161086,35.567971899546,45.7647263740122));
#30465=CARTESIAN_POINT('Ctrl Pts',(41.7037964030363,35.563750179864,45.7413962294207));
#30466=CARTESIAN_POINT('Ctrl Pts',(41.779458625519,35.5595298415098,45.7180737183487));
#30467=CARTESIAN_POINT('Ctrl Pts',(41.8563217455693,35.5553095031556,45.6985488046853));
#30468=CARTESIAN_POINT('Ctrl Pts',(41.9339703460991,35.5510891648014,45.6829314203967));
#30469=CARTESIAN_POINT('Ctrl Pts',(42.01161778838,35.5468688894001,45.6673142690655));
#30470=CARTESIAN_POINT('Ctrl Pts',(42.0900502274505,35.5426486139988,45.6556046224865));
#30471=CARTESIAN_POINT('Ctrl Pts',(42.168842027597,35.5384283385975,45.6478613066627));
#30472=CARTESIAN_POINT('Ctrl Pts',(42.247712637899,35.5342038419376,45.6401102457192));
#30473=CARTESIAN_POINT('Ctrl Pts',(42.3269428590963,35.5299793452778,45.6363334866369));
#30474=CARTESIAN_POINT('Ctrl Pts',(42.4061025050981,35.5257548486179,45.6365378783802));
#30475=CARTESIAN_POINT('Ctrl Pts',(42.4853001554389,35.5215283237882,45.6367423682515));
#30476=CARTESIAN_POINT('Ctrl Pts',(42.5644266937462,35.5173017989586,45.6409317917222));
#30477=CARTESIAN_POINT('Ctrl Pts',(42.6430550960828,35.5130752741289,45.6490608980307));
#30478=CARTESIAN_POINT('Ctrl Pts',(42.721827228503,35.5088410233535,45.6572048640731));
#30479=CARTESIAN_POINT('Ctrl Pts',(42.8000989403447,35.5046067725782,45.669302831574));
#30480=CARTESIAN_POINT('Ctrl Pts',(42.8774516614981,35.5003725218028,45.6852580377432));
#30481=CARTESIAN_POINT('Ctrl Pts',(42.9512257883815,35.4963341615577,45.7004751029843));
#30482=CARTESIAN_POINT('Ctrl Pts',(43.0241637384678,35.4922958013126,45.7192002777303));
#30483=CARTESIAN_POINT('Ctrl Pts',(43.0959171705692,35.4882574410675,45.7413079597681));
#30484=CARTESIAN_POINT('Ctrl Pts',(43.1711733791099,35.4840219408013,45.7644948691752));
#30485=CARTESIAN_POINT('Ctrl Pts',(43.2454125328606,35.479786440535,45.7914911032359));
#30486=CARTESIAN_POINT('Ctrl Pts',(43.3182211254831,35.4755509402688,45.8221890794616));
#30487=CARTESIAN_POINT('Ctrl Pts',(43.3909241687566,35.4713215801336,45.8528425533656));
#30488=CARTESIAN_POINT('Ctrl Pts',(43.4622003403966,35.4670922199983,45.8871869320056));
#30489=CARTESIAN_POINT('Ctrl Pts',(43.5316513456607,35.4628628598631,45.925064899144));
#30490=CARTESIAN_POINT('Ctrl Pts',(43.6010212465498,35.4586384387436,45.96289863267));
#30491=CARTESIAN_POINT('Ctrl Pts',(43.668569806671,35.4544140176242,46.0042575310109));
#30492=CARTESIAN_POINT('Ctrl Pts',(43.7339201940952,35.4501895965047,46.0489368650182));
#30493=CARTESIAN_POINT('Ctrl Pts',(43.7992287911819,35.4459678768227,46.0935876274359));
#30494=CARTESIAN_POINT('Ctrl Pts',(43.8623416191588,35.4417461571407,46.1415543469306));
#30495=CARTESIAN_POINT('Ctrl Pts',(43.9229089413283,35.4375244374587,46.1925878175352));
#30496=CARTESIAN_POINT('Ctrl Pts',(43.9834564461398,35.4333040991045,46.2436045902155));
#30497=CARTESIAN_POINT('Ctrl Pts',(44.0414597403089,35.4290837607504,46.2976858193327));
#30498=CARTESIAN_POINT('Ctrl Pts',(44.0966016308579,35.4248634223963,46.3545415997144));
#30499=CARTESIAN_POINT('Ctrl Pts',(44.1517426988804,35.420643146995,46.4113965320044));
#30500=CARTESIAN_POINT('Ctrl Pts',(44.2040221223187,35.4164228715937,46.4710255954416));
#30501=CARTESIAN_POINT('Ctrl Pts',(44.2531601615548,35.4122025961925,46.5331026428117));
#30502=CARTESIAN_POINT('Ctrl Pts',(44.3023473502774,35.4079780995326,46.5952417816906));
#30503=CARTESIAN_POINT('Ctrl Pts',(44.3483865860238,35.4037536028728,46.6598334269079));
#30504=CARTESIAN_POINT('Ctrl Pts',(44.3910393816092,35.399529106213,46.7265194851191));
#30505=CARTESIAN_POINT('Ctrl Pts',(44.4337126546901,35.3953025813834,46.7932375591324));
#30506=CARTESIAN_POINT('Ctrl Pts',(44.4729960157661,35.3910760565538,46.8620516410921));
#30507=CARTESIAN_POINT('Ctrl Pts',(44.508696505682,35.3868495317241,46.9325781116051));
#30508=CARTESIAN_POINT('Ctrl Pts',(44.5444622548967,35.3826152809488,47.0032335021419));
#30509=CARTESIAN_POINT('Ctrl Pts',(44.5766318546358,35.3783810301735,47.0756071060647));
#30510=CARTESIAN_POINT('Ctrl Pts',(44.6050602422551,35.3741467793982,47.1492945463172));
#30511=CARTESIAN_POINT('Ctrl Pts',(44.6321734380714,35.3701084191527,47.2195729603982));
#30512=CARTESIAN_POINT('Ctrl Pts',(44.6558838508024,35.3660700589071,47.2910459837102));
#30513=CARTESIAN_POINT('Ctrl Pts',(44.6761086658167,35.3620316986616,47.3633527018089));
#30514=CARTESIAN_POINT('Ctrl Pts',(44.6973207925635,35.3577961983954,47.4391892060176));
#30515=CARTESIAN_POINT('Ctrl Pts',(44.7147789523769,35.3535606981292,47.5162311508201));
#30516=CARTESIAN_POINT('Ctrl Pts',(44.7283499217397,35.3493251978629,47.5940725645698));
#30517=CARTESIAN_POINT('Ctrl Pts',(44.7419012175044,35.3450958377277,47.6718011329772));
#30518=CARTESIAN_POINT('Ctrl Pts',(44.7515764333856,35.3408664775925,47.7503264103434));
#30519=CARTESIAN_POINT('Ctrl Pts',(44.7572924026886,35.3366371174573,47.8292283128655));
#30520=CARTESIAN_POINT('Ctrl Pts',(44.7630016969245,35.3324126963378,47.9080380743241));
#30521=CARTESIAN_POINT('Ctrl Pts',(44.7647608987576,35.3281882752184,47.9872231212413));
#30522=CARTESIAN_POINT('Ctrl Pts',(44.7625383282817,35.3239638540989,48.0663557706616));
#30523=CARTESIAN_POINT('Ctrl Pts',(44.7603171790975,35.3197421344169,48.1454378162483));
#30524=CARTESIAN_POINT('Ctrl Pts',(44.7541193245437,35.3155204147349,48.2244670629436));
#30525=CARTESIAN_POINT('Ctrl Pts',(44.743965149256,35.3112986950529,48.3030145540616));
#30526=CARTESIAN_POINT('Ctrl Pts',(44.7338142963693,35.3070783566988,48.3815363447903));
#30527=CARTESIAN_POINT('Ctrl Pts',(44.7197097533064,35.3028580183447,48.4595762278133));
#30528=CARTESIAN_POINT('Ctrl Pts',(44.7017237397524,35.2986376799906,48.536710598703));
#30529=CARTESIAN_POINT('Ctrl Pts',(44.6837379944876,35.2944174045893,48.6138438190142));
#30530=CARTESIAN_POINT('Ctrl Pts',(44.6618710017028,35.2901971291881,48.6900710972545));
#30531=CARTESIAN_POINT('Ctrl Pts',(44.6362457236063,35.2859768537868,48.7649807216868));
#30532=CARTESIAN_POINT('Ctrl Pts',(44.610594814262,35.281752357127,48.8399652731946));
#30533=CARTESIAN_POINT('Ctrl Pts',(44.5811782624854,35.2775278604672,48.913629092954));
#30534=CARTESIAN_POINT('Ctrl Pts',(44.5481682152923,35.2733033638074,48.9855778810971));
#30535=CARTESIAN_POINT('Ctrl Pts',(44.5151423200618,35.2690768389778,49.0575612116653));
#30536=CARTESIAN_POINT('Ctrl Pts',(44.478519709777,35.2648503141482,49.1278274535547));
#30537=CARTESIAN_POINT('Ctrl Pts',(44.4385186298535,35.2606237893186,49.1960067878737));
#30538=CARTESIAN_POINT('Ctrl Pts',(44.398444429297,35.2563895385433,49.2643107517302));
#30539=CARTESIAN_POINT('Ctrl Pts',(44.3549796767984,35.252155287768,49.3305197917651));
#30540=CARTESIAN_POINT('Ctrl Pts',(44.3083859871555,35.2479210369927,49.3942931416773));
#30541=CARTESIAN_POINT('Ctrl Pts',(44.2639478766286,35.2438826767471,49.4551161242269));
#30542=CARTESIAN_POINT('Ctrl Pts',(44.216664189521,35.2398443165014,49.5137235441245));
#30543=CARTESIAN_POINT('Ctrl Pts',(44.1667936629992,35.2358059562558,49.5698505002981));
#30544=CARTESIAN_POINT('Ctrl Pts',(44.1144886145335,35.2315704559894,49.6287173975946));
#30545=CARTESIAN_POINT('Ctrl Pts',(44.0591388925338,35.2273349557229,49.6850792364415));
#30546=CARTESIAN_POINT('Ctrl Pts',(44.0010138577604,35.2230994554565,49.7386043449156));
#30547=CARTESIAN_POINT('Ctrl Pts',(43.9429730858376,35.2188700953211,49.7920518589721));
#30548=CARTESIAN_POINT('Ctrl Pts',(43.8821653330907,35.2146407351856,49.8426704938245));
#30549=CARTESIAN_POINT('Ctrl Pts',(43.8188989093145,35.2104113750502,49.8901630421861));
#30550=CARTESIAN_POINT('Ctrl Pts',(43.7557063676045,35.2061869539305,49.9376001290976));
#30551=CARTESIAN_POINT('Ctrl Pts',(43.6900612339192,35.2019625328108,49.9819181036721));
#30552=CARTESIAN_POINT('Ctrl Pts',(43.6223060630681,35.1977381116912,50.0228589493801));
#30553=CARTESIAN_POINT('Ctrl Pts',(43.5545942203681,35.193516392009,50.063773614191));
#30554=CARTESIAN_POINT('Ctrl Pts',(43.4847754192573,35.1892946723268,50.1013151944229));
#30555=CARTESIAN_POINT('Ctrl Pts',(43.4132214522624,35.1850729526445,50.13526877221));
#30556=CARTESIAN_POINT('Ctrl Pts',(43.3416908974067,35.1808526142902,50.1692112405378));
#30557=CARTESIAN_POINT('Ctrl Pts',(43.2684267277205,35.1766322759359,50.1995678364937));
#30558=CARTESIAN_POINT('Ctrl Pts',(43.1938242766516,35.1724119375815,50.2261701324694));
#30559=CARTESIAN_POINT('Ctrl Pts',(43.1192229383935,35.1681916621801,50.2527720316307));
#30560=CARTESIAN_POINT('Ctrl Pts',(43.0432838009675,35.1639713867786,50.2756195857444));
#30561=CARTESIAN_POINT('Ctrl Pts',(42.9664196470083,35.1597511113771,50.2945934769329));
#30562=CARTESIAN_POINT('Ctrl Pts',(42.8894786109889,35.1555266147171,50.3135863464327));
#30563=CARTESIAN_POINT('Ctrl Pts',(42.8116111669309,35.1513021180571,50.3286977003229));
#30564=CARTESIAN_POINT('Ctrl Pts',(42.73324206216,35.1470776213971,50.3398590062026));
#30565=CARTESIAN_POINT('Ctrl Pts',(42.6548353325869,35.1428510965673,50.351025670596));
#30566=CARTESIAN_POINT('Ctrl Pts',(42.5759269305515,35.1386245717375,50.3582384663198));
#30567=CARTESIAN_POINT('Ctrl Pts',(42.4969459530339,35.1343980469076,50.3614808750211));
#30568=CARTESIAN_POINT('Ctrl Pts',(42.4178206009374,35.1301637961321,50.3647292107367));
#30569=CARTESIAN_POINT('Ctrl Pts',(42.3386228788274,35.1259295453566,50.3639926611499));
#30570=CARTESIAN_POINT('Ctrl Pts',(42.2597809121065,35.1216952945811,50.3593068999794));
#30571=CARTESIAN_POINT('Ctrl Pts',(42.184586437139,35.1176569343374,50.354837917714));
#30572=CARTESIAN_POINT('Ctrl Pts',(42.1097158798324,35.1136185740936,50.3467771251438));
#30573=CARTESIAN_POINT('Ctrl Pts',(42.0355320040277,35.1095802138499,50.3351988182619));
#30574=CARTESIAN_POINT('Ctrl Pts',(41.9577267051587,35.1053447135838,50.3230552949212));
#30575=CARTESIAN_POINT('Ctrl Pts',(41.8803810882845,35.1011092133178,50.3069959003845));
#30576=CARTESIAN_POINT('Ctrl Pts',(41.8039198206799,35.0968737130518,50.2870677429236));
#30577=CARTESIAN_POINT('Ctrl Pts',(41.7275693976435,35.0926443529168,50.2671684749656));
#30578=CARTESIAN_POINT('Ctrl Pts',(41.6521012283375,35.0884149927817,50.2434116989024));
#30579=CARTESIAN_POINT('Ctrl Pts',(41.5779320654063,35.0841856326467,50.2158959253117));
#30580=CARTESIAN_POINT('Ctrl Pts',(41.5038495166799,35.0799612115274,50.1884122844397));
#30581=CARTESIAN_POINT('Ctrl Pts',(41.4310633975859,35.0757367904082,50.1571785316532));
#30582=CARTESIAN_POINT('Ctrl Pts',(41.3599760265035,35.0715123692889,50.1223431804147));
#30583=CARTESIAN_POINT('Ctrl Pts',(41.2889341144513,35.0672906496071,50.0875301057248));
#30584=CARTESIAN_POINT('Ctrl Pts',(41.2195892146319,35.0630689299253,50.0491202098274));
#30585=CARTESIAN_POINT('Ctrl Pts',(41.1523232155949,35.0588472102435,50.007309911936));
#30586=CARTESIAN_POINT('Ctrl Pts',(41.0850792256931,35.0546268718895,49.9655132941879));
#30587=CARTESIAN_POINT('Ctrl Pts',(41.0199131842295,35.0504065335356,49.9203187312767));
#30588=CARTESIAN_POINT('Ctrl Pts',(40.9571806155803,35.0461861951817,49.8719675918249));
#30589=CARTESIAN_POINT('Ctrl Pts',(40.8944489826845,35.0419659197806,49.8236171736053));
#30590=CARTESIAN_POINT('Ctrl Pts',(40.8341511213803,35.0377456443796,49.7721105600202));
#30591=CARTESIAN_POINT('Ctrl Pts',(40.7766106932438,35.0335253689785,49.7177303628945));
#30592=CARTESIAN_POINT('Ctrl Pts',(40.7190127112742,35.0293008723189,49.6632957729029));
#30593=CARTESIAN_POINT('Ctrl Pts',(40.6641780140076,35.0250763756593,49.60598218084));
#30594=CARTESIAN_POINT('Ctrl Pts',(40.6123940238051,35.0208518789996,49.5461097356825));
#30595=CARTESIAN_POINT('Ctrl Pts',(40.5605851722442,35.0166253541702,49.4862085459205));
#30596=CARTESIAN_POINT('Ctrl Pts',(40.5118302346726,35.0123988293408,49.4237464262382));
#30597=CARTESIAN_POINT('Ctrl Pts',(40.4663752413027,35.0081723045113,49.3590753229505));
#30598=CARTESIAN_POINT('Ctrl Pts',(40.4208371577289,35.0039380537362,49.294286003054));
#30599=CARTESIAN_POINT('Ctrl Pts',(40.378611322974,34.9997038029611,49.2272800289112));
#30600=CARTESIAN_POINT('Ctrl Pts',(40.3398993466385,34.995469552186,49.1584367651796));
#30601=CARTESIAN_POINT('Ctrl Pts',(40.3029783151194,34.9914311919386,49.0927784198632));
#30602=CARTESIAN_POINT('Ctrl Pts',(40.2692533335794,34.9873928316913,49.025449359582));
#30603=CARTESIAN_POINT('Ctrl Pts',(40.238858169154,34.983354471444,48.9567948724086));
#30604=CARTESIAN_POINT('Ctrl Pts',(40.203843215612,34.9787023170925,48.8777055263148));
#30605=CARTESIAN_POINT('Ctrl Pts',(40.173132350658,34.9740501627411,48.7965988730332));
#30606=CARTESIAN_POINT('Ctrl Pts',(40.1469392857684,34.9693980083896,48.7139382738627));
#30607=CARTESIAN_POINT('Ctrl Pts',(40.1208200312477,34.9647589635093,48.6315106069341));
#30608=CARTESIAN_POINT('Ctrl Pts',(40.099193315503,34.960119918629,48.5475380103431));
#30609=CARTESIAN_POINT('Ctrl Pts',(40.0822249547242,34.9554808737487,48.4625032760932));
#30610=CARTESIAN_POINT('Ctrl Pts',(40.0653374664262,34.9508639389044,48.3778738237676));
#30611=CARTESIAN_POINT('Ctrl Pts',(40.053064163275,34.9462470040601,48.2921926237583));
#30612=CARTESIAN_POINT('Ctrl Pts',(40.0455206172929,34.9416300692159,48.2059545515576));
#30613=CARTESIAN_POINT('Ctrl Pts',(40.0395687950972,34.9379873294026,48.1379131193904));
#30614=CARTESIAN_POINT('Ctrl Pts',(40.0365603984321,34.9343445895893,48.0695254491627));
#30615=CARTESIAN_POINT('Ctrl Pts',(40.0365302293311,34.930701849776,48.0010411697218));
#30616=CARTESIAN_POINT('',(40.0365309009773,34.1369518496884,47.9979362983109));
#30617=CARTESIAN_POINT('Ctrl Pts',(40.0365302293307,34.9307018497283,48.0010411688257));
#30618=CARTESIAN_POINT('Ctrl Pts',(40.0364946440264,34.9264051318271,47.9202619629236));
#30619=CARTESIAN_POINT('Ctrl Pts',(40.0406047391561,34.9221084139259,47.8394991116311));
#30620=CARTESIAN_POINT('Ctrl Pts',(40.048829165374,34.9178116960247,47.7591968702359));
#30621=CARTESIAN_POINT('Ctrl Pts',(40.057057704256,34.913512829529,47.6788544733172));
#30622=CARTESIAN_POINT('Ctrl Pts',(40.0694046197622,34.9092139630333,47.5989735871373));
#30623=CARTESIAN_POINT('Ctrl Pts',(40.0857869235253,34.9049150965376,47.5199913776052));
#30624=CARTESIAN_POINT('Ctrl Pts',(40.1021952311961,34.9006094063784,47.4408837982761));
#30625=CARTESIAN_POINT('Ctrl Pts',(40.1226516265555,34.8963037162192,47.362678180888));
#30626=CARTESIAN_POINT('Ctrl Pts',(40.1470224109709,34.89199802606,47.2857994509714));
#30627=CARTESIAN_POINT('Ctrl Pts',(40.1714137197927,34.8876887097666,47.2088559758968));
#30628=CARTESIAN_POINT('Ctrl Pts',(40.1997258277564,34.8833793934732,47.1332420309795));
#30629=CARTESIAN_POINT('Ctrl Pts',(40.2317766603203,34.8790700771798,47.0593629870306));
#30630=CARTESIAN_POINT('Ctrl Pts',(40.2638943265441,34.8747517749302,46.9853298875857));
#30631=CARTESIAN_POINT('Ctrl Pts',(40.2997660943098,34.8704334726805,46.9130393157213));
#30632=CARTESIAN_POINT('Ctrl Pts',(40.3391636555107,34.8661151704309,46.8428725212268));
#30633=CARTESIAN_POINT('Ctrl Pts',(40.3664925959349,34.8631196899667,46.794199860076));
#30634=CARTESIAN_POINT('Ctrl Pts',(40.3955171271908,34.8601242095025,46.7465485590536));
#30635=CARTESIAN_POINT('Ctrl Pts',(40.4261493209387,34.8571287290383,46.7000369475754));
#30636=CARTESIAN_POINT('Ctrl Pts',(40.4694621271366,34.8528932287707,46.6342712231063));
#30637=CARTESIAN_POINT('Ctrl Pts',(40.5161476800916,34.8486577285031,46.5705475402857));
#30638=CARTESIAN_POINT('Ctrl Pts',(40.5659870212995,34.8444222282355,46.5092328032661));
#30639=CARTESIAN_POINT('Ctrl Pts',(40.6157541112821,34.840192868099,46.4480069531532));
#30640=CARTESIAN_POINT('Ctrl Pts',(40.6686656168081,34.8359635079624,46.3891834750637));
#30641=CARTESIAN_POINT('Ctrl Pts',(40.7244590862551,34.8317341478258,46.3331007567142));
#30642=CARTESIAN_POINT('Ctrl Pts',(40.7801874004975,34.827509726705,46.277083531352));
#30643=CARTESIAN_POINT('Ctrl Pts',(40.8387906614109,34.8232853055842,46.2238010364743));
#30644=CARTESIAN_POINT('Ctrl Pts',(40.8999669011061,34.8190608844634,46.1735577909162));
#30645=CARTESIAN_POINT('Ctrl Pts',(40.9611040197523,34.81483916478,46.1233466749641));
#30646=CARTESIAN_POINT('Ctrl Pts',(41.0248104897444,34.8106174450967,46.0761712478957));
#30647=CARTESIAN_POINT('Ctrl Pts',(41.090749221371,34.8063957254133,46.0322975734224));
#30648=CARTESIAN_POINT('Ctrl Pts',(41.1566663781384,34.8021753870578,45.98843825422));
#30649=CARTESIAN_POINT('Ctrl Pts',(41.2248139557738,34.7979550487023,45.9478788022596));
#30650=CARTESIAN_POINT('Ctrl Pts',(41.2948248936639,34.7937347103469,45.9108426518726));
#30651=CARTESIAN_POINT('Ctrl Pts',(41.3648347872325,34.7895144349443,45.873807053937));
#30652=CARTESIAN_POINT('Ctrl Pts',(41.436707570305,34.7852941595416,45.8402948713989));
#30653=CARTESIAN_POINT('Ctrl Pts',(41.5100518639737,34.781073884139,45.810483442382));
#30654=CARTESIAN_POINT('Ctrl Pts',(41.5834695190221,34.7768493874779,45.7806421949914));
#30655=CARTESIAN_POINT('Ctrl Pts',(41.658361189034,34.7726248908168,45.7545092727193));
#30656=CARTESIAN_POINT('Ctrl Pts',(41.7343163639405,34.7684003941556,45.7322134717786));
#30657=CARTESIAN_POINT('Ctrl Pts',(41.8103080047276,34.7641738693247,45.7099069666822));
#30658=CARTESIAN_POINT('Ctrl Pts',(41.887363710503,34.7599473444937,45.6914413623176));
#30659=CARTESIAN_POINT('Ctrl Pts',(41.9650611998378,34.7557208196628,45.6768946039808));
#30660=CARTESIAN_POINT('Ctrl Pts',(42.0429007175777,34.7514865688862,45.6623212546575));
#30661=CARTESIAN_POINT('Ctrl Pts',(42.1213838968034,34.7472523181096,45.651681128974));
#30662=CARTESIAN_POINT('Ctrl Pts',(42.2000819252879,34.743018067333,45.645000381252));
#30663=CARTESIAN_POINT('Ctrl Pts',(42.275139120872,34.7389797070994,45.6386287071697));
#30664=CARTESIAN_POINT('Ctrl Pts',(42.3503913677707,34.7349413468658,45.6358581410795));
#30665=CARTESIAN_POINT('Ctrl Pts',(42.4254689940191,34.7309029866323,45.636667232224));
#30666=CARTESIAN_POINT('Ctrl Pts',(42.5042116735762,34.7266674863681,45.6375158206505));
#30667=CARTESIAN_POINT('Ctrl Pts',(42.5830615660862,34.7224319861039,45.6423057109072));
#30668=CARTESIAN_POINT('Ctrl Pts',(42.6615916401724,34.7181964858398,45.651051244771));
#30669=CARTESIAN_POINT('Ctrl Pts',(42.7400078705775,34.7139671257066,45.6597841003866));
#30670=CARTESIAN_POINT('Ctrl Pts',(42.8181047407343,34.7097377655734,45.6724611605396));
#30671=CARTESIAN_POINT('Ctrl Pts',(42.8954556729822,34.7055084054402,45.6890447609247));
#30672=CARTESIAN_POINT('Ctrl Pts',(42.9727162753786,34.7012839843228,45.7056089951028));
#30673=CARTESIAN_POINT('Ctrl Pts',(43.0492322143667,34.6970595632054,45.726070606033));
#30674=CARTESIAN_POINT('Ctrl Pts',(43.1245840190017,34.692835142088,45.7503403723436));
#30675=CARTESIAN_POINT('Ctrl Pts',(43.1998876375823,34.688613422408,45.7745946185974));
#30676=CARTESIAN_POINT('Ctrl Pts',(43.2740281538242,34.684391702728,45.8026520432908));
#30677=CARTESIAN_POINT('Ctrl Pts',(43.3465994380146,34.680169983048,45.8343730827194));
#30678=CARTESIAN_POINT('Ctrl Pts',(43.4191469772041,34.6759496446959,45.8660837431651));
#30679=CARTESIAN_POINT('Ctrl Pts',(43.4901258741377,34.6717293063438,45.9014554502498));
#30680=CARTESIAN_POINT('Ctrl Pts',(43.5591496376044,34.6675089679917,45.9403003717674));
#30681=CARTESIAN_POINT('Ctrl Pts',(43.6281723714752,34.6632886925924,45.9791447138531));
#30682=CARTESIAN_POINT('Ctrl Pts',(43.6952396214777,34.6590684171932,46.0214619360348));
#30683=CARTESIAN_POINT('Ctrl Pts',(43.7599905086148,34.6548481417939,46.0670188160829));
#30684=CARTESIAN_POINT('Ctrl Pts',(43.8248061617241,34.650623645136,46.1126212636244));
#30685=CARTESIAN_POINT('Ctrl Pts',(43.8873004388834,34.6463991484782,46.161469571445));
#30686=CARTESIAN_POINT('Ctrl Pts',(43.94714293641,34.6421746518203,46.2132881667105));
#30687=CARTESIAN_POINT('Ctrl Pts',(44.0070141641634,34.6379481269926,46.2651316399483));
#30688=CARTESIAN_POINT('Ctrl Pts',(44.064230736708,34.6337216021649,46.3199479163091));
#30689=CARTESIAN_POINT('Ctrl Pts',(44.1184986492037,34.6294950773373,46.3774240130012));
#30690=CARTESIAN_POINT('Ctrl Pts',(44.1728657616248,34.6252608265638,46.4350051740719));
#30691=CARTESIAN_POINT('Ctrl Pts',(44.224273137964,34.6210265757904,46.4952555130286));
#30692=CARTESIAN_POINT('Ctrl Pts',(44.2724667979375,34.616792325017,46.5578285360188));
#30693=CARTESIAN_POINT('Ctrl Pts',(44.3184308590675,34.6127539647535,46.6175067230539));
#30694=CARTESIAN_POINT('Ctrl Pts',(44.361471808364,34.60871560449,46.6792971225263));
#30695=CARTESIAN_POINT('Ctrl Pts',(44.4014076971255,34.6046772442265,46.7428772252533));
#30696=CARTESIAN_POINT('Ctrl Pts',(44.4432931299291,34.600441743961,46.8095611079214));
#30697=CARTESIAN_POINT('Ctrl Pts',(44.4819218185688,34.5962062436954,46.8784673704397));
#30698=CARTESIAN_POINT('Ctrl Pts',(44.5170506808672,34.5919707434299,46.9492446262141));
#30699=CARTESIAN_POINT('Ctrl Pts',(44.5521286174653,34.5877413832954,47.0199192774328));
#30700=CARTESIAN_POINT('Ctrl Pts',(44.5837165961697,34.5835120231609,47.0924591188066));
#30701=CARTESIAN_POINT('Ctrl Pts',(44.6116155188343,34.5792826630264,47.1664850104819));
#30702=CARTESIAN_POINT('Ctrl Pts',(44.6394818613413,34.5750582419077,47.2404244552629));
#30703=CARTESIAN_POINT('Ctrl Pts',(44.6636675440464,34.570833820789,47.3158460648713));
#30704=CARTESIAN_POINT('Ctrl Pts',(44.6840206744163,34.5666093996702,47.3923487844667));
#30705=CARTESIAN_POINT('Ctrl Pts',(44.7043607893438,34.562387679989,47.4688025820186));
#30706=CARTESIAN_POINT('Ctrl Pts',(44.720873095994,34.5581659603078,47.546335665028));
#30707=CARTESIAN_POINT('Ctrl Pts',(44.7334552586409,34.5539442406265,47.6245309642312));
#30708=CARTESIAN_POINT('Ctrl Pts',(44.7460333044602,34.5497239022732,47.7027006782804));
#30709=CARTESIAN_POINT('Ctrl Pts',(44.7546836851917,34.5455035639199,47.78153171524));
#30710=CARTESIAN_POINT('Ctrl Pts',(44.7593552845364,34.5412832255665,47.8605974095289));
#30711=CARTESIAN_POINT('Ctrl Pts',(44.764026814197,34.5370629501661,47.9396619244302));
#30712=CARTESIAN_POINT('Ctrl Pts',(44.7647196540934,34.5328426747656,48.0189606210902));
#30713=CARTESIAN_POINT('Ctrl Pts',(44.7614347182004,34.5286223993652,48.0980638189019));
#30714=CARTESIAN_POINT('Ctrl Pts',(44.7581464966063,34.5243979027062,48.1772461383392));
#30715=CARTESIAN_POINT('Ctrl Pts',(44.7508725707835,34.5201734060472,48.2562320982361));
#30716=CARTESIAN_POINT('Ctrl Pts',(44.7396659596394,34.5159489093882,48.3345947372639));
#30717=CARTESIAN_POINT('Ctrl Pts',(44.7284539682306,34.5117223845594,48.4129949979896));
#30718=CARTESIAN_POINT('Ctrl Pts',(44.7133056200825,34.5074958597306,48.4907708803665));
#30719=CARTESIAN_POINT('Ctrl Pts',(44.6943250883908,34.5032693349019,48.5675057970456));
#30720=CARTESIAN_POINT('Ctrl Pts',(44.6753098609236,34.4990350841274,48.6443809825796));
#30721=CARTESIAN_POINT('Ctrl Pts',(44.6524485879072,34.4948008333529,48.7202109495185));
#30722=CARTESIAN_POINT('Ctrl Pts',(44.6258952792242,34.4905665825785,48.7945946430902));
#30723=CARTESIAN_POINT('Ctrl Pts',(44.6005704149039,34.4865282223258,48.8655370996341));
#30724=CARTESIAN_POINT('Ctrl Pts',(44.5718877420354,34.4824898620732,48.9351638260439));
#30725=CARTESIAN_POINT('Ctrl Pts',(44.5400200671921,34.4784515018206,49.0031473236345));
#30726=CARTESIAN_POINT('Ctrl Pts',(44.5065967128721,34.4742160015445,49.0744495613741));
#30727=CARTESIAN_POINT('Ctrl Pts',(44.4695424038322,34.4699805012685,49.1442150744385));
#30728=CARTESIAN_POINT('Ctrl Pts',(44.429021160673,34.4657450009925,49.212049326736));
#30729=CARTESIAN_POINT('Ctrl Pts',(44.3885586604541,34.4615156408474,49.2797852408997));
#30730=CARTESIAN_POINT('Ctrl Pts',(44.3446394454327,34.4572862807023,49.3455950545097));
#30731=CARTESIAN_POINT('Ctrl Pts',(44.2974746724665,34.4530569205573,49.4091062090021));
#30732=CARTESIAN_POINT('Ctrl Pts',(44.2503649781762,34.4488324994279,49.472543195634));
#30733=CARTESIAN_POINT('Ctrl Pts',(44.2000175360269,34.4446080782986,49.5336864826118));
#30734=CARTESIAN_POINT('Ctrl Pts',(44.1466874718296,34.4403836571693,49.5921913567953));
#30735=CARTESIAN_POINT('Ctrl Pts',(44.0933915112003,34.4361619374775,49.6506588182176));
#30736=CARTESIAN_POINT('Ctrl Pts',(44.0371170294983,34.4319402177856,49.7064908696767));
#30737=CARTESIAN_POINT('Ctrl Pts',(43.9781594309252,34.4277184980938,49.7593758130319));
#30738=CARTESIAN_POINT('Ctrl Pts',(43.9192211230161,34.4234981597298,49.812243452669));
#30739=CARTESIAN_POINT('Ctrl Pts',(43.8576017905845,34.4192778213659,49.8621655857811));
#30740=CARTESIAN_POINT('Ctrl Pts',(43.7936326178781,34.4150574830019,49.9088683996772));
#30741=CARTESIAN_POINT('Ctrl Pts',(43.729664399371,34.4108372075909,49.9555705169285));
#30742=CARTESIAN_POINT('Ctrl Pts',(43.6633467901245,34.4066169321798,49.9990531347413));
#30743=CARTESIAN_POINT('Ctrl Pts',(43.5950416580426,34.4023966567687,50.039084568242));
#30744=CARTESIAN_POINT('Ctrl Pts',(43.5266682049184,34.3981721600992,50.0791560425008));
#30745=CARTESIAN_POINT('Ctrl Pts',(43.456303663607,34.3939476634297,50.1157691987805));
#30746=CARTESIAN_POINT('Ctrl Pts',(43.3843358033486,34.3897231667602,50.1487376450247));
#30747=CARTESIAN_POINT('Ctrl Pts',(43.3123333915096,34.385496641921,50.1817219193332));
#30748=CARTESIAN_POINT('Ctrl Pts',(43.2387265638878,34.3812701170817,50.2110578237531));
#30749=CARTESIAN_POINT('Ctrl Pts',(43.1639220389498,34.3770435922425,50.2366076006548));
#30750=CARTESIAN_POINT('Ctrl Pts',(43.0889807738518,34.3728093414577,50.2622040816908));
#30751=CARTESIAN_POINT('Ctrl Pts',(43.0128378890165,34.368575090673,50.2840004760918));
#30752=CARTESIAN_POINT('Ctrl Pts',(42.9359140008011,34.3643408398882,50.3019093432725));
#30753=CARTESIAN_POINT('Ctrl Pts',(42.8625488693661,34.3603024797304,50.3189896862589));
#30754=CARTESIAN_POINT('Ctrl Pts',(42.7884737580912,34.3562641195726,50.3325342193753));
#30755=CARTESIAN_POINT('Ctrl Pts',(42.7140575894208,34.3522257594148,50.3425111038002));
#30756=CARTESIAN_POINT('Ctrl Pts',(42.6360086565505,34.3479902591667,50.3529750284639));
#30757=CARTESIAN_POINT('Ctrl Pts',(42.5572878366582,34.3437547589187,50.3595538633806));
#30758=CARTESIAN_POINT('Ctrl Pts',(42.4783156794139,34.3395192586706,50.3621721138092));
#30759=CARTESIAN_POINT('Ctrl Pts',(42.399458006731,34.3352898985536,50.3647865686058));
#30760=CARTESIAN_POINT('Ctrl Pts',(42.3203501853755,34.3310605384365,50.3634518252778));
#30761=CARTESIAN_POINT('Ctrl Pts',(42.2414197816143,34.3268311783194,50.3581439216547));
#30762=CARTESIAN_POINT('Ctrl Pts',(42.1625815521981,34.322606757218,50.3528422165623));
#30763=CARTESIAN_POINT('Ctrl Pts',(42.0839207945184,34.3183823361165,50.3435766027034));
#30764=CARTESIAN_POINT('Ctrl Pts',(42.0058654428886,34.3141579150151,50.3303751611684));
#30765=CARTESIAN_POINT('Ctrl Pts',(41.9278600061794,34.309936195351,50.3171821617055));
#30766=CARTESIAN_POINT('Ctrl Pts',(41.8504596686479,34.3057144756869,50.3000584081078));
#30767=CARTESIAN_POINT('Ctrl Pts',(41.7740863883335,34.3014927560229,50.2790837175564));
#30768=CARTESIAN_POINT('Ctrl Pts',(41.6977380970143,34.2972724176865,50.2581158898298));
#30769=CARTESIAN_POINT('Ctrl Pts',(41.6224166478823,34.2930520793503,50.2332997513138));
#30770=CARTESIAN_POINT('Ctrl Pts',(41.5485314929506,34.288831741014,50.2047657069183));
#30771=CARTESIAN_POINT('Ctrl Pts',(41.4746474401278,34.2846114656304,50.1762320881513));
#30772=CARTESIAN_POINT('Ctrl Pts',(41.4022000762725,34.2803911902468,50.1439808440776));
#30773=CARTESIAN_POINT('Ctrl Pts',(41.3315800223182,34.2761709148632,50.1081909762141));
#30774=CARTESIAN_POINT('Ctrl Pts',(41.2608893318526,34.2719464182208,50.0723653101422));
#30775=CARTESIAN_POINT('Ctrl Pts',(41.1920300220774,34.2677219215783,50.0329941624658));
#30776=CARTESIAN_POINT('Ctrl Pts',(41.1253686337984,34.2634974249359,49.9903028214809));
#30777=CARTESIAN_POINT('Ctrl Pts',(41.0586752415587,34.2592709001235,49.9475909844933));
#30778=CARTESIAN_POINT('Ctrl Pts',(40.9941822554756,34.2550443753111,49.9015560517779));
#30779=CARTESIAN_POINT('Ctrl Pts',(40.9322255648067,34.2508178504987,49.8524655592731));
#30780=CARTESIAN_POINT('Ctrl Pts',(40.870155619377,34.2465835997401,49.8032853309879));
#30781=CARTESIAN_POINT('Ctrl Pts',(40.8106315873747,34.2423493489816,49.7510386922827));
#30782=CARTESIAN_POINT('Ctrl Pts',(40.7539545586514,34.238115098223,49.6960320887045));
#30783=CARTESIAN_POINT('Ctrl Pts',(40.6998995955178,34.2340767378183,49.6435702713599));
#30784=CARTESIAN_POINT('Ctrl Pts',(40.6484342549836,34.2300383774136,49.5885984976851));
#30785=CARTESIAN_POINT('Ctrl Pts',(40.5997848983345,34.2260000170089,49.5314098173367));
#30786=CARTESIAN_POINT('Ctrl Pts',(40.5491120042058,34.2217936837019,49.4718424120461));
#30787=CARTESIAN_POINT('Ctrl Pts',(40.5012948400351,34.2175873503948,49.4096347864003));
#30788=CARTESIAN_POINT('Ctrl Pts',(40.4566233196973,34.2133810170877,49.3450938700907));
#30789=CARTESIAN_POINT('Ctrl Pts',(40.4120127572409,34.2091804236607,49.2806410250509));
#30790=CARTESIAN_POINT('Ctrl Pts',(40.3705395910079,34.2049798302336,49.213861593386));
#30791=CARTESIAN_POINT('Ctrl Pts',(40.3324545938023,34.2007792368066,49.1450966920792));
#30792=CARTESIAN_POINT('Ctrl Pts',(40.2944092730564,34.1965830195037,49.0764034291612));
#30793=CARTESIAN_POINT('Ctrl Pts',(40.2597453453305,34.1923868022008,49.0057292157322));
#30794=CARTESIAN_POINT('Ctrl Pts',(40.2286703096372,34.1881905848979,48.9334440618746));
#30795=CARTESIAN_POINT('Ctrl Pts',(40.197049657644,34.1839206903004,48.8598897233707));
#30796=CARTESIAN_POINT('Ctrl Pts',(40.1691454159207,34.179650795703,48.7846677500641));
#30797=CARTESIAN_POINT('Ctrl Pts',(40.1451269353427,34.1753809011055,48.7081934080342));
#30798=CARTESIAN_POINT('Ctrl Pts',(40.121545235019,34.1711886552853,48.6331097652391));
#30799=CARTESIAN_POINT('Ctrl Pts',(40.1017092685791,34.1669964094651,48.5568194022073));
#30800=CARTESIAN_POINT('Ctrl Pts',(40.0857297276285,34.1628041636449,48.4797327874113));
#30801=CARTESIAN_POINT('Ctrl Pts',(40.0693062270907,34.1584954446588,48.4005044751918));
#30802=CARTESIAN_POINT('Ctrl Pts',(40.0569567714156,34.1541867256727,48.3204355148518));
#30803=CARTESIAN_POINT('Ctrl Pts',(40.0487453046816,34.1498780066866,48.2399829132314));
#30804=CARTESIAN_POINT('Ctrl Pts',(40.0405338379475,34.1455692877005,48.1595303116111));
#30805=CARTESIAN_POINT('Ctrl Pts',(40.0364603855593,34.1412605687144,48.0786946135994));
#30806=CARTESIAN_POINT('Ctrl Pts',(40.0365309009766,34.1369518497283,47.9979362990588));
#30807=CARTESIAN_POINT('',(40.0365300017577,33.3432018497554,47.9999088486209));
#30808=CARTESIAN_POINT('Ctrl Pts',(40.0365309009773,34.1369518496884,47.9979362983109));
#30809=CARTESIAN_POINT('Ctrl Pts',(40.0366146349956,34.1318354334801,47.9020393157517));
#30810=CARTESIAN_POINT('Ctrl Pts',(40.0425386403499,34.1267190172719,47.8063991429868));
#30811=CARTESIAN_POINT('Ctrl Pts',(40.054186890387,34.1216026010636,47.711640336268));
#30812=CARTESIAN_POINT('Ctrl Pts',(40.066007939675,34.1164102839359,47.6154758033015));
#30813=CARTESIAN_POINT('Ctrl Pts',(40.0837242615162,34.1112179668082,47.5202189535493));
#30814=CARTESIAN_POINT('Ctrl Pts',(40.10716584825,34.1060256496804,47.4265002236539));
#30815=CARTESIAN_POINT('Ctrl Pts',(40.1165734754215,34.103941857988,47.388888824739));
#30816=CARTESIAN_POINT('Ctrl Pts',(40.1269026727228,34.1018580662955,47.3515249082308));
#30817=CARTESIAN_POINT('Ctrl Pts',(40.1381403134859,34.0997742746031,47.3144482518275));
#30818=CARTESIAN_POINT('Ctrl Pts',(40.1609818630579,34.095538774266,47.2390865008115));
#30819=CARTESIAN_POINT('Ctrl Pts',(40.1876373614446,34.0913032739288,47.1647243248294));
#30820=CARTESIAN_POINT('Ctrl Pts',(40.21800112357,34.0870677735917,47.0917757192421));
#30821=CARTESIAN_POINT('Ctrl Pts',(40.248320867881,34.0828384133853,47.0189328659713));
#30822=CARTESIAN_POINT('Ctrl Pts',(40.2823380216964,34.0786090531788,46.9474999433386));
#30823=CARTESIAN_POINT('Ctrl Pts',(40.3198970969558,34.0743796929724,46.8778759633413));
#30824=CARTESIAN_POINT('Ctrl Pts',(40.357412311004,34.0701552717816,46.8083332897146));
#30825=CARTESIAN_POINT('Ctrl Pts',(40.3984610053576,34.0659308505909,46.7405957717856));
#30826=CARTESIAN_POINT('Ctrl Pts',(40.4428401811182,34.0617064294001,46.6750411763929));
#30827=CARTESIAN_POINT('Ctrl Pts',(40.4871909772354,34.0574847096467,46.6095285019236));
#30828=CARTESIAN_POINT('Ctrl Pts',(40.5348677651948,34.0532629898934,46.546196366967));
#30829=CARTESIAN_POINT('Ctrl Pts',(40.5856229454918,34.0490412701401,46.4853956473804));
#30830=CARTESIAN_POINT('Ctrl Pts',(40.6363615189194,34.0448209317146,46.424614821519));
#30831=CARTESIAN_POINT('Ctrl Pts',(40.690176184096,34.0406005932892,46.366364126399));
#30832=CARTESIAN_POINT('Ctrl Pts',(40.7467784934986,34.0363802548638,46.3109620811417));
#30833=CARTESIAN_POINT('Ctrl Pts',(40.803379958588,34.0321599793915,46.2555608622936));
#30834=CARTESIAN_POINT('Ctrl Pts',(40.8627686488952,34.0279397039191,46.2030085361961));
#30835=CARTESIAN_POINT('Ctrl Pts',(40.9246197034793,34.0237194284467,46.1535863352059));
#30836=CARTESIAN_POINT('Ctrl Pts',(40.9865326235147,34.0194949317165,46.104114700511));
#30837=CARTESIAN_POINT('Ctrl Pts',(41.0509124603078,34.0152704349864,46.057779738888));
#30838=CARTESIAN_POINT('Ctrl Pts',(41.1174022179446,34.0110459382562,46.014821577196));
#30839=CARTESIAN_POINT('Ctrl Pts',(41.1839238971349,34.0068194133565,45.9718427914063));
#30840=CARTESIAN_POINT('Ctrl Pts',(41.252557108026,34.0025928884568,45.9322442700401));
#30841=CARTESIAN_POINT('Ctrl Pts',(41.3229191201371,33.9983663635571,45.8962207294648));
#30842=CARTESIAN_POINT('Ctrl Pts',(41.3934097516231,33.9941321127131,45.8601313390775));
#30843=CARTESIAN_POINT('Ctrl Pts',(41.4656350699925,33.989897861869,45.8276301809428));
#30844=CARTESIAN_POINT('Ctrl Pts',(41.5391913676716,33.985663611025,45.7988641706135));
#30845=CARTESIAN_POINT('Ctrl Pts',(41.6093446940789,33.9816252514158,45.7714289764053));
#30846=CARTESIAN_POINT('Ctrl Pts',(41.6807082215308,33.9775868918065,45.7473910500946));
#30847=CARTESIAN_POINT('Ctrl Pts',(41.7529214193359,33.9735485321973,45.7268348605203));
#30848=CARTESIAN_POINT('Ctrl Pts',(41.82865984706,33.9693130320853,45.70527517994));
#30849=CARTESIAN_POINT('Ctrl Pts',(41.9056209179429,33.9650775319733,45.6874638985284));
#30850=CARTESIAN_POINT('Ctrl Pts',(41.9833992755834,33.9608420318614,45.6735361001478));
#30851=CARTESIAN_POINT('Ctrl Pts',(42.061064879291,33.9566126718803,45.6596284926543));
#30852=CARTESIAN_POINT('Ctrl Pts',(42.1395449588451,33.9523833118992,45.6495932703991));
#30853=CARTESIAN_POINT('Ctrl Pts',(42.2184198162798,33.9481539519181,45.6435155256654));
#30854=CARTESIAN_POINT('Ctrl Pts',(42.2972025642471,33.9439295309519,45.6374448784764));
#30855=CARTESIAN_POINT('Ctrl Pts',(42.3763787084319,33.9397051099857,45.6353225608754));
#30856=CARTESIAN_POINT('Ctrl Pts',(42.4555207156813,33.9354806890195,45.6371822137477));
#30857=CARTESIAN_POINT('Ctrl Pts',(42.5346121131225,33.9312589694902,45.6390406774074));
#30858=CARTESIAN_POINT('Ctrl Pts',(42.6136689490017,33.9270372499608,45.6448760464962));
#30859=CARTESIAN_POINT('Ctrl Pts',(42.6922621776862,33.9228155304315,45.6546699037462));
#30860=CARTESIAN_POINT('Ctrl Pts',(42.7708296910304,33.9185951922292,45.6644605564914));
#30861=CARTESIAN_POINT('Ctrl Pts',(42.8489334329895,33.9143748540269,45.6782070675668));
#30862=CARTESIAN_POINT('Ctrl Pts',(42.9261494724226,33.9101545158247,45.6958391606554));
#30863=CARTESIAN_POINT('Ctrl Pts',(43.0033643600774,33.9059342405743,45.7134709907382));
#30864=CARTESIAN_POINT('Ctrl Pts',(43.0796911142504,33.9017139653239,45.7349881818388));
#30865=CARTESIAN_POINT('Ctrl Pts',(43.1547174636666,33.8974936900734,45.7602696611117));
#30866=CARTESIAN_POINT('Ctrl Pts',(43.2298188569599,33.8932691935618,45.7855764277702));
#30867=CARTESIAN_POINT('Ctrl Pts',(43.303616801326,33.8890446970502,45.8146548537638));
#30868=CARTESIAN_POINT('Ctrl Pts',(43.3757162116203,33.8848202005386,45.8473346021081));
#30869=CARTESIAN_POINT('Ctrl Pts',(43.4478502366745,33.8805936758561,45.8800300399238));
#30870=CARTESIAN_POINT('Ctrl Pts',(43.5182836853803,33.8763671511735,45.9163300291294));
#30871=CARTESIAN_POINT('Ctrl Pts',(43.586645741911,33.8721406264909,45.9560180225588));
#30872=CARTESIAN_POINT('Ctrl Pts',(43.6551327620544,33.8679063758588,45.9957785643475));
#30873=CARTESIAN_POINT('Ctrl Pts',(43.7215404292606,33.8636721252268,46.0389392293035));
#30874=CARTESIAN_POINT('Ctrl Pts',(43.7855267811018,33.8594378745947,46.0852399681031));
#30875=CARTESIAN_POINT('Ctrl Pts',(43.8465529339506,33.8553995129936,46.1293986969836));
#30876=CARTESIAN_POINT('Ctrl Pts',(43.9053765954837,33.8513611513925,46.1764131347739));
#30877=CARTESIAN_POINT('Ctrl Pts',(43.9617316806105,33.8473227897913,46.2260257615519));
#30878=CARTESIAN_POINT('Ctrl Pts',(44.0208378242783,33.8430872894733,46.2780603035899));
#30879=CARTESIAN_POINT('Ctrl Pts',(44.0774528983318,33.8388517891552,46.333150975109));
#30880=CARTESIAN_POINT('Ctrl Pts',(44.1312439990707,33.8346162888371,46.3910299391904));
#30881=CARTESIAN_POINT('Ctrl Pts',(44.1849571197706,33.8303869286515,46.4488249971272));
#30882=CARTESIAN_POINT('Ctrl Pts',(44.2358540800347,33.8261575684658,46.5093999797577));
#30883=CARTESIAN_POINT('Ctrl Pts',(44.2836362618204,33.8219282082801,46.5724479434868));
#30884=CARTESIAN_POINT('Ctrl Pts',(44.331362643899,33.8177037871125,46.6354222802323));
#30885=CARTESIAN_POINT('Ctrl Pts',(44.3759811937051,33.8134793659449,46.7008634871008));
#30886=CARTESIAN_POINT('Ctrl Pts',(44.4172323264973,33.8092549447773,46.7684301961179));
#30887=CARTESIAN_POINT('Ctrl Pts',(44.4584570799563,33.8050332250486,46.8359536974794));
#30888=CARTESIAN_POINT('Ctrl Pts',(44.4963184465296,33.8008115053199,46.9055996037187));
#30889=CARTESIAN_POINT('Ctrl Pts',(44.5305998056052,33.7965897855912,46.9769971118051));
#30890=CARTESIAN_POINT('Ctrl Pts',(44.564869947961,33.7923694471918,47.0483712589203));
#30891=CARTESIAN_POINT('Ctrl Pts',(44.5955622057589,33.7881491087924,47.1214954470759));
#30892=CARTESIAN_POINT('Ctrl Pts',(44.6225063401989,33.7839287703931,47.1959751193679));
#30893=CARTESIAN_POINT('Ctrl Pts',(44.6494500727158,33.7797084949481,47.2704536806535));
#30894=CARTESIAN_POINT('Ctrl Pts',(44.672645634599,33.7754882195031,47.3462872440715));
#30895=CARTESIAN_POINT('Ctrl Pts',(44.6919718162422,33.7712679440581,47.4230635785016));
#30896=CARTESIAN_POINT('Ctrl Pts',(44.7113173285569,33.7670434473573,47.4999167071025));
#30897=CARTESIAN_POINT('Ctrl Pts',(44.7267856144159,33.7628189506564,47.5777140342167));
#30898=CARTESIAN_POINT('Ctrl Pts',(44.7383061942865,33.7585944539556,47.6560311312614));
#30899=CARTESIAN_POINT('Ctrl Pts',(44.7498323051536,33.7543679290863,47.7343858281133));
#30900=CARTESIAN_POINT('Ctrl Pts',(44.7574068894699,33.7501414042171,47.8132603241657));
#30901=CARTESIAN_POINT('Ctrl Pts',(44.7610114612567,33.7459148793478,47.8922256026953));
#30902=CARTESIAN_POINT('Ctrl Pts',(44.7646226220774,33.7416806285357,47.9713352270527));
#30903=CARTESIAN_POINT('Ctrl Pts',(44.764249271304,33.7374463777236,48.050535494908));
#30904=CARTESIAN_POINT('Ctrl Pts',(44.7599251189361,33.7332121269114,48.129398121757));
#30905=CARTESIAN_POINT('Ctrl Pts',(44.7558010166928,33.7291737670695,48.2046122929127));
#30906=CARTESIAN_POINT('Ctrl Pts',(44.7480836571655,33.7251354072275,48.2795190215198));
#30907=CARTESIAN_POINT('Ctrl Pts',(44.7368456719384,33.7210970473855,48.3537552069477));
#30908=CARTESIAN_POINT('Ctrl Pts',(44.725059081124,33.7168615466212,48.431615385938));
#30909=CARTESIAN_POINT('Ctrl Pts',(44.70935455133,33.7126260458568,48.5090338451429));
#30910=CARTESIAN_POINT('Ctrl Pts',(44.6897772429322,33.7083905450925,48.5855857056399));
#30911=CARTESIAN_POINT('Ctrl Pts',(44.6702283154024,33.7041611844565,48.6620265902968));
#30912=CARTESIAN_POINT('Ctrl Pts',(44.6468178735759,33.6999318238206,48.7376029201498));
#30913=CARTESIAN_POINT('Ctrl Pts',(44.6196425158882,33.6957024631847,48.8118974951072));
#30914=CARTESIAN_POINT('Ctrl Pts',(44.5924988933709,33.6914780415631,48.8861053094407));
#30915=CARTESIAN_POINT('Ctrl Pts',(44.5615992523267,33.6872536199415,48.9590339048458));
#30916=CARTESIAN_POINT('Ctrl Pts',(44.5270902597421,33.6830291983198,49.0302802860436));
#30917=CARTESIAN_POINT('Ctrl Pts',(44.4926033349979,33.678807478135,49.1014811065443));
#30918=CARTESIAN_POINT('Ctrl Pts',(44.4545118438668,33.6745857579502,49.1710014266907));
#30919=CARTESIAN_POINT('Ctrl Pts',(44.4130104522693,33.6703640377653,49.2384584611341));
#30920=CARTESIAN_POINT('Ctrl Pts',(44.3715226397408,33.6661436989083,49.3058934239387));
#30921=CARTESIAN_POINT('Ctrl Pts',(44.3266273879185,33.6619233600514,49.3712660421081));
#30922=CARTESIAN_POINT('Ctrl Pts',(44.2785644325601,33.6577030211944,49.4342196880604));
#30923=CARTESIAN_POINT('Ctrl Pts',(44.2305021941429,33.653482745291,49.4971723949515));
#30924=CARTESIAN_POINT('Ctrl Pts',(44.1792726319915,33.6492624693877,49.5577058291042));
#30925=CARTESIAN_POINT('Ctrl Pts',(44.1251568707502,33.6450421934843,49.6154950362671));
#30926=CARTESIAN_POINT('Ctrl Pts',(44.0709869812064,33.6408176963269,49.6733420460295));
#30927=CARTESIAN_POINT('Ctrl Pts',(44.0139254472705,33.6365931991696,49.7284390021823));
#30928=CARTESIAN_POINT('Ctrl Pts',(43.9542910965313,33.6323687020123,49.7804970171678));
#30929=CARTESIAN_POINT('Ctrl Pts',(43.8946281155237,33.6281421766868,49.8325800250463));
#30930=CARTESIAN_POINT('Ctrl Pts',(43.8323902262042,33.6239156513614,49.8816208943922));
#30931=CARTESIAN_POINT('Ctrl Pts',(43.7679282429864,33.619689126036,49.9273719835414));
#30932=CARTESIAN_POINT('Ctrl Pts',(43.7033484255725,33.6154548747737,49.9732067040425));
#30933=CARTESIAN_POINT('Ctrl Pts',(43.6365367872811,33.6112206235114,50.0157393750479));
#30934=CARTESIAN_POINT('Ctrl Pts',(43.5678717642886,33.6069863722491,50.0547666493005));
#30935=CARTESIAN_POINT('Ctrl Pts',(43.5023834940629,33.6029480164926,50.091988346331));
#30936=CARTESIAN_POINT('Ctrl Pts',(43.4352098736056,33.5989096607361,50.1260216957278));
#30937=CARTESIAN_POINT('Ctrl Pts',(43.3666955727028,33.5948713049797,50.1567313487351));
#30938=CARTESIAN_POINT('Ctrl Pts',(43.2948365613139,33.5906358059894,50.1889401763247));
#30939=CARTESIAN_POINT('Ctrl Pts',(43.221229477731,33.5864003069991,50.2176149438563));
#30940=CARTESIAN_POINT('Ctrl Pts',(43.1462560880774,33.5821648080087,50.242563776553));
#30941=CARTESIAN_POINT('Ctrl Pts',(43.0713913860735,33.5779354491494,50.2674764413506));
#30942=CARTESIAN_POINT('Ctrl Pts',(42.995164752915,33.57370609029,50.2886737506457));
#30943=CARTESIAN_POINT('Ctrl Pts',(42.9179793241891,33.5694767314307,50.3060112446848));
#30944=CARTESIAN_POINT('Ctrl Pts',(42.8408840319596,33.5652523115811,50.3233284921437));
#30945=CARTESIAN_POINT('Ctrl Pts',(42.7628326247246,33.5610278917316,50.3367947791789));
#30946=CARTESIAN_POINT('Ctrl Pts',(42.6842433781053,33.556803471882,50.3463154397701));
#30947=CARTESIAN_POINT('Ctrl Pts',(42.6057043877616,33.5525817534658,50.3558300120862));
#30948=CARTESIAN_POINT('Ctrl Pts',(42.5266287053627,33.5483600350495,50.3614039095781));
#30949=CARTESIAN_POINT('Ctrl Pts',(42.4474435764409,33.5441383166333,50.3629937680736));
#30950=CARTESIAN_POINT('Ctrl Pts',(42.3682843564389,33.5399179795391,50.3645831063765));
#30951=CARTESIAN_POINT('Ctrl Pts',(42.2890162299233,33.5356976424449,50.3621909846959));
#30952=CARTESIAN_POINT('Ctrl Pts',(42.2100688254176,33.5314773053507,50.355826094987));
#30953=CARTESIAN_POINT('Ctrl Pts',(42.1311225983941,33.5272570312019,50.3494613002089));
#30954=CARTESIAN_POINT('Ctrl Pts',(42.0524975515986,33.523036757053,50.3391238942317));
#30955=CARTESIAN_POINT('Ctrl Pts',(41.9746190664326,33.5188164829042,50.3248745132281));
#30956=CARTESIAN_POINT('Ctrl Pts',(41.8966626842367,33.5145919874762,50.3106108794502));
#30957=CARTESIAN_POINT('Ctrl Pts',(41.8194548181666,33.5103674920483,50.2924275387982));
#30958=CARTESIAN_POINT('Ctrl Pts',(41.7434109134956,33.5061429966203,50.2704363484545));
#30959=CARTESIAN_POINT('Ctrl Pts',(41.6673305001692,33.5019164730134,50.248434600147));
#30960=CARTESIAN_POINT('Ctrl Pts',(41.5924156058328,33.4976899494065,50.2226215133649));
#30961=CARTESIAN_POINT('Ctrl Pts',(41.5190642913965,33.4934634257996,50.1931581607826));
#30962=CARTESIAN_POINT('Ctrl Pts',(41.4455788926556,33.4892291762169,50.1636409499542));
#30963=CARTESIAN_POINT('Ctrl Pts',(41.3736632124349,33.4849949266342,50.1304603370704));
#30964=CARTESIAN_POINT('Ctrl Pts',(41.3036930019361,33.4807606770515,50.093824588378));
#30965=CARTESIAN_POINT('Ctrl Pts',(41.2369596415406,33.4767223055589,50.0588836241673));
#30966=CARTESIAN_POINT('Ctrl Pts',(41.1719960242722,33.4726839340663,50.0208003394924));
#30967=CARTESIAN_POINT('Ctrl Pts',(41.1091024491847,33.4686455625738,49.9797913915863));
#30968=CARTESIAN_POINT('Ctrl Pts',(41.0432115943436,33.4644147369379,49.9368281059103));
#30969=CARTESIAN_POINT('Ctrl Pts',(40.9793413080481,33.4601839113021,49.8904892083675));
#30970=CARTESIAN_POINT('Ctrl Pts',(40.9178590231447,33.4559530856662,49.8409911910779));
#30971=CARTESIAN_POINT('Ctrl Pts',(40.8564659153205,33.4517283966382,49.7915649682672));
#30972=CARTESIAN_POINT('Ctrl Pts',(40.7974542944261,33.4475037076102,49.7389890170494));
#30973=CARTESIAN_POINT('Ctrl Pts',(40.7411633225029,33.4432790185822,49.683523483142));
#30974=CARTESIAN_POINT('Ctrl Pts',(40.684937948313,33.4390592527242,49.6281225850575));
#30975=CARTESIAN_POINT('Ctrl Pts',(40.631427256575,33.4348394868662,49.569839123921));
#30976=CARTESIAN_POINT('Ctrl Pts',(40.58093675295,33.4306197210082,49.5089729434724));
#30977=CARTESIAN_POINT('Ctrl Pts',(40.5304783742662,33.4264026400061,49.4481454895631));
#30978=CARTESIAN_POINT('Ctrl Pts',(40.4830366695324,33.4221855590041,49.3847389388626));
#30979=CARTESIAN_POINT('Ctrl Pts',(40.4388788661868,33.4179684780021,49.3190884501849));
#30980=CARTESIAN_POINT('Ctrl Pts',(40.3947352858967,33.4137527553053,49.2534591072724));
#30981=CARTESIAN_POINT('Ctrl Pts',(40.3538737691867,33.4095370326085,49.1855876516346));
#30982=CARTESIAN_POINT('Ctrl Pts',(40.3165190562355,33.4053213099118,49.1158394140154));
#30983=CARTESIAN_POINT('Ctrl Pts',(40.2791646398873,33.4011056206886,49.0460917302095));
#30984=CARTESIAN_POINT('Ctrl Pts',(40.2453171927927,33.3968899314654,48.9744677095271));
#30985=CARTESIAN_POINT('Ctrl Pts',(40.2151554674143,33.3926742422422,48.9013572040709));
#30986=CARTESIAN_POINT('Ctrl Pts',(40.1849635162688,33.3884543283787,48.8281734328751));
#30987=CARTESIAN_POINT('Ctrl Pts',(40.1584648442828,33.3842344145152,48.7535006374389));
#30988=CARTESIAN_POINT('Ctrl Pts',(40.1357897395433,33.3800145006517,48.6777479895525));
#30989=CARTESIAN_POINT('Ctrl Pts',(40.1131035277608,33.3757925197299,48.6019582354247));
#30990=CARTESIAN_POINT('Ctrl Pts',(40.0942447258862,33.371570538808,48.5250880328208));
#30991=CARTESIAN_POINT('Ctrl Pts',(40.0792928199903,33.3673485578862,48.4475585163433));
#30992=CARTESIAN_POINT('Ctrl Pts',(40.064313858222,33.3631189371773,48.3698887081383));
#30993=CARTESIAN_POINT('Ctrl Pts',(40.0532559831891,33.3588893164684,48.2915576693378));
#30994=CARTESIAN_POINT('Ctrl Pts',(40.0461469170547,33.3546596957595,48.2129932036679));
#30995=CARTESIAN_POINT('Ctrl Pts',(40.0397275404243,33.3508404137581,48.1420507077958));
#30996=CARTESIAN_POINT('Ctrl Pts',(40.036527263158,33.3470211317567,48.0709181788555));
#30997=CARTESIAN_POINT('Ctrl Pts',(40.0365300017577,33.3432018497554,47.9999088486209));
#30998=CARTESIAN_POINT('',(40.0365309427124,32.5494518497613,48.0021109581357));
#30999=CARTESIAN_POINT('Ctrl Pts',(40.0365300017577,33.3432018497283,47.999908848118));
#31000=CARTESIAN_POINT('Ctrl Pts',(40.0365301886757,33.3429411732082,47.995062265673));
#31001=CARTESIAN_POINT('Ctrl Pts',(40.0365452833311,33.3426804966881,47.9902157169632));
#31002=CARTESIAN_POINT('Ctrl Pts',(40.0365752852343,33.342419820168,47.9853692606322));
#31003=CARTESIAN_POINT('Ctrl Pts',(40.0370627597868,33.3381843165302,47.9066234518049));
#31004=CARTESIAN_POINT('Ctrl Pts',(40.0414910096202,33.3339488128924,47.8277523584294));
#31005=CARTESIAN_POINT('Ctrl Pts',(40.0498763342247,33.3297133092546,47.7491829422411));
#31006=CARTESIAN_POINT('Ctrl Pts',(40.0582495028227,33.3254839457262,47.6707274262747));
#31007=CARTESIAN_POINT('Ctrl Pts',(40.0705683051724,33.3212545821977,47.5925731817794));
#31008=CARTESIAN_POINT('Ctrl Pts',(40.0867970331473,33.3170252186692,47.5151469552082));
#31009=CARTESIAN_POINT('Ctrl Pts',(40.1030068094114,33.3128007941399,47.4378111460411));
#31010=CARTESIAN_POINT('Ctrl Pts',(40.1231173420964,33.3085763696107,47.3612021223331));
#31011=CARTESIAN_POINT('Ctrl Pts',(40.1470413339673,33.3043519450814,47.2857397602776));
#31012=CARTESIAN_POINT('Ctrl Pts',(40.1709500269587,33.300130221981,47.210325654784));
#31013=CARTESIAN_POINT('Ctrl Pts',(40.1986671975273,33.2959084988806,47.1360572017636));
#31014=CARTESIAN_POINT('Ctrl Pts',(40.2300551454641,33.2916867757802,47.0633411671409));
#31015=CARTESIAN_POINT('Ctrl Pts',(40.2614328234411,33.2874664340038,46.990648924795));
#31016=CARTESIAN_POINT('Ctrl Pts',(40.2964787080179,33.2832460922275,46.9195085228346));
#31017=CARTESIAN_POINT('Ctrl Pts',(40.335006740943,33.2790257504511,46.8503073102132));
#31018=CARTESIAN_POINT('Ctrl Pts',(40.3735341991558,33.2748054716284,46.7811071298479));
#31019=CARTESIAN_POINT('Ctrl Pts',(40.4155434729893,33.2705851928057,46.7138464907509));
#31020=CARTESIAN_POINT('Ctrl Pts',(40.4608029972008,33.2663649139831,46.6488873380674));
#31021=CARTESIAN_POINT('Ctrl Pts',(40.5061077911708,33.2621404139273,46.5838632115425));
#31022=CARTESIAN_POINT('Ctrl Pts',(40.5546690608197,33.2579159138715,46.5211455559961));
#31023=CARTESIAN_POINT('Ctrl Pts',(40.6062127509982,33.2536914138157,46.4610660357838));
#31024=CARTESIAN_POINT('Ctrl Pts',(40.6577811870465,33.2494648855984,46.4009576716919));
#31025=CARTESIAN_POINT('Ctrl Pts',(40.712334572453,33.2452383573811,46.343490306935));
#31026=CARTESIAN_POINT('Ctrl Pts',(40.7695612755813,33.2410118291638,46.2889593789697));
#31027=CARTESIAN_POINT('Ctrl Pts',(40.8268925863817,33.2367775750553,46.2343287710801));
#31028=CARTESIAN_POINT('Ctrl Pts',(40.8869066230888,33.2325433209469,46.1826456329205));
#31029=CARTESIAN_POINT('Ctrl Pts',(40.949258059808,33.2283090668384,46.1341655314932));
#31030=CARTESIAN_POINT('Ctrl Pts',(41.0087244148732,33.2242707371463,46.0879286670877));
#31031=CARTESIAN_POINT('Ctrl Pts',(41.0703163320914,33.2202324074542,46.0446051538659));
#31032=CARTESIAN_POINT('Ctrl Pts',(41.1337121478315,33.2161940777621,46.0043784135387));
#31033=CARTESIAN_POINT('Ctrl Pts',(41.2002030886068,33.2119585878129,45.9621877140823));
#31034=CARTESIAN_POINT('Ctrl Pts',(41.2689313141011,33.2077230978637,45.9232435152126));
#31035=CARTESIAN_POINT('Ctrl Pts',(41.3395465581916,33.2034876079144,45.887790507867));
#31036=CARTESIAN_POINT('Ctrl Pts',(41.4100594322341,33.1992582581027,45.8523888963088));
#31037=CARTESIAN_POINT('Ctrl Pts',(41.4824534765709,33.1950289082911,45.820468634562));
#31038=CARTESIAN_POINT('Ctrl Pts',(41.556350470286,33.1907995584794,45.7922305573468));
#31039=CARTESIAN_POINT('Ctrl Pts',(41.6301611680874,33.1865751476454,45.7640254561777));
#31040=CARTESIAN_POINT('Ctrl Pts',(41.7054708913532,33.1823507368114,45.7394941612978));
#31041=CARTESIAN_POINT('Ctrl Pts',(41.7818792878239,33.1781263259774,45.7187904028611));
#31042=CARTESIAN_POINT('Ctrl Pts',(41.8582388229468,33.1739046165535,45.6980998839842));
#31043=CARTESIAN_POINT('Ctrl Pts',(41.9356951850186,33.1696829071295,45.6812321659715));
#31044=CARTESIAN_POINT('Ctrl Pts',(42.0138317801886,33.1654611977055,45.668291496154));
#31045=CARTESIAN_POINT('Ctrl Pts',(42.0919428101117,33.1612408695683,45.6553550603503));
#31046=CARTESIAN_POINT('Ctrl Pts',(42.1707331685003,33.1570205414311,45.6463431980313));
#31047=CARTESIAN_POINT('Ctrl Pts',(42.2497764303575,33.1528002132939,45.6413089816545));
#31048=CARTESIAN_POINT('Ctrl Pts',(42.3288185141863,33.1485799480547,45.6362748403056));
#31049=CARTESIAN_POINT('Ctrl Pts',(42.4081130255018,33.1443596828155,45.6352182555618));
#31050=CARTESIAN_POINT('Ctrl Pts',(42.4872302856977,33.1401394175764,45.6381402839802));
#31051=CARTESIAN_POINT('Ctrl Pts',(42.5664266847193,33.1359149309216,45.6410652352235));
#31052=CARTESIAN_POINT('Ctrl Pts',(42.6454450082886,33.1316904442669,45.6479767322123));
#31053=CARTESIAN_POINT('Ctrl Pts',(42.7238580581001,33.1274659576121,45.6588237146461));
#31054=CARTESIAN_POINT('Ctrl Pts',(42.8023087551845,33.1232394427184,45.6696759048777));
#31055=CARTESIAN_POINT('Ctrl Pts',(42.8801531378612,33.1190129278247,45.6844672569032));
#31056=CARTESIAN_POINT('Ctrl Pts',(42.9569741471685,33.114786412931,45.7030955091067));
#31057=CARTESIAN_POINT('Ctrl Pts',(43.0339355873157,33.1105521718561,45.7217578142486));
#31058=CARTESIAN_POINT('Ctrl Pts',(43.1098694647127,33.1063179307812,45.7442709013296));
#31059=CARTESIAN_POINT('Ctrl Pts',(43.1843740243166,33.1020836897063,45.7704826013513));
#31060=CARTESIAN_POINT('Ctrl Pts',(43.2554335226878,33.0980452382563,45.7954822827788));
#31061=CARTESIAN_POINT('Ctrl Pts',(43.3251926467937,33.0940067868063,45.8238459238552));
#31062=CARTESIAN_POINT('Ctrl Pts',(43.3933230863742,33.0899683353563,45.8554022085771));
#31063=CARTESIAN_POINT('Ctrl Pts',(43.4647779751452,33.085732826222,45.8884982935094));
#31064=CARTESIAN_POINT('Ctrl Pts',(43.5347127990157,33.0814973170877,45.9252323543139));
#31065=CARTESIAN_POINT('Ctrl Pts',(43.6027322727976,33.0772618079534,45.9654421805043));
#31066=CARTESIAN_POINT('Ctrl Pts',(43.6706531389894,33.0730324390217,46.0055937146522));
#31067=CARTESIAN_POINT('Ctrl Pts',(43.7366637684668,33.0688030700899,46.0492107711841));
#31068=CARTESIAN_POINT('Ctrl Pts',(43.8003906372222,33.0645737011582,46.0960839030881));
#31069=CARTESIAN_POINT('Ctrl Pts',(43.8640430841429,33.0603492713895,46.1429022953736));
#31070=CARTESIAN_POINT('Ctrl Pts',(43.9254166941085,33.0561248416209,46.1929689300503));
#31071=CARTESIAN_POINT('Ctrl Pts',(43.9841655866422,33.0519004118522,46.2460302639445));
#31072=CARTESIAN_POINT('Ctrl Pts',(44.0428769091537,33.047678683614,46.2990576650205));
#31073=CARTESIAN_POINT('Ctrl Pts',(44.0989664983492,33.0434569553757,46.3550756504771));
#31074=CARTESIAN_POINT('Ctrl Pts',(44.1521213036876,33.0392352271375,46.4137902477717));
#31075=CARTESIAN_POINT('Ctrl Pts',(44.2052587157395,33.0350148803308,46.4724856325077));
#31076=CARTESIAN_POINT('Ctrl Pts',(44.2554629360496,33.0307945335242,46.5338755292781));
#31077=CARTESIAN_POINT('Ctrl Pts',(44.3024586350226,33.0265741867175,46.5976300121124));
#31078=CARTESIAN_POINT('Ctrl Pts',(44.3494536317073,33.0223539029784,46.6613835422206));
#31079=CARTESIAN_POINT('Ctrl Pts',(44.3932399249475,33.0181336192392,46.7275012095623));
#31080=CARTESIAN_POINT('Ctrl Pts',(44.4335841717754,33.0139133355,46.7956222115945));
#31081=CARTESIAN_POINT('Ctrl Pts',(44.4739687699017,33.0096888307395,46.8638113465352));
#31082=CARTESIAN_POINT('Ctrl Pts',(44.5109042047491,33.0054643259789,46.9340074139761));
#31083=CARTESIAN_POINT('Ctrl Pts',(44.5442023068821,33.0012398212184,47.0058235025604));
#31084=CARTESIAN_POINT('Ctrl Pts',(44.577516394402,32.9970132884041,47.0776740678228));
#31085=CARTESIAN_POINT('Ctrl Pts',(44.6071894946154,32.9927867555897,47.1511457677516));
#31086=CARTESIAN_POINT('Ctrl Pts',(44.6330819850572,32.9885602227754,47.2258325188222));
#31087=CARTESIAN_POINT('Ctrl Pts',(44.6590218042317,32.9843259643063,47.3006557893711));
#31088=CARTESIAN_POINT('Ctrl Pts',(44.6811670731451,32.9800917058371,47.3766980972965));
#31089=CARTESIAN_POINT('Ctrl Pts',(44.6994284220833,32.975857447368,47.453539230488));
#31090=CARTESIAN_POINT('Ctrl Pts',(44.7168445832576,32.9718191625621,47.5268239349756));
#31091=CARTESIAN_POINT('Ctrl Pts',(44.7307283585708,32.9677808777563,47.6008347990511));
#31092=CARTESIAN_POINT('Ctrl Pts',(44.7410462183001,32.9637425929504,47.6752030716234));
#31093=CARTESIAN_POINT('Ctrl Pts',(44.7518680209965,32.9595070709964,47.753203625398));
#31094=CARTESIAN_POINT('Ctrl Pts',(44.7588078116323,32.9552715490425,47.8318938707056));
#31095=CARTESIAN_POINT('Ctrl Pts',(44.7617881702188,32.9510360270885,47.9108536040287));
#31096=CARTESIAN_POINT('Ctrl Pts',(44.76476420838,32.9468066450858,47.9896988747386));
#31097=CARTESIAN_POINT('Ctrl Pts',(44.7637921950172,32.9425772630831,48.0688123926393));
#31098=CARTESIAN_POINT('Ctrl Pts',(44.7588462100641,32.9383478810803,48.1477667018179));
#31099=CARTESIAN_POINT('Ctrl Pts',(44.7539060007715,32.9341234379269,48.2266288123171));
#31100=CARTESIAN_POINT('Ctrl Pts',(44.7450010708078,32.9298989947735,48.3053316175483));
#31101=CARTESIAN_POINT('Ctrl Pts',(44.7321575411424,32.92567455162,48.3834470552665));
#31102=CARTESIAN_POINT('Ctrl Pts',(44.7193222243507,32.9214528098126,48.4615125415903));
#31103=CARTESIAN_POINT('Ctrl Pts',(44.7025533826062,32.9172310680052,48.5389909440019));
#31104=CARTESIAN_POINT('Ctrl Pts',(44.6819288998,32.9130093261978,48.615459939523));
#31105=CARTESIAN_POINT('Ctrl Pts',(44.6613111649013,32.9087889656577,48.6919039159582));
#31106=CARTESIAN_POINT('Ctrl Pts',(44.6368404159638,32.9045686051175,48.7673386884742));
#31107=CARTESIAN_POINT('Ctrl Pts',(44.6086451813714,32.9003482445774,48.8413542082292));
#31108=CARTESIAN_POINT('Ctrl Pts',(44.580450367153,32.8961279469603,48.9153686244573));
#31109=CARTESIAN_POINT('Ctrl Pts',(44.5485313459866,32.8919076493432,48.9879633918609));
#31110=CARTESIAN_POINT('Ctrl Pts',(44.513065328651,32.8876873517261,49.0587470697731));
#31111=CARTESIAN_POINT('Ctrl Pts',(44.477563838149,32.8834628329607,49.1296015456313));
#31112=CARTESIAN_POINT('Ctrl Pts',(44.4385084752291,32.8792383141953,49.198640892767));
#31113=CARTESIAN_POINT('Ctrl Pts',(44.3961228473338,32.8750137954299,49.2654975382244));
#31114=CARTESIAN_POINT('Ctrl Pts',(44.3537168705543,32.8707872485184,49.3323862808385));
#31115=CARTESIAN_POINT('Ctrl Pts',(44.3079777150414,32.8665607016069,49.3970898504622));
#31116=CARTESIAN_POINT('Ctrl Pts',(44.2591713759898,32.8623341546955,49.4592711316271));
#31117=CARTESIAN_POINT('Ctrl Pts',(44.2102758245718,32.8580998821431,49.5215660730121));
#31118=CARTESIAN_POINT('Ctrl Pts',(44.1583021953996,32.8538656095907,49.5813291580854));
#31119=CARTESIAN_POINT('Ctrl Pts',(44.103555552443,32.8496313370383,49.6382578919818));
#31120=CARTESIAN_POINT('Ctrl Pts',(44.0513445009608,32.8455931748737,49.6925499708338));
#31121=CARTESIAN_POINT('Ctrl Pts',(43.9966118976582,32.8415550127092,49.7442642130799));
#31122=CARTESIAN_POINT('Ctrl Pts',(43.9396497050753,32.8375168505446,49.7931729494283));
#31123=CARTESIAN_POINT('Ctrl Pts',(43.8799050192773,32.8332814319488,49.8444707831917));
#31124=CARTESIAN_POINT('Ctrl Pts',(43.8174802415135,32.829046013353,49.8928770260256));
#31125=CARTESIAN_POINT('Ctrl Pts',(43.7526868699549,32.8248105947572,49.9380992422349));
#31126=CARTESIAN_POINT('Ctrl Pts',(43.6879874316164,32.8205813163961,49.9832558982135));
#31127=CARTESIAN_POINT('Ctrl Pts',(43.6209266001007,32.8163520380349,50.0252374277449));
#31128=CARTESIAN_POINT('Ctrl Pts',(43.5518498352913,32.8121227596738,50.0637907834467));
#31129=CARTESIAN_POINT('Ctrl Pts',(43.4828537357243,32.8078984201046,50.1022991179927));
#31130=CARTESIAN_POINT('Ctrl Pts',(43.4118467886812,32.8036740805353,50.1373870064232));
#31131=CARTESIAN_POINT('Ctrl Pts',(43.339203118874,32.799449740966,50.168844840554));
#31132=CARTESIAN_POINT('Ctrl Pts',(43.2666059012847,32.7952281026637,50.2002825588759));
#31133=CARTESIAN_POINT('Ctrl Pts',(43.1923744677768,32.7910064643614,50.2280946440591));
#31134=CARTESIAN_POINT('Ctrl Pts',(43.1169061203529,32.786784826059,50.2521181264535));
#31135=CARTESIAN_POINT('Ctrl Pts',(43.0414624613174,32.7825645688052,50.27613374991));
#31136=CARTESIAN_POINT('Ctrl Pts',(42.9647831387621,32.7783443115513,50.2963630893206));
#31137=CARTESIAN_POINT('Ctrl Pts',(42.8872825306362,32.7741240542975,50.3126924084791));
#31138=CARTESIAN_POINT('Ctrl Pts',(42.8097830714399,32.769903859608,50.329021485559));
#31139=CARTESIAN_POINT('Ctrl Pts',(42.7314628104373,32.7656836649185,50.3414505618484));
#31140=CARTESIAN_POINT('Ctrl Pts',(42.6527468126245,32.761463470229,50.3499169112137));
#31141=CARTESIAN_POINT('Ctrl Pts',(42.5739520570758,32.7572390531072,50.3583917314175));
#31142=CARTESIAN_POINT('Ctrl Pts',(42.4947612415589,32.7530146359853,50.3628958541422));
#31143=CARTESIAN_POINT('Ctrl Pts',(42.4156044580236,32.7487902188635,50.3634184863857));
#31144=CARTESIAN_POINT('Ctrl Pts',(42.3364096612673,32.7445637730626,50.3639413696114));
#31145=CARTESIAN_POINT('Ctrl Pts',(42.257249398617,32.7403373272618,50.3604789739278));
#31146=CARTESIAN_POINT('Ctrl Pts',(42.1785510773987,32.736110881461,50.3530726328736));
#31147=CARTESIAN_POINT('Ctrl Pts',(42.0997088620007,32.7318767079102,50.3456527498613));
#31148=CARTESIAN_POINT('Ctrl Pts',(42.0213307415196,32.7276425343593,50.3342745793876));
#31149=CARTESIAN_POINT('Ctrl Pts',(41.9438361418862,32.7234083608085,50.3190310423646));
#31150=CARTESIAN_POINT('Ctrl Pts',(41.8699121019261,32.7193692765852,50.3044898505222));
#31151=CARTESIAN_POINT('Ctrl Pts',(41.7967922975485,32.715330192362,50.2864317634616));
#31152=CARTESIAN_POINT('Ctrl Pts',(41.7248263995385,32.7112911081387,50.2649792604216));
#31153=CARTESIAN_POINT('Ctrl Pts',(41.6493592792177,32.7070555179009,50.2424830688521));
#31154=CARTESIAN_POINT('Ctrl Pts',(41.5748742971278,32.7028199276631,50.2161682479835));
#31155=CARTESIAN_POINT('Ctrl Pts',(41.5017859410379,32.6985843374253,50.1861385924005));
#31156=CARTESIAN_POINT('Ctrl Pts',(41.4288035460196,32.6943548878056,50.156152472815));
#31157=CARTESIAN_POINT('Ctrl Pts',(41.3572141865826,32.6901254381859,50.1224623903211));
#31158=CARTESIAN_POINT('Ctrl Pts',(41.287417594974,32.6858959885662,50.0852220104648));
#31159=CARTESIAN_POINT('Ctrl Pts',(41.21770252839,32.6816714791015,50.0480251287623));
#31160=CARTESIAN_POINT('Ctrl Pts',(41.1497764803467,32.6774469696368,50.0072864101184));
#31161=CARTESIAN_POINT('Ctrl Pts',(41.0840181554684,32.6732224601722,49.9632071275755));
#31162=CARTESIAN_POINT('Ctrl Pts',(41.0183018922523,32.6690006528732,49.9191560399098));
#31163=CARTESIAN_POINT('Ctrl Pts',(40.954750988961,32.6647788455742,49.8717688899777));
#31164=CARTESIAN_POINT('Ctrl Pts',(40.8937174639057,32.6605570382752,49.821291674158));
#31165=CARTESIAN_POINT('Ctrl Pts',(40.8327039204864,32.6563366131448,49.7708309839667));
#31166=CARTESIAN_POINT('Ctrl Pts',(40.7742064801868,32.6521161880143,49.7172825355787));
#31167=CARTESIAN_POINT('Ctrl Pts',(40.7185449923322,32.6478957628839,49.6609333213855));
#31168=CARTESIAN_POINT('Ctrl Pts',(40.6628843473165,32.6436754016601,49.604584960445));
#31169=CARTESIAN_POINT('Ctrl Pts',(40.61005989826,32.6394550404363,49.5454362528354));
#31170=CARTESIAN_POINT('Ctrl Pts',(40.5603543753744,32.6352346792125,49.4838107752324));
#31171=CARTESIAN_POINT('Ctrl Pts',(40.5105991610115,32.63101009882,49.4221236895657));
#31172=CARTESIAN_POINT('Ctrl Pts',(40.4639693968664,32.6267855184275,49.3579552538229));
#31173=CARTESIAN_POINT('Ctrl Pts',(40.4207068556936,32.622560938035,49.2916613680844));
#31174=CARTESIAN_POINT('Ctrl Pts',(40.3774235549587,32.6183343304746,49.2253356711762));
#31175=CARTESIAN_POINT('Ctrl Pts',(40.3375109327348,32.6141077229141,49.1568828985045));
#31176=CARTESIAN_POINT('Ctrl Pts',(40.3011654703015,32.6098811153537,49.0866848935387));
#31177=CARTESIAN_POINT('Ctrl Pts',(40.2647535939065,32.605646784525,49.0163586159551));
#31178=CARTESIAN_POINT('Ctrl Pts',(40.2319220973869,32.6014124536964,48.9442811618195));
#31179=CARTESIAN_POINT('Ctrl Pts',(40.202819758277,32.5971781228678,48.8708555714251));
#31180=CARTESIAN_POINT('Ctrl Pts',(40.1750696382883,32.5931405371561,48.8008416479397));
#31181=CARTESIAN_POINT('Ctrl Pts',(40.1507099100065,32.5891029514445,48.7296024347614));
#31182=CARTESIAN_POINT('Ctrl Pts',(40.1298266558031,32.5850653657328,48.6574978541392));
#31183=CARTESIAN_POINT('Ctrl Pts',(40.1025025412974,32.579782498741,48.5631546163417));
#31184=CARTESIAN_POINT('Ctrl Pts',(40.0810445127194,32.5744996317493,48.4670411181778));
#31185=CARTESIAN_POINT('Ctrl Pts',(40.0656409106017,32.5692167647575,48.3698081700603));
#31186=CARTESIAN_POINT('Ctrl Pts',(40.0504879803225,32.5640198689543,48.2741575506527));
#31187=CARTESIAN_POINT('Ctrl Pts',(40.0411940473043,32.558822973151,48.1774235249491));
#31188=CARTESIAN_POINT('Ctrl Pts',(40.0378927055361,32.5536260773478,48.0802469335257));
#31189=CARTESIAN_POINT('Ctrl Pts',(40.0370088091741,32.5522346681523,48.0542290166743));
#31190=CARTESIAN_POINT('Ctrl Pts',(40.0365542261138,32.5508432589568,48.0281794990929));
#31191=CARTESIAN_POINT('Ctrl Pts',(40.0365309427124,32.5494518497613,48.0021109581356));
#31192=CARTESIAN_POINT('',(40.036530204639,31.7557018496867,47.9990164777473));
#31193=CARTESIAN_POINT('Ctrl Pts',(40.0365309427119,32.5494518497283,48.0021109575178));
#31194=CARTESIAN_POINT('Ctrl Pts',(40.0364608572083,32.5452635594843,47.923641865808));
#31195=CARTESIAN_POINT('Ctrl Pts',(40.0403028998604,32.5410752692403,47.845091734552));
#31196=CARTESIAN_POINT('Ctrl Pts',(40.0480545536977,32.5368869789963,47.7668840234603));
#31197=CARTESIAN_POINT('Ctrl Pts',(40.0558026175344,32.5327006284628,47.6887125324764));
#31198=CARTESIAN_POINT('Ctrl Pts',(40.0674566527063,32.5285142779294,47.6108836216765));
#31199=CARTESIAN_POINT('Ctrl Pts',(40.0829621346619,32.5243279273959,47.5338176628296));
#31200=CARTESIAN_POINT('Ctrl Pts',(40.0984654725121,32.520142155753,47.4567623607004));
#31201=CARTESIAN_POINT('Ctrl Pts',(40.1178191046942,32.5159563841101,47.3804702691739));
#31202=CARTESIAN_POINT('Ctrl Pts',(40.1409173179971,32.5117706124672,47.3053519763402));
#31203=CARTESIAN_POINT('Ctrl Pts',(40.1640198407705,32.5075840598782,47.2302196685665));
#31204=CARTESIAN_POINT('Ctrl Pts',(40.1908681884987,32.5033975072892,47.1562620499446));
#31205=CARTESIAN_POINT('Ctrl Pts',(40.2213071605378,32.4992109547002,47.0838733972993));
#31206=CARTESIAN_POINT('Ctrl Pts',(40.2517803805662,32.4950196916694,47.0114032975602));
#31207=CARTESIAN_POINT('Ctrl Pts',(40.285852097053,32.4908284286385,46.9405061254933));
#31208=CARTESIAN_POINT('Ctrl Pts',(40.3233197885971,32.4866371656076,46.8715542811161));
#31209=CARTESIAN_POINT('Ctrl Pts',(40.3608130679852,32.4824430402337,46.8025553473943));
#31210=CARTESIAN_POINT('Ctrl Pts',(40.4017066855213,32.4782489148598,46.7355047899506));
#31211=CARTESIAN_POINT('Ctrl Pts',(40.4457545542511,32.474054789486,46.6707463828638));
#31212=CARTESIAN_POINT('Ctrl Pts',(40.4898735926267,32.4698538875205,46.6058833434071));
#31213=CARTESIAN_POINT('Ctrl Pts',(40.5371567570249,32.465652985555,46.5433202181791));
#31214=CARTESIAN_POINT('Ctrl Pts',(40.5873180183348,32.4614520835895,46.483367389825));
#31215=CARTESIAN_POINT('Ctrl Pts',(40.5977161267224,32.460581263502,46.4709395522649));
#31216=CARTESIAN_POINT('Ctrl Pts',(40.608237786181,32.4597104434145,46.4586237507235));
#31217=CARTESIAN_POINT('Ctrl Pts',(40.6188802620662,32.458839623327,46.4464225413444));
#31218=CARTESIAN_POINT('Ctrl Pts',(40.6706354675536,32.4546047560784,46.3870870910772));
#31219=CARTESIAN_POINT('Ctrl Pts',(40.7254574787414,32.4503698888297,46.3302277192351));
#31220=CARTESIAN_POINT('Ctrl Pts',(40.7830801107519,32.4461350215811,46.2761785148532));
#31221=CARTESIAN_POINT('Ctrl Pts',(40.8406191793464,32.4419062956689,46.2222076917599));
#31222=CARTESIAN_POINT('Ctrl Pts',(40.9009504640461,32.4376775697568,46.1710392619322));
#31223=CARTESIAN_POINT('Ctrl Pts',(40.9637685103185,32.4334488438446,46.1229732157087));
#31224=CARTESIAN_POINT('Ctrl Pts',(41.0265132040005,32.4292250558129,46.0749632961749));
#31225=CARTESIAN_POINT('Ctrl Pts',(41.0917385180085,32.4250012677811,46.0300488452585));
#31226=CARTESIAN_POINT('Ctrl Pts',(41.1591043888966,32.4207774797494,45.9884909835538));
#31227=CARTESIAN_POINT('Ctrl Pts',(41.226427189383,32.4165563921985,45.9469596918878));
#31228=CARTESIAN_POINT('Ctrl Pts',(41.295887431959,32.4123353046477,45.9087809758935));
#31229=CARTESIAN_POINT('Ctrl Pts',(41.3671154168577,32.4081142170968,45.8741731305661));
#31230=CARTESIAN_POINT('Ctrl Pts',(41.4383201232241,32.4038945090701,45.8395765956787));
#31231=CARTESIAN_POINT('Ctrl Pts',(41.5112910027688,32.3996748010433,45.8085488191928));
#31232=CARTESIAN_POINT('Ctrl Pts',(41.5856343863434,32.3954550930166,45.7812618252273));
#31233=CARTESIAN_POINT('Ctrl Pts',(41.6599767075322,32.3912354452905,45.7539752211999));
#31234=CARTESIAN_POINT('Ctrl Pts',(41.7356910525477,32.3870157975645,45.7304294539531));
#31235=CARTESIAN_POINT('Ctrl Pts',(41.812365852117,32.3827961498385,45.7107476003853));
#31236=CARTESIAN_POINT('Ctrl Pts',(41.8891175111503,32.378572272302,45.6910460175619));
#31237=CARTESIAN_POINT('Ctrl Pts',(41.9668310921309,32.3743483947656,45.6752162026539));
#31238=CARTESIAN_POINT('Ctrl Pts',(42.04508259513,32.3701245172292,45.6633305589749));
#31239=CARTESIAN_POINT('Ctrl Pts',(42.1233717394494,32.365898607881,45.6514391979448));
#31240=CARTESIAN_POINT('Ctrl Pts',(42.202198853473,32.3616726985328,45.6434958347941));
#31241=CARTESIAN_POINT('Ctrl Pts',(42.2811351138128,32.3574467891846,45.6395209003824));
#31242=CARTESIAN_POINT('Ctrl Pts',(42.3602159403493,32.3532131403813,45.6355386861584));
#31243=CARTESIAN_POINT('Ctrl Pts',(42.4394058418959,32.348979491578,45.6355394235851));
#31244=CARTESIAN_POINT('Ctrl Pts',(42.5182764905371,32.3447458427747,45.6394913445009));
#31245=CARTESIAN_POINT('Ctrl Pts',(42.5936138449197,32.3407018554902,45.6432662249115));
#31246=CARTESIAN_POINT('Ctrl Pts',(42.6686595840971,32.3366578682057,45.6506457692674));
#31247=CARTESIAN_POINT('Ctrl Pts',(42.743048710163,32.3326138809212,45.6615586337572));
#31248=CARTESIAN_POINT('Ctrl Pts',(42.8209763868576,32.3283775287777,45.6729906026584));
#31249=CARTESIAN_POINT('Ctrl Pts',(42.8984798686474,32.3241411766341,45.6883438939023));
#31250=CARTESIAN_POINT('Ctrl Pts',(42.9751339462279,32.3199048244906,45.7075752171998));
#31251=CARTESIAN_POINT('Ctrl Pts',(43.0516768649382,32.3156746156356,45.7267786524549));
#31252=CARTESIAN_POINT('Ctrl Pts',(43.1273723743003,32.3114444067807,45.749848838815));
#31253=CARTESIAN_POINT('Ctrl Pts',(43.2018027161336,32.3072141979257,45.7766910144335));
#31254=CARTESIAN_POINT('Ctrl Pts',(43.27614600427,32.3029889367213,45.8035017954545));
#31255=CARTESIAN_POINT('Ctrl Pts',(43.3492266264,32.2987636755168,45.8340756403681));
#31256=CARTESIAN_POINT('Ctrl Pts',(43.4206408061468,32.2945384143124,45.8682676561707));
#31257=CARTESIAN_POINT('Ctrl Pts',(43.4920092323684,32.2903158601417,45.902437765886));
#31258=CARTESIAN_POINT('Ctrl Pts',(43.5617129132941,32.286093305971,45.9402212434752));
#31259=CARTESIAN_POINT('Ctrl Pts',(43.6293680649197,32.2818707518003,45.9814251062059));
#31260=CARTESIAN_POINT('Ctrl Pts',(43.697000977395,32.2776495856395,46.0226154246778));
#31261=CARTESIAN_POINT('Ctrl Pts',(43.7625862973116,32.2734284194786,46.0672236518772));
#31262=CARTESIAN_POINT('Ctrl Pts',(43.8257661917328,32.2692072533178,46.115011616107));
#31263=CARTESIAN_POINT('Ctrl Pts',(43.8889450275653,32.2649861578832,46.1627987796421));
#31264=CARTESIAN_POINT('Ctrl Pts',(43.9497181446446,32.2607650624487,46.2137652902326));
#31265=CARTESIAN_POINT('Ctrl Pts',(44.007759191331,32.2565439670141,46.2676314411793));
#31266=CARTESIAN_POINT('Ctrl Pts',(44.0658580353617,32.2523186682076,46.3215512321039));
#31267=CARTESIAN_POINT('Ctrl Pts',(44.1212190295284,32.2480933694012,46.3783761115966));
#31268=CARTESIAN_POINT('Ctrl Pts',(44.1735517137177,32.2438680705947,46.4377885035409));
#31269=CARTESIAN_POINT('Ctrl Pts',(44.2259094134132,32.2396407520564,46.497229295157));
#31270=CARTESIAN_POINT('Ctrl Pts',(44.27523562692,32.2354134335181,46.5592596955544));
#31271=CARTESIAN_POINT('Ctrl Pts',(44.3212809875985,32.2311861149798,46.6235299467142));
#31272=CARTESIAN_POINT('Ctrl Pts',(44.3674102436011,32.2269510942049,46.6879172992166));
#31273=CARTESIAN_POINT('Ctrl Pts',(44.4102464473705,32.2227160734301,46.7545522617234));
#31274=CARTESIAN_POINT('Ctrl Pts',(44.4495843956108,32.2184810526553,46.8230572460104));
#31275=CARTESIAN_POINT('Ctrl Pts',(44.4870269849002,32.2144500812753,46.8882615615802));
#31276=CARTESIAN_POINT('Ctrl Pts',(44.5213005112486,32.2104191098953,46.9551595267172));
#31277=CARTESIAN_POINT('Ctrl Pts',(44.5522687182219,32.2063881385153,47.0234090900159));
#31278=CARTESIAN_POINT('Ctrl Pts',(44.584813386975,32.2021519672565,47.0951329528803));
#31279=CARTESIAN_POINT('Ctrl Pts',(44.6138305078913,32.1979157959978,47.1686212744498));
#31280=CARTESIAN_POINT('Ctrl Pts',(44.6391265225361,32.193679624739,47.2434929894737));
#31281=CARTESIAN_POINT('Ctrl Pts',(44.6643859409941,32.1894495820233,47.3182563862778));
#31282=CARTESIAN_POINT('Ctrl Pts',(44.6859347948584,32.1852195393076,47.3943987613566));
#31283=CARTESIAN_POINT('Ctrl Pts',(44.7036268507566,32.180989496592,47.4715174805413));
#31284=CARTESIAN_POINT('Ctrl Pts',(44.721298308255,32.1767643788048,47.5485464124106));
#31285=CARTESIAN_POINT('Ctrl Pts',(44.7351217866846,32.1725392610176,47.6265489745438));
#31286=CARTESIAN_POINT('Ctrl Pts',(44.7450007815637,32.1683141432305,47.7051071798673));
#31287=CARTESIAN_POINT('Ctrl Pts',(44.7548734793124,32.1640917186442,47.7836153101311));
#31288=CARTESIAN_POINT('Ctrl Pts',(44.7608066255724,32.1598692940578,47.8626779163478));
#31289=CARTESIAN_POINT('Ctrl Pts',(44.7627549789776,32.1556468694715,47.941867821161));
#31290=CARTESIAN_POINT('Ctrl Pts',(44.7647026983203,32.15142581901,48.0210319548058));
#31291=CARTESIAN_POINT('Ctrl Pts',(44.7626681883074,32.1472047685486,48.1003228361092));
#31292=CARTESIAN_POINT('Ctrl Pts',(44.756658253001,32.1429837180871,48.1793106786063));
#31293=CARTESIAN_POINT('Ctrl Pts',(44.7506483985321,32.1387627244014,48.258297458667));
#31294=CARTESIAN_POINT('Ctrl Pts',(44.7406632619964,32.1345417307157,48.3369807403088));
#31295=CARTESIAN_POINT('Ctrl Pts',(44.7267616098647,32.13032073703,48.4149347560278));
#31296=CARTESIAN_POINT('Ctrl Pts',(44.7128460402428,32.1260955175417,48.4929668145752));
#31297=CARTESIAN_POINT('Ctrl Pts',(44.6950062049653,32.1218702980534,48.5702676857593));
#31298=CARTESIAN_POINT('Ctrl Pts',(44.6733521350314,32.117645078565,48.6464213107936));
#31299=CARTESIAN_POINT('Ctrl Pts',(44.6516876520385,32.1134178272434,48.7226115567583));
#31300=CARTESIAN_POINT('Ctrl Pts',(44.626205431482,32.1091905759218,48.7976530126676));
#31301=CARTESIAN_POINT('Ctrl Pts',(44.5970647971759,32.1049633246002,48.8711467832177));
#31302=CARTESIAN_POINT('Ctrl Pts',(44.5678709214925,32.1007283498818,48.9447748305144));
#31303=CARTESIAN_POINT('Ctrl Pts',(44.5350054708115,32.0964933751634,49.0168491140407));
#31304=CARTESIAN_POINT('Ctrl Pts',(44.4986750622441,32.0922584004449,49.0869928353098));
#31305=CARTESIAN_POINT('Ctrl Pts',(44.4640858923939,32.0882263989998,49.1537747181615));
#31306=CARTESIAN_POINT('Ctrl Pts',(44.4263564860087,32.0841943975546,49.2188065591027));
#31307=CARTESIAN_POINT('Ctrl Pts',(44.3857010299083,32.0801623961095,49.2817885397839));
#31308=CARTESIAN_POINT('Ctrl Pts',(44.3430420096339,32.0759316913556,49.347874370531));
#31309=CARTESIAN_POINT('Ctrl Pts',(44.2969980803195,32.0717009866017,49.4119556142401));
#31310=CARTESIAN_POINT('Ctrl Pts',(44.2477839303533,32.0674702818478,49.4736637973528));
#31311=CARTESIAN_POINT('Ctrl Pts',(44.1986413466439,32.0632457293022,49.5352822456293));
#31312=CARTESIAN_POINT('Ctrl Pts',(44.1463379872993,32.0590211767567,49.594534120947));
#31313=CARTESIAN_POINT('Ctrl Pts',(44.0911323333135,32.0547966242111,49.6510790023865));
#31314=CARTESIAN_POINT('Ctrl Pts',(44.035991168931,32.0505770066622,49.7075578297769));
#31315=CARTESIAN_POINT('Ctrl Pts',(43.9779547736778,32.0463573891133,49.7613356118631));
#31316=CARTESIAN_POINT('Ctrl Pts',(43.9173214936809,32.0421377715644,49.8121053848256));
#31317=CARTESIAN_POINT('Ctrl Pts',(43.8567269689845,32.0379208510912,49.8628427069985));
#31318=CARTESIAN_POINT('Ctrl Pts',(43.793539213529,32.033703930618,49.9105755345289));
#31319=CARTESIAN_POINT('Ctrl Pts',(43.728092079237,32.0294870101448,49.9550350047935));
#31320=CARTESIAN_POINT('Ctrl Pts',(43.6626662169804,32.0252714602814,49.9994800245641));
#31321=CARTESIAN_POINT('Ctrl Pts',(43.5949828228806,32.021055910418,50.0406535353018));
#31322=CARTESIAN_POINT('Ctrl Pts',(43.5254061330093,32.0168403605545,50.0783290106922));
#31323=CARTESIAN_POINT('Ctrl Pts',(43.4558302002533,32.0126248565636,50.1160040761081));
#31324=CARTESIAN_POINT('Ctrl Pts',(43.3843614270841,32.0084093525727,50.1501809589749));
#31325=CARTESIAN_POINT('Ctrl Pts',(43.3113888010036,32.0041938485818,50.1806789984556));
#31326=CARTESIAN_POINT('Ctrl Pts',(43.2383420628195,31.9999740632612,50.2112080122068));
#31327=CARTESIAN_POINT('Ctrl Pts',(43.1637888559236,31.9957542779406,50.2380505371248));
#31328=CARTESIAN_POINT('Ctrl Pts',(43.0881377505087,31.99153449262,50.261074275035));
#31329=CARTESIAN_POINT('Ctrl Pts',(43.0124498389637,31.9873126542697,50.2841092145618));
#31330=CARTESIAN_POINT('Ctrl Pts',(42.9356634220074,31.9830908159194,50.3033215519959));
#31331=CARTESIAN_POINT('Ctrl Pts',(42.8581992873437,31.9788689775691,50.3186297362834));
#31332=CARTESIAN_POINT('Ctrl Pts',(42.7805915934368,31.9746393151604,50.3339662902334));
#31333=CARTESIAN_POINT('Ctrl Pts',(42.7023041389721,31.9704096527516,50.3453841654492));
#31334=CARTESIAN_POINT('Ctrl Pts',(42.6237647000761,31.9661799903429,50.3528535440821));
#31335=CARTESIAN_POINT('Ctrl Pts',(42.5479836489396,31.9620988781298,50.3600605902758));
#31336=CARTESIAN_POINT('Ctrl Pts',(42.4719684048579,31.9580177659167,50.3635919372317));
#31337=CARTESIAN_POINT('Ctrl Pts',(42.396101149199,31.9539366537036,50.3634667841674));
#31338=CARTESIAN_POINT('Ctrl Pts',(42.31722052377,31.949693443889,50.3633366601514));
#31339=CARTESIAN_POINT('Ctrl Pts',(42.23819890299,31.9454502340745,50.3592530261779));
#31340=CARTESIAN_POINT('Ctrl Pts',(42.1594644392978,31.9412070242599,50.3511982232338));
#31341=CARTESIAN_POINT('Ctrl Pts',(42.0808442658474,31.9369699738507,50.3431551125694));
#31342=CARTESIAN_POINT('Ctrl Pts',(42.0025108828749,31.9327329234415,50.3311523285694));
#31343=CARTESIAN_POINT('Ctrl Pts',(41.9248923818167,31.9284958730323,50.3152242206845));
#31344=CARTESIAN_POINT('Ctrl Pts',(41.8473655468738,31.9242638265068,50.2993149236212));
#31345=CARTESIAN_POINT('Ctrl Pts',(41.7705523715381,31.9200317799812,50.2794896094482));
#31346=CARTESIAN_POINT('Ctrl Pts',(41.6948742435766,31.9157997334557,50.2558342378216));
#31347=CARTESIAN_POINT('Ctrl Pts',(41.619245190707,31.9115704312908,50.232194206024));
#31348=CARTESIAN_POINT('Ctrl Pts',(41.5447501691425,31.9073411291258,50.2047291860695));
#31349=CARTESIAN_POINT('Ctrl Pts',(41.471797652959,31.9031118269609,50.1735755896328));
#31350=CARTESIAN_POINT('Ctrl Pts',(41.3988698801052,31.8988839592498,50.142432559572));
#31351=CARTESIAN_POINT('Ctrl Pts',(41.3274840032654,31.8946560915387,50.107603620975));
#31352=CARTESIAN_POINT('Ctrl Pts',(41.258029291252,31.8904282238276,50.0692736264838));
#31353=CARTESIAN_POINT('Ctrl Pts',(41.1885766545262,31.886200482444,50.0309447772823));
#31354=CARTESIAN_POINT('Ctrl Pts',(41.121055476621,31.8819727410605,49.9891153071296));
#31355=CARTESIAN_POINT('Ctrl Pts',(41.0558298434275,31.8777449996769,49.9440156972308));
#31356=CARTESIAN_POINT('Ctrl Pts',(40.9905414240873,31.8735131886726,49.8988726744806));
#31357=CARTESIAN_POINT('Ctrl Pts',(40.9275533492749,31.8692813776682,49.8504534899445));
#31358=CARTESIAN_POINT('Ctrl Pts',(40.867199632914,31.8650495666639,49.7990312603068));
#31359=CARTESIAN_POINT('Ctrl Pts',(40.8068180043334,31.8608157985433,49.7475852490586));
#31360=CARTESIAN_POINT('Ctrl Pts',(40.7490735025845,31.8565820304227,49.6931337464098));
#31361=CARTESIAN_POINT('Ctrl Pts',(40.6942641376324,31.8523482623022,49.6359876554342));
#31362=CARTESIAN_POINT('Ctrl Pts',(40.6393574214939,31.8481069742559,49.5787400628309));
#31363=CARTESIAN_POINT('Ctrl Pts',(40.5873965671617,31.8438656862097,49.5187886719602));
#31364=CARTESIAN_POINT('Ctrl Pts',(40.5386399076417,31.8396243981635,49.4564783031257));
#31365=CARTESIAN_POINT('Ctrl Pts',(40.4929885381772,31.8356532358749,49.3981364540914));
#31366=CARTESIAN_POINT('Ctrl Pts',(40.4501459827415,31.8316820735863,49.337727110732));
#31367=CARTESIAN_POINT('Ctrl Pts',(40.4102885577865,31.8277109112977,49.2755543177868));
#31368=CARTESIAN_POINT('Ctrl Pts',(40.3669097120312,31.8233888950967,49.2078885315904));
#31369=CARTESIAN_POINT('Ctrl Pts',(40.3269112702481,31.8190668788957,49.1378906414038));
#31370=CARTESIAN_POINT('Ctrl Pts',(40.2905461636704,31.8147448626947,49.065924459469));
#31371=CARTESIAN_POINT('Ctrl Pts',(40.2542398387595,31.8104298327324,48.9940746058644));
#31372=CARTESIAN_POINT('Ctrl Pts',(40.2215553756603,31.8061148027702,48.9202631763286));
#31373=CARTESIAN_POINT('Ctrl Pts',(40.1927018902877,31.8017997728079,48.8448819419069));
#31374=CARTESIAN_POINT('Ctrl Pts',(40.1638961493857,31.7974918830167,48.7696254424033));
#31375=CARTESIAN_POINT('Ctrl Pts',(40.1389089291594,31.7931839932255,48.692804719184));
#31376=CARTESIAN_POINT('Ctrl Pts',(40.1179022731241,31.7888761034343,48.614833640823));
#31377=CARTESIAN_POINT('Ctrl Pts',(40.0969160724432,31.784572408476,48.5369384872566));
#31378=CARTESIAN_POINT('Ctrl Pts',(40.0799028481842,31.7802687135178,48.4578956312762));
#31379=CARTESIAN_POINT('Ctrl Pts',(40.0669753931644,31.7759650185595,48.3781357227233));
#31380=CARTESIAN_POINT('Ctrl Pts',(40.0540580840903,31.7716647013005,48.2984384127022));
#31381=CARTESIAN_POINT('Ctrl Pts',(40.0452202372997,31.7673643840415,48.2180256065206));
#31382=CARTESIAN_POINT('Ctrl Pts',(40.0405236688884,31.7630640667825,48.1373385736929));
#31383=CARTESIAN_POINT('Ctrl Pts',(40.0378434669426,31.7606099944311,48.0912927113866));
#31384=CARTESIAN_POINT('Ctrl Pts',(40.036511003673,31.7581559220797,48.0451577207413));
#31385=CARTESIAN_POINT('Ctrl Pts',(40.0365302046386,31.7557018497283,47.9990164785296));
#31386=CARTESIAN_POINT('',(40.2639804386337,31.6997437308952,46.9881764997223));
#31387=CARTESIAN_POINT('Ctrl Pts',(40.036530204639,31.7557018496867,47.9990164777473));
#31388=CARTESIAN_POINT('Ctrl Pts',(40.0365663398342,31.7510834198396,47.912181185345));
#31389=CARTESIAN_POINT('Ctrl Pts',(40.0413922398844,31.7464649899924,47.8254998942774));
#31390=CARTESIAN_POINT('Ctrl Pts',(40.0509321358632,31.7418465601453,47.7394801148097));
#31391=CARTESIAN_POINT('Ctrl Pts',(40.0605002169713,31.737214485386,47.6532061943516));
#31392=CARTESIAN_POINT('Ctrl Pts',(40.0748100619829,31.7325824106267,47.5675980002164));
#31393=CARTESIAN_POINT('Ctrl Pts',(40.0937349511213,31.7279503358674,47.483151893473));
#31394=CARTESIAN_POINT('Ctrl Pts',(40.1127460894233,31.7232971506768,47.3983209281438));
#31395=CARTESIAN_POINT('Ctrl Pts',(40.1364142967733,31.7186439654861,47.3146629597844));
#31396=CARTESIAN_POINT('Ctrl Pts',(40.1645624236317,31.7139907802954,47.2326609073814));
#31397=CARTESIAN_POINT('Ctrl Pts',(40.1897788092404,31.7098222431609,47.1591997003714));
#31398=CARTESIAN_POINT('Ctrl Pts',(40.2185897699603,31.7056537060265,47.0870672898386));
#31399=CARTESIAN_POINT('Ctrl Pts',(40.2508364890358,31.701485168892,47.0165943644456));
#31400=CARTESIAN_POINT('Ctrl Pts',(40.2551818317863,31.700923445928,47.0070979249863));
#31401=CARTESIAN_POINT('Ctrl Pts',(40.2595901732973,31.700361722964,46.9976301622621));
#31402=CARTESIAN_POINT('Ctrl Pts',(40.2640612763241,31.6998,46.9881916141869));
#31403=CARTESIAN_POINT('',(40.03653,31.6998,48.));
#31404=CARTESIAN_POINT('Origin',(42.4,31.6998,48.));
#31405=CARTESIAN_POINT('',(40.3450946017473,31.6998,49.167627614067));
#31406=CARTESIAN_POINT('Origin',(42.4,31.6998,48.));
#31407=CARTESIAN_POINT('',(40.0365309987239,32.4282731502717,48.0021727647993));
#31408=CARTESIAN_POINT('Ctrl Pts',(40.3450946017473,31.6998,49.167627614067));
#31409=CARTESIAN_POINT('Ctrl Pts',(40.733984951581,31.7418752474686,49.8520349281576));
#31410=CARTESIAN_POINT('Ctrl Pts',(42.2432941503802,31.8260257424058,50.7894931656538));
#31411=CARTESIAN_POINT('Ctrl Pts',(44.6658134148021,31.9522514848118,49.6394916517794));
#31412=CARTESIAN_POINT('Ctrl Pts',(45.002413620778,32.0784772272174,46.9819641293264));
#31413=CARTESIAN_POINT('Ctrl Pts',(42.9528043529522,32.2047029696235,45.2602400010695));
#31414=CARTESIAN_POINT('Ctrl Pts',(40.5894215430047,32.3213015890215,45.9925773628642));
#31415=CARTESIAN_POINT('Ctrl Pts',(40.041973387172,32.3958249609508,47.3953266536232));
#31416=CARTESIAN_POINT('Ctrl Pts',(40.0363942808121,32.4282730854115,48.0021716774805));
#31417=CARTESIAN_POINT('',(40.0365301523602,33.2220231503183,47.9991513555514));
#31418=CARTESIAN_POINT('Ctrl Pts',(40.0365309987239,32.4282731502717,48.0021727647993));
#31419=CARTESIAN_POINT('Ctrl Pts',(40.0366288369523,32.433964126123,48.108598283094));
#31420=CARTESIAN_POINT('Ctrl Pts',(40.043918722001,32.4396551019744,48.2147058241217));
#31421=CARTESIAN_POINT('Ctrl Pts',(40.0582509534344,32.4453460778257,48.319690231019));
#31422=CARTESIAN_POINT('Ctrl Pts',(40.0681637458294,32.4492822033622,48.3923019966833));
#31423=CARTESIAN_POINT('Ctrl Pts',(40.0814443994366,32.4532183288986,48.4643771967112));
#31424=CARTESIAN_POINT('Ctrl Pts',(40.0980306723185,32.4571544544351,48.5356562846768));
#31425=CARTESIAN_POINT('Ctrl Pts',(40.115881679449,32.4613907168865,48.6123705360693));
#31426=CARTESIAN_POINT('Ctrl Pts',(40.1376054805314,32.4656269793378,48.6883366720028));
#31427=CARTESIAN_POINT('Ctrl Pts',(40.1631235815122,32.4698632417892,48.7631345420782));
#31428=CARTESIAN_POINT('Ctrl Pts',(40.1886047934042,32.4740933802793,48.8378242839952));
#31429=CARTESIAN_POINT('Ctrl Pts',(40.2178692624813,32.4783235187694,48.9113486735642));
#31430=CARTESIAN_POINT('Ctrl Pts',(40.2507878209739,32.4825536572596,48.9832992679881));
#31431=CARTESIAN_POINT('Ctrl Pts',(40.2836681061506,32.486778877508,49.0551662078426));
#31432=CARTESIAN_POINT('Ctrl Pts',(40.3201938439724,32.4910040977564,49.1254625643036));
#31433=CARTESIAN_POINT('Ctrl Pts',(40.3601870708306,32.4952293180048,49.1937979958491));
#31434=CARTESIAN_POINT('Ctrl Pts',(40.4001548439042,32.4994518491017,49.2620899351464));
#31435=CARTESIAN_POINT('Ctrl Pts',(40.4435854894103,32.5036743801987,49.3284230228211));
#31436=CARTESIAN_POINT('Ctrl Pts',(40.4902547835621,32.5078969112956,49.3924308417988));
#31437=CARTESIAN_POINT('Ctrl Pts',(40.5369089341258,32.5121180722353,49.4564178910594));
#31438=CARTESIAN_POINT('Ctrl Pts',(40.5867993703725,32.516339233175,49.5180807910649));
#31439=CARTESIAN_POINT('Ctrl Pts',(40.6396589950288,32.5205603941147,49.5770827458053));
#31440=CARTESIAN_POINT('Ctrl Pts',(40.6925179574176,32.5247815021683,49.6360839613222));
#31441=CARTESIAN_POINT('Ctrl Pts',(40.748345720209,32.5290026102219,49.6924239493138));
#31442=CARTESIAN_POINT('Ctrl Pts',(40.8068364142566,32.5332237182755,49.745800741769));
#31443=CARTESIAN_POINT('Ctrl Pts',(40.8653857410508,32.5374490576887,49.7992310406494));
#31444=CARTESIAN_POINT('Ctrl Pts',(40.9266029841594,32.5416743971019,49.8496918932931));
#31445=CARTESIAN_POINT('Ctrl Pts',(40.990147520111,32.5458997365151,49.8969202476253));
#31446=CARTESIAN_POINT('Ctrl Pts',(41.0537226611592,32.550127110988,49.9441713486551));
#31447=CARTESIAN_POINT('Ctrl Pts',(41.1196269373464,32.5543544854608,49.9881865889613));
#31448=CARTESIAN_POINT('Ctrl Pts',(41.1874910744808,32.5585818599337,50.0287465456376));
#31449=CARTESIAN_POINT('Ctrl Pts',(41.2554792674611,32.5628169620597,50.0693806460361));
#31450=CARTESIAN_POINT('Ctrl Pts',(41.3254340649262,32.5670520641858,50.1065466207299));
#31451=CARTESIAN_POINT('Ctrl Pts',(41.3969621315318,32.5712871663118,50.1400713715479));
#31452=CARTESIAN_POINT('Ctrl Pts',(41.4650432204419,32.5753181764882,50.1719805457984));
#31453=CARTESIAN_POINT('Ctrl Pts',(41.5345491053882,32.5793491866646,50.2005912390327));
#31454=CARTESIAN_POINT('Ctrl Pts',(41.6051276134198,32.583380196841,50.2257961114964));
#31455=CARTESIAN_POINT('Ctrl Pts',(41.679276065189,32.5876151002413,50.2522758759791));
#31456=CARTESIAN_POINT('Ctrl Pts',(41.7548904835065,32.5918500036415,50.2750968677632));
#31457=CARTESIAN_POINT('Ctrl Pts',(41.831575399182,32.5960849070417,50.2940976252298));
#31458=CARTESIAN_POINT('Ctrl Pts',(41.9081489701943,32.6003136614635,50.313070794051));
#31459=CARTESIAN_POINT('Ctrl Pts',(41.9857895001044,32.6045424158853,50.3282346316287));
#31460=CARTESIAN_POINT('Ctrl Pts',(42.0640839130019,32.6087711703071,50.3394766131329));
#31461=CARTESIAN_POINT('Ctrl Pts',(42.1422866868052,32.6129949752158,50.3507054365462));
#31462=CARTESIAN_POINT('Ctrl Pts',(42.2211413604342,32.6172187801245,50.3580214592381));
#31463=CARTESIAN_POINT('Ctrl Pts',(42.3002236499624,32.6214425850331,50.3613629794831));
#31464=CARTESIAN_POINT('Ctrl Pts',(42.3792552459753,32.6256636823884,50.3647023577389));
#31465=CARTESIAN_POINT('Ctrl Pts',(42.4585137004836,32.6298847797437,50.3640722704571));
#31466=CARTESIAN_POINT('Ctrl Pts',(42.5375697915496,32.634105877099,50.3594628611938));
#31467=CARTESIAN_POINT('Ctrl Pts',(42.6165999135277,32.6383255878686,50.3548549660727));
#31468=CARTESIAN_POINT('Ctrl Pts',(42.6954273357058,32.6425452986382,50.3462703718458));
#31469=CARTESIAN_POINT('Ctrl Pts',(42.7736245259,32.6467650094078,50.333751305205));
#31470=CARTESIAN_POINT('Ctrl Pts',(42.85182046785,32.650984652819,50.3212324384032));
#31471=CARTESIAN_POINT('Ctrl Pts',(42.9293857344215,32.6552042962303,50.3047792995598));
#31472=CARTESIAN_POINT('Ctrl Pts',(43.0059010863693,32.6594239396416,50.2844855688834));
#31473=CARTESIAN_POINT('Ctrl Pts',(43.0824929371117,32.6636478017831,50.2641715488677));
#31474=CARTESIAN_POINT('Ctrl Pts',(43.1580323214428,32.6678716639247,50.2400093872476));
#31475=CARTESIAN_POINT('Ctrl Pts',(43.2321139099739,32.6720955260663,50.2121430518228));
#31476=CARTESIAN_POINT('Ctrl Pts',(43.3062310277249,32.6763214139545,50.1842633518202));
#31477=CARTESIAN_POINT('Ctrl Pts',(43.3788885257198,32.6805473018427,50.1526761264666));
#31478=CARTESIAN_POINT('Ctrl Pts',(43.4497022551402,32.6847731897309,50.11757304867));
#31479=CARTESIAN_POINT('Ctrl Pts',(43.5206455067916,32.689006807002,50.082405765401));
#31480=CARTESIAN_POINT('Ctrl Pts',(43.5897378404033,32.6932404242731,50.0437100096986));
#31481=CARTESIAN_POINT('Ctrl Pts',(43.6566210405138,32.6974740415442,50.0017227583854));
#31482=CARTESIAN_POINT('Ctrl Pts',(43.7205081052318,32.7015180074451,49.9616163903057));
#31483=CARTESIAN_POINT('Ctrl Pts',(43.7823794542321,32.705561973346,49.9185073546962));
#31484=CARTESIAN_POINT('Ctrl Pts',(43.8419514606082,32.7096059392468,49.8726362236564));
#31485=CARTESIAN_POINT('Ctrl Pts',(43.9043469228363,32.7138415716684,49.8245909990908));
#31486=CARTESIAN_POINT('Ctrl Pts',(43.9644570313206,32.7180772040899,49.7733325933318));
#31487=CARTESIAN_POINT('Ctrl Pts',(44.0219320147086,32.7223128365114,49.7191064482933));
#31488=CARTESIAN_POINT('Ctrl Pts',(44.0793236902889,32.7265423295444,49.6649589019944));
#31489=CARTESIAN_POINT('Ctrl Pts',(44.1340874871881,32.7307718225775,49.6078524780488));
#31490=CARTESIAN_POINT('Ctrl Pts',(44.1859052814896,32.7350013156105,49.548073889208));
#31491=CARTESIAN_POINT('Ctrl Pts',(44.2376625711192,32.7392258701067,49.4883651004031));
#31492=CARTESIAN_POINT('Ctrl Pts',(44.2864803880359,32.7434504246028,49.4259906997908));
#31493=CARTESIAN_POINT('Ctrl Pts',(44.3320772999161,32.747674979099,49.3612743103611));
#31494=CARTESIAN_POINT('Ctrl Pts',(44.3776450568527,32.7518968323892,49.2965993009856));
#31495=CARTESIAN_POINT('Ctrl Pts',(44.4199957267821,32.7561186856795,49.2295856576005));
#31496=CARTESIAN_POINT('Ctrl Pts',(44.4588888182748,32.7603405389697,49.1605891929891));
#31497=CARTESIAN_POINT('Ctrl Pts',(44.4977691849325,32.7645610109764,49.0916153022743));
#31498=CARTESIAN_POINT('Ctrl Pts',(44.5331939891252,32.7687814829831,49.0206602870238));
#31499=CARTESIAN_POINT('Ctrl Pts',(44.5649674630409,32.7730019549899,48.9481067054264));
#31500=CARTESIAN_POINT('Ctrl Pts',(44.596740461947,32.777222363901,48.8755542084961));
#31501=CARTESIAN_POINT('Ctrl Pts',(44.6248620520384,32.7814427728122,48.8014036231594));
#31502=CARTESIAN_POINT('Ctrl Pts',(44.6491842294469,32.7856631817234,48.7260583605381));
#31503=CARTESIAN_POINT('Ctrl Pts',(44.6735307271568,32.7898878107179,48.650637758466));
#31504=CARTESIAN_POINT('Ctrl Pts',(44.6940700784421,32.7941124397125,48.5740205404645));
#31505=CARTESIAN_POINT('Ctrl Pts',(44.7107040998377,32.798337068707,48.4966256174355));
#31506=CARTESIAN_POINT('Ctrl Pts',(44.7273461052669,32.8025637254481,48.4191935462241));
#31507=CARTESIAN_POINT('Ctrl Pts',(44.7400789710655,32.8067903821892,48.3409834902103));
#31508=CARTESIAN_POINT('Ctrl Pts',(44.7488560940843,32.8110170389303,48.2624223507687));
#31509=CARTESIAN_POINT('Ctrl Pts',(44.7576492561023,32.815251419312,48.1837176515242));
#31510=CARTESIAN_POINT('Ctrl Pts',(44.7624722022754,32.8194857996937,48.1046610565485));
#31511=CARTESIAN_POINT('Ctrl Pts',(44.7633304609072,32.8237201800754,48.0256821620638));
#31512=CARTESIAN_POINT('Ctrl Pts',(44.7641487467668,32.8277573472679,47.9503816521985));
#31513=CARTESIAN_POINT('Ctrl Pts',(44.7613634749228,32.8317945144603,47.8751521212201));
#31514=CARTESIAN_POINT('Ctrl Pts',(44.7550232350933,32.8358316816527,47.8003603168944));
#31515=CARTESIAN_POINT('Ctrl Pts',(44.7483713953103,32.840067261073,47.7218927647446));
#31516=CARTESIAN_POINT('Ctrl Pts',(44.7377809076998,32.8443028404933,47.6436089492841));
#31517=CARTESIAN_POINT('Ctrl Pts',(44.7232689731068,32.8485384199136,47.5659358117754));
#31518=CARTESIAN_POINT('Ctrl Pts',(44.7087780695174,32.8527678610423,47.4883752398254));
#31519=CARTESIAN_POINT('Ctrl Pts',(44.6903770899501,32.856997302171,47.4114240458049));
#31520=CARTESIAN_POINT('Ctrl Pts',(44.6681350661798,32.8612267432998,47.3355048815335));
#31521=CARTESIAN_POINT('Ctrl Pts',(44.6459190033573,32.8654512478138,47.2596743303078));
#31522=CARTESIAN_POINT('Ctrl Pts',(44.6198709367108,32.8696757523279,47.1848738631517));
#31523=CARTESIAN_POINT('Ctrl Pts',(44.5901107904022,32.873900256842,47.1115152411751));
#31524=CARTESIAN_POINT('Ctrl Pts',(44.5603696647349,32.8781220613429,47.0382035049912));
#31525=CARTESIAN_POINT('Ctrl Pts',(44.5269213442865,32.8823438658438,46.9663322186796));
#31526=CARTESIAN_POINT('Ctrl Pts',(44.4899349742621,32.8865656703448,46.8962961247435));
#31527=CARTESIAN_POINT('Ctrl Pts',(44.4529606943075,32.8907860948262,46.82628292414));
#31528=CARTESIAN_POINT('Ctrl Pts',(44.412450880239,32.8950065193077,46.7581041394352));
#31529=CARTESIAN_POINT('Ctrl Pts',(44.3686213656833,32.8992269437891,46.6921313676537));
#31530=CARTESIAN_POINT('Ctrl Pts',(44.3247924925016,32.9034473065115,46.626159561277));
#31531=CARTESIAN_POINT('Ctrl Pts',(44.2776442762216,32.9076676692339,46.562394093839));
#31532=CARTESIAN_POINT('Ctrl Pts',(44.2274359277515,32.9118880319562,46.5011776720162));
#31533=CARTESIAN_POINT('Ctrl Pts',(44.1771773450496,32.916112617217,46.4399000022133));
#31534=CARTESIAN_POINT('Ctrl Pts',(44.1238528123531,32.9203372024778,46.3811768364409));
#31535=CARTESIAN_POINT('Ctrl Pts',(44.0677615282317,32.9245617877386,46.3253173656331));
#31536=CARTESIAN_POINT('Ctrl Pts',(44.0116433041987,32.9287884020125,46.2694310662505));
#31537=CARTESIAN_POINT('Ctrl Pts',(43.9527560308078,32.9330150162864,46.2164115162541));
#31538=CARTESIAN_POINT('Ctrl Pts',(43.8914335303496,32.9372416305604,46.1665288479366));
#31539=CARTESIAN_POINT('Ctrl Pts',(43.8299989312255,32.9414759711634,46.116554993178));
#31540=CARTESIAN_POINT('Ctrl Pts',(43.7661205891331,32.9457103117665,46.0697297567315));
#31541=CARTESIAN_POINT('Ctrl Pts',(43.7001627945513,32.9499446523695,46.0262808840758));
#31542=CARTESIAN_POINT('Ctrl Pts',(43.6372697507637,32.9539822429325,45.984850877694));
#31543=CARTESIAN_POINT('Ctrl Pts',(43.5724865318398,32.9580198334955,45.9464905883132));
#31544=CARTESIAN_POINT('Ctrl Pts',(43.5061479811823,32.9620574240585,45.9113575977142));
#31545=CARTESIAN_POINT('Ctrl Pts',(43.4365589853085,32.966292847809,45.8745031667144));
#31546=CARTESIAN_POINT('Ctrl Pts',(43.3649937905135,32.9705282715595,45.8410602963793));
#31547=CARTESIAN_POINT('Ctrl Pts',(43.2918207282089,32.97476369531,45.8112455072263));
#31548=CARTESIAN_POINT('Ctrl Pts',(43.2187537660668,32.9789929777411,45.7814739492006));
#31549=CARTESIAN_POINT('Ctrl Pts',(43.1440839971346,32.9832222601722,45.755320201202));
#31550=CARTESIAN_POINT('Ctrl Pts',(43.0682041896879,32.9874515426033,45.7329548743389));
#31551=CARTESIAN_POINT('Ctrl Pts',(42.9924130213608,32.9916758845913,45.7106156735686));
#31552=CARTESIAN_POINT('Ctrl Pts',(42.915415071303,32.9959002265793,45.6920562317595));
#31553=CARTESIAN_POINT('Ctrl Pts',(42.8376214845264,33.0001245685673,45.6773984678424));
#31554=CARTESIAN_POINT('Ctrl Pts',(42.7598776615587,33.0043462082843,45.6627500803558));
#31555=CARTESIAN_POINT('Ctrl Pts',(42.6813396720579,33.0085678480014,45.6519985036822));
#31556=CARTESIAN_POINT('Ctrl Pts',(42.6024309798725,33.0127894877185,45.6452150545564));
#31557=CARTESIAN_POINT('Ctrl Pts',(42.5235481202644,33.0170097453846,45.6384338261489));
#31558=CARTESIAN_POINT('Ctrl Pts',(42.4442952662404,33.0212300030507,45.6356181859657));
#31559=CARTESIAN_POINT('Ctrl Pts',(42.3651016770439,33.0254502607168,45.6367876633796));
#31560=CARTESIAN_POINT('Ctrl Pts',(42.2859092806767,33.0296704548166,45.6379571231786));
#31561=CARTESIAN_POINT('Ctrl Pts',(42.2067766166628,33.0338906489163,45.6431115729954));
#31562=CARTESIAN_POINT('Ctrl Pts',(42.128132116221,33.0381108430161,45.6522184312271));
#31563=CARTESIAN_POINT('Ctrl Pts',(42.0494089588806,33.0423352579752,45.6613343977528));
#31564=CARTESIAN_POINT('Ctrl Pts',(41.9711754078042,33.0465596729344,45.6744106152543));
#31565=CARTESIAN_POINT('Ctrl Pts',(41.8938533417299,33.0507840878936,45.6913627393586));
#31566=CARTESIAN_POINT('Ctrl Pts',(41.8164941592577,33.0550105306706,45.7083230008784));
#31567=CARTESIAN_POINT('Ctrl Pts',(41.740047786877,33.0592369734476,45.7291627517744));
#31568=CARTESIAN_POINT('Ctrl Pts',(41.6649219867698,33.0634634162246,45.753747397249));
#31569=CARTESIAN_POINT('Ctrl Pts',(41.5896588498976,33.0676975853218,45.7783769856817));
#31570=CARTESIAN_POINT('Ctrl Pts',(41.5157215486243,33.0719317544189,45.806764979937));
#31571=CARTESIAN_POINT('Ctrl Pts',(41.4434986810422,33.076165923516,45.8387282290901));
#31572=CARTESIAN_POINT('Ctrl Pts',(41.3746034611575,33.0802050044988,45.8692187807998));
#31573=CARTESIAN_POINT('Ctrl Pts',(41.3072684728443,33.0842440854816,45.9029621911566));
#31574=CARTESIAN_POINT('Ctrl Pts',(41.2418077577091,33.0882831664644,45.9397618655124));
#31575=CARTESIAN_POINT('Ctrl Pts',(41.1731633574778,33.0925186883492,45.978351293838));
#31576=CARTESIAN_POINT('Ctrl Pts',(41.1063192262536,33.096754210234,46.0204485310013));
#31577=CARTESIAN_POINT('Ctrl Pts',(41.0416567358416,33.1009897321188,46.0658609104784));
#31578=CARTESIAN_POINT('Ctrl Pts',(40.9770879822644,33.1052191140543,46.1112074587033));
#31579=CARTESIAN_POINT('Ctrl Pts',(40.9146949700175,33.1094484959898,46.1598593384299));
#31580=CARTESIAN_POINT('Ctrl Pts',(40.854833677621,33.1136778779252,46.211578495688));
#31581=CARTESIAN_POINT('Ctrl Pts',(40.7950422880421,33.1179023210145,46.2632372580786));
#31582=CARTESIAN_POINT('Ctrl Pts',(40.7377770966868,33.1221267641038,46.3179558750393));
#31583=CARTESIAN_POINT('Ctrl Pts',(40.6833630704725,33.1263512071931,46.3754544964568));
#31584=CARTESIAN_POINT('Ctrl Pts',(40.6289838396155,33.1305729489384,46.4329163500551));
#31585=CARTESIAN_POINT('Ctrl Pts',(40.5774524769848,33.1347946906836,46.4931543398004));
#31586=CARTESIAN_POINT('Ctrl Pts',(40.5290580545538,33.1390164324288,46.5558508810826));
#31587=CARTESIAN_POINT('Ctrl Pts',(40.4806794657617,33.1432367929088,46.6185269093729));
#31588=CARTESIAN_POINT('Ctrl Pts',(40.4354360657627,33.1474571533888,46.6836595206978));
#31589=CARTESIAN_POINT('Ctrl Pts',(40.3935765061138,33.1516775138687,46.7508982411022));
#31590=CARTESIAN_POINT('Ctrl Pts',(40.3517175705451,33.1558978114278,46.8181359590511));
#31591=CARTESIAN_POINT('Ctrl Pts',(40.3132426219625,33.1601181089868,46.8874793245161));
#31592=CARTESIAN_POINT('Ctrl Pts',(40.278356036486,33.1643384065458,46.9585503694444));
#31593=CARTESIAN_POINT('Ctrl Pts',(40.2434345573606,33.1685629252569,47.0296924998073));
#31594=CARTESIAN_POINT('Ctrl Pts',(40.2121088183092,33.1727874439679,47.1025653392601));
#31595=CARTESIAN_POINT('Ctrl Pts',(40.1845361162486,33.177011962679,47.17676842827));
#31596=CARTESIAN_POINT('Ctrl Pts',(40.1569501768173,33.181238509538,47.2510071414195));
#31597=CARTESIAN_POINT('Ctrl Pts',(40.1331210051139,33.185465056397,47.3265769281391));
#31598=CARTESIAN_POINT('Ctrl Pts',(40.1131559989364,33.1896916032561,47.4030620168732));
#31599=CARTESIAN_POINT('Ctrl Pts',(40.0931544990082,33.19392587576,47.4796869116126));
#31600=CARTESIAN_POINT('Ctrl Pts',(40.0770313744407,33.1981601482639,47.5572299908215));
#31601=CARTESIAN_POINT('Ctrl Pts',(40.0648428182954,33.2023944207678,47.6352653325588));
#31602=CARTESIAN_POINT('Ctrl Pts',(40.0532187736082,33.2064325834686,47.7096864771737));
#31603=CARTESIAN_POINT('Ctrl Pts',(40.0451729101829,33.2104707461694,47.7845549367905));
#31604=CARTESIAN_POINT('Ctrl Pts',(40.0407097821507,33.2145089088703,47.8595005022767));
#31605=CARTESIAN_POINT('Ctrl Pts',(40.0379414421964,33.2170136560041,47.9059869131148));
#31606=CARTESIAN_POINT('Ctrl Pts',(40.0365468832596,33.2195184031379,47.9525559457422));
#31607=CARTESIAN_POINT('Ctrl Pts',(40.0365301523605,33.2220231502717,47.9991513546838));
#31608=CARTESIAN_POINT('',(40.0365306333283,34.0157731502431,47.9982697675646));
#31609=CARTESIAN_POINT('Ctrl Pts',(40.0365301523602,33.2220231503183,47.9991513555514));
#31610=CARTESIAN_POINT('Ctrl Pts',(40.0365021154589,33.2262204991601,48.0772339624199));
#31611=CARTESIAN_POINT('Ctrl Pts',(40.0403477846679,33.2304178480019,48.1554743222026));
#31612=CARTESIAN_POINT('Ctrl Pts',(40.0480878668836,33.2346151968436,48.2334518344325));
#31613=CARTESIAN_POINT('Ctrl Pts',(40.0558171140975,33.2388066700007,48.3113201893608));
#31614=CARTESIAN_POINT('Ctrl Pts',(40.0674299063109,33.2429981431578,48.3889259549904));
#31615=CARTESIAN_POINT('Ctrl Pts',(40.0828949330752,33.2471896163149,48.4658482046025));
#31616=CARTESIAN_POINT('Ctrl Pts',(40.0983433617521,33.2513765909064,48.5426878961793));
#31617=CARTESIAN_POINT('Ctrl Pts',(40.1176357195175,33.2555635654978,48.6188450619448));
#31618=CARTESIAN_POINT('Ctrl Pts',(40.1406890375124,33.2597505400893,48.6939051921432));
#31619=CARTESIAN_POINT('Ctrl Pts',(40.1637293049397,33.2639351444191,48.7689228305275));
#31620=CARTESIAN_POINT('Ctrl Pts',(40.1905261684422,33.2681197487489,48.8428442090526));
#31621=CARTESIAN_POINT('Ctrl Pts',(40.220946176901,33.2723043530788,48.9152676531692));
#31622=CARTESIAN_POINT('Ctrl Pts',(40.251358878258,33.276487952237,48.9876737006605));
#31623=CARTESIAN_POINT('Ctrl Pts',(40.2853928113643,33.2806715513951,49.0585820871903));
#31624=CARTESIAN_POINT('Ctrl Pts',(40.3228661062038,33.2848551505533,49.1276104061878));
#31625=CARTESIAN_POINT('Ctrl Pts',(40.3603426120758,33.2890391081981,49.1966446401223));
#31626=CARTESIAN_POINT('Ctrl Pts',(40.4012588342473,33.2932230658428,49.2637980674233));
#31627=CARTESIAN_POINT('Ctrl Pts',(40.445387385082,33.2974070234876,49.3287136510563));
#31628=CARTESIAN_POINT('Ctrl Pts',(40.4895621377561,33.3015953616646,49.3936972001973));
#31629=CARTESIAN_POINT('Ctrl Pts',(40.5369556607667,33.3057836998416,49.4564378340769));
#31630=CARTESIAN_POINT('Ctrl Pts',(40.5872982097622,33.3099720380185,49.5166089346198));
#31631=CARTESIAN_POINT('Ctrl Pts',(40.6376707183786,33.3141628687396,49.576815843905));
#31632=CARTESIAN_POINT('Ctrl Pts',(40.6909954190013,33.3183536994607,49.6344498273763));
#31633=CARTESIAN_POINT('Ctrl Pts',(40.7469651827797,33.3225445301818,49.6892206291534));
#31634=CARTESIAN_POINT('Ctrl Pts',(40.8030277856186,33.3267423123846,49.7440822812297));
#31635=CARTESIAN_POINT('Ctrl Pts',(40.8617438479482,33.3309400945874,49.7960709592963));
#31636=CARTESIAN_POINT('Ctrl Pts',(40.922773184784,33.3351378767901,49.8449366865307));
#31637=CARTESIAN_POINT('Ctrl Pts',(40.9498960335329,33.3370034682855,49.8666537458582));
#31638=CARTESIAN_POINT('Ctrl Pts',(40.9774754008023,33.3388690597808,49.8877545615961));
#31639=CARTESIAN_POINT('Ctrl Pts',(41.005479749451,33.3407346512761,49.9082200375504));
#31640=CARTESIAN_POINT('Ctrl Pts',(41.069058596954,33.3449701419377,49.9546832276463));
#31641=CARTESIAN_POINT('Ctrl Pts',(41.1350829584756,33.3492056325992,49.9980537394834));
#31642=CARTESIAN_POINT('Ctrl Pts',(41.2032193813288,33.3534411232608,50.0380644228466));
#31643=CARTESIAN_POINT('Ctrl Pts',(41.2712570252651,33.3576704736355,50.078017101815));
#31644=CARTESIAN_POINT('Ctrl Pts',(41.341400248826,33.3618998240102,50.114619389241));
#31645=CARTESIAN_POINT('Ctrl Pts',(41.4132848266376,33.366129174385,50.1476460619842));
#31646=CARTESIAN_POINT('Ctrl Pts',(41.4850854547547,33.3703535855546,50.1806341648538));
#31647=CARTESIAN_POINT('Ctrl Pts',(41.5586229716564,33.3745779967243,50.2100547560943));
#31648=CARTESIAN_POINT('Ctrl Pts',(41.6335079770185,33.3788024078939,50.2357281631732));
#31649=CARTESIAN_POINT('Ctrl Pts',(41.7083450927587,33.3830241175153,50.2613851518817));
#31650=CARTESIAN_POINT('Ctrl Pts',(41.7845275438216,33.3872458271367,50.2832995608808));
#31651=CARTESIAN_POINT('Ctrl Pts',(41.8616464758864,33.3914675367582,50.3013400278913));
#31652=CARTESIAN_POINT('Ctrl Pts',(41.9387401731499,33.3956878649548,50.3193745917131));
#31653=CARTESIAN_POINT('Ctrl Pts',(42.0167692862679,33.3999081931514,50.3335376238067));
#31654=CARTESIAN_POINT('Ctrl Pts',(42.0953117925022,33.4041285213481,50.3437481812498));
#31655=CARTESIAN_POINT('Ctrl Pts',(42.1738531256036,33.4083487865087,50.3539585861852));
#31656=CARTESIAN_POINT('Ctrl Pts',(42.2529073709692,33.4125690516694,50.3602165746351));
#31657=CARTESIAN_POINT('Ctrl Pts',(42.3320458456057,33.41678931683,50.3624928939154));
#31658=CARTESIAN_POINT('Ctrl Pts',(42.411263476228,33.4210138031896,50.3647714900186));
#31659=CARTESIAN_POINT('Ctrl Pts',(42.4905650341362,33.4252382895492,50.3630604477787));
#31660=CARTESIAN_POINT('Ctrl Pts',(42.5695208910285,33.4294627759089,50.3573826817903));
#31661=CARTESIAN_POINT('Ctrl Pts',(42.6485146535901,33.4336892903889,50.3517021899811));
#31662=CARTESIAN_POINT('Ctrl Pts',(42.7271619180104,33.4379158048689,50.3420512379268));
#31663=CARTESIAN_POINT('Ctrl Pts',(42.8050398132651,33.4421423193489,50.3285044965751));
#31664=CARTESIAN_POINT('Ctrl Pts',(42.8830600677609,33.4463765598132,50.31493299205));
#31665=CARTESIAN_POINT('Ctrl Pts',(42.9603076838087,33.4506108002775,50.2974515718185));
#31666=CARTESIAN_POINT('Ctrl Pts',(43.0363717860428,33.4548450407418,50.276185710971));
#31667=CARTESIAN_POINT('Ctrl Pts',(43.1089187164316,33.4588834917218,50.255903174515));
#31668=CARTESIAN_POINT('Ctrl Pts',(43.1803888367674,33.4629219427019,50.232178591211));
#31669=CARTESIAN_POINT('Ctrl Pts',(43.250443301507,33.4669603936819,50.2051613618559));
#31670=CARTESIAN_POINT('Ctrl Pts',(43.3239160109902,33.4711958972536,50.1768258510382));
#31671=CARTESIAN_POINT('Ctrl Pts',(43.3961106755326,33.4754314008253,50.1447604597992));
#31672=CARTESIAN_POINT('Ctrl Pts',(43.4666222177561,33.479666904397,50.1091011084083));
#31673=CARTESIAN_POINT('Ctrl Pts',(43.5370315412657,33.4838962678714,50.0734934514339));
#31674=CARTESIAN_POINT('Ctrl Pts',(43.6057621725277,33.4881256313459,50.0343023906085));
#31675=CARTESIAN_POINT('Ctrl Pts',(43.6724276485817,33.4923549948203,49.991712408965));
#31676=CARTESIAN_POINT('Ctrl Pts',(43.7390152737942,33.496579419314,49.9491721631983));
#31677=CARTESIAN_POINT('Ctrl Pts',(43.8035421427342,33.5008038438076,49.9032411355331));
#31678=CARTESIAN_POINT('Ctrl Pts',(43.8656464826084,33.5050282683013,49.8541496241991));
#31679=CARTESIAN_POINT('Ctrl Pts',(43.9277111082535,33.5092499913772,49.8050895057038));
#31680=CARTESIAN_POINT('Ctrl Pts',(43.98735591235,33.5134717144532,49.7528732051682));
#31681=CARTESIAN_POINT('Ctrl Pts',(44.0442492281593,33.5176934375292,49.6977735174627));
#31682=CARTESIAN_POINT('Ctrl Pts',(44.101123928947,33.5219137792923,49.6426918579185));
#31683=CARTESIAN_POINT('Ctrl Pts',(44.1552485921758,33.5261341210555,49.5847290108015));
#31684=CARTESIAN_POINT('Ctrl Pts',(44.2063268313671,33.5303544628186,49.5241961222832));
#31685=CARTESIAN_POINT('Ctrl Pts',(44.2574043087735,33.5345747416393,49.4636641365573));
#31686=CARTESIAN_POINT('Ctrl Pts',(44.3054351507928,33.5387950204599,49.4005625451917));
#31687=CARTESIAN_POINT('Ctrl Pts',(44.3501628408623,33.5430152992805,49.3352360596613));
#31688=CARTESIAN_POINT('Ctrl Pts',(44.3949352689227,33.5472397993519,49.2698442326006));
#31689=CARTESIAN_POINT('Ctrl Pts',(44.4363976792592,33.5514642994233,49.202223454044));
#31690=CARTESIAN_POINT('Ctrl Pts',(44.4743369181271,33.5556887994947,49.1327474524338));
#31691=CARTESIAN_POINT('Ctrl Pts',(44.5122943715217,33.5599153277372,49.0632380955816));
#31692=CARTESIAN_POINT('Ctrl Pts',(44.5467250796167,33.5641418559798,48.9918721646229));
#31693=CARTESIAN_POINT('Ctrl Pts',(44.5774630728789,33.5683683842223,48.9190457046027));
#31694=CARTESIAN_POINT('Ctrl Pts',(44.6082572538374,33.5726026383721,48.8460861210251));
#31695=CARTESIAN_POINT('Ctrl Pts',(44.6353450706936,33.5768368925219,48.7716611157403));
#31696=CARTESIAN_POINT('Ctrl Pts',(44.6586097711944,33.5810711466717,48.6961841296418));
#31697=CARTESIAN_POINT('Ctrl Pts',(44.6807979843064,33.585109476477,48.6241995600339));
#31698=CARTESIAN_POINT('Ctrl Pts',(44.6995090032818,33.5891478062824,48.5512585643751));
#31699=CARTESIAN_POINT('Ctrl Pts',(44.7146851706425,33.5931861360878,48.4777269112241));
#31700=CARTESIAN_POINT('Ctrl Pts',(44.7306023130197,33.5974216369854,48.4006050816728));
#31701=CARTESIAN_POINT('Ctrl Pts',(44.7426911152079,33.601657137883,48.3225402899882));
#31702=CARTESIAN_POINT('Ctrl Pts',(44.750846746316,33.6058926387806,48.2439467487705));
#31703=CARTESIAN_POINT('Ctrl Pts',(44.7589905543899,33.6101219995683,48.1654671428329));
#31704=CARTESIAN_POINT('Ctrl Pts',(44.763212466175,33.6143513603559,48.086460772424));
#31705=CARTESIAN_POINT('Ctrl Pts',(44.7634585636582,33.6185807211436,48.0073524669862));
#31706=CARTESIAN_POINT('Ctrl Pts',(44.7637043737522,33.6228051429444,47.9283365430936));
#31707=CARTESIAN_POINT('Ctrl Pts',(44.7599835943962,33.6270295647452,47.8492193876342));
#31708=CARTESIAN_POINT('Ctrl Pts',(44.7522941966099,33.631253986546,47.7704298505999));
#31709=CARTESIAN_POINT('Ctrl Pts',(44.7446097160159,33.6354757069265,47.6916906976552));
#31710=CARTESIAN_POINT('Ctrl Pts',(44.7329616995274,33.6396974273071,47.6132792131841));
#31711=CARTESIAN_POINT('Ctrl Pts',(44.7174001461527,33.6439191476877,47.5356219174944));
#31712=CARTESIAN_POINT('Ctrl Pts',(44.7018436843879,33.6481394867567,47.4579900306215));
#31713=CARTESIAN_POINT('Ctrl Pts',(44.6823763204877,33.6523598258258,47.3811123023922));
#31714=CARTESIAN_POINT('Ctrl Pts',(44.6590993943052,33.6565801648948,47.3054063291752));
#31715=CARTESIAN_POINT('Ctrl Pts',(44.635822815249,33.6608004410264,47.2297014849533));
#31716=CARTESIAN_POINT('Ctrl Pts',(44.6087369260511,33.665020717158,47.1551688092414));
#31717=CARTESIAN_POINT('Ctrl Pts',(44.5779928652158,33.6692409932895,47.0822105252461));
#31718=CARTESIAN_POINT('Ctrl Pts',(44.5472180530222,33.673465490699,47.0091792656491));
#31719=CARTESIAN_POINT('Ctrl Pts',(44.5127779424928,33.6776899881084,46.9377259771127));
#31720=CARTESIAN_POINT('Ctrl Pts',(44.4748715351361,33.6819144855179,46.8682321114372));
#31721=CARTESIAN_POINT('Ctrl Pts',(44.4369469289101,33.6861410111089,46.7987048817509));
#31722=CARTESIAN_POINT('Ctrl Pts',(44.3955529561559,33.6903675366999,46.7311393497179));
#31723=CARTESIAN_POINT('Ctrl Pts',(44.3509329135256,33.6945940622909,46.6658893569787));
#31724=CARTESIAN_POINT('Ctrl Pts',(44.3062313068501,33.6988283138388,46.6005200892895));
#31725=CARTESIAN_POINT('Ctrl Pts',(44.2582921312371,33.7030625653866,46.5374751934799));
#31726=CARTESIAN_POINT('Ctrl Pts',(44.2073999398629,33.7072968169345,46.4770765290785));
#31727=CARTESIAN_POINT('Ctrl Pts',(44.1588622762872,33.7113351707875,46.4194722095557));
#31728=CARTESIAN_POINT('Ctrl Pts',(44.107639066577,33.7153735246406,46.3642749174909));
#31729=CARTESIAN_POINT('Ctrl Pts',(44.0540067454563,33.7194118784936,46.3117310264993));
#31730=CARTESIAN_POINT('Ctrl Pts',(43.9977561900654,33.7236473775798,46.2566220364553));
#31731=CARTESIAN_POINT('Ctrl Pts',(43.9386414792717,33.7278828766661,46.2042226495555));
#31732=CARTESIAN_POINT('Ctrl Pts',(43.8769542643098,33.7321183757523,46.1548451170601));
#31733=CARTESIAN_POINT('Ctrl Pts',(43.8153564765458,33.7363477346875,46.1055391665671));
#31734=CARTESIAN_POINT('Ctrl Pts',(43.7511939537218,33.7405770936227,46.0592466619137));
#31735=CARTESIAN_POINT('Ctrl Pts',(43.6847948196123,33.7448064525579,46.016242778867));
#31736=CARTESIAN_POINT('Ctrl Pts',(43.6184732263326,33.7490308724528,45.9732891157038));
#31737=CARTESIAN_POINT('Ctrl Pts',(43.5499206040223,33.7532552923477,45.9336166962783));
#31738=CARTESIAN_POINT('Ctrl Pts',(43.4794965294163,33.7574797122426,45.8974592313398));
#31739=CARTESIAN_POINT('Ctrl Pts',(43.4091174899281,33.7617014306856,45.8613248885467));
#31740=CARTESIAN_POINT('Ctrl Pts',(43.3368697898738,33.7659231491286,45.8287012527122));
#31741=CARTESIAN_POINT('Ctrl Pts',(43.2631391934012,33.7701448675717,45.7997770172742));
#31742=CARTESIAN_POINT('Ctrl Pts',(43.1894327214801,33.7743652046741,45.770862245807));
#31743=CARTESIAN_POINT('Ctrl Pts',(43.1142447531929,33.7785855417766,45.7456446424839));
#31744=CARTESIAN_POINT('Ctrl Pts',(43.0379813224048,33.782805878879,45.7242648938941));
#31745=CARTESIAN_POINT('Ctrl Pts',(42.9617190294029,33.7870261530176,45.7028854642723));
#31746=CARTESIAN_POINT('Ctrl Pts',(42.8843817580829,33.7912464271562,45.6853439009779));
#31747=CARTESIAN_POINT('Ctrl Pts',(42.8063895537328,33.7954667012948,45.6717306917977));
#31748=CARTESIAN_POINT('Ctrl Pts',(42.7283193391435,33.7996911966834,45.6581038662604));
#31749=CARTESIAN_POINT('Ctrl Pts',(42.6495933463761,33.803915692072,45.6484133249306));
#31750=CARTESIAN_POINT('Ctrl Pts',(42.5706400448906,33.8081401874606,45.642698064316));
#31751=CARTESIAN_POINT('Ctrl Pts',(42.4916488382462,33.8123667110122,45.636980059828));
#31752=CARTESIAN_POINT('Ctrl Pts',(42.412430575367,33.8165932345639,45.6352411483672));
#31753=CARTESIAN_POINT('Ctrl Pts',(42.3334144681154,33.8208197581155,45.637468136121));
#31754=CARTESIAN_POINT('Ctrl Pts',(42.254253921957,33.8250540076165,45.6396991947369));
#31755=CARTESIAN_POINT('Ctrl Pts',(42.1752967389788,33.8292882571175,45.645910601936));
#31756=CARTESIAN_POINT('Ctrl Pts',(42.0969675526403,33.8335225066185,45.6560371639578));
#31757=CARTESIAN_POINT('Ctrl Pts',(42.0222619057637,33.8375608780455,45.6656952671736));
#31758=CARTESIAN_POINT('Ctrl Pts',(41.9481277827892,33.8415992494725,45.6789142031845));
#31759=CARTESIAN_POINT('Ctrl Pts',(41.8749219445824,33.8456376208995,45.6955947672732));
#31760=CARTESIAN_POINT('Ctrl Pts',(41.7981426318956,33.8498731216483,45.7130895774868));
#31761=CARTESIAN_POINT('Ctrl Pts',(41.72209268972,33.8541086223971,45.7344590981521));
#31762=CARTESIAN_POINT('Ctrl Pts',(41.6471925112131,33.8583441231458,45.7596269672828));
#31763=CARTESIAN_POINT('Ctrl Pts',(41.5724009140803,33.8625734837691,45.784758351029));
#31764=CARTESIAN_POINT('Ctrl Pts',(41.4987562118072,33.8668028443925,45.8136770002822));
#31765=CARTESIAN_POINT('Ctrl Pts',(41.4266673473084,33.8710322050158,45.8462558211096));
#31766=CARTESIAN_POINT('Ctrl Pts',(41.3546626675442,33.8752566266294,45.8787965966799));
#31767=CARTESIAN_POINT('Ctrl Pts',(41.2842106405299,33.879481048243,45.9149888576775));
#31768=CARTESIAN_POINT('Ctrl Pts',(41.2157023516839,33.8837054698566,45.9546566251378));
#31769=CARTESIAN_POINT('Ctrl Pts',(41.1472378725322,33.8879271900363,45.9942990258461));
#31770=CARTESIAN_POINT('Ctrl Pts',(41.0807150695741,33.8921489102159,46.0374122872457));
#31771=CARTESIAN_POINT('Ctrl Pts',(41.0165013345407,33.8963706303955,46.0837740520564));
#31772=CARTESIAN_POINT('Ctrl Pts',(40.9523086099107,33.9005909692501,46.1301206475365));
#31773=CARTESIAN_POINT('Ctrl Pts',(40.8904238332502,33.9048113081046,46.1797133613383));
#31774=CARTESIAN_POINT('Ctrl Pts',(40.8311849869034,33.9090316469591,46.2322868175005));
#31775=CARTESIAN_POINT('Ctrl Pts',(40.771947024166,33.9132519228629,46.2848594894745));
#31776=CARTESIAN_POINT('Ctrl Pts',(40.715355263448,33.9174721987667,46.3404125028882));
#31777=CARTESIAN_POINT('Ctrl Pts',(40.6617130485338,33.9216924746704,46.3986415406716));
#31778=CARTESIAN_POINT('Ctrl Pts',(40.6080171789178,33.9259169718325,46.4569288210476));
#31779=CARTESIAN_POINT('Ctrl Pts',(40.5572770673334,33.9301414689946,46.5178971267101));
#31780=CARTESIAN_POINT('Ctrl Pts',(40.5097573093474,33.9343659661566,46.5812071992943));
#31781=CARTESIAN_POINT('Ctrl Pts',(40.4622147372448,33.9385924914892,46.6445476668856));
#31782=CARTESIAN_POINT('Ctrl Pts',(40.4178958616058,33.9428190168218,46.7102317514898));
#31783=CARTESIAN_POINT('Ctrl Pts',(40.3770217860997,33.9470455421544,46.7778913358524));
#31784=CARTESIAN_POINT('Ctrl Pts',(40.3360729942093,33.9512797934278,46.8456745995751));
#31785=CARTESIAN_POINT('Ctrl Pts',(40.298581808044,33.9555140447013,46.9154401644476));
#31786=CARTESIAN_POINT('Ctrl Pts',(40.2647231209757,33.9597482959747,46.9867956322616));
#31787=CARTESIAN_POINT('Ctrl Pts',(40.2324308889635,33.9637866517516,47.0548498753969));
#31788=CARTESIAN_POINT('Ctrl Pts',(40.2034425813174,33.9678250075285,47.1243498189802));
#31789=CARTESIAN_POINT('Ctrl Pts',(40.177867767415,33.9718633633054,47.194941752538));
#31790=CARTESIAN_POINT('Ctrl Pts',(40.1467834353712,33.9767716919587,47.2807411296398));
#31791=CARTESIAN_POINT('Ctrl Pts',(40.1206435182197,33.981680020612,47.3684219008596));
#31792=CARTESIAN_POINT('Ctrl Pts',(40.0996463022741,33.9865883492653,47.4574474161349));
#31793=CARTESIAN_POINT('Ctrl Pts',(40.0788348930446,33.9914532435684,47.5456851346521));
#31794=CARTESIAN_POINT('Ctrl Pts',(40.0630756547469,33.9963181378716,47.6352437461937));
#31795=CARTESIAN_POINT('Ctrl Pts',(40.0525154170653,34.0011830321747,47.7255795674808));
#31796=CARTESIAN_POINT('Ctrl Pts',(40.0419584823543,34.0060464048642,47.8158871340487));
#31797=CARTESIAN_POINT('Ctrl Pts',(40.0365974704945,34.0109097775536,47.906971285491));
#31798=CARTESIAN_POINT('Ctrl Pts',(40.0365306333283,34.0157731502431,47.9982697675646));
#31799=CARTESIAN_POINT('',(40.0365305376038,34.8095231503011,48.0015941206072));
#31800=CARTESIAN_POINT('Ctrl Pts',(40.0365306333279,34.0157731502717,47.9982697681018));
#31801=CARTESIAN_POINT('Ctrl Pts',(40.0364725206114,34.020001694087,48.0776508183265));
#31802=CARTESIAN_POINT('Ctrl Pts',(40.0404179459887,34.0242302379023,48.1570685937256));
#31803=CARTESIAN_POINT('Ctrl Pts',(40.048351385374,34.0284587817177,48.2360915801712));
#31804=CARTESIAN_POINT('Ctrl Pts',(40.0562842671246,34.0326870283122,48.3151090121576));
#31805=CARTESIAN_POINT('Ctrl Pts',(40.0682045589376,34.0369152749067,48.3937312464129));
#31806=CARTESIAN_POINT('Ctrl Pts',(40.0840448505842,34.0411435215013,48.471531745267));
#31807=CARTESIAN_POINT('Ctrl Pts',(40.0998888941178,34.0453727695864,48.5493506717282));
#31808=CARTESIAN_POINT('Ctrl Pts',(40.1196546870358,34.0496020176715,48.6263470196808));
#31809=CARTESIAN_POINT('Ctrl Pts',(40.1432239853927,34.0538312657566,48.702105733343));
#31810=CARTESIAN_POINT('Ctrl Pts',(40.1668223317924,34.0580657261895,48.7779578160282));
#31811=CARTESIAN_POINT('Ctrl Pts',(40.1942334000401,34.0623001866224,48.8525687743477));
#31812=CARTESIAN_POINT('Ctrl Pts',(40.225289637487,34.0665346470552,48.9255405340008));
#31813=CARTESIAN_POINT('Ctrl Pts',(40.2563674008764,34.0707720425105,48.9985628724116));
#31814=CARTESIAN_POINT('Ctrl Pts',(40.2910951577676,34.0750094379658,49.0699433321022));
#31815=CARTESIAN_POINT('Ctrl Pts',(40.32925907647,34.079246833421,49.1393078901325));
#31816=CARTESIAN_POINT('Ctrl Pts',(40.367491204594,34.0834918022677,49.20879642171));
#31817=CARTESIAN_POINT('Ctrl Pts',(40.4091715081891,34.0877367711143,49.2762614638197));
#31818=CARTESIAN_POINT('Ctrl Pts',(40.4540427571723,34.0919817399609,49.3413578381575));
#31819=CARTESIAN_POINT('Ctrl Pts',(40.4755619672545,34.0940175285443,49.372576549174));
#31820=CARTESIAN_POINT('Ctrl Pts',(40.4978144785519,34.0960533171277,49.4032509714174));
#31821=CARTESIAN_POINT('Ctrl Pts',(40.5207687907589,34.0980891057111,49.4333459118839));
#31822=CARTESIAN_POINT('Ctrl Pts',(40.5685257106106,34.1023246058357,49.4959590560652));
#31823=CARTESIAN_POINT('Ctrl Pts',(40.6195060929958,34.1065601059603,49.5563018166407));
#31824=CARTESIAN_POINT('Ctrl Pts',(40.6734661316249,34.1107956060848,49.6140233090801));
#31825=CARTESIAN_POINT('Ctrl Pts',(40.7273479452908,34.1150249660759,49.6716611236397));
#31826=CARTESIAN_POINT('Ctrl Pts',(40.784200519511,34.119254326067,49.7266848762439));
#31827=CARTESIAN_POINT('Ctrl Pts',(40.8437386309448,34.1234836860581,49.778775138146));
#31828=CARTESIAN_POINT('Ctrl Pts',(40.9032072141622,34.1277081070302,49.8308045693816));
#31829=CARTESIAN_POINT('Ctrl Pts',(40.9653547510696,34.1319325280024,49.8799070099948));
#31830=CARTESIAN_POINT('Ctrl Pts',(41.0298589387366,34.1361569489746,49.9257995516512));
#31831=CARTESIAN_POINT('Ctrl Pts',(41.0943218771653,34.1403786685075,49.9716627458737));
#31832=CARTESIAN_POINT('Ctrl Pts',(41.1611380938088,34.1446003880404,50.0143198438972));
#31833=CARTESIAN_POINT('Ctrl Pts',(41.2299529072174,34.1488221075733,50.0535287291808));
#31834=CARTESIAN_POINT('Ctrl Pts',(41.2987452046983,34.1530424457766,50.0927247854763));
#31835=CARTESIAN_POINT('Ctrl Pts',(41.3695343929576,34.15726278398,50.1284746371659));
#31836=CARTESIAN_POINT('Ctrl Pts',(41.4419388392728,34.1614831221834,50.1605807675729));
#31837=CARTESIAN_POINT('Ctrl Pts',(41.5143422055393,34.1657033974325,50.1926864190565));
#31838=CARTESIAN_POINT('Ctrl Pts',(41.5883603523654,34.1699236726816,50.2211482682615));
#31839=CARTESIAN_POINT('Ctrl Pts',(41.6635905745683,34.1741439479307,50.2458164660175));
#31840=CARTESIAN_POINT('Ctrl Pts',(41.7388960445005,34.1783684444372,50.270509337712));
#31841=CARTESIAN_POINT('Ctrl Pts',(41.8154155645938,34.1825929409436,50.291400831307));
#31842=CARTESIAN_POINT('Ctrl Pts',(41.8927307010451,34.1868174374501,50.3083908462905));
#31843=CARTESIAN_POINT('Ctrl Pts',(41.9700829562763,34.1910439621255,50.3253890181325));
#31844=CARTESIAN_POINT('Ctrl Pts',(42.0482311252671,34.1952704868008,50.3384819022801));
#31845=CARTESIAN_POINT('Ctrl Pts',(42.1267485474494,34.1994970114762,50.3476209414169));
#31846=CARTESIAN_POINT('Ctrl Pts',(42.2054094968579,34.2037312620975,50.356776686412));
#31847=CARTESIAN_POINT('Ctrl Pts',(42.2844405786557,34.2079655127189,50.3619641133402));
#31848=CARTESIAN_POINT('Ctrl Pts',(42.3634121985332,34.2121997633402,50.3631867834947));
#31849=CARTESIAN_POINT('Ctrl Pts',(42.4387303563637,34.2162381249325,50.3643528892908));
#31850=CARTESIAN_POINT('Ctrl Pts',(42.513994076582,34.2202764865248,50.3619130169859));
#31851=CARTESIAN_POINT('Ctrl Pts',(42.5888360551186,34.224314848117,50.3559141294171));
#31852=CARTESIAN_POINT('Ctrl Pts',(42.6673315582741,34.2285503484513,50.3496223970592));
#31853=CARTESIAN_POINT('Ctrl Pts',(42.7456614707067,34.2327858487856,50.3393913836042));
#31854=CARTESIAN_POINT('Ctrl Pts',(42.8233987915123,34.2370213491198,50.3252363114845));
#31855=CARTESIAN_POINT('Ctrl Pts',(42.901023417895,34.241250709324,50.3111017597231));
#31856=CARTESIAN_POINT('Ctrl Pts',(42.9780567007583,34.2454800695281,50.2930545292986));
#31857=CARTESIAN_POINT('Ctrl Pts',(43.0540756881294,34.2497094297322,50.2711616928564));
#31858=CARTESIAN_POINT('Ctrl Pts',(43.1300059011028,34.2539338509215,50.2492944227027));
#31859=CARTESIAN_POINT('Ctrl Pts',(43.2049237237017,34.2581582721109,50.2235905999403));
#31860=CARTESIAN_POINT('Ctrl Pts',(43.2784168589071,34.2623826933002,50.1941682394219));
#31861=CARTESIAN_POINT('Ctrl Pts',(43.3518629966521,34.2666044130526,50.1647646939427));
#31862=CARTESIAN_POINT('Ctrl Pts',(43.4238858207104,34.270826132805,50.131647504368));
#31863=CARTESIAN_POINT('Ctrl Pts',(43.4940898246073,34.2750478525574,50.0949839848053));
#31864=CARTESIAN_POINT('Ctrl Pts',(43.5642708580748,34.2792681909824,50.0583324613788));
#31865=CARTESIAN_POINT('Ctrl Pts',(43.6326338373523,34.2834885294074,50.0181371291271));
#31866=CARTESIAN_POINT('Ctrl Pts',(43.6988061852967,34.2877088678324,49.9746120970801));
#31867=CARTESIAN_POINT('Ctrl Pts',(43.7649775461838,34.2919291433049,49.9310877142726));
#31868=CARTESIAN_POINT('Ctrl Pts',(43.8289579492947,34.2961494187773,49.8842339894366));
#31869=CARTESIAN_POINT('Ctrl Pts',(43.8904035071785,34.3003696942498,49.8343085418463));
#31870=CARTESIAN_POINT('Ctrl Pts',(43.9519105249346,34.3045941909809,49.7843331571776));
#31871=CARTESIAN_POINT('Ctrl Pts',(44.0108772674731,34.308818687712,49.7312802088515));
#31872=CARTESIAN_POINT('Ctrl Pts',(44.0669931783131,34.3130431844431,49.6754474579519));
#31873=CARTESIAN_POINT('Ctrl Pts',(44.1231360302568,34.3172697093442,49.619587901893));
#31874=CARTESIAN_POINT('Ctrl Pts',(44.1764250078465,34.3214962342452,49.5609462324549));
#31875=CARTESIAN_POINT('Ctrl Pts',(44.2265884532666,34.3257227591463,49.4998550140907));
#31876=CARTESIAN_POINT('Ctrl Pts',(44.2768435957747,34.3299570099924,49.4386521230379));
#31877=CARTESIAN_POINT('Ctrl Pts',(44.3239615095059,34.3341912608386,49.3749911138297));
#31878=CARTESIAN_POINT('Ctrl Pts',(44.3677127827298,34.3384255116848,49.3092352140016));
#31879=CARTESIAN_POINT('Ctrl Pts',(44.4094399692409,34.3424638712975,49.2465214117702));
#31880=CARTESIAN_POINT('Ctrl Pts',(44.4481049796522,34.3465022309102,49.1819025916229));
#31881=CARTESIAN_POINT('Ctrl Pts',(44.4835486028899,34.3505405905229,49.1157130725664));
#31882=CARTESIAN_POINT('Ctrl Pts',(44.5207224779323,34.354776090788,49.0462923789195));
#31883=CARTESIAN_POINT('Ctrl Pts',(44.5544937239808,34.3590115910531,48.9748798342005));
#31884=CARTESIAN_POINT('Ctrl Pts',(44.5846441396699,34.3632470913182,48.9018427933437));
#31885=CARTESIAN_POINT('Ctrl Pts',(44.6147508468276,34.3674764514524,48.8289116330103));
#31886=CARTESIAN_POINT('Ctrl Pts',(44.6412469697431,34.3717058115867,48.7543610833301));
#31887=CARTESIAN_POINT('Ctrl Pts',(44.6639601049717,34.375935171721,48.6785831444979));
#31888=CARTESIAN_POINT('Ctrl Pts',(44.6866467159688,34.3801595928398,48.6028936985827));
#31889=CARTESIAN_POINT('Ctrl Pts',(44.7055589841037,34.3843840139585,48.5259801590757));
#31890=CARTESIAN_POINT('Ctrl Pts',(44.7205731139964,34.3886084350773,48.4482531243582));
#31891=CARTESIAN_POINT('Ctrl Pts',(44.7355776426375,34.3928301547587,48.3705757946073));
#31892=CARTESIAN_POINT('Ctrl Pts',(44.7466888919066,34.3970518744402,48.292086461749));
#31893=CARTESIAN_POINT('Ctrl Pts',(44.7538336120224,34.4012735941217,48.213208273324));
#31894=CARTESIAN_POINT('Ctrl Pts',(44.7609759944178,34.4054939324754,48.1343558934879));
#31895=CARTESIAN_POINT('Ctrl Pts',(44.764154382413,34.4097142708292,48.0551153778093));
#31896=CARTESIAN_POINT('Ctrl Pts',(44.7633472866427,34.4139346091829,47.9759159052734));
#31897=CARTESIAN_POINT('Ctrl Pts',(44.7625402029114,34.418154884584,47.8967176141169));
#31898=CARTESIAN_POINT('Ctrl Pts',(44.757747759704,34.422375159985,47.8175608341996));
#31899=CARTESIAN_POINT('Ctrl Pts',(44.7490005818709,34.4265954353861,47.7388741543426));
#31900=CARTESIAN_POINT('Ctrl Pts',(44.7402446548217,34.430819932046,47.6601087694699));
#31901=CARTESIAN_POINT('Ctrl Pts',(44.7275261432045,34.4350444287058,47.581814891553));
#31902=CARTESIAN_POINT('Ctrl Pts',(44.71092746403,34.4392689253657,47.5044147935097));
#31903=CARTESIAN_POINT('Ctrl Pts',(44.6943208158723,34.4434954501955,47.426977535879));
#31904=CARTESIAN_POINT('Ctrl Pts',(44.6738304106541,34.4477219750253,47.3504353669544));
#31905=CARTESIAN_POINT('Ctrl Pts',(44.6495889798429,34.4519484998552,47.2751966731111));
#31906=CARTESIAN_POINT('Ctrl Pts',(44.6253032365076,34.4561827506309,47.1998204454535));
#31907=CARTESIAN_POINT('Ctrl Pts',(44.5972529328508,34.4604170014067,47.1257528941725));
#31908=CARTESIAN_POINT('Ctrl Pts',(44.5656194436254,34.4646512521825,47.0533834639668));
#31909=CARTESIAN_POINT('Ctrl Pts',(44.5354494248471,34.4686896124312,46.9843620843543));
#31910=CARTESIAN_POINT('Ctrl Pts',(44.5020206202816,34.47272797268,46.9168854827684));
#31911=CARTESIAN_POINT('Ctrl Pts',(44.4655280698614,34.4767663329287,46.8512684240805));
#31912=CARTESIAN_POINT('Ctrl Pts',(44.4272540683125,34.4810018331784,46.782448147697));
#31913=CARTESIAN_POINT('Ctrl Pts',(44.3854640708046,34.4852373334281,46.7154120032883));
#31914=CARTESIAN_POINT('Ctrl Pts',(44.3403489880603,34.4894728336778,46.6505422402189));
#31915=CARTESIAN_POINT('Ctrl Pts',(44.2952993078694,34.4937021937961,46.5857665177206));
#31916=CARTESIAN_POINT('Ctrl Pts',(44.2469343804596,34.4979315539145,46.5231513220195));
#31917=CARTESIAN_POINT('Ctrl Pts',(44.1954906201956,34.5021609140329,46.4630537180208));
#31918=CARTESIAN_POINT('Ctrl Pts',(44.1441069355828,34.5063853351351,46.4030262955695));
#31919=CARTESIAN_POINT('Ctrl Pts',(44.0896518665518,34.5106097562374,46.3455109771495));
#31920=CARTESIAN_POINT('Ctrl Pts',(44.0324037656135,34.5148341773396,46.2908340083799));
#31921=CARTESIAN_POINT('Ctrl Pts',(43.9751922737569,34.5190558970041,46.2361920045014));
#31922=CARTESIAN_POINT('Ctrl Pts',(43.9151916335014,34.5232776166686,46.1843850710417));
#31923=CARTESIAN_POINT('Ctrl Pts',(43.8527180962922,34.5274993363332,46.1357037323416));
#31924=CARTESIAN_POINT('Ctrl Pts',(43.7902650001494,34.5317196746696,46.0870383219612));
#31925=CARTESIAN_POINT('Ctrl Pts',(43.7253409836413,34.5359400130061,46.0414967639062));
#31926=CARTESIAN_POINT('Ctrl Pts',(43.6582953727722,34.5401603513425,45.9993293135151));
#31927=CARTESIAN_POINT('Ctrl Pts',(43.591250761995,34.5443806267259,45.9571624921186));
#31928=CARTESIAN_POINT('Ctrl Pts',(43.5220850177789,34.5486009021093,45.9183699270908));
#31929=CARTESIAN_POINT('Ctrl Pts',(43.4511751631312,34.5528211774927,45.883157724979));
#31930=CARTESIAN_POINT('Ctrl Pts',(43.3801943821118,34.5570456741345,45.8479103024631));
#31931=CARTESIAN_POINT('Ctrl Pts',(43.3074664271477,34.5612701707763,45.8162506060025));
#31932=CARTESIAN_POINT('Ctrl Pts',(43.2333910285123,34.5654946674181,45.7883377666345));
#31933=CARTESIAN_POINT('Ctrl Pts',(43.1592800664735,34.5697211922296,45.760411526386));
#31934=CARTESIAN_POINT('Ctrl Pts',(43.0838208196378,34.5739477170411,45.7362358701697));
#31935=CARTESIAN_POINT('Ctrl Pts',(43.0074285589998,34.5781742418525,45.7159201006507));
#31936=CARTESIAN_POINT('Ctrl Pts',(42.9308966558697,34.5824084926097,45.695567194586));
#31937=CARTESIAN_POINT('Ctrl Pts',(42.8534287911998,34.5866427433669,45.6790883721612));
#31938=CARTESIAN_POINT('Ctrl Pts',(42.7754506211068,34.5908769941241,45.6665417783876));
#31939=CARTESIAN_POINT('Ctrl Pts',(42.7010799773968,34.5949153545276,45.6545756312698));
#31940=CARTESIAN_POINT('Ctrl Pts',(42.6262455599381,34.5989537149311,45.6461859265064));
#31941=CARTESIAN_POINT('Ctrl Pts',(42.5513176098108,34.6029920753346,45.641378915158));
#31942=CARTESIAN_POINT('Ctrl Pts',(42.4727319161874,34.6072275756102,45.6363372408506));
#31943=CARTESIAN_POINT('Ctrl Pts',(42.3937446037544,34.6114630758858,45.635217818096));
#31944=CARTESIAN_POINT('Ctrl Pts',(42.3147804360375,34.6156985761613,45.6380668792665));
#31945=CARTESIAN_POINT('Ctrl Pts',(42.235930741297,34.619927936306,45.6409118102027));
#31946=CARTESIAN_POINT('Ctrl Pts',(42.1571045897222,34.6241572964507,45.6477137837584));
#31947=CARTESIAN_POINT('Ctrl Pts',(42.0787301810835,34.6283866565954,45.6584671378874));
#31948=CARTESIAN_POINT('Ctrl Pts',(42.0004472975019,34.6326110777245,45.6692079343287));
#31949=CARTESIAN_POINT('Ctrl Pts',(41.9226155711116,34.6368354988536,45.6838908782171));
#31950=CARTESIAN_POINT('Ctrl Pts',(41.8456599699784,34.6410599199826,45.7024583633771));
#31951=CARTESIAN_POINT('Ctrl Pts',(41.7687535804959,34.6452816396743,45.7210139749818));
#31952=CARTESIAN_POINT('Ctrl Pts',(41.6927226592897,34.6495033593661,45.7434490876825));
#31953=CARTESIAN_POINT('Ctrl Pts',(41.6179826348283,34.6537250790578,45.7696548963289));
#31954=CARTESIAN_POINT('Ctrl Pts',(41.5432670649687,34.6579454174216,45.7958521305518));
#31955=CARTESIAN_POINT('Ctrl Pts',(41.4698419957355,34.6621657557855,45.8258174557124));
#31956=CARTESIAN_POINT('Ctrl Pts',(41.3981068812904,34.6663860941494,45.8593924648403));
#31957=CARTESIAN_POINT('Ctrl Pts',(41.3263728368844,34.6706063695605,45.8929669731456));
#31958=CARTESIAN_POINT('Ctrl Pts',(41.2563291216867,34.6748266449716,45.9301508582183));
#31959=CARTESIAN_POINT('Ctrl Pts',(41.1883530433289,34.6790469203827,45.9707385350109));
#31960=CARTESIAN_POINT('Ctrl Pts',(41.1203089730569,34.6832714170523,46.0113668089357));
#31961=CARTESIAN_POINT('Ctrl Pts',(41.0543370748975,34.687495913722,46.055405434477));
#31962=CARTESIAN_POINT('Ctrl Pts',(40.9907874331974,34.6917204103917,46.1026043157882));
#31963=CARTESIAN_POINT('Ctrl Pts',(40.92720728148,34.6959469352312,46.1498258571593));
#31964=CARTESIAN_POINT('Ctrl Pts',(40.8660520656411,34.7001734600706,46.2002103779536));
#31965=CARTESIAN_POINT('Ctrl Pts',(40.8076383703661,34.7043999849101,46.2534677554166));
#31966=CARTESIAN_POINT('Ctrl Pts',(40.7491178968157,34.7086342356952,46.3068224855789));
#31967=CARTESIAN_POINT('Ctrl Pts',(40.6933492891554,34.7128684864804,46.3630602319651));
#31968=CARTESIAN_POINT('Ctrl Pts',(40.64061172531,34.7171027372655,46.4218544617865));
#31969=CARTESIAN_POINT('Ctrl Pts',(40.5903139778477,34.7211410974238,46.4779286735658));
#31970=CARTESIAN_POINT('Ctrl Pts',(40.5427732208033,34.7251794575822,46.5363277566628));
#31971=CARTESIAN_POINT('Ctrl Pts',(40.4981950087289,34.7292178177405,46.5967437097678));
#31972=CARTESIAN_POINT('Ctrl Pts',(40.4511793296354,34.7334769891256,46.6604631128379));
#31973=CARTESIAN_POINT('Ctrl Pts',(40.407280079481,34.7377361605108,46.7266690778517));
#31974=CARTESIAN_POINT('Ctrl Pts',(40.3667688384094,34.7419953318959,46.7950263552936));
#31975=CARTESIAN_POINT('Ctrl Pts',(40.3263172950927,34.7462482269251,46.8632829007934));
#31976=CARTESIAN_POINT('Ctrl Pts',(40.2892440808813,34.7505011219543,46.933684070064));
#31977=CARTESIAN_POINT('Ctrl Pts',(40.2557791489135,34.7547540169835,47.0058634989773));
#31978=CARTESIAN_POINT('Ctrl Pts',(40.2223534731393,34.7590019231345,47.0779582574765));
#31979=CARTESIAN_POINT('Ctrl Pts',(40.1925278654198,34.7632498292854,47.1518267152404));
#31980=CARTESIAN_POINT('Ctrl Pts',(40.166487024296,34.7674977354364,47.2270768290044));
#31981=CARTESIAN_POINT('Ctrl Pts',(40.1404699613832,34.7717417627722,47.3022582309678));
#31982=CARTESIAN_POINT('Ctrl Pts',(40.1182309459455,34.775985790108,47.378818345628));
#31983=CARTESIAN_POINT('Ctrl Pts',(40.0999065078837,34.7802298174438,47.456345359236));
#31984=CARTESIAN_POINT('Ctrl Pts',(40.0815916823042,34.7844716184829,47.5338317043641));
#31985=CARTESIAN_POINT('Ctrl Pts',(40.0671874585047,34.7887134195219,47.612283491084));
#31986=CARTESIAN_POINT('Ctrl Pts',(40.0567801120093,34.7929552205609,47.6912752076284));
#31987=CARTESIAN_POINT('Ctrl Pts',(40.0463738175627,34.7971965928085,47.7702589391271));
#31988=CARTESIAN_POINT('Ctrl Pts',(40.039963661291,34.8014379650561,47.8497820342824));
#31989=CARTESIAN_POINT('Ctrl Pts',(40.0375843491048,34.8056793373036,47.9294115214396));
#31990=CARTESIAN_POINT('Ctrl Pts',(40.0368655855772,34.806960608293,47.953466696472));
#31991=CARTESIAN_POINT('Ctrl Pts',(40.036514307811,34.8082418792823,47.9775315541757));
#31992=CARTESIAN_POINT('Ctrl Pts',(40.0365305376034,34.8095231502717,48.0015941200547));
#31993=CARTESIAN_POINT('',(40.0365302359838,35.6032731502447,48.0010561633842));
#31994=CARTESIAN_POINT('Ctrl Pts',(40.0365305376038,34.8095231503011,48.0015941206072));
#31995=CARTESIAN_POINT('Ctrl Pts',(40.0365912402537,34.8143153568354,48.0915928690318));
#31996=CARTESIAN_POINT('Ctrl Pts',(40.041796590266,34.8191075633696,48.1813911678018));
#31997=CARTESIAN_POINT('Ctrl Pts',(40.0520539960474,34.8238997699039,48.2704440855758));
#31998=CARTESIAN_POINT('Ctrl Pts',(40.0623637324262,34.8287164250207,48.3599513280101));
#31999=CARTESIAN_POINT('Ctrl Pts',(40.0777770724225,34.8335330801374,48.4487053652302));
#32000=CARTESIAN_POINT('Ctrl Pts',(40.0981505996024,34.8383497352542,48.5361714080302));
#32001=CARTESIAN_POINT('Ctrl Pts',(40.1186432407031,34.8431945509674,48.624148821454));
#32002=CARTESIAN_POINT('Ctrl Pts',(40.1441541195929,34.8480393666806,48.7108229431661));
#32003=CARTESIAN_POINT('Ctrl Pts',(40.1744893222028,34.8528841823937,48.795671203394));
#32004=CARTESIAN_POINT('Ctrl Pts',(40.179831062548,34.8537373083113,48.8106121741438));
#32005=CARTESIAN_POINT('Ctrl Pts',(40.1853222779565,34.8545904342288,48.8254965869542));
#32006=CARTESIAN_POINT('Ctrl Pts',(40.1909617610073,34.8554435601464,48.8403216643452));
#32007=CARTESIAN_POINT('Ctrl Pts',(40.2189600101066,34.8596790604108,48.9139234831599));
#32008=CARTESIAN_POINT('Ctrl Pts',(40.2506939558323,34.8639145606751,48.9862643795161));
#32009=CARTESIAN_POINT('Ctrl Pts',(40.2860295377095,34.8681500609395,49.0569386573795));
#32010=CARTESIAN_POINT('Ctrl Pts',(40.3213138942085,34.8723794210728,49.1275104799722));
#32011=CARTESIAN_POINT('Ctrl Pts',(40.3601893103022,34.8766087812062,49.1964200657025));
#32012=CARTESIAN_POINT('Ctrl Pts',(40.4024730778727,34.8808381413395,49.2632801099822));
#32013=CARTESIAN_POINT('Ctrl Pts',(40.4447074667689,34.8850625624571,49.3300620755916));
#32014=CARTESIAN_POINT('Ctrl Pts',(40.4903420480824,34.8892869835746,49.3947988613403));
#32015=CARTESIAN_POINT('Ctrl Pts',(40.5391481857246,34.8935114046921,49.4571276423869));
#32016=CARTESIAN_POINT('Ctrl Pts',(40.587923112764,34.8977331243722,49.5194165653557));
#32017=CARTESIAN_POINT('Ctrl Pts',(40.6398652821042,34.9019548440522,49.5793001714016));
#32018=CARTESIAN_POINT('Ctrl Pts',(40.6947034233684,34.9061765637322,49.6364455464905));
#32019=CARTESIAN_POINT('Ctrl Pts',(40.7495236218367,34.9103969020844,49.6935722238668));
#32020=CARTESIAN_POINT('Ctrl Pts',(40.8072375859817,34.9146172404365,49.7479621109285));
#32021=CARTESIAN_POINT('Ctrl Pts',(40.8675355327081,34.9188375787886,49.7993173976227));
#32022=CARTESIAN_POINT('Ctrl Pts',(40.9278325799971,34.9230578541879,49.8506719182732));
#32023=CARTESIAN_POINT('Ctrl Pts',(40.9907131750664,34.9272781295871,49.8989916252247));
#32024=CARTESIAN_POINT('Ctrl Pts',(41.0558337870064,34.9314984049863,49.944018423973));
#32025=CARTESIAN_POINT('Ctrl Pts',(41.1210195347285,34.9357229016441,49.9890902600092));
#32026=CARTESIAN_POINT('Ctrl Pts',(41.1884493881031,34.9399473983019,50.0308623407405));
#32027=CARTESIAN_POINT('Ctrl Pts',(41.2577506006802,34.9441718949597,50.0691198009428));
#32028=CARTESIAN_POINT('Ctrl Pts',(41.327085084588,34.9483984197872,50.1073956284515));
#32029=CARTESIAN_POINT('Ctrl Pts',(41.3982922951244,34.9526249446148,50.1421532678384));
#32030=CARTESIAN_POINT('Ctrl Pts',(41.4709769530811,34.9568514694424,50.1732249352503));
#32031=CARTESIAN_POINT('Ctrl Pts',(41.5437944761557,34.9610857202156,50.2043534006284));
#32032=CARTESIAN_POINT('Ctrl Pts',(41.618094401867,34.9653199709889,50.231782267287));
#32033=CARTESIAN_POINT('Ctrl Pts',(41.6934638296276,34.9695542217621,50.2553928883579));
#32034=CARTESIAN_POINT('Ctrl Pts',(41.7653464172302,34.9735925820255,50.2779112036472));
#32035=CARTESIAN_POINT('Ctrl Pts',(41.8382013829943,34.9776309422888,50.2969566951741));
#32036=CARTESIAN_POINT('Ctrl Pts',(41.911663217944,34.9816693025522,50.3124700275228));
#32037=CARTESIAN_POINT('Ctrl Pts',(41.9887112278512,34.9859048028197,50.328740671801));
#32038=CARTESIAN_POINT('Ctrl Pts',(42.0667197466616,34.9901403030872,50.3411873420431));
#32039=CARTESIAN_POINT('Ctrl Pts',(42.1452750470471,34.9943758033547,50.3497033087697));
#32040=CARTESIAN_POINT('Ctrl Pts',(42.2237164671818,34.9986051634912,50.3582069300477));
#32041=CARTESIAN_POINT('Ctrl Pts',(42.3027026321385,35.0028345236277,50.362791113416));
#32042=CARTESIAN_POINT('Ctrl Pts',(42.381808964351,35.0070638837642,50.3633999930444));
#32043=CARTESIAN_POINT('Ctrl Pts',(42.4608229167689,35.011288304885,50.3640081616275));
#32044=CARTESIAN_POINT('Ctrl Pts',(42.5399562906803,35.0155127260058,50.3606502480517));
#32045=CARTESIAN_POINT('Ctrl Pts',(42.6187802500317,35.0197371471265,50.3533222565335));
#32046=CARTESIAN_POINT('Ctrl Pts',(42.6975538029512,35.0239588668099,50.3459989511274));
#32047=CARTESIAN_POINT('Ctrl Pts',(42.7760178679561,35.0281805864932,50.3347106500631));
#32048=CARTESIAN_POINT('Ctrl Pts',(42.8537457000342,35.0324023061765,50.3195053956826));
#32049=CARTESIAN_POINT('Ctrl Pts',(42.9314480999121,35.036622644532,50.3043051163935));
#32050=CARTESIAN_POINT('Ctrl Pts',(43.008414284923,35.0408429828875,50.2851905186792));
#32051=CARTESIAN_POINT('Ctrl Pts',(43.0842261984354,35.0450633212429,50.2622610261141));
#32052=CARTESIAN_POINT('Ctrl Pts',(43.1600369810961,35.0492835966455,50.2393318755777));
#32053=CARTESIAN_POINT('Ctrl Pts',(43.2346930776167,35.0535038720481,50.2125880804597));
#32054=CARTESIAN_POINT('Ctrl Pts',(43.3077915759767,35.0577241474507,50.1821789329672));
#32055=CARTESIAN_POINT('Ctrl Pts',(43.3809631898641,35.0619486441119,50.151739369243));
#32056=CARTESIAN_POINT('Ctrl Pts',(43.4525736589824,35.066173140773,50.1176273101401));
#32057=CARTESIAN_POINT('Ctrl Pts',(43.52224062299,35.0703976374342,50.0800400056276));
#32058=CARTESIAN_POINT('Ctrl Pts',(43.5919410339249,35.0746241622652,50.0424346555484));
#32059=CARTESIAN_POINT('Ctrl Pts',(43.6596956790694,35.0788506870962,50.0013509799785));
#32060=CARTESIAN_POINT('Ctrl Pts',(43.7251496048058,35.0830772119271,49.95703065019));
#32061=CARTESIAN_POINT('Ctrl Pts',(43.790723178124,35.0873114627038,49.9126293043246));
#32062=CARTESIAN_POINT('Ctrl Pts',(43.8539872522894,35.0915457134804,49.8649797648117));
#32063=CARTESIAN_POINT('Ctrl Pts',(43.9146186662522,35.0957799642571,49.8143651056886));
#32064=CARTESIAN_POINT('Ctrl Pts',(43.9724450690735,35.0998183244907,49.7660920492676));
#32065=CARTESIAN_POINT('Ctrl Pts',(44.0278767779848,35.1038566847244,49.7151224274638));
#32066=CARTESIAN_POINT('Ctrl Pts',(44.0806661529964,35.107895044958,49.6617315436232));
#32067=CARTESIAN_POINT('Ctrl Pts',(44.1360325390962,35.1121305452241,49.6057342849271));
#32068=CARTESIAN_POINT('Ctrl Pts',(44.1887024828509,35.1163660454902,49.5468604738782));
#32069=CARTESIAN_POINT('Ctrl Pts',(44.2383623988095,35.1206015457562,49.4854003270308));
#32070=CARTESIAN_POINT('Ctrl Pts',(44.2879503236526,35.1248309058913,49.4240292778883));
#32071=CARTESIAN_POINT('Ctrl Pts',(44.3345365935244,35.1290602660263,49.3600797005107));
#32072=CARTESIAN_POINT('Ctrl Pts',(44.3778445308435,35.1332896261614,49.2938784536085));
#32073=CARTESIAN_POINT('Ctrl Pts',(44.4211018934708,35.1375140472807,49.2277545160374));
#32074=CARTESIAN_POINT('Ctrl Pts',(44.461088275703,35.1417384684,49.1593845249455));
#32075=CARTESIAN_POINT('Ctrl Pts',(44.4975683203187,35.1459628895193,49.0891269818049));
#32076=CARTESIAN_POINT('Ctrl Pts',(44.5340250366355,35.1501846092011,49.018914367035));
#32077=CARTESIAN_POINT('Ctrl Pts',(44.5669796499953,35.1544063288829,48.9468170113821));
#32078=CARTESIAN_POINT('Ctrl Pts',(44.5962416999364,35.1586280485648,48.8732198098763));
#32079=CARTESIAN_POINT('Ctrl Pts',(44.6254941754652,35.1628483869187,48.799646689047));
#32080=CARTESIAN_POINT('Ctrl Pts',(44.6510563133627,35.1670687252727,48.7245751326297));
#32081=CARTESIAN_POINT('Ctrl Pts',(44.6727855665659,35.1712890636266,48.6484105252922));
#32082=CARTESIAN_POINT('Ctrl Pts',(44.6945144956437,35.1755093390277,48.5722470540676));
#32083=CARTESIAN_POINT('Ctrl Pts',(44.712410526193,35.1797296144288,48.4949910160413));
#32084=CARTESIAN_POINT('Ctrl Pts',(44.7263812451759,35.1839498898299,48.4170620373444));
#32085=CARTESIAN_POINT('Ctrl Pts',(44.7403659381325,35.1881743864895,48.3390551115142));
#32086=CARTESIAN_POINT('Ctrl Pts',(44.7504173933706,35.1923988831492,48.2603743635062));
#32087=CARTESIAN_POINT('Ctrl Pts',(44.75649464996,35.1966233798089,48.1814480796533));
#32088=CARTESIAN_POINT('Ctrl Pts',(44.7625748242244,35.2008499046383,48.1024839034978));
#32089=CARTESIAN_POINT('Ctrl Pts',(44.7646769863967,35.2050764294678,48.023274426495));
#32090=CARTESIAN_POINT('Ctrl Pts',(44.7628123619134,35.2093029542972,47.9442489167004));
#32091=CARTESIAN_POINT('Ctrl Pts',(44.7609443289591,35.2135372050724,47.8650789509233));
#32092=CARTESIAN_POINT('Ctrl Pts',(44.7550950545986,35.2177714558475,47.7860940936335));
#32093=CARTESIAN_POINT('Ctrl Pts',(44.7453277846642,35.2220057066227,47.7077192729887));
#32094=CARTESIAN_POINT('Ctrl Pts',(44.7360123811323,35.2260440668698,47.6329703322973));
#32095=CARTESIAN_POINT('Ctrl Pts',(44.723133581382,35.2300824271168,47.5587765774757));
#32096=CARTESIAN_POINT('Ctrl Pts',(44.7067889521281,35.2341207873639,47.4854952174762));
#32097=CARTESIAN_POINT('Ctrl Pts',(44.6896464295898,35.23835628763,47.4086364924533));
#32098=CARTESIAN_POINT('Ctrl Pts',(44.6686258934281,35.242591787896,47.3324893607809));
#32099=CARTESIAN_POINT('Ctrl Pts',(44.6438017768508,35.246827288162,47.2574745613104));
#32100=CARTESIAN_POINT('Ctrl Pts',(44.6190136473631,35.2510566482971,47.1825685094887));
#32101=CARTESIAN_POINT('Ctrl Pts',(44.5904330334664,35.2552860084321,47.1087919719138));
#32102=CARTESIAN_POINT('Ctrl Pts',(44.5581851522933,35.2595153685672,47.0365544699774));
#32103=CARTESIAN_POINT('Ctrl Pts',(44.5259749299596,35.2637397896865,46.9644013264664));
#32104=CARTESIAN_POINT('Ctrl Pts',(44.490106141021,35.2679642108057,46.8937840734335));
#32105=CARTESIAN_POINT('Ctrl Pts',(44.4507529690236,35.272188631925,46.8250945991524));
#32106=CARTESIAN_POINT('Ctrl Pts',(44.4114249626358,35.2764103516068,46.7564490504918));
#32107=CARTESIAN_POINT('Ctrl Pts',(44.3686172283732,35.2806320712886,46.6897292399323));
#32108=CARTESIAN_POINT('Ctrl Pts',(44.32255043627,35.2848537909704,46.6253035750035));
#32109=CARTESIAN_POINT('Ctrl Pts',(44.276498717016,35.2890741293244,46.5608989898654));
#32110=CARTESIAN_POINT('Ctrl Pts',(44.2271903301258,35.2932944676783,46.4987874413494));
#32111=CARTESIAN_POINT('Ctrl Pts',(44.1748890987347,35.2975148060322,46.4393081251917));
#32112=CARTESIAN_POINT('Ctrl Pts',(44.1225886474974,35.3017350814333,46.37982969626));
#32113=CARTESIAN_POINT('Ctrl Pts',(44.0672957514324,35.3059553568343,46.3229837732254));
#32114=CARTESIAN_POINT('Ctrl Pts',(44.0093133332261,35.3101756322354,46.2690750922121));
#32115=CARTESIAN_POINT('Ctrl Pts',(43.9512729190941,35.314400128895,46.2151124899592));
#32116=CARTESIAN_POINT('Ctrl Pts',(43.8905379534679,35.3186246255546,46.1640933189559));
#32117=CARTESIAN_POINT('Ctrl Pts',(43.8274464776591,35.3228491222143,46.1162837277555));
#32118=CARTESIAN_POINT('Ctrl Pts',(43.7643247117978,35.3270756470437,46.0684511832955));
#32119=CARTESIAN_POINT('Ctrl Pts',(43.6988445703532,35.3313021718731,46.0238315529827));
#32120=CARTESIAN_POINT('Ctrl Pts',(43.6313731526737,35.3355286967025,45.9826476262749));
#32121=CARTESIAN_POINT('Ctrl Pts',(43.5637783995047,35.3397629474776,45.9413884167297));
#32122=CARTESIAN_POINT('Ctrl Pts',(43.4941855100515,35.3439971982527,45.9035776850628));
#32123=CARTESIAN_POINT('Ctrl Pts',(43.4229860762779,35.3482314490278,45.8693921222708));
#32124=CARTESIAN_POINT('Ctrl Pts',(43.3550805651844,35.3522698092751,45.8367880973457));
#32125=CARTESIAN_POINT('Ctrl Pts',(43.2857142139623,35.3563081695224,45.8074813394831));
#32126=CARTESIAN_POINT('Ctrl Pts',(43.2152402281285,35.3603465297697,45.7815830393407));
#32127=CARTESIAN_POINT('Ctrl Pts',(43.1413259244272,35.3645820300361,45.7544204658119));
#32128=CARTESIAN_POINT('Ctrl Pts',(43.0659121183401,35.3688175303026,45.7309043765296));
#32129=CARTESIAN_POINT('Ctrl Pts',(42.9893929307821,35.373053030569,45.7111997872151));
#32130=CARTESIAN_POINT('Ctrl Pts',(42.9129846717578,35.3772823907044,45.6915237633006));
#32131=CARTESIAN_POINT('Ctrl Pts',(42.8354746641284,35.3815117508398,45.6756483828109));
#32132=CARTESIAN_POINT('Ctrl Pts',(42.7572750682811,35.3857411109752,45.6636898822107));
#32133=CARTESIAN_POINT('Ctrl Pts',(42.6791667933487,35.3899655320949,45.6517453466598));
#32134=CARTESIAN_POINT('Ctrl Pts',(42.6003709920194,35.3941899532146,45.6437086719844));
#32135=CARTESIAN_POINT('Ctrl Pts',(42.5213114851465,35.3984143743342,45.6396453731544));
#32136=CARTESIAN_POINT('Ctrl Pts',(42.4423025353339,35.4026360940164,45.6355846727272));
#32137=CARTESIAN_POINT('Ctrl Pts',(42.3630306821481,35.4068578136986,45.6354923290302));
#32138=CARTESIAN_POINT('Ctrl Pts',(42.2839251472717,35.4110795333808,45.6393820577094));
#32139=CARTESIAN_POINT('Ctrl Pts',(42.2048454953741,35.4152998717352,45.6432705136867));
#32140=CARTESIAN_POINT('Ctrl Pts',(42.125932522159,35.4195202100895,45.6511384318469));
#32141=CARTESIAN_POINT('Ctrl Pts',(42.0476142268314,35.4237405484438,45.6629474315351));
#32142=CARTESIAN_POINT('Ctrl Pts',(41.9692970997422,35.4279608238453,45.6747562550738));
#32143=CARTESIAN_POINT('Ctrl Pts',(41.8915750968142,35.4321810992468,45.6905059719863));
#32144=CARTESIAN_POINT('Ctrl Pts',(41.814868388276,35.4364013746482,45.7101066754407));
#32145=CARTESIAN_POINT('Ctrl Pts',(41.7380849551596,35.4406258713082,45.7297269841648));
#32146=CARTESIAN_POINT('Ctrl Pts',(41.6623193009106,35.4448503679683,45.7532058575779));
#32147=CARTESIAN_POINT('Ctrl Pts',(41.5879781414048,35.4490748646283,45.7804029775512));
#32148=CARTESIAN_POINT('Ctrl Pts',(41.5136012909027,35.4533013894581,45.8076131547907));
#32149=CARTESIAN_POINT('Ctrl Pts',(41.4406507302551,35.4575279142879,45.838544951297));
#32150=CARTESIAN_POINT('Ctrl Pts',(41.3695124292721,35.4617544391177,45.8730101534151));
#32151=CARTESIAN_POINT('Ctrl Pts',(41.2982440898598,35.4659886898932,45.9075383567672));
#32152=CARTESIAN_POINT('Ctrl Pts',(41.2287950424061,35.4702229406688,45.9456126459984));
#32153=CARTESIAN_POINT('Ctrl Pts',(41.161525736918,35.4744571914443,45.9869992696018));
#32154=CARTESIAN_POINT('Ctrl Pts',(41.0973685333625,35.4784955516881,46.0264712102698));
#32155=CARTESIAN_POINT('Ctrl Pts',(41.035194121869,35.4825339119318,46.0689555518998));
#32156=CARTESIAN_POINT('Ctrl Pts',(40.9752870980793,35.4865722721756,46.1142153919387));
#32157=CARTESIAN_POINT('Ctrl Pts',(40.9131124855492,35.4907634916275,46.1611883984343));
#32158=CARTESIAN_POINT('Ctrl Pts',(40.8531332119513,35.4949547110795,46.2113381526252));
#32159=CARTESIAN_POINT('Ctrl Pts',(40.795697314067,35.4991459305314,46.2644299689128));
#32160=CARTESIAN_POINT('Ctrl Pts',(40.7362412652663,35.5034845646861,46.3193891449053));
#32161=CARTESIAN_POINT('Ctrl Pts',(40.6795113023837,35.5078231988408,46.3775009674271));
#32162=CARTESIAN_POINT('Ctrl Pts',(40.6258601075221,35.5121618329955,46.4384565062674));
#32163=CARTESIAN_POINT('Ctrl Pts',(40.5741683302032,35.5163420140926,46.4971858625887));
#32164=CARTESIAN_POINT('Ctrl Pts',(40.5253347037497,35.5205221951896,46.5585544384093));
#32165=CARTESIAN_POINT('Ctrl Pts',(40.4796388749424,35.5247023762866,46.6222469051868));
#32166=CARTESIAN_POINT('Ctrl Pts',(40.4339704875959,35.5288800470829,46.6859011230829));
#32167=CARTESIAN_POINT('Ctrl Pts',(40.3914364389047,35.5330577178791,46.7518760741883));
#32168=CARTESIAN_POINT('Ctrl Pts',(40.3522756935313,35.5372353886753,46.8198239090724));
#32169=CARTESIAN_POINT('Ctrl Pts',(40.3131256126739,35.5414119217803,46.8877532399478));
#32170=CARTESIAN_POINT('Ctrl Pts',(40.2773472508029,35.5455884548853,46.9576539720652));
#32171=CARTESIAN_POINT('Ctrl Pts',(40.2451349916197,35.5497649879903,47.0291512802923));
#32172=CARTESIAN_POINT('Ctrl Pts',(40.2129209329773,35.5539417544071,47.1006525825418));
#32173=CARTESIAN_POINT('Ctrl Pts',(40.1842735669987,35.5581185208239,47.1737501990012));
#32174=CARTESIAN_POINT('Ctrl Pts',(40.1593395727421,35.5622952872407,47.2480483455564));
#32175=CARTESIAN_POINT('Ctrl Pts',(40.1343816814018,35.566476056728,47.322417700479));
#32176=CARTESIAN_POINT('Ctrl Pts',(40.1131444144949,35.5706568262153,47.3979894250277));
#32177=CARTESIAN_POINT('Ctrl Pts',(40.0957246066908,35.5748375957026,47.4743524444177));
#32178=CARTESIAN_POINT('Ctrl Pts',(40.0782947730842,35.5790207713914,47.5507594138075));
#32179=CARTESIAN_POINT('Ctrl Pts',(40.064686851524,35.5832039470803,47.6279581114337));
#32180=CARTESIAN_POINT('Ctrl Pts',(40.0549461281531,35.5873871227692,47.7055296635727));
#32181=CARTESIAN_POINT('Ctrl Pts',(40.0451907017365,35.5915766127142,47.7832183053804));
#32182=CARTESIAN_POINT('Ctrl Pts',(40.0393141504531,35.5957661026593,47.8612804466963));
#32183=CARTESIAN_POINT('Ctrl Pts',(40.0373097124553,35.5999555926044,47.9392954199253));
#32184=CARTESIAN_POINT('Ctrl Pts',(40.0367806234985,35.6010614451512,47.95988815507));
#32185=CARTESIAN_POINT('Ctrl Pts',(40.036521040056,35.6021672976979,47.9804776262913));
#32186=CARTESIAN_POINT('Ctrl Pts',(40.0365302359838,35.6032731502447,48.0010561633842));
#32187=CARTESIAN_POINT('',(40.0365309734993,36.3970231502996,47.9978548492323));
#32188=CARTESIAN_POINT('Ctrl Pts',(40.036530235984,35.6032731502717,48.0010561638867));
#32189=CARTESIAN_POINT('Ctrl Pts',(40.0365566379387,35.6064481050416,48.0601381135477));
#32190=CARTESIAN_POINT('Ctrl Pts',(40.0387982312214,35.6096230598115,48.1191684352402));
#32191=CARTESIAN_POINT('Ctrl Pts',(40.0432446627774,35.6127980145814,48.1780301136687));
#32192=CARTESIAN_POINT('Ctrl Pts',(40.0491763573697,35.6170335148476,48.256553643206));
#32193=CARTESIAN_POINT('Ctrl Pts',(40.0590480508809,35.6212690151138,48.334929648911));
#32194=CARTESIAN_POINT('Ctrl Pts',(40.0728464792292,35.6255045153801,48.4127310645737));
#32195=CARTESIAN_POINT('Ctrl Pts',(40.0866249042362,35.6297338755153,48.4904196928788));
#32196=CARTESIAN_POINT('Ctrl Pts',(40.1043186784733,35.6339632356505,48.5675349270486));
#32197=CARTESIAN_POINT('Ctrl Pts',(40.1258626696229,35.6381925957857,48.6436535119807));
#32198=CARTESIAN_POINT('Ctrl Pts',(40.1473815018575,35.6424170169052,48.7196832061872));
#32199=CARTESIAN_POINT('Ctrl Pts',(40.1727414889524,35.6466414380247,48.7947181147361));
#32200=CARTESIAN_POINT('Ctrl Pts',(40.2018265080558,35.6508658591441,48.8683454037502));
#32201=CARTESIAN_POINT('Ctrl Pts',(40.2308929278394,35.6550875788261,48.9419256095046));
#32202=CARTESIAN_POINT('Ctrl Pts',(40.2636794797217,35.6593092985082,49.0140995469749));
#32203=CARTESIAN_POINT('Ctrl Pts',(40.3000206651146,35.6635310181902,49.08447094657));
#32204=CARTESIAN_POINT('Ctrl Pts',(40.3363499598335,35.6677513565443,49.1548193209564));
#32205=CARTESIAN_POINT('Ctrl Pts',(40.3762313634132,35.6719716948984,49.2233659118693));
#32206=CARTESIAN_POINT('Ctrl Pts',(40.4194524776835,35.6761920332525,49.2897371642106));
#32207=CARTESIAN_POINT('Ctrl Pts',(40.4626729472441,35.6804123086538,49.3561074265221));
#32208=CARTESIAN_POINT('Ctrl Pts',(40.5092327712286,35.6846325840551,49.420302022182));
#32209=CARTESIAN_POINT('Ctrl Pts',(40.558875910112,35.6888528594563,49.481975885949));
#32210=CARTESIAN_POINT('Ctrl Pts',(40.6085687036992,35.6930773561162,49.5437114379473));
#32211=CARTESIAN_POINT('Ctrl Pts',(40.6613506779281,35.697301852776,49.6029208549052));
#32212=CARTESIAN_POINT('Ctrl Pts',(40.7169254990333,35.7015263494358,49.6592922181146));
#32213=CARTESIAN_POINT('Ctrl Pts',(40.7725270014648,35.7057528742654,49.7156906450682));
#32214=CARTESIAN_POINT('Ctrl Pts',(40.8309236755072,35.7099793990951,49.7692479862471));
#32215=CARTESIAN_POINT('Ctrl Pts',(40.8917842060067,35.7142059239247,49.8196910615951));
#32216=CARTESIAN_POINT('Ctrl Pts',(40.9527559875157,35.7184401747,49.8702263451938));
#32217=CARTESIAN_POINT('Ctrl Pts',(41.0162002482608,35.7226744254753,49.9176357057742));
#32218=CARTESIAN_POINT('Ctrl Pts',(41.0817548165928,35.7269086762506,49.9616880683034));
#32219=CARTESIAN_POINT('Ctrl Pts',(41.1442766124703,35.7309470364962,50.003702421964));
#32220=CARTESIAN_POINT('Ctrl Pts',(41.2087174496573,35.7349853967418,50.0426633669731));
#32221=CARTESIAN_POINT('Ctrl Pts',(41.2747437426207,35.7390237569874,50.0784101607067));
#32222=CARTESIAN_POINT('Ctrl Pts',(41.3439932311313,35.7432592572536,50.1159020002579));
#32223=CARTESIAN_POINT('Ctrl Pts',(41.4152501538411,35.7474947575199,50.1500003809986));
#32224=CARTESIAN_POINT('Ctrl Pts',(41.4881481603261,35.7517302577862,50.1804854192091));
#32225=CARTESIAN_POINT('Ctrl Pts',(41.5609404878403,35.7559596179215,50.2109262637904));
#32226=CARTESIAN_POINT('Ctrl Pts',(41.6353687454045,35.7601889780567,50.2377639884319));
#32227=CARTESIAN_POINT('Ctrl Pts',(41.7110417275687,35.764418338192,50.2608243938326));
#32228=CARTESIAN_POINT('Ctrl Pts',(41.7866263393789,35.7686427593115,50.2838578694609));
#32229=CARTESIAN_POINT('Ctrl Pts',(41.8634523406194,35.7728671804311,50.3031226554696));
#32230=CARTESIAN_POINT('Ctrl Pts',(41.9411097049378,35.7770916015506,50.318493074822));
#32231=CARTESIAN_POINT('Ctrl Pts',(42.0187174088397,35.7813133212326,50.3338536650819));
#32232=CARTESIAN_POINT('Ctrl Pts',(42.09715496145,35.7855350409147,50.3453247406623));
#32233=CARTESIAN_POINT('Ctrl Pts',(42.1759995555927,35.7897567605967,50.3528311120447));
#32234=CARTESIAN_POINT('Ctrl Pts',(42.2548183521354,35.7939770989509,50.3603350273758));
#32235=CARTESIAN_POINT('Ctrl Pts',(42.3340434588698,35.7981974373051,50.363876769935));
#32236=CARTESIAN_POINT('Ctrl Pts',(42.4132457998714,35.8024177756593,50.3634328824161));
#32237=CARTESIAN_POINT('Ctrl Pts',(42.4924469594477,35.8066380510606,50.3629890015185));
#32238=CARTESIAN_POINT('Ctrl Pts',(42.5716248846297,35.8108583264619,50.3585596126844));
#32239=CARTESIAN_POINT('Ctrl Pts',(42.6503508506604,35.8150786018632,50.3501733749819));
#32240=CARTESIAN_POINT('Ctrl Pts',(42.7291555609973,35.819303098523,50.3417787490879));
#32241=CARTESIAN_POINT('Ctrl Pts',(42.8075069413014,35.8235275951829,50.3294194180143));
#32242=CARTESIAN_POINT('Ctrl Pts',(42.8849823451398,35.8277520918428,50.3131758614085));
#32243=CARTESIAN_POINT('Ctrl Pts',(42.9624949447169,35.8319786166724,50.2969245063135));
#32244=CARTESIAN_POINT('Ctrl Pts',(43.0391302754707,35.8362051415021,50.2767853302189));
#32245=CARTESIAN_POINT('Ctrl Pts',(43.1144793466283,35.8404316663318,50.2528891903824));
#32246=CARTESIAN_POINT('Ctrl Pts',(43.1899661533618,35.8446659171071,50.2289493692033));
#32247=CARTESIAN_POINT('Ctrl Pts',(43.2641615613275,35.8489001678825,50.2012390258438));
#32248=CARTESIAN_POINT('Ctrl Pts',(43.3366752981571,35.8531344186579,50.1699377471998));
#32249=CARTESIAN_POINT('Ctrl Pts',(43.4058343082324,35.8571727789029,50.1400845698604));
#32250=CARTESIAN_POINT('Ctrl Pts',(43.4734635009498,35.861211139148,50.1069655568262));
#32251=CARTESIAN_POINT('Ctrl Pts',(43.5392472203167,35.8652494993931,50.0707743025015));
#32252=CARTESIAN_POINT('Ctrl Pts',(43.6082422935601,35.8694849996593,50.0328163051895));
#32253=CARTESIAN_POINT('Ctrl Pts',(43.6754693775186,35.8737204999256,49.9913341670389));
#32254=CARTESIAN_POINT('Ctrl Pts',(43.7405453513509,35.8779560001918,49.9465170438173));
#32255=CARTESIAN_POINT('Ctrl Pts',(43.805526985677,35.8821853603271,49.9017648911991));
#32256=CARTESIAN_POINT('Ctrl Pts',(43.8683633192411,35.8864147204623,49.8536876182718));
#32257=CARTESIAN_POINT('Ctrl Pts',(43.9286962067227,35.8906440805976,49.8025199994596));
#32258=CARTESIAN_POINT('Ctrl Pts',(43.9889586379004,35.8948685017171,49.7514121338177));
#32259=CARTESIAN_POINT('Ctrl Pts',(44.0467230764509,35.8990929228366,49.6972213958138));
#32260=CARTESIAN_POINT('Ctrl Pts',(44.1016620036921,35.9033173439561,49.6402246389109));
#32261=CARTESIAN_POINT('Ctrl Pts',(44.1565657985279,35.9075390636381,49.5832643303568));
#32262=CARTESIAN_POINT('Ctrl Pts',(44.208647343442,35.9117607833201,49.5235019014091));
#32263=CARTESIAN_POINT('Ctrl Pts',(44.2576146668553,35.9159825030021,49.4612522678799));
#32264=CARTESIAN_POINT('Ctrl Pts',(44.3065659683785,35.9202028413563,49.3990230021536));
#32265=CARTESIAN_POINT('Ctrl Pts',(44.352404781752,35.9244231797104,49.3343085164039));
#32266=CARTESIAN_POINT('Ctrl Pts',(44.3948792522998,35.9286435180646,49.267456985323));
#32267=CARTESIAN_POINT('Ctrl Pts',(44.4373530892751,35.9328637934659,49.2006064514359));
#32268=CARTESIAN_POINT('Ctrl Pts',(44.4764624326073,35.9370840688672,49.1316193324528));
#32269=CARTESIAN_POINT('Ctrl Pts',(44.5119994489321,35.9413043442684,49.0608717022386));
#32270=CARTESIAN_POINT('Ctrl Pts',(44.5475720105519,35.9455288409283,48.9900533079128));
#32271=CARTESIAN_POINT('Ctrl Pts',(44.579564896151,35.9497533375881,48.9174713051084));
#32272=CARTESIAN_POINT('Ctrl Pts',(44.6078171432482,35.953977834248,48.843524690142));
#32273=CARTESIAN_POINT('Ctrl Pts',(44.6360829541754,35.9582043590776,48.7695425735992));
#32274=CARTESIAN_POINT('Ctrl Pts',(44.6606044035574,35.9624308839072,48.6941949866861));
#32275=CARTESIAN_POINT('Ctrl Pts',(44.6812702854933,35.9666574087369,48.6178966947843));
#32276=CARTESIAN_POINT('Ctrl Pts',(44.7019739439685,35.9708916595122,48.5414589321629));
#32277=CARTESIAN_POINT('Ctrl Pts',(44.7188078517222,35.9751259102875,48.4640674517408));
#32278=CARTESIAN_POINT('Ctrl Pts',(44.7317119123445,35.9793601610629,48.3861476385152));
#32279=CARTESIAN_POINT('Ctrl Pts',(44.7440189881853,35.9833985213083,48.3118326551205));
#32280=CARTESIAN_POINT('Ctrl Pts',(44.7527517863751,35.9874368815536,48.2370375017441));
#32281=CARTESIAN_POINT('Ctrl Pts',(44.7579023580358,35.991475241799,48.1621323868604));
#32282=CARTESIAN_POINT('Ctrl Pts',(44.7633043643738,35.9957107420653,48.0835706403209));
#32283=CARTESIAN_POINT('Ctrl Pts',(44.7647860022,35.9999462423315,48.0045892921905));
#32284=CARTESIAN_POINT('Ctrl Pts',(44.7622990917098,36.0041817425978,47.9256128895103));
#32285=CARTESIAN_POINT('Ctrl Pts',(44.7598157864504,36.008411102733,47.846750977546));
#32286=CARTESIAN_POINT('Ctrl Pts',(44.7533753722327,36.0126404628683,47.7678944619458));
#32287=CARTESIAN_POINT('Ctrl Pts',(44.7429815473663,36.0168698230036,47.6894715639411));
#32288=CARTESIAN_POINT('Ctrl Pts',(44.7325998603324,36.021094244123,47.6111402476221));
#32289=CARTESIAN_POINT('Ctrl Pts',(44.7182739983652,36.0253186652425,47.5332420055022));
#32290=CARTESIAN_POINT('Ctrl Pts',(44.700059618178,36.029543086362,47.4562020653524));
#32291=CARTESIAN_POINT('Ctrl Pts',(44.6818568857426,36.033764806044,47.3792113907882));
#32292=CARTESIAN_POINT('Ctrl Pts',(44.6597706782225,36.0379865257261,47.3030783843339));
#32293=CARTESIAN_POINT('Ctrl Pts',(44.6339078945148,36.0422082454081,47.2282189690564));
#32294=CARTESIAN_POINT('Ctrl Pts',(44.6080535729948,36.0464285837622,47.1533840474462));
#32295=CARTESIAN_POINT('Ctrl Pts',(44.5784252820845,36.0506489221164,47.0798223328449));
#32296=CARTESIAN_POINT('Ctrl Pts',(44.5451795952357,36.0548692604706,47.0079340016489));
#32297=CARTESIAN_POINT('Ctrl Pts',(44.5119344042977,36.0590895358718,46.9360467427785));
#32298=CARTESIAN_POINT('Ctrl Pts',(44.4750721229008,36.0633098112731,46.8658332431383));
#32299=CARTESIAN_POINT('Ctrl Pts',(44.4347966036396,36.0675300866744,46.7976717491813));
#32300=CARTESIAN_POINT('Ctrl Pts',(44.3944807994765,36.0717545833342,46.7294420778514));
#32301=CARTESIAN_POINT('Ctrl Pts',(44.3507451768233,36.0759790799941,46.6632689173466));
#32302=CARTESIAN_POINT('Ctrl Pts',(44.3038382234481,36.0802035766539,46.5995034952425));
#32303=CARTESIAN_POINT('Ctrl Pts',(44.2569087501673,36.0844301014836,46.5357074595261));
#32304=CARTESIAN_POINT('Ctrl Pts',(44.2068052102526,36.0886566263132,46.474321829111));
#32305=CARTESIAN_POINT('Ctrl Pts',(44.153816271585,36.0928831511428,46.4156645158226));
#32306=CARTESIAN_POINT('Ctrl Pts',(44.100730470914,36.0971174019182,46.3568999789321));
#32307=CARTESIAN_POINT('Ctrl Pts',(44.0447490645993,36.1013516526935,46.3008740577952));
#32308=CARTESIAN_POINT('Ctrl Pts',(43.9861973017163,36.1055859034688,46.2478674248426));
#32309=CARTESIAN_POINT('Ctrl Pts',(43.9303543382109,36.1096242637142,46.1973130551059));
#32310=CARTESIAN_POINT('Ctrl Pts',(43.8721738844849,36.1136626239595,46.1495049853175));
#32311=CARTESIAN_POINT('Ctrl Pts',(43.8119629959803,36.1177009842048,46.1046501803408));
#32312=CARTESIAN_POINT('Ctrl Pts',(43.748812801644,36.1219364844711,46.0576057051378));
#32313=CARTESIAN_POINT('Ctrl Pts',(43.6831888245936,36.1261719847373,46.0136313689946));
#32314=CARTESIAN_POINT('Ctrl Pts',(43.6154220559417,36.1304074850036,45.9729973688151));
#32315=CARTESIAN_POINT('Ctrl Pts',(43.5477535275945,36.1346368451388,45.9324222750382));
#32316=CARTESIAN_POINT('Ctrl Pts',(43.4779487754724,36.1388662052741,45.8951781403443));
#32317=CARTESIAN_POINT('Ctrl Pts',(43.406369946404,36.1430955654094,45.8614935183931));
#32318=CARTESIAN_POINT('Ctrl Pts',(43.3348747065675,36.1473199865289,45.8278482330965));
#32319=CARTESIAN_POINT('Ctrl Pts',(43.2616099292165,36.1515444076484,45.7977543990737));
#32320=CARTESIAN_POINT('Ctrl Pts',(43.1869633526491,36.1557688287679,45.771395252072));
#32321=CARTESIAN_POINT('Ctrl Pts',(43.1123645111564,36.1599905484499,45.7450529612466));
#32322=CARTESIAN_POINT('Ctrl Pts',(43.0363860656463,36.1642122681319,45.7224407731108));
#32323=CARTESIAN_POINT('Ctrl Pts',(42.9594356504853,36.168433987814,45.7036937935314));
#32324=CARTESIAN_POINT('Ctrl Pts',(42.8825104131574,36.1726543261681,45.6849529478802));
#32325=CARTESIAN_POINT('Ctrl Pts',(42.8046142933375,36.1768746645223,45.670074910564));
#32326=CARTESIAN_POINT('Ctrl Pts',(42.7261685555116,36.1810950028765,45.6591444909402));
#32327=CARTESIAN_POINT('Ctrl Pts',(42.6477239878251,36.1853152782777,45.6482142343605));
#32328=CARTESIAN_POINT('Ctrl Pts',(42.5687302834738,36.189535553679,45.6412315418742));
#32329=CARTESIAN_POINT('Ctrl Pts',(42.4896158408591,36.1937558290803,45.6382295958398));
#32330=CARTESIAN_POINT('Ctrl Pts',(42.4104222653713,36.1979803257402,45.63522464716));
#32331=CARTESIAN_POINT('Ctrl Pts',(42.3311081805084,36.2022048224,45.6362084166665));
#32332=CARTESIAN_POINT('Ctrl Pts',(42.2521034082872,36.2064293190599,45.6411619303013));
#32333=CARTESIAN_POINT('Ctrl Pts',(42.1730607060814,36.2106558438895,45.6461178221051));
#32334=CARTESIAN_POINT('Ctrl Pts',(42.0943280793503,36.2148823687192,45.6550472017864));
#32335=CARTESIAN_POINT('Ctrl Pts',(42.0163290677288,36.2191088935488,45.6678792791474));
#32336=CARTESIAN_POINT('Ctrl Pts',(41.9381874765289,36.2233431443242,45.6807348131156));
#32337=CARTESIAN_POINT('Ctrl Pts',(41.8607826400316,36.2275773950995,45.6975072005145));
#32338=CARTESIAN_POINT('Ctrl Pts',(41.7845265686104,36.2318116458749,45.7180747391394));
#32339=CARTESIAN_POINT('Ctrl Pts',(41.7117983567903,36.2358500061202,45.7376907549904));
#32340=CARTESIAN_POINT('Ctrl Pts',(41.64011529799,36.2398883663654,45.7607583906208));
#32341=CARTESIAN_POINT('Ctrl Pts',(41.5698175698493,36.2439267266107,45.7871313700156));
#32342=CARTESIAN_POINT('Ctrl Pts',(41.4960881281522,36.248162226877,45.8147917951544));
#32343=CARTESIAN_POINT('Ctrl Pts',(41.4236024641777,36.2523977271432,45.8461936600882));
#32344=CARTESIAN_POINT('Ctrl Pts',(41.3527668844805,36.2566332274095,45.881204766227));
#32345=CARTESIAN_POINT('Ctrl Pts',(41.2820339938899,36.2608625875447,45.9161651173747));
#32346=CARTESIAN_POINT('Ctrl Pts',(41.212946854495,36.26509194768,45.9547241131883));
#32347=CARTESIAN_POINT('Ctrl Pts',(41.1458936046904,36.2693213078153,45.9967008236053));
#32348=CARTESIAN_POINT('Ctrl Pts',(41.0789186591795,36.2735457289347,46.0386285139276));
#32349=CARTESIAN_POINT('Ctrl Pts',(41.0139732791313,36.2777701500542,46.0839657398779));
#32350=CARTESIAN_POINT('Ctrl Pts',(40.9514213340713,36.2819945711737,46.1324855316447));
#32351=CARTESIAN_POINT('Ctrl Pts',(40.8889093897979,36.2862162908557,46.1809742959219));
#32352=CARTESIAN_POINT('Ctrl Pts',(40.8287882125454,36.2904380105378,46.2326412997073));
#32353=CARTESIAN_POINT('Ctrl Pts',(40.7713919568624,36.2946597302198,46.2872168021821));
#32354=CARTESIAN_POINT('Ctrl Pts',(40.7140144809787,36.298880068574,46.3417744477954));
#32355=CARTESIAN_POINT('Ctrl Pts',(40.6593604961549,36.3031004069281,46.3992383792675));
#32356=CARTESIAN_POINT('Ctrl Pts',(40.6077292299424,36.3073207452822,46.4593001824829));
#32357=CARTESIAN_POINT('Ctrl Pts',(40.5560987338901,36.3115410206835,46.5193610897837));
#32358=CARTESIAN_POINT('Ctrl Pts',(40.5074911717723,36.3157612960848,46.5820194350096));
#32359=CARTESIAN_POINT('Ctrl Pts',(40.4621662107731,36.3199815714861,46.646932874455));
#32360=CARTESIAN_POINT('Ctrl Pts',(40.416795914254,36.3242060681459,46.7119112424621));
#32361=CARTESIAN_POINT('Ctrl Pts',(40.3747150471325,36.3284305648058,46.7791488248277));
#32362=CARTESIAN_POINT('Ctrl Pts',(40.3361401817462,36.3326550614656,46.8482738643682));
#32363=CARTESIAN_POINT('Ctrl Pts',(40.2975467966679,36.3368815862953,46.9174320906594));
#32364=CARTESIAN_POINT('Ctrl Pts',(40.2624629746092,36.3411081111249,46.9884791578979));
#32365=CARTESIAN_POINT('Ctrl Pts',(40.2310583103646,36.3453346359546,47.0610205604692));
#32366=CARTESIAN_POINT('Ctrl Pts',(40.1995962394466,36.3495688867299,47.1336945662924));
#32367=CARTESIAN_POINT('Ctrl Pts',(40.1718269302199,36.3538031375052,47.2078679251033));
#32368=CARTESIAN_POINT('Ctrl Pts',(40.1478709218199,36.3580373882806,47.283128284757));
#32369=CARTESIAN_POINT('Ctrl Pts',(40.1250231980802,36.3620757485259,47.3549068497501));
#32370=CARTESIAN_POINT('Ctrl Pts',(40.1056438023386,36.3661141087712,47.4276737086444));
#32371=CARTESIAN_POINT('Ctrl Pts',(40.0897937455689,36.3701524690165,47.5010636284182));
#32372=CARTESIAN_POINT('Ctrl Pts',(40.0666639190707,36.376045607014,47.6081607912697));
#32373=CARTESIAN_POINT('Ctrl Pts',(40.0509743135021,36.3819387450114,47.7169176509785));
#32374=CARTESIAN_POINT('Ctrl Pts',(40.0429090143393,36.3878318830088,47.8264703880687));
#32375=CARTESIAN_POINT('Ctrl Pts',(40.0387159839485,36.3908956387631,47.8834252445147));
#32376=CARTESIAN_POINT('Ctrl Pts',(40.0365829442789,36.3939593945174,47.9405948654727));
#32377=CARTESIAN_POINT('Ctrl Pts',(40.0365309734998,36.3970231502717,47.9978548487108));
#32378=CARTESIAN_POINT('',(40.0365300000534,37.1907731503223,48.0000158946174));
#32379=CARTESIAN_POINT('Ctrl Pts',(40.0365309734993,36.3970231502996,47.9978548492323));
#32380=CARTESIAN_POINT('Ctrl Pts',(40.0364602792016,36.4011906867027,48.0757439121105));
#32381=CARTESIAN_POINT('Ctrl Pts',(40.0402441056578,36.4053582231059,48.1537521997897));
#32382=CARTESIAN_POINT('Ctrl Pts',(40.047891134619,36.4095257595091,48.2314612846587));
#32383=CARTESIAN_POINT('Ctrl Pts',(40.0555321839855,36.4136900371069,48.3091096049048));
#32384=CARTESIAN_POINT('Ctrl Pts',(40.0670303989496,36.4178543147047,48.3864587069638));
#32385=CARTESIAN_POINT('Ctrl Pts',(40.082342420306,36.4220185923026,48.4630915505459));
#32386=CARTESIAN_POINT('Ctrl Pts',(40.0976475630965,36.4261809991965,48.5396899686227));
#32387=CARTESIAN_POINT('Ctrl Pts',(40.1167630190008,36.4303434060904,48.6155722928962));
#32388=CARTESIAN_POINT('Ctrl Pts',(40.1395939776329,36.4345058129844,48.6903296712053));
#32389=CARTESIAN_POINT('Ctrl Pts',(40.1624222753605,36.4386677347578,48.7650783366855));
#32390=CARTESIAN_POINT('Ctrl Pts',(40.188965073726,36.4428296565312,48.8387018543109));
#32391=CARTESIAN_POINT('Ctrl Pts',(40.2190776109635,36.4469915783046,48.9108062219261));
#32392=CARTESIAN_POINT('Ctrl Pts',(40.2492173909904,36.4511572653654,48.9829758223076));
#32393=CARTESIAN_POINT('Ctrl Pts',(40.2829331750889,36.4553229524263,49.0536230795644));
#32394=CARTESIAN_POINT('Ctrl Pts',(40.3200322191805,36.4594886394871,49.1223744792416));
#32395=CARTESIAN_POINT('Ctrl Pts',(40.3571470655116,36.4636561009113,49.1911551633952));
#32396=CARTESIAN_POINT('Ctrl Pts',(40.3976477897498,36.4678235623355,49.2580379681821));
#32397=CARTESIAN_POINT('Ctrl Pts',(40.44129726956,36.4719910237597,49.3226768519434));
#32398=CARTESIAN_POINT('Ctrl Pts',(40.4850252896868,36.4761659838699,49.387432043125));
#32399=CARTESIAN_POINT('Ctrl Pts',(40.5319130921366,36.48034094398,49.4499348602826));
#32400=CARTESIAN_POINT('Ctrl Pts',(40.581682336817,36.4845159040901,49.5098712914208));
#32401=CARTESIAN_POINT('Ctrl Pts',(40.6288187613196,36.4884700065342,49.5666370526743));
#32402=CARTESIAN_POINT('Ctrl Pts',(40.6785392535147,36.4924241089783,49.6211008174602));
#32403=CARTESIAN_POINT('Ctrl Pts',(40.7305785860932,36.4963782114224,49.6730279685915));
#32404=CARTESIAN_POINT('Ctrl Pts',(40.78632135202,36.5006137116887,49.7286505695615));
#32405=CARTESIAN_POINT('Ctrl Pts',(40.84495300563,36.5048492119549,49.7815899480815));
#32406=CARTESIAN_POINT('Ctrl Pts',(40.9061847714878,36.5090847122211,49.831531191098));
#32407=CARTESIAN_POINT('Ctrl Pts',(40.9673277707206,36.5133140723564,49.8814000351641));
#32408=CARTESIAN_POINT('Ctrl Pts',(41.0310630363231,36.5175434324917,49.9282790806586));
#32409=CARTESIAN_POINT('Ctrl Pts',(41.0970649818335,36.5217727926269,49.971890153973));
#32410=CARTESIAN_POINT('Ctrl Pts',(41.1629898507557,36.5259972137464,50.0154502985955));
#32411=CARTESIAN_POINT('Ctrl Pts',(41.2311757499249,36.5302216348659,50.0557497973636));
#32412=CARTESIAN_POINT('Ctrl Pts',(41.3012652609604,36.5344460559854,50.0925516514838));
#32413=CARTESIAN_POINT('Ctrl Pts',(41.3713099510784,36.5386677756674,50.129329971514));
#32414=CARTESIAN_POINT('Ctrl Pts',(41.4432554225069,36.5428894953494,50.1626148686195));
#32415=CARTESIAN_POINT('Ctrl Pts',(41.5167176576929,36.5471112150315,50.1922141192567));
#32416=CARTESIAN_POINT('Ctrl Pts',(41.5901558563627,36.5513315533856,50.2218036851509));
#32417=CARTESIAN_POINT('Ctrl Pts',(41.6651093983326,36.5555518917398,50.2477098238734));
#32418=CARTESIAN_POINT('Ctrl Pts',(41.7411735569024,36.5597722300939,50.2697881308121));
#32419=CARTESIAN_POINT('Ctrl Pts',(41.8172365808575,36.5639925054952,50.2918661084186));
#32420=CARTESIAN_POINT('Ctrl Pts',(41.8944097373622,36.5682127808965,50.3101162381872));
#32421=CARTESIAN_POINT('Ctrl Pts',(41.9722738284938,36.5724330562978,50.324444183694));
#32422=CARTESIAN_POINT('Ctrl Pts',(42.0502158018559,36.5766575529576,50.3387864604841));
#32423=CARTESIAN_POINT('Ctrl Pts',(42.1288496276913,36.5808820496175,50.3491986309863));
#32424=CARTESIAN_POINT('Ctrl Pts',(42.2077472120124,36.5851065462773,50.3556377706284));
#32425=CARTESIAN_POINT('Ctrl Pts',(42.2866826748575,36.5893330711069,50.3620800016846));
#32426=CARTESIAN_POINT('Ctrl Pts',(42.3658816786816,36.5935595959366,50.3645453873998));
#32427=CARTESIAN_POINT('Ctrl Pts',(42.4449149084639,36.5977861207662,50.3630431845182));
#32428=CARTESIAN_POINT('Ctrl Pts',(42.5240926083407,36.6020203715416,50.36153823566));
#32429=CARTESIAN_POINT('Ctrl Pts',(42.6031034591966,36.6062546223169,50.3560512383724));
#32430=CARTESIAN_POINT('Ctrl Pts',(42.6815222473042,36.6104888730922,50.3466434891506));
#32431=CARTESIAN_POINT('Ctrl Pts',(42.7563131213414,36.6145272333376,50.3376709737113));
#32432=CARTESIAN_POINT('Ctrl Pts',(42.8305651566769,36.6185655935829,50.3251325535074));
#32433=CARTESIAN_POINT('Ctrl Pts',(42.903920700685,36.6226039538282,50.3091241561079));
#32434=CARTESIAN_POINT('Ctrl Pts',(42.9808572311832,36.6268394540945,50.2923342791954));
#32435=CARTESIAN_POINT('Ctrl Pts',(43.0570999599424,36.6310749543607,50.2716631661511));
#32436=CARTESIAN_POINT('Ctrl Pts',(43.1322278111933,36.635310454627,50.2471833199397));
#32437=CARTESIAN_POINT('Ctrl Pts',(43.2072467509061,36.6395398147623,50.2227389617351));
#32438=CARTESIAN_POINT('Ctrl Pts',(43.2811535801512,36.6437691748975,50.1944969791762));
#32439=CARTESIAN_POINT('Ctrl Pts',(43.3535382076112,36.6479985350328,50.1625807100605));
#32440=CARTESIAN_POINT('Ctrl Pts',(43.4258383048338,36.6522229561523,50.1307017125299));
#32441=CARTESIAN_POINT('Ctrl Pts',(43.4966193054986,36.6564473772718,50.0951571434457));
#32442=CARTESIAN_POINT('Ctrl Pts',(43.5654885266666,36.6606717983913,50.0561193873675));
#32443=CARTESIAN_POINT('Ctrl Pts',(43.6343137072693,36.6648935180733,50.0171065951965));
#32444=CARTESIAN_POINT('Ctrl Pts',(43.7012291276562,36.6691152377553,49.9746052805247));
#32445=CARTESIAN_POINT('Ctrl Pts',(43.7658653722042,36.6733369574374,49.9288344215908));
#32446=CARTESIAN_POINT('Ctrl Pts',(43.8304804680608,36.6775572957915,49.8830785386781));
#32447=CARTESIAN_POINT('Ctrl Pts',(43.8928174861141,36.6817776341457,49.8340555067686));
#32448=CARTESIAN_POINT('Ctrl Pts',(43.9525360243316,36.6859979724999,49.7820275907102));
#32449=CARTESIAN_POINT('Ctrl Pts',(44.0122536717547,36.6902182479011,49.7300004507288));
#32450=CARTESIAN_POINT('Ctrl Pts',(44.0693525639732,36.6944385233024,49.6749688250133));
#32451=CARTESIAN_POINT('Ctrl Pts',(44.1235265788985,36.6986587987037,49.6172342355796));
#32452=CARTESIAN_POINT('Ctrl Pts',(44.1777547804591,36.7028832953636,49.5594418981064));
#32453=CARTESIAN_POINT('Ctrl Pts',(44.2290519386273,36.7071077920234,49.4989415392319));
#32454=CARTESIAN_POINT('Ctrl Pts',(44.2771503574292,36.7113322886833,49.4360699761862));
#32455=CARTESIAN_POINT('Ctrl Pts',(44.3252718681562,36.7155588135129,49.3731682286675));
#32456=CARTESIAN_POINT('Ctrl Pts',(44.3701913137622,36.7197853383426,49.3078933963054));
#32457=CARTESIAN_POINT('Ctrl Pts',(44.4116842236564,36.7240118631722,49.2406115529013));
#32458=CARTESIAN_POINT('Ctrl Pts',(44.4532529811988,36.7282461139475,49.173206720543));
#32459=CARTESIAN_POINT('Ctrl Pts',(44.4913824603497,36.7324803647229,49.1037879585842));
#32460=CARTESIAN_POINT('Ctrl Pts',(44.5258941761743,36.7367146154982,49.032746044586));
#32461=CARTESIAN_POINT('Ctrl Pts',(44.5588092651896,36.7407529757435,48.9649907659165));
#32462=CARTESIAN_POINT('Ctrl Pts',(44.5884338210638,36.7447913359888,48.8957595415893));
#32463=CARTESIAN_POINT('Ctrl Pts',(44.6146550345483,36.7488296962341,48.8254050634992));
#32464=CARTESIAN_POINT('Ctrl Pts',(44.6421562850433,36.7530651965004,48.7516161014992));
#32465=CARTESIAN_POINT('Ctrl Pts',(44.6660179661831,36.7573006967666,48.6763109305192));
#32466=CARTESIAN_POINT('Ctrl Pts',(44.6860732565879,36.7615361970329,48.5998829105863));
#32467=CARTESIAN_POINT('Ctrl Pts',(44.7060994731875,36.7657655571681,48.5235656870231));
#32468=CARTESIAN_POINT('Ctrl Pts',(44.7223301388211,36.7699949173034,48.4461292971214));
#32469=CARTESIAN_POINT('Ctrl Pts',(44.7346471281255,36.7742242774386,48.3679853638874));
#32470=CARTESIAN_POINT('Ctrl Pts',(44.7469497337401,36.7784486985581,48.289932686566));
#32471=CARTESIAN_POINT('Ctrl Pts',(44.7553476724894,36.7826731196776,48.2111745690717));
#32472=CARTESIAN_POINT('Ctrl Pts',(44.7597734864983,36.7868975407971,48.1321345273571));
#32473=CARTESIAN_POINT('Ctrl Pts',(44.7641964702827,36.7911192604791,48.0531450302552));
#32474=CARTESIAN_POINT('Ctrl Pts',(44.7646523447103,36.7953409801612,47.9738744341119));
#32475=CARTESIAN_POINT('Ctrl Pts',(44.7611254259176,36.7995626998432,47.8947518931982));
#32476=CARTESIAN_POINT('Ctrl Pts',(44.7575996611171,36.8037830381974,47.8156552408277));
#32477=CARTESIAN_POINT('Ctrl Pts',(44.7500937116094,36.8080033765515,47.736707016026));
#32478=CARTESIAN_POINT('Ctrl Pts',(44.7386439948903,36.8122237149057,47.6583353895069));
#32479=CARTESIAN_POINT('Ctrl Pts',(44.7271944489615,36.8164439903069,47.5799649320218));
#32480=CARTESIAN_POINT('Ctrl Pts',(44.7118013219268,36.8206642657082,47.5021715199513));
#32481=CARTESIAN_POINT('Ctrl Pts',(44.6925525928199,36.8248845411095,47.4253757314081));
#32482=CARTESIAN_POINT('Ctrl Pts',(44.6732846104996,36.8291090377693,47.3485031291859));
#32483=CARTESIAN_POINT('Ctrl Pts',(44.6501534366463,36.8333335344292,47.27263060019));
#32484=CARTESIAN_POINT('Ctrl Pts',(44.6232975227603,36.837558031089,47.1981654995026));
#32485=CARTESIAN_POINT('Ctrl Pts',(44.5964287154202,36.8417845559187,47.1236646483149));
#32486=CARTESIAN_POINT('Ctrl Pts',(44.5658317871443,36.8460110807483,47.0505730050612));
#32487=CARTESIAN_POINT('Ctrl Pts',(44.5316931795947,36.850237605578,46.9792773986193));
#32488=CARTESIAN_POINT('Ctrl Pts',(44.4974921678151,36.8544718563533,46.9078514661991));
#32489=CARTESIAN_POINT('Ctrl Pts',(44.4597367643785,36.8587061071286,46.8382285446606));
#32490=CARTESIAN_POINT('Ctrl Pts',(44.4186590653512,36.862940357904,46.7707701521784));
#32491=CARTESIAN_POINT('Ctrl Pts',(44.3794817573638,36.8669787181493,46.7064326093951));
#32492=CARTESIAN_POINT('Ctrl Pts',(44.3372829872294,36.8710170783946,46.6440640232978));
#32493=CARTESIAN_POINT('Ctrl Pts',(44.2922983498868,36.8750554386399,46.5839500729439));
#32494=CARTESIAN_POINT('Ctrl Pts',(44.245117704311,36.8792909389062,46.5209015489732));
#32495=CARTESIAN_POINT('Ctrl Pts',(44.1946929083828,36.8835264391724,46.4600937488261));
#32496=CARTESIAN_POINT('Ctrl Pts',(44.1412645399784,36.8877619394387,46.4018797783916));
#32497=CARTESIAN_POINT('Ctrl Pts',(44.0879136257495,36.8919912995739,46.3437501997365));
#32498=CARTESIAN_POINT('Ctrl Pts',(44.0315681004492,36.8962206597092,46.2882073265073));
#32499=CARTESIAN_POINT('Ctrl Pts',(43.9725102457625,36.9004500198445,46.2355731899929));
#32500=CARTESIAN_POINT('Ctrl Pts',(43.9135213584058,36.904674440964,46.1830005192374));
#32501=CARTESIAN_POINT('Ctrl Pts',(43.8518267845221,36.9088988620835,46.1333301457761));
#32502=CARTESIAN_POINT('Ctrl Pts',(43.7877462187777,36.913123283203,46.0868479221012));
#32503=CARTESIAN_POINT('Ctrl Pts',(43.7237066313438,36.917345002885,46.0403954229298));
#32504=CARTESIAN_POINT('Ctrl Pts',(43.6572844593278,36.921566722567,45.9971273018812));
#32505=CARTESIAN_POINT('Ctrl Pts',(43.5888321486797,36.9257884422491,45.9572889183329));
#32506=CARTESIAN_POINT('Ctrl Pts',(43.5204022353227,36.9300087806032,45.9174635697262));
#32507=CARTESIAN_POINT('Ctrl Pts',(43.4499439076649,36.9342291189574,45.8810659662195));
#32508=CARTESIAN_POINT('Ctrl Pts',(43.3778369708489,36.9384494573115,45.8482971163888));
#32509=CARTESIAN_POINT('Ctrl Pts',(43.3057311096197,36.9426697327128,45.8155287553562));
#32510=CARTESIAN_POINT('Ctrl Pts',(43.2319771159644,36.9468900081141,45.7863892333742));
#32511=CARTESIAN_POINT('Ctrl Pts',(43.1569763037883,36.9511102835154,45.7610320867857));
#32512=CARTESIAN_POINT('Ctrl Pts',(43.0819004733276,36.9553347801752,45.7356495771434));
#32513=CARTESIAN_POINT('Ctrl Pts',(43.005575778778,36.9595592768351,45.7140571511106));
#32514=CARTESIAN_POINT('Ctrl Pts',(42.92841971828,36.9637837734949,45.6963587427221));
#32515=CARTESIAN_POINT('Ctrl Pts',(42.8512266153592,36.9680102983246,45.678651837374));
#32516=CARTESIAN_POINT('Ctrl Pts',(42.7732018141652,36.9722368231542,45.6648427558669));
#32517=CARTESIAN_POINT('Ctrl Pts',(42.6947715119937,36.9764633479838,45.654983966661));
#32518=CARTESIAN_POINT('Ctrl Pts',(42.6161978418591,36.9806975987592,45.6451071559189));
#32519=CARTESIAN_POINT('Ctrl Pts',(42.5372176588444,36.9849318495345,45.6391951018615));
#32520=CARTESIAN_POINT('Ctrl Pts',(42.4582605718773,36.9891661003099,45.6372481834385));
#32521=CARTESIAN_POINT('Ctrl Pts',(42.3829563024771,36.9932044605552,45.6353913359401));
#32522=CARTESIAN_POINT('Ctrl Pts',(42.3076733956048,36.9972428208005,45.6371408117188));
#32523=CARTESIAN_POINT('Ctrl Pts',(42.2327795702227,37.0012811810458,45.6424530187576));
#32524=CARTESIAN_POINT('Ctrl Pts',(42.1542296643014,37.0055166813121,45.6480245510035));
#32525=CARTESIAN_POINT('Ctrl Pts',(42.0758092122744,37.0097521815783,45.6575367172658));
#32526=CARTESIAN_POINT('Ctrl Pts',(41.9979453366885,37.0139876818446,45.6709782120793));
#32527=CARTESIAN_POINT('Ctrl Pts',(41.920194339007,37.0182170419798,45.6844002209918));
#32528=CARTESIAN_POINT('Ctrl Pts',(41.8429987740852,37.0224464021151,45.7017401674841));
#32529=CARTESIAN_POINT('Ctrl Pts',(41.7667821912645,37.0266757622504,45.7229348609229));
#32530=CARTESIAN_POINT('Ctrl Pts',(41.6906546136108,37.0309001833699,45.744104803354));
#32531=CARTESIAN_POINT('Ctrl Pts',(41.6155041960551,37.0351246044893,45.7691204222288));
#32532=CARTESIAN_POINT('Ctrl Pts',(41.5417443006599,37.0393490256088,45.7978674891256));
#32533=CARTESIAN_POINT('Ctrl Pts',(41.4680315733236,37.0435707452909,45.8265961728164));
#32534=CARTESIAN_POINT('Ctrl Pts',(41.3957080393815,37.0477924649729,45.8590513984745));
#32535=CARTESIAN_POINT('Ctrl Pts',(41.3251707232159,37.0520141846549,45.895069486499));
#32536=CARTESIAN_POINT('Ctrl Pts',(41.2546564865458,37.0562345230091,45.9310757895655));
#32537=CARTESIAN_POINT('Ctrl Pts',(41.185927724836,37.0604548613632,45.9706424269158));
#32538=CARTESIAN_POINT('Ctrl Pts',(41.1193589632904,37.0646751997174,46.013558715694));
#32539=CARTESIAN_POINT('Ctrl Pts',(41.0527911947207,37.0688954751187,46.0564743643095));
#32540=CARTESIAN_POINT('Ctrl Pts',(40.9883837560255,37.07311575052,46.1027393095946));
#32541=CARTESIAN_POINT('Ctrl Pts',(40.9264828829859,37.0773360259213,46.1520990971466));
#32542=CARTESIAN_POINT('Ctrl Pts',(40.8645200946529,37.0815605225811,46.2015082559849));
#32543=CARTESIAN_POINT('Ctrl Pts',(40.8050692481665,37.085785019241,46.2540181475494));
#32544=CARTESIAN_POINT('Ctrl Pts',(40.7484436179076,37.0900095159008,46.3093338716145));
#32545=CARTESIAN_POINT('Ctrl Pts',(40.6917908018319,37.0942360407304,46.364676152614));
#32546=CARTESIAN_POINT('Ctrl Pts',(40.6379662233171,37.0984625655601,46.4228266047286));
#32547=CARTESIAN_POINT('Ctrl Pts',(40.5872445789206,37.1026890903897,46.4834551690612));
#32548=CARTESIAN_POINT('Ctrl Pts',(40.5364302170585,37.1069233411651,46.5441945603769));
#32549=CARTESIAN_POINT('Ctrl Pts',(40.4887304068365,37.1111575919404,46.6074207400574));
#32550=CARTESIAN_POINT('Ctrl Pts',(40.4443778817356,37.1153918427157,46.6727725999457));
#32551=CARTESIAN_POINT('Ctrl Pts',(40.4020772520258,37.119430202961,46.7351010653418));
#32552=CARTESIAN_POINT('Ctrl Pts',(40.3628211983546,37.1234685632063,46.7993625544527));
#32553=CARTESIAN_POINT('Ctrl Pts',(40.3267719914411,37.1275069234516,46.8652242224004));
#32554=CARTESIAN_POINT('Ctrl Pts',(40.2870375488266,37.1319581168942,46.9378187921463));
#32555=CARTESIAN_POINT('Ctrl Pts',(40.2510607328626,37.1364093103368,47.0126102428298));
#32556=CARTESIAN_POINT('Ctrl Pts',(40.2190773612624,37.1408605037794,47.0891943759825));
#32557=CARTESIAN_POINT('Ctrl Pts',(40.1871847111452,37.1452990713214,47.1655612766866));
#32558=CARTESIAN_POINT('Ctrl Pts',(40.1592630955621,37.1497376388635,47.243710364221));
#32559=CARTESIAN_POINT('Ctrl Pts',(40.1355019575057,37.1541762064055,47.3232141724007));
#32560=CARTESIAN_POINT('Ctrl Pts',(40.1117812132541,37.1586072284069,47.4025828245411));
#32561=CARTESIAN_POINT('Ctrl Pts',(40.09220699208,37.1630382504084,47.4833012358813));
#32562=CARTESIAN_POINT('Ctrl Pts',(40.0769205382994,37.1674692724099,47.5649227016671));
#32563=CARTESIAN_POINT('Ctrl Pts',(40.0616673408257,37.1718906545413,47.6463665966073));
#32564=CARTESIAN_POINT('Ctrl Pts',(40.0506834047931,37.1763120366727,47.7287092417238));
#32565=CARTESIAN_POINT('Ctrl Pts',(40.04405967581,37.1807334188041,47.8114910353449));
#32566=CARTESIAN_POINT('Ctrl Pts',(40.039046125874,37.18407999596,47.8741491931837));
#32567=CARTESIAN_POINT('Ctrl Pts',(40.0365295766833,37.1874265731158,47.9370585780173));
#32568=CARTESIAN_POINT('Ctrl Pts',(40.0365300000534,37.1907731502717,48.0000158936656));
#32569=CARTESIAN_POINT('',(40.0365309678968,37.9845231502406,48.0021389691475));
#32570=CARTESIAN_POINT('Ctrl Pts',(40.0365300000535,37.1907731503223,48.0000158946174));
#32571=CARTESIAN_POINT('Ctrl Pts',(40.0365305596263,37.1951960923782,48.0832222712021));
#32572=CARTESIAN_POINT('Ctrl Pts',(40.0409293600083,37.199619034434,48.1663427328736));
#32573=CARTESIAN_POINT('Ctrl Pts',(40.0496735435784,37.2040419764899,48.2489096003468));
#32574=CARTESIAN_POINT('Ctrl Pts',(40.0584419788841,37.2084771854452,48.3317054645947));
#32575=CARTESIAN_POINT('Ctrl Pts',(40.0715798424985,37.2129123944006,48.4139442671402));
#32576=CARTESIAN_POINT('Ctrl Pts',(40.0889826968161,37.217347603356,48.4951660986827));
#32577=CARTESIAN_POINT('Ctrl Pts',(40.106410421701,37.2217891507062,48.5765040050364));
#32578=CARTESIAN_POINT('Ctrl Pts',(40.1281151866957,37.2262306980565,48.6568216568936));
#32579=CARTESIAN_POINT('Ctrl Pts',(40.153942725368,37.2306722454067,48.7356746291485));
#32580=CARTESIAN_POINT('Ctrl Pts',(40.1798413381919,37.235126015339,48.8147445949066));
#32581=CARTESIAN_POINT('Ctrl Pts',(40.2098852628717,37.2395797852712,48.8923414489889));
#32582=CARTESIAN_POINT('Ctrl Pts',(40.2438718313794,37.2440335552035,48.9680401651691));
#32583=CARTESIAN_POINT('Ctrl Pts',(40.268543027072,37.2472665920881,49.0229906330324));
#32584=CARTESIAN_POINT('Ctrl Pts',(40.2952907833685,37.2504996289728,49.076941352625));
#32585=CARTESIAN_POINT('Ctrl Pts',(40.3240230140222,37.2537326658574,49.1297389054956));
#32586=CARTESIAN_POINT('Ctrl Pts',(40.3616642086403,37.2579681661237,49.1989073242974));
#32587=CARTESIAN_POINT('Ctrl Pts',(40.4028376148377,37.2622036663899,49.2663239337141));
#32588=CARTESIAN_POINT('Ctrl Pts',(40.4473558357842,37.2664391666562,49.331604749486));
#32589=CARTESIAN_POINT('Ctrl Pts',(40.4918095194408,37.2706685267914,49.396790928796));
#32590=CARTESIAN_POINT('Ctrl Pts',(40.5395981265472,37.2748978869267,49.4598470785257));
#32591=CARTESIAN_POINT('Ctrl Pts',(40.5904885275618,37.279127247062,49.520413980472));
#32592=CARTESIAN_POINT('Ctrl Pts',(40.6413194991391,37.2833516681814,49.580910152834));
#32593=CARTESIAN_POINT('Ctrl Pts',(40.6952447661712,37.2875760893009,49.6389224965377));
#32594=CARTESIAN_POINT('Ctrl Pts',(40.7519889800698,37.2918005104204,49.6941222267265));
#32595=CARTESIAN_POINT('Ctrl Pts',(40.8086969071162,37.2960222301025,49.7492866577312));
#32596=CARTESIAN_POINT('Ctrl Pts',(40.8682198676082,37.3002439497845,49.8016417186962));
#32597=CARTESIAN_POINT('Ctrl Pts',(40.9302442879937,37.3044656694665,49.8508939969444));
#32598=CARTESIAN_POINT('Ctrl Pts',(40.992248414265,37.3086860078207,49.9001301600665));
#32599=CARTESIAN_POINT('Ctrl Pts',(41.0567520079436,37.3129063461748,49.9462652647038));
#32600=CARTESIAN_POINT('Ctrl Pts',(41.1234080529754,37.317126684529,49.989045862139));
#32601=CARTESIAN_POINT('Ctrl Pts',(41.1900631037294,37.3213469599303,50.0318258214354));
#32602=CARTESIAN_POINT('Ctrl Pts',(41.2588701462979,37.3255672353316,50.0712511206032));
#32603=CARTESIAN_POINT('Ctrl Pts',(41.3294540638705,37.3297875107329,50.1071122038317));
#32604=CARTESIAN_POINT('Ctrl Pts',(41.4001085818039,37.3340120073927,50.1430091564977));
#32605=CARTESIAN_POINT('Ctrl Pts',(41.4725431056581,37.3382365040526,50.1753345584918));
#32606=CARTESIAN_POINT('Ctrl Pts',(41.5463593814678,37.3424610007124,50.2039256192739));
#32607=CARTESIAN_POINT('Ctrl Pts',(41.6202110962784,37.3466875255421,50.2325304065495));
#32608=CARTESIAN_POINT('Ctrl Pts',(41.6954454383171,37.3509140503717,50.2573971335446));
#32609=CARTESIAN_POINT('Ctrl Pts',(41.7716481565412,37.3551405752014,50.2784126934605));
#32610=CARTESIAN_POINT('Ctrl Pts',(41.8479901707795,37.3593748259767,50.2994666691154));
#32611=CARTESIAN_POINT('Ctrl Pts',(41.9253036390266,37.363609076752,50.3166553083815));
#32612=CARTESIAN_POINT('Ctrl Pts',(42.0031634563534,37.3678433275274,50.3299165647136));
#32613=CARTESIAN_POINT('Ctrl Pts',(42.0774212194581,37.3718816877727,50.3425643112019));
#32614=CARTESIAN_POINT('Ctrl Pts',(42.152175538726,37.375920048018,50.3516400196285));
#32615=CARTESIAN_POINT('Ctrl Pts',(42.2270562460282,37.3799584082634,50.3571340434651));
#32616=CARTESIAN_POINT('Ctrl Pts',(42.3055923934863,37.3841939085296,50.3628962682319));
#32617=CARTESIAN_POINT('Ctrl Pts',(42.384566116487,37.3884294087959,50.3647400899557));
#32618=CARTESIAN_POINT('Ctrl Pts',(42.4635530934007,37.3926649090621,50.362615382414));
#32619=CARTESIAN_POINT('Ctrl Pts',(42.5424255642691,37.3968942691974,50.3604937550238));
#32620=CARTESIAN_POINT('Ctrl Pts',(42.6213107856818,37.4011236293326,50.3544150355381));
#32621=CARTESIAN_POINT('Ctrl Pts',(42.6997805239498,37.4053529894679,50.3443809584537));
#32622=CARTESIAN_POINT('Ctrl Pts',(42.7781586258327,37.4095774105874,50.3343585990911));
#32623=CARTESIAN_POINT('Ctrl Pts',(42.8561217456078,37.4138018317069,50.3203901202401));
#32624=CARTESIAN_POINT('Ctrl Pts',(42.9332444047402,37.4180262528264,50.3025292279824));
#32625=CARTESIAN_POINT('Ctrl Pts',(43.0103177453898,37.4222479725084,50.2846797574278));
#32626=CARTESIAN_POINT('Ctrl Pts',(43.086551236123,37.4264696921904,50.2629429194557));
#32627=CARTESIAN_POINT('Ctrl Pts',(43.1615284680203,37.4306914118725,50.2374237044634));
#32628=CARTESIAN_POINT('Ctrl Pts',(43.2364811677012,37.4349117502266,50.2119128392446));
#32629=CARTESIAN_POINT('Ctrl Pts',(43.3101779807556,37.4391320885808,50.1826222055372));
#32630=CARTESIAN_POINT('Ctrl Pts',(43.3822180169668,37.4433524269349,50.149706539983));
#32631=CARTESIAN_POINT('Ctrl Pts',(43.4542569785896,37.4475727023362,50.1167913654169));
#32632=CARTESIAN_POINT('Ctrl Pts',(43.5246387861474,37.4517929777375,50.0802514627571));
#32633=CARTESIAN_POINT('Ctrl Pts',(43.59298426232,37.4560132531388,50.0402889478593));
#32634=CARTESIAN_POINT('Ctrl Pts',(43.6613980998906,37.4602377497986,50.0002864611369));
#32635=CARTESIAN_POINT('Ctrl Pts',(43.7277711311593,37.4644622464585,49.9568547609598));
#32636=CARTESIAN_POINT('Ctrl Pts',(43.7917509927071,37.4686867431183,49.9102407217937));
#32637=CARTESIAN_POINT('Ctrl Pts',(43.8557615708191,37.472913267948,49.8636043033493));
#32638=CARTESIAN_POINT('Ctrl Pts',(43.9173763248841,37.4771397927776,49.8137827978025));
#32639=CARTESIAN_POINT('Ctrl Pts',(43.9762760226218,37.4813663176073,49.7610634120916));
#32640=CARTESIAN_POINT('Ctrl Pts',(44.0352833870323,37.4856005683826,49.7082476571109));
#32641=CARTESIAN_POINT('Ctrl Pts',(44.0915654434044,37.4898348191579,49.6525237679543));
#32642=CARTESIAN_POINT('Ctrl Pts',(44.1448400307035,37.4940690699333,49.5942157031452));
#32643=CARTESIAN_POINT('Ctrl Pts',(44.1956499583269,37.4981074301786,49.5386051634299));
#32644=CARTESIAN_POINT('Ctrl Pts',(44.2437243343442,37.5021457904239,49.4806445638542));
#32645=CARTESIAN_POINT('Ctrl Pts',(44.2888547879471,37.5061841506692,49.420640007514));
#32646=CARTESIAN_POINT('Ctrl Pts',(44.3361883680735,37.5104196509355,49.357706217828));
#32647=CARTESIAN_POINT('Ctrl Pts',(44.3804631859095,37.5146551512017,49.2922845921318));
#32648=CARTESIAN_POINT('Ctrl Pts',(44.4214075295047,37.518890651468,49.2247048789654));
#32649=CARTESIAN_POINT('Ctrl Pts',(44.4622925167979,37.5231200116032,49.1572231349325));
#32650=CARTESIAN_POINT('Ctrl Pts',(44.4998563765131,37.5273493717385,49.0875899141883));
#32651=CARTESIAN_POINT('Ctrl Pts',(44.5338688966298,37.5315787318737,49.016166311632));
#32652=CARTESIAN_POINT('Ctrl Pts',(44.5678416971748,37.5358031529932,48.9448261170354));
#32653=CARTESIAN_POINT('Ctrl Pts',(44.598271198688,37.5400275741127,48.8717001169798));
#32654=CARTESIAN_POINT('Ctrl Pts',(44.6249723892253,37.5442519952322,48.7971752053879));
#32655=CARTESIAN_POINT('Ctrl Pts',(44.6516565048559,37.5484737149142,48.7226979510682));
#32656=CARTESIAN_POINT('Ctrl Pts',(44.6746168837267,37.5526954345963,48.6468240014116));
#32657=CARTESIAN_POINT('Ctrl Pts',(44.6937165520271,37.5569171542783,48.5699603669176));
#32658=CARTESIAN_POINT('Ctrl Pts',(44.7128099710011,37.5611374926325,48.4931218818626));
#32659=CARTESIAN_POINT('Ctrl Pts',(44.7280450746151,37.5653578309866,48.4152948101251));
#32660=CARTESIAN_POINT('Ctrl Pts',(44.7393351225324,37.5695781693408,48.3369000228352));
#32661=CARTESIAN_POINT('Ctrl Pts',(44.7506250020412,37.5737984447421,48.2585064049247));
#32662=CARTESIAN_POINT('Ctrl Pts',(44.7579698772445,37.5780187201433,48.1795455530439));
#32663=CARTESIAN_POINT('Ctrl Pts',(44.7613346015463,37.5822389955446,48.100445708919));
#32664=CARTESIAN_POINT('Ctrl Pts',(44.7647026913562,37.5864634922045,48.0212667465227));
#32665=CARTESIAN_POINT('Ctrl Pts',(44.7640826575644,37.5906879888643,47.9419489842108));
#32666=CARTESIAN_POINT('Ctrl Pts',(44.7594915029145,37.5949124855242,47.8629223264931));
#32667=CARTESIAN_POINT('Ctrl Pts',(44.7548981440633,37.5991390103538,47.7838577282837));
#32668=CARTESIAN_POINT('Ctrl Pts',(44.7463299171458,37.6033655351834,47.7050849803251));
#32669=CARTESIAN_POINT('Ctrl Pts',(44.733855669311,37.6075920600131,47.6270279424343));
#32670=CARTESIAN_POINT('Ctrl Pts',(44.7213586189694,37.6118263107884,47.5488282188951));
#32671=CARTESIAN_POINT('Ctrl Pts',(44.7049413777103,37.6160605615638,47.4713472800671));
#32672=CARTESIAN_POINT('Ctrl Pts',(44.6847237570263,37.6202948123391,47.3949976901039));
#32673=CARTESIAN_POINT('Ctrl Pts',(44.6654414707478,37.6243331725844,47.3221802862202));
#32674=CARTESIAN_POINT('Ctrl Pts',(44.6427028080316,37.6283715328297,47.2503921956308));
#32675=CARTESIAN_POINT('Ctrl Pts',(44.6166524833386,37.632409893075,47.1799742632035));
#32676=CARTESIAN_POINT('Ctrl Pts',(44.5893304638875,37.6366453933413,47.1061187492256));
#32677=CARTESIAN_POINT('Ctrl Pts',(44.5582613401604,37.6408808936075,47.0334898420745));
#32678=CARTESIAN_POINT('Ctrl Pts',(44.5235754460815,37.6451163938738,46.96249445028));
#32679=CARTESIAN_POINT('Ctrl Pts',(44.4889398355394,37.649345754009,46.891601979269));
#32680=CARTESIAN_POINT('Ctrl Pts',(44.4506980709443,37.6535751141443,46.8223387391732));
#32681=CARTESIAN_POINT('Ctrl Pts',(44.4090293004974,37.6578044742796,46.7550936940304));
#32682=CARTESIAN_POINT('Ctrl Pts',(44.3674091905354,37.6620288953991,46.6879271771586));
#32683=CARTESIAN_POINT('Ctrl Pts',(44.322370273441,37.6662533165185,46.6227745686656));
#32684=CARTESIAN_POINT('Ctrl Pts',(44.2741378479749,37.670477737638,46.5600007751086));
#32685=CARTESIAN_POINT('Ctrl Pts',(44.2259362662332,37.6746994573201,46.497267124206));
#32686=CARTESIAN_POINT('Ctrl Pts',(44.1745455146176,37.6789211770021,46.43690964014));
#32687=CARTESIAN_POINT('Ctrl Pts',(44.1202337987159,37.6831428966841,46.3792637109463));
#32688=CARTESIAN_POINT('Ctrl Pts',(44.0659398533657,37.6873632350383,46.3216366432439));
#32689=CARTESIAN_POINT('Ctrl Pts',(44.0087271630969,37.6915835733925,46.266719710067));
#32690=CARTESIAN_POINT('Ctrl Pts',(43.9489027665584,37.6958039117466,46.2148135501725));
#32691=CARTESIAN_POINT('Ctrl Pts',(43.8890792623932,37.7000241871479,46.1629081645386));
#32692=CARTESIAN_POINT('Ctrl Pts',(43.8266444847843,37.7042444625492,46.1140137694976));
#32693=CARTESIAN_POINT('Ctrl Pts',(43.7619395830336,37.7084647379505,46.0683915994523));
#32694=CARTESIAN_POINT('Ctrl Pts',(43.6971699613073,37.7126892346103,46.0227237966088));
#32695=CARTESIAN_POINT('Ctrl Pts',(43.6301260640298,37.7169137312702,45.9803350280738));
#32696=CARTESIAN_POINT('Ctrl Pts',(43.5611786512994,37.72113822793,45.9414435687437));
#32697=CARTESIAN_POINT('Ctrl Pts',(43.4921981370964,37.7253647527597,45.9025334377257));
#32698=CARTESIAN_POINT('Ctrl Pts',(43.4213127073509,37.7295912775893,45.8671241708138));
#32699=CARTESIAN_POINT('Ctrl Pts',(43.3489160857868,37.7338178024189,45.8353871701768));
#32700=CARTESIAN_POINT('Ctrl Pts',(43.2763871256255,37.7380520531943,45.8035921553667));
#32701=CARTESIAN_POINT('Ctrl Pts',(43.2023418936577,37.7422863039696,45.7754829875554));
#32702=CARTESIAN_POINT('Ctrl Pts',(43.1271921849133,37.746520554745,45.7511820956109));
#32703=CARTESIAN_POINT('Ctrl Pts',(43.0555191517504,37.7505589149903,45.7280054437871));
#32704=CARTESIAN_POINT('Ctrl Pts',(42.9828419297207,37.7545972752356,45.7082925512877));
#32705=CARTESIAN_POINT('Ctrl Pts',(42.9095254682162,37.7586356354809,45.692106103362));
#32706=CARTESIAN_POINT('Ctrl Pts',(42.8326299281061,37.7628711357472,45.6751294840575));
#32707=CARTESIAN_POINT('Ctrl Pts',(42.7547388472413,37.7671066360134,45.661967868471));
#32708=CARTESIAN_POINT('Ctrl Pts',(42.6762649566596,37.7713421362797,45.6527317761658));
#32709=CARTESIAN_POINT('Ctrl Pts',(42.5979048283107,37.7755714964149,45.6435090732628));
#32710=CARTESIAN_POINT('Ctrl Pts',(42.5189640302368,37.7798008565502,45.6382006471894));
#32711=CARTESIAN_POINT('Ctrl Pts',(42.4398666097627,37.7840302166855,45.6368662555145));
#32712=CARTESIAN_POINT('Ctrl Pts',(42.3608615586765,37.7882546378049,45.6355334221324));
#32713=CARTESIAN_POINT('Ctrl Pts',(42.2817007154983,37.7924790589244,45.6381654087955));
#32714=CARTESIAN_POINT('Ctrl Pts',(42.2028128615963,37.7967034800439,45.6447701442644));
#32715=CARTESIAN_POINT('Ctrl Pts',(42.1239754549856,37.8009251997259,45.6513706561299));
#32716=CARTESIAN_POINT('Ctrl Pts',(42.0454111576157,37.805146919408,45.6619388354037));
#32717=CARTESIAN_POINT('Ctrl Pts',(41.9675471371779,37.80936863909,45.6764305557318));
#32718=CARTESIAN_POINT('Ctrl Pts',(41.8897085935008,37.8135889774442,45.6909175344335));
#32719=CARTESIAN_POINT('Ctrl Pts',(41.8125703328633,37.8178093157983,45.7093254192435));
#32720=CARTESIAN_POINT('Ctrl Pts',(41.7365513061938,37.8220296541525,45.7315586250496));
#32721=CARTESIAN_POINT('Ctrl Pts',(41.6605334134655,37.8262499295538,45.7537914992131));
#32722=CARTESIAN_POINT('Ctrl Pts',(41.5856351716246,37.830470204955,45.7798494479168));
#32723=CARTESIAN_POINT('Ctrl Pts',(41.5122608450046,37.8346904803563,45.8095868806118));
#32724=CARTESIAN_POINT('Ctrl Pts',(41.4388131269647,37.8389149770162,45.8393540576671));
#32725=CARTESIAN_POINT('Ctrl Pts',(41.3668928050917,37.843139473676,45.8728078939457));
#32726=CARTESIAN_POINT('Ctrl Pts',(41.2968840327574,37.8473639703359,45.9097546546603));
#32727=CARTESIAN_POINT('Ctrl Pts',(41.2268416493946,37.8515904951655,45.946719153418));
#32728=CARTESIAN_POINT('Ctrl Pts',(41.1587130479057,37.8558170199952,45.9871796772976));
#32729=CARTESIAN_POINT('Ctrl Pts',(41.0928553835091,37.8600435448248,46.0308978207115));
#32730=CARTESIAN_POINT('Ctrl Pts',(41.0268773335099,37.8642777956001,46.0746958794258));
#32731=CARTESIAN_POINT('Ctrl Pts',(40.9631788941426,37.8685120463755,46.1217631771429));
#32732=CARTESIAN_POINT('Ctrl Pts',(40.9020858091279,37.8727462971508,46.1718196156604));
#32733=CARTESIAN_POINT('Ctrl Pts',(40.8438190935089,37.8767846573961,46.2195602767729));
#32734=CARTESIAN_POINT('Ctrl Pts',(40.7879222390666,37.8808230176414,46.2700193532216));
#32735=CARTESIAN_POINT('Ctrl Pts',(40.7346454003701,37.8848613778867,46.3229238245114));
#32736=CARTESIAN_POINT('Ctrl Pts',(40.6795730505441,37.8890358370625,46.3776112575783));
#32737=CARTESIAN_POINT('Ctrl Pts',(40.627078497172,37.8932102962383,46.4351326267141));
#32738=CARTESIAN_POINT('Ctrl Pts',(40.5774737031317,37.897384755414,46.4952115304391));
#32739=CARTESIAN_POINT('Ctrl Pts',(40.5279334280921,37.9015537850353,46.5552122919017));
#32740=CARTESIAN_POINT('Ctrl Pts',(40.4812757654333,37.9057228146565,46.6177636240106));
#32741=CARTESIAN_POINT('Ctrl Pts',(40.4377767362262,37.9098918442777,46.6825515934182));
#32742=CARTESIAN_POINT('Ctrl Pts',(40.3943197909756,37.9140568404926,46.7472768824825));
#32743=CARTESIAN_POINT('Ctrl Pts',(40.3540156865703,37.9182218367075,46.8142341180397));
#32744=CARTESIAN_POINT('Ctrl Pts',(40.317099846657,37.9223868329223,46.8830768190679));
#32745=CARTESIAN_POINT('Ctrl Pts',(40.2802074295698,37.9265491864781,46.9518758399137));
#32746=CARTESIAN_POINT('Ctrl Pts',(40.2466992389077,37.9307115400338,47.0225575270902));
#32747=CARTESIAN_POINT('Ctrl Pts',(40.2167661554737,37.9348738935895,47.0947484211476));
#32748=CARTESIAN_POINT('Ctrl Pts',(40.1868300921433,37.9390366615155,47.1669465019482));
#32749=CARTESIAN_POINT('Ctrl Pts',(40.1604700500129,37.9431994294416,47.2406536501797));
#32750=CARTESIAN_POINT('Ctrl Pts',(40.1378293684167,37.9473621973677,47.3154750008202));
#32751=CARTESIAN_POINT('Ctrl Pts',(40.1151890988125,37.9515248895439,47.3902949899385));
#32752=CARTESIAN_POINT('Ctrl Pts',(40.0962681870432,37.9556875817202,47.4662286750739));
#32753=CARTESIAN_POINT('Ctrl Pts',(40.0811598566571,37.9598502738965,47.5428667256461));
#32754=CARTESIAN_POINT('Ctrl Pts',(40.0660351583016,37.9640174758244,47.6195878038747));
#32755=CARTESIAN_POINT('Ctrl Pts',(40.0547313773445,37.9681846777524,47.697014294305));
#32756=CARTESIAN_POINT('Ctrl Pts',(40.0472902807315,37.9723518796803,47.7747281247921));
#32757=CARTESIAN_POINT('Ctrl Pts',(40.0400458033653,37.9764089698671,47.8503884898277));
#32758=CARTESIAN_POINT('Ctrl Pts',(40.0364623514731,37.9804660600538,47.9263207683451));
#32759=CARTESIAN_POINT('Ctrl Pts',(40.0365309678968,37.9845231502406,48.0021389691475));
#32760=CARTESIAN_POINT('',(40.0365302498269,38.7782731502987,47.9989133001977));
#32761=CARTESIAN_POINT('Ctrl Pts',(40.0365309678973,37.9845231502717,48.0021389697293));
#32762=CARTESIAN_POINT('Ctrl Pts',(40.036631185905,37.9904487488876,48.1128755333861));
#32763=CARTESIAN_POINT('Ctrl Pts',(40.0445174814273,37.9963743475034,48.2232732264897));
#32764=CARTESIAN_POINT('Ctrl Pts',(40.0600271988848,38.0022999461193,48.3324420715571));
#32765=CARTESIAN_POINT('Ctrl Pts',(40.0676937429487,38.005229004177,48.3864048702607));
#32766=CARTESIAN_POINT('Ctrl Pts',(40.0772222871004,38.0081580622348,48.440067915169));
#32767=CARTESIAN_POINT('Ctrl Pts',(40.0885892018617,38.0110871202926,48.493326021156));
#32768=CARTESIAN_POINT('Ctrl Pts',(40.1050260800485,38.0153226205589,48.5703387391143));
#32769=CARTESIAN_POINT('Ctrl Pts',(40.1253473352508,38.0195581208251,48.6466754615364));
#32770=CARTESIAN_POINT('Ctrl Pts',(40.1494823962719,38.0237936210914,48.7219147845903));
#32771=CARTESIAN_POINT('Ctrl Pts',(40.1735824691154,38.0280229812266,48.7970450345077));
#32772=CARTESIAN_POINT('Ctrl Pts',(40.2014852263923,38.0322523413619,48.8710806011245));
#32773=CARTESIAN_POINT('Ctrl Pts',(40.2330692122343,38.0364817014972,48.9436108318227));
#32774=CARTESIAN_POINT('Ctrl Pts',(40.2646163145292,38.0407061226167,49.0160563622492));
#32775=CARTESIAN_POINT('Ctrl Pts',(40.2998359162372,38.0449305437362,49.0869996219856));
#32776=CARTESIAN_POINT('Ctrl Pts',(40.3385574354109,38.0491549648557,49.156047141686));
#32777=CARTESIAN_POINT('Ctrl Pts',(40.377254192905,38.0533766845377,49.2250505068028));
#32778=CARTESIAN_POINT('Ctrl Pts',(40.4194481941604,38.0575984042197,49.2921601297526));
#32779=CARTESIAN_POINT('Ctrl Pts',(40.4649221573388,38.0618201239018,49.3570055945875));
#32780=CARTESIAN_POINT('Ctrl Pts',(40.5103812416391,38.0660404622559,49.4218298422752));
#32781=CARTESIAN_POINT('Ctrl Pts',(40.559117887587,38.0702608006101,49.4843910188875));
#32782=CARTESIAN_POINT('Ctrl Pts',(40.6108713941373,38.0744811389643,49.5443475232549));
#32783=CARTESIAN_POINT('Ctrl Pts',(40.662624128704,38.0787014143656,49.6043031332784));
#32784=CARTESIAN_POINT('Ctrl Pts',(40.7173933267255,38.0829216897669,49.6616537938639));
#32785=CARTESIAN_POINT('Ctrl Pts',(40.7748788731974,38.0871419651682,49.7160920033961));
#32786=CARTESIAN_POINT('Ctrl Pts',(40.8324219186076,38.091366461828,49.7705846638196));
#32787=CARTESIAN_POINT('Ctrl Pts',(40.8926863983753,38.0955909584879,49.8221587303494));
#32788=CARTESIAN_POINT('Ctrl Pts',(40.9553367264353,38.0998154551477,49.8705449652209));
#32789=CARTESIAN_POINT('Ctrl Pts',(41.0180171327539,38.1040419799774,49.9189544301973));
#32790=CARTESIAN_POINT('Ctrl Pts',(41.0830852832688,38.108268504807,49.9641727464203));
#32791=CARTESIAN_POINT('Ctrl Pts',(41.1501761374244,38.1124950296367,50.0059737668864));
#32792=CARTESIAN_POINT('Ctrl Pts',(41.2173896314122,38.116729280412,50.0478511982167));
#32793=CARTESIAN_POINT('Ctrl Pts',(41.2866328059631,38.1209635311874,50.0862986229723));
#32794=CARTESIAN_POINT('Ctrl Pts',(41.3575157061365,38.1251977819627,50.1211357660339));
#32795=CARTESIAN_POINT('Ctrl Pts',(41.4251193274894,38.129236142208,50.1543612269389));
#32796=CARTESIAN_POINT('Ctrl Pts',(41.4942139689906,38.1332745024533,50.1843029578225));
#32797=CARTESIAN_POINT('Ctrl Pts',(41.5644474597846,38.1373128626985,50.2108465332174));
#32798=CARTESIAN_POINT('Ctrl Pts',(41.6381095282704,38.1415483629648,50.2386858823157));
#32799=CARTESIAN_POINT('Ctrl Pts',(41.7133044804439,38.145783863231,50.2628926534915));
#32800=CARTESIAN_POINT('Ctrl Pts',(41.7896397254383,38.1500193634973,50.283298223215));
#32801=CARTESIAN_POINT('Ctrl Pts',(41.865864308557,38.1542487236325,50.3036742113395));
#32802=CARTESIAN_POINT('Ctrl Pts',(41.9432254522109,38.1584780837678,50.3202598207785));
#32803=CARTESIAN_POINT('Ctrl Pts',(42.0213120794316,38.1627074439031,50.3329350397548));
#32804=CARTESIAN_POINT('Ctrl Pts',(42.0993075176613,38.1669318650225,50.3455954567033));
#32805=CARTESIAN_POINT('Ctrl Pts',(42.1780262950039,38.171156286142,50.3543544829134));
#32806=CARTESIAN_POINT('Ctrl Pts',(42.2570452093146,38.1753807072615,50.3591427190232));
#32807=CARTESIAN_POINT('Ctrl Pts',(42.3360135925232,38.1796024269436,50.3639278931465));
#32808=CARTESIAN_POINT('Ctrl Pts',(42.4152812645295,38.1838241466256,50.3647472887163));
#32809=CARTESIAN_POINT('Ctrl Pts',(42.4944191474996,38.1880458663076,50.3615832539814));
#32810=CARTESIAN_POINT('Ctrl Pts',(42.5735311369069,38.1922662046618,50.3584202545046));
#32811=CARTESIAN_POINT('Ctrl Pts',(42.6525129529803,38.1964865430159,50.3512764315013));
#32812=CARTESIAN_POINT('Ctrl Pts',(42.7309362625019,38.2007068813701,50.340186238542));
#32813=CARTESIAN_POINT('Ctrl Pts',(42.8093584022186,38.2049271567713,50.3290962110101));
#32814=CARTESIAN_POINT('Ctrl Pts',(42.8872215874029,38.2091474321726,50.3140599975754));
#32815=CARTESIAN_POINT('Ctrl Pts',(42.9641048409025,38.2133677075739,50.2951636476231));
#32816=CARTESIAN_POINT('Ctrl Pts',(43.0410649955664,38.2175922042337,50.2762483969186));
#32817=CARTESIAN_POINT('Ctrl Pts',(43.1170428036769,38.2218167008936,50.2534654090814));
#32818=CARTESIAN_POINT('Ctrl Pts',(43.1916302795124,38.2260411975534,50.2269512660719));
#32819=CARTESIAN_POINT('Ctrl Pts',(43.2662535646001,38.2302677223831,50.2004243936916));
#32820=CARTESIAN_POINT('Ctrl Pts',(43.3394847533105,38.2344942472127,50.1701629771104));
#32821=CARTESIAN_POINT('Ctrl Pts',(43.4109361658329,38.2387207720423,50.1363516820765));
#32822=CARTESIAN_POINT('Ctrl Pts',(43.4825181891421,38.2429550228177,50.1024785811288));
#32823=CARTESIAN_POINT('Ctrl Pts',(43.5523135205644,38.247189273593,50.0650428574967));
#32824=CARTESIAN_POINT('Ctrl Pts',(43.6199595813607,38.2514235243683,50.0242749469245));
#32825=CARTESIAN_POINT('Ctrl Pts',(43.6844761102974,38.2554618846137,49.9853930955476));
#32826=CARTESIAN_POINT('Ctrl Pts',(43.7470375593339,38.259500244859,49.9434807843835));
#32827=CARTESIAN_POINT('Ctrl Pts',(43.8073571720049,38.2635386051043,49.8987722958023));
#32828=CARTESIAN_POINT('Ctrl Pts',(43.870621398079,38.2677741053706,49.8518812797002));
#32829=CARTESIAN_POINT('Ctrl Pts',(43.9316598011957,38.2720096056368,49.8017358716542));
#32830=CARTESIAN_POINT('Ctrl Pts',(43.990118175916,38.2762451059031,49.7485750277073));
#32831=CARTESIAN_POINT('Ctrl Pts',(44.0484918045484,38.2804744660383,49.6954912501102));
#32832=CARTESIAN_POINT('Ctrl Pts',(44.1042924879004,38.2847038261736,49.6394010305941));
#32833=CARTESIAN_POINT('Ctrl Pts',(44.1571969035576,38.2889331863089,49.5805851710767));
#32834=CARTESIAN_POINT('Ctrl Pts',(44.2100395378259,38.2931576074283,49.521837996289));
#32835=CARTESIAN_POINT('Ctrl Pts',(44.259992313289,38.2973820285478,49.4603718538201));
#32836=CARTESIAN_POINT('Ctrl Pts',(44.306767914377,38.3016064496673,49.3965051240874));
#32837=CARTESIAN_POINT('Ctrl Pts',(44.3535136033523,38.3058281693494,49.3326792359213));
#32838=CARTESIAN_POINT('Ctrl Pts',(44.397085873951,38.3100498890314,49.2664561850306));
#32839=CARTESIAN_POINT('Ctrl Pts',(44.4372377530987,38.3142716087134,49.1981872884693));
#32840=CARTESIAN_POINT('Ctrl Pts',(44.4773764947304,38.3184919470676,49.1299407291868));
#32841=CARTESIAN_POINT('Ctrl Pts',(44.514096829383,38.3227122854218,49.0596500576837));
#32842=CARTESIAN_POINT('Ctrl Pts',(44.5471960088507,38.3269326237759,48.9876941533064));
#32843=CARTESIAN_POINT('Ctrl Pts',(44.580294694593,38.3311528991772,48.9157393222626));
#32844=CARTESIAN_POINT('Ctrl Pts',(44.6097721375908,38.3353731745785,48.8421197346801));
#32845=CARTESIAN_POINT('Ctrl Pts',(44.6354729627353,38.3395934499798,48.7672359961443));
#32846=CARTESIAN_POINT('Ctrl Pts',(44.6611994946922,38.3438179466396,48.6922773564249));
#32847=CARTESIAN_POINT('Ctrl Pts',(44.6831417100419,38.3480424432995,48.6160524848565));
#32848=CARTESIAN_POINT('Ctrl Pts',(44.7011937612435,38.3522669399593,48.5389783985599));
#32849=CARTESIAN_POINT('Ctrl Pts',(44.7192544791876,38.356493464789,48.4618673091959));
#32850=CARTESIAN_POINT('Ctrl Pts',(44.7334212283509,38.3607199896186,48.3839066553275));
#32851=CARTESIAN_POINT('Ctrl Pts',(44.7436395863326,38.3649465144483,48.3055223891544));
#32852=CARTESIAN_POINT('Ctrl Pts',(44.7538766231302,38.3691807652236,48.2269948391707));
#32853=CARTESIAN_POINT('Ctrl Pts',(44.7601508091553,38.373415015999,48.1480425986582));
#32854=CARTESIAN_POINT('Ctrl Pts',(44.7624597953243,38.3776492667743,48.0690952702895));
#32855=CARTESIAN_POINT('Ctrl Pts',(44.7646619601101,38.3816876270196,47.9938003080227));
#32856=CARTESIAN_POINT('Ctrl Pts',(44.763257741574,38.3857259872649,47.9185101698709));
#32857=CARTESIAN_POINT('Ctrl Pts',(44.7582890449573,38.3897643475102,47.8435927708376));
#32858=CARTESIAN_POINT('Ctrl Pts',(44.7530777922299,38.3939998477765,47.7650181404736));
#32859=CARTESIAN_POINT('Ctrl Pts',(44.7439253532618,38.3982353480427,47.6865548913434));
#32860=CARTESIAN_POINT('Ctrl Pts',(44.7308410746641,38.402470848309,47.608630193348));
#32861=CARTESIAN_POINT('Ctrl Pts',(44.7177757641172,38.4067002084442,47.5308184614305));
#32862=CARTESIAN_POINT('Ctrl Pts',(44.7007900100373,38.4109295685795,47.4535441892162));
#32863=CARTESIAN_POINT('Ctrl Pts',(44.6799450600438,38.4151589287148,47.3772312113778));
#32864=CARTESIAN_POINT('Ctrl Pts',(44.6591244526301,38.4193833498342,47.3010073512756));
#32865=CARTESIAN_POINT('Ctrl Pts',(44.6344537280659,38.4236077709537,47.2257430051616));
#32866=CARTESIAN_POINT('Ctrl Pts',(44.6060452179403,38.4278321920732,47.1518520545903));
#32867=CARTESIAN_POINT('Ctrl Pts',(44.57765487452,38.4320539117553,47.0780083558852));
#32868=CARTESIAN_POINT('Ctrl Pts',(44.5455316576349,38.4362756314373,47.0055367464692));
#32869=CARTESIAN_POINT('Ctrl Pts',(44.5098374244564,38.4404973511193,46.9348349971655));
#32870=CARTESIAN_POINT('Ctrl Pts',(44.4741548702719,38.4447176894735,46.8641563811594));
#32871=CARTESIAN_POINT('Ctrl Pts',(44.4349038312564,38.4489380278276,46.7952468940508));
#32872=CARTESIAN_POINT('Ctrl Pts',(44.3922932705203,38.4531583661818,46.7284820232732));
#32873=CARTESIAN_POINT('Ctrl Pts',(44.3496833453866,38.4573786415831,46.6617181483968));
#32874=CARTESIAN_POINT('Ctrl Pts',(44.3037142517748,38.4615989169843,46.597099221185));
#32875=CARTESIAN_POINT('Ctrl Pts',(44.2546388536143,38.4658191923856,46.5349726406772));
#32876=CARTESIAN_POINT('Ctrl Pts',(44.2055143686229,38.4700436890455,46.4727839191158));
#32877=CARTESIAN_POINT('Ctrl Pts',(44.1532776640307,38.4742681857053,46.4130928933797));
#32878=CARTESIAN_POINT('Ctrl Pts',(44.0982222003218,38.4784926823652,46.3562141869348));
#32879=CARTESIAN_POINT('Ctrl Pts',(44.0431403046286,38.4827192071948,46.2993081731717));
#32880=CARTESIAN_POINT('Ctrl Pts',(43.9852372973732,38.4869457320244,46.2452174892767));
#32881=CARTESIAN_POINT('Ctrl Pts',(43.9248419742549,38.4911722568541,46.1942183425313));
#32882=CARTESIAN_POINT('Ctrl Pts',(43.8643362505107,38.4954065076294,46.1431259710553));
#32883=CARTESIAN_POINT('Ctrl Pts',(43.8013294815712,38.4996407584048,46.0951367143406));
#32884=CARTESIAN_POINT('Ctrl Pts',(43.7361817045074,38.5038750091801,46.050484959422));
#32885=CARTESIAN_POINT('Ctrl Pts',(43.674047880385,38.5079133694254,46.0078989432614));
#32886=CARTESIAN_POINT('Ctrl Pts',(43.6099670907946,38.5119517296707,45.9683486064981));
#32887=CARTESIAN_POINT('Ctrl Pts',(43.5442714329593,38.515990089916,45.9319977445338));
#32888=CARTESIAN_POINT('Ctrl Pts',(43.4753687201376,38.5202255901823,45.8938723480422));
#32889=CARTESIAN_POINT('Ctrl Pts',(43.404427533846,38.5244610904485,45.8591218560936));
#32890=CARTESIAN_POINT('Ctrl Pts',(43.3318121923973,38.5286965907148,45.8279695032068));
#32891=CARTESIAN_POINT('Ctrl Pts',(43.2593021201448,38.53292595085,45.7968623113436));
#32892=CARTESIAN_POINT('Ctrl Pts',(43.1851231400017,38.5371553109853,45.7693430836499));
#32893=CARTESIAN_POINT('Ctrl Pts',(43.1096648432644,38.5413846711206,45.7455896001095));
#32894=CARTESIAN_POINT('Ctrl Pts',(43.034294666173,38.54560909224,45.7218638557131));
#32895=CARTESIAN_POINT('Ctrl Pts',(42.957648586665,38.5498335133595,45.7018952568009));
#32896=CARTESIAN_POINT('Ctrl Pts',(42.8801354611772,38.554057934479,45.6858132357521));
#32897=CARTESIAN_POINT('Ctrl Pts',(42.8026719038681,38.5582796541611,45.6697414988519));
#32898=CARTESIAN_POINT('Ctrl Pts',(42.724342859386,38.5625013738431,45.6575515019318));
#32899=CARTESIAN_POINT('Ctrl Pts',(42.6455704275094,38.5667230935251,45.6493223091983));
#32900=CARTESIAN_POINT('Ctrl Pts',(42.5668237696217,38.5709434318793,45.64109580902));
#32901=CARTESIAN_POINT('Ctrl Pts',(42.487634478867,38.5751637702335,45.6368275884164));
#32902=CARTESIAN_POINT('Ctrl Pts',(42.4084313979796,38.5793841085876,45.6365450390523));
#32903=CARTESIAN_POINT('Ctrl Pts',(42.3292294985286,38.5836043839889,45.636262493903));
#32904=CARTESIAN_POINT('Ctrl Pts',(42.250014278707,38.5878246593902,45.639965502155));
#32905=CARTESIAN_POINT('Ctrl Pts',(42.171214708091,38.5920449347915,45.6476293380706));
#32906=CARTESIAN_POINT('Ctrl Pts',(42.0923363195471,38.5962694314513,45.6553008396075));
#32907=CARTESIAN_POINT('Ctrl Pts',(42.0138748789772,38.6004939281112,45.6669410373619));
#32908=CARTESIAN_POINT('Ctrl Pts',(41.9362537531706,38.604718424771,45.6824733314476));
#32909=CARTESIAN_POINT('Ctrl Pts',(41.8585953616645,38.6089449496007,45.6980130825471));
#32910=CARTESIAN_POINT('Ctrl Pts',(41.7817785442484,38.6131714744303,45.7174485371472));
#32911=CARTESIAN_POINT('Ctrl Pts',(41.7062134746732,38.61739799926,45.7406525946249));
#32912=CARTESIAN_POINT('Ctrl Pts',(41.6305102746842,38.6216322500353,45.7638990683419));
#32913=CARTESIAN_POINT('Ctrl Pts',(41.5560638371381,38.6258665008106,45.7909277499394));
#32914=CARTESIAN_POINT('Ctrl Pts',(41.4832660651006,38.630100751586,45.8215626395272));
#32915=CARTESIAN_POINT('Ctrl Pts',(41.4138361602268,38.6341391118313,45.8507802571872));
#32916=CARTESIAN_POINT('Ctrl Pts',(41.3459060551789,38.6381774720766,45.8832776041683));
#32917=CARTESIAN_POINT('Ctrl Pts',(41.2797931682581,38.6422158323219,45.9188639893033));
#32918=CARTESIAN_POINT('Ctrl Pts',(41.2104528585419,38.6464513325882,45.9561875896158));
#32919=CARTESIAN_POINT('Ctrl Pts',(41.1428481414697,38.6506868328544,45.997051397964));
#32920=CARTESIAN_POINT('Ctrl Pts',(41.0773638566439,38.6549223331207,46.0412697803965));
#32921=CARTESIAN_POINT('Ctrl Pts',(41.0119745032457,38.6591516932559,46.0854240602098));
#32922=CARTESIAN_POINT('Ctrl Pts',(40.9486998634504,38.6633810533912,46.1329229964788));
#32923=CARTESIAN_POINT('Ctrl Pts',(40.8879002207895,38.6676104135264,46.183535109447));
#32924=CARTESIAN_POINT('Ctrl Pts',(40.8271715795058,38.6718348346459,46.2340881179607));
#32925=CARTESIAN_POINT('Ctrl Pts',(40.7689125506755,38.6760592557654,46.2877467799475));
#32926=CARTESIAN_POINT('Ctrl Pts',(40.7134531784151,38.6802836768849,46.3442372574847));
#32927=CARTESIAN_POINT('Ctrl Pts',(40.658029271375,38.6845053965669,46.4006916104291));
#32928=CARTESIAN_POINT('Ctrl Pts',(40.6054017954103,38.688727116249,46.45997385067));
#32929=CARTESIAN_POINT('Ctrl Pts',(40.5558655981254,38.692948835931,46.5217717535094));
#32930=CARTESIAN_POINT('Ctrl Pts',(40.5063456088636,38.6971691742851,46.5835494363503));
#32931=CARTESIAN_POINT('Ctrl Pts',(40.4599151832051,38.7013895126393,46.6478407814173));
#32932=CARTESIAN_POINT('Ctrl Pts',(40.4168293585783,38.7056098509934,46.7142999385925));
#32933=CARTESIAN_POINT('Ctrl Pts',(40.3737441766433,38.7098301263947,46.7807581044266));
#32934=CARTESIAN_POINT('Ctrl Pts',(40.3340037507722,38.714050401796,46.8493836235362));
#32935=CARTESIAN_POINT('Ctrl Pts',(40.2978193548152,38.7182706771973,46.9198023440545));
#32936=CARTESIAN_POINT('Ctrl Pts',(40.2615987660326,38.7224951738571,46.9902914996981));
#32937=CARTESIAN_POINT('Ctrl Pts',(40.2289415274616,38.726719670517,47.0625770212704));
#32938=CARTESIAN_POINT('Ctrl Pts',(40.2000122542779,38.7309441671768,47.1362614055327));
#32939=CARTESIAN_POINT('Ctrl Pts',(40.1710690922257,38.7351706920065,47.2099811654751));
#32940=CARTESIAN_POINT('Ctrl Pts',(40.1458576105764,38.7393972168361,47.2851006804262));
#32941=CARTESIAN_POINT('Ctrl Pts',(40.1244928146473,38.7436237416657,47.3612062223941));
#32942=CARTESIAN_POINT('Ctrl Pts',(40.1030889645874,38.7478579924411,47.4374508827413));
#32943=CARTESIAN_POINT('Ctrl Pts',(40.0855459552939,38.7520922432164,47.5146847128752));
#32944=CARTESIAN_POINT('Ctrl Pts',(40.0719277821424,38.7563264939918,47.5924828968751));
#32945=CARTESIAN_POINT('Ctrl Pts',(40.0589396309943,38.7603648542371,47.6666818780156));
#32946=CARTESIAN_POINT('Ctrl Pts',(40.049521203197,38.7644032144824,47.7413937910581));
#32947=CARTESIAN_POINT('Ctrl Pts',(40.0436838427263,38.7684415747277,47.8162485160041));
#32948=CARTESIAN_POINT('Ctrl Pts',(40.038946734349,38.7717187665757,47.876994283958));
#32949=CARTESIAN_POINT('Ctrl Pts',(40.0365582913862,38.7749959584237,47.9379255771268));
#32950=CARTESIAN_POINT('Ctrl Pts',(40.0365302498271,38.7782731502717,47.9989132996958));
#32951=CARTESIAN_POINT('',(40.036530522818,39.5720231502423,47.9984279538409));
#32952=CARTESIAN_POINT('Ctrl Pts',(40.0365302498269,38.7782731502987,47.9989133001977));
#32953=CARTESIAN_POINT('Ctrl Pts',(40.0364944094856,38.7824617807574,48.0768626678913));
#32954=CARTESIAN_POINT('Ctrl Pts',(40.0403190670139,38.7866504112161,48.1549693244316));
#32955=CARTESIAN_POINT('Ctrl Pts',(40.0480246341257,38.7908390416748,48.2328139154357));
#32956=CARTESIAN_POINT('Ctrl Pts',(40.0559832392965,38.7951652198189,48.3132147938517));
#32957=CARTESIAN_POINT('Ctrl Pts',(40.0680821762149,38.799491397963,48.3933355850916));
#32958=CARTESIAN_POINT('Ctrl Pts',(40.0842854859267,38.8038175761071,48.4727121007655));
#32959=CARTESIAN_POINT('Ctrl Pts',(40.0999358242399,38.8079961144899,48.5493797289548));
#32960=CARTESIAN_POINT('Ctrl Pts',(40.1194148280676,38.8121746528727,48.6253525429861));
#32961=CARTESIAN_POINT('Ctrl Pts',(40.1426374764409,38.8163531912554,48.7002177362298));
#32962=CARTESIAN_POINT('Ctrl Pts',(40.1658480869031,38.8205295636116,48.7750441216459));
#32963=CARTESIAN_POINT('Ctrl Pts',(40.1927983500028,38.8247059359678,48.8487635673267));
#32964=CARTESIAN_POINT('Ctrl Pts',(40.2233528447225,38.828882308324,48.9209764396131));
#32965=CARTESIAN_POINT('Ctrl Pts',(40.2539015380945,38.8330578877171,48.9931756009222));
#32966=CARTESIAN_POINT('Ctrl Pts',(40.2880529168436,38.8372334671101,49.0638683146151));
#32967=CARTESIAN_POINT('Ctrl Pts',(40.325623280202,38.8414090465031,49.1326745628203));
#32968=CARTESIAN_POINT('Ctrl Pts',(40.3631988521081,38.8455852047755,49.2014903499437));
#32969=CARTESIAN_POINT('Ctrl Pts',(40.4041941166697,38.8497613630478,49.2684187322828));
#32970=CARTESIAN_POINT('Ctrl Pts',(40.4483800556006,38.8539375213201,49.3331054097566));
#32971=CARTESIAN_POINT('Ctrl Pts',(40.4926135023509,38.8581181697125,49.3978616370254));
#32972=CARTESIAN_POINT('Ctrl Pts',(40.5400441945344,38.8622988181049,49.4603709549415));
#32973=CARTESIAN_POINT('Ctrl Pts',(40.59040104084,38.8664794664973,49.5203098525982));
#32974=CARTESIAN_POINT('Ctrl Pts',(40.6407904831372,38.8706628210238,49.5802875487091));
#32975=CARTESIAN_POINT('Ctrl Pts',(40.6941095189094,38.8748461755504,49.6376911652412));
#32976=CARTESIAN_POINT('Ctrl Pts',(40.7500500103594,38.8790295300769,49.6922338705347));
#32977=CARTESIAN_POINT('Ctrl Pts',(40.8060799215419,38.8832195716101,49.7468637612282));
#32978=CARTESIAN_POINT('Ctrl Pts',(40.8647392847159,38.8874096131434,49.7986233057304));
#32979=CARTESIAN_POINT('Ctrl Pts',(40.9256874243613,38.8915996546766,49.8472663235748));
#32980=CARTESIAN_POINT('Ctrl Pts',(40.9405614471548,38.892622208829,49.8591373562326));
#32981=CARTESIAN_POINT('Ctrl Pts',(40.9555716547226,38.8936447629813,49.8708229831906));
#32982=CARTESIAN_POINT('Ctrl Pts',(40.9707128576697,38.8946673171336,49.882320032744));
#32983=CARTESIAN_POINT('Ctrl Pts',(41.0334289191787,38.8989028173999,49.9299417223468));
#32984=CARTESIAN_POINT('Ctrl Pts',(41.0986468176736,38.9031383176661,49.9745160907557));
#32985=CARTESIAN_POINT('Ctrl Pts',(41.1660380541219,38.9073738179324,50.0157699166881));
#32986=CARTESIAN_POINT('Ctrl Pts',(41.2333315946683,38.9116031780677,50.0569639376675));
#32987=CARTESIAN_POINT('Ctrl Pts',(41.3027918196159,38.9158325382029,50.0948467324187));
#32988=CARTESIAN_POINT('Ctrl Pts',(41.3740586935887,38.9200618983382,50.1291864354018));
#32989=CARTESIAN_POINT('Ctrl Pts',(41.4452423426282,38.9242863194577,50.1634860367314));
#32990=CARTESIAN_POINT('Ctrl Pts',(41.5182280275148,38.9285107405772,50.1942505657886));
#32991=CARTESIAN_POINT('Ctrl Pts',(41.5926297068378,38.9327351616967,50.2212932383229));
#32992=CARTESIAN_POINT('Ctrl Pts',(41.6669838076932,38.9369568813787,50.2483186175794));
#32993=CARTESIAN_POINT('Ctrl Pts',(41.7427516658322,38.9411786010607,50.271626704318));
#32994=CARTESIAN_POINT('Ctrl Pts',(41.8195269031812,38.9454003207427,50.2910786596644));
#32995=CARTESIAN_POINT('Ctrl Pts',(41.8962770200146,38.9496206590969,50.3105242504177));
#32996=CARTESIAN_POINT('Ctrl Pts',(41.9740334069304,38.953840997451,50.3261160999281));
#32997=CARTESIAN_POINT('Ctrl Pts',(42.0523755950056,38.9580613358052,50.3377655387041));
#32998=CARTESIAN_POINT('Ctrl Pts',(42.1307166144861,38.9622816112065,50.3494148037106));
#32999=CARTESIAN_POINT('Ctrl Pts',(42.2096429533133,38.9665018866078,50.3571217071647));
#33000=CARTESIAN_POINT('Ctrl Pts',(42.2887265354423,38.9707221620091,50.3608491389721));
#33001=CARTESIAN_POINT('Ctrl Pts',(42.3678892195767,38.9749466586689,50.3645802990797));
#33002=CARTESIAN_POINT('Ctrl Pts',(42.4472089912483,38.9791711553287,50.3643240140422));
#33003=CARTESIAN_POINT('Ctrl Pts',(42.5262558724953,38.9833956519886,50.3600953149313));
#33004=CARTESIAN_POINT('Ctrl Pts',(42.6053407039433,38.9876221768182,50.355864585633));
#33005=CARTESIAN_POINT('Ctrl Pts',(42.6841519165021,38.9918487016479,50.347657691673));
#33006=CARTESIAN_POINT('Ctrl Pts',(42.7622653390865,38.9960752264775,50.3355415357036));
#33007=CARTESIAN_POINT('Ctrl Pts',(42.8405215503886,39.0003094772528,50.3234032318072));
#33008=CARTESIAN_POINT('Ctrl Pts',(42.9180769620872,39.0045437280282,50.3073414819502));
#33009=CARTESIAN_POINT('Ctrl Pts',(42.9945184649252,39.0087779788035,50.2874742043929));
#33010=CARTESIAN_POINT('Ctrl Pts',(43.0674235294882,39.0128163390488,50.2685260532024));
#33011=CARTESIAN_POINT('Ctrl Pts',(43.1393151421295,39.0168546992941,50.2461168416051));
#33012=CARTESIAN_POINT('Ctrl Pts',(43.2098517979214,39.0208930595394,50.2203897194645));
#33013=CARTESIAN_POINT('Ctrl Pts',(43.2838318309644,39.0251285598057,50.1934066802957));
#33014=CARTESIAN_POINT('Ctrl Pts',(43.3566024538726,39.0293640600719,50.1626709511733));
#33015=CARTESIAN_POINT('Ctrl Pts',(43.4277561646983,39.0335995603382,50.1283109986148));
#33016=CARTESIAN_POINT('Ctrl Pts',(43.4988067252283,39.0378289204734,50.0940008570812));
#33017=CARTESIAN_POINT('Ctrl Pts',(43.5682446093869,39.0420582806087,50.0560771279466));
#33018=CARTESIAN_POINT('Ctrl Pts',(43.6356800356732,39.0462876407439,50.0147171737836));
#33019=CARTESIAN_POINT('Ctrl Pts',(43.703036711363,39.0505120618634,49.9734055194719));
#33020=CARTESIAN_POINT('Ctrl Pts',(43.7683951781113,39.0547364829829,49.9286658584228));
#33021=CARTESIAN_POINT('Ctrl Pts',(43.8313895000035,39.0589609041024,49.8807218136077));
#33022=CARTESIAN_POINT('Ctrl Pts',(43.8943435382175,39.0631826237844,49.8328084281031));
#33023=CARTESIAN_POINT('Ctrl Pts',(43.954936059751,39.0674043434665,49.7816950094286));
#33024=CARTESIAN_POINT('Ctrl Pts',(44.0128304501349,39.0716260631485,49.7276482223004));
#33025=CARTESIAN_POINT('Ctrl Pts',(44.070705897732,39.0758464015027,49.6736191190403));
#33026=CARTESIAN_POINT('Ctrl Pts',(44.1258846243335,39.0800667398568,49.6166588731842));
#33027=CARTESIAN_POINT('Ctrl Pts',(44.1780645862994,39.084287078211,49.5570731414574));
#33028=CARTESIAN_POINT('Ctrl Pts',(44.2302437699205,39.0885073536123,49.4974882985438));
#33029=CARTESIAN_POINT('Ctrl Pts',(44.2794239696128,39.0927276290135,49.4352784015845));
#33030=CARTESIAN_POINT('Ctrl Pts',(44.3253423892487,39.0969479044148,49.3707833983026));
#33031=CARTESIAN_POINT('Ctrl Pts',(44.3713067380016,39.1011724010747,49.3062238849925));
#33032=CARTESIAN_POINT('Ctrl Pts',(44.4140025164947,39.1053968977345,49.2393750827672));
#33033=CARTESIAN_POINT('Ctrl Pts',(44.4532097518632,39.1096213943944,49.1706067468428));
#33034=CARTESIAN_POINT('Ctrl Pts',(44.4924358105229,39.113847919224,49.1018053954202));
#33035=CARTESIAN_POINT('Ctrl Pts',(44.5281697776149,39.1180744440537,49.0310830939211));
#33036=CARTESIAN_POINT('Ctrl Pts',(44.5602384472003,39.1223009688833,48.9588327758986));
#33037=CARTESIAN_POINT('Ctrl Pts',(44.5923657372387,39.1265352196587,48.886450386717));
#33038=CARTESIAN_POINT('Ctrl Pts',(44.6208141724858,39.130769470434,48.8125348387977));
#33039=CARTESIAN_POINT('Ctrl Pts',(44.6454594369158,39.1350037212094,48.7374973613957));
#33040=CARTESIAN_POINT('Ctrl Pts',(44.6689645294081,39.1390420814547,48.6659313673799));
#33041=CARTESIAN_POINT('Ctrl Pts',(44.6890105040941,39.1430804417,48.5933453106503));
#33042=CARTESIAN_POINT('Ctrl Pts',(44.7055330027674,39.1471188019453,48.520103849294));
#33043=CARTESIAN_POINT('Ctrl Pts',(44.7228620777578,39.1513543022116,48.4432869706032));
#33044=CARTESIAN_POINT('Ctrl Pts',(44.7363807545826,39.1555898024778,48.3654570664529));
#33045=CARTESIAN_POINT('Ctrl Pts',(44.7459766221029,39.1598253027441,48.287026356711));
#33046=CARTESIAN_POINT('Ctrl Pts',(44.7555585786611,39.1640546628793,48.2087093466035));
#33047=CARTESIAN_POINT('Ctrl Pts',(44.7612289624345,39.1682840230146,48.1297937224487));
#33048=CARTESIAN_POINT('Ctrl Pts',(44.7629260718499,39.1725133831498,48.0507032530708));
#33049=CARTESIAN_POINT('Ctrl Pts',(44.7646211993933,39.1767378042693,47.9717051449633));
#33050=CARTESIAN_POINT('Ctrl Pts',(44.7623522630275,39.1809622253888,47.8925330641883));
#33051=CARTESIAN_POINT('Ctrl Pts',(44.7561093677323,39.1851866465083,47.8136157512448));
#33052=CARTESIAN_POINT('Ctrl Pts',(44.7498704646507,39.1894083661903,47.7347489044312));
#33053=CARTESIAN_POINT('Ctrl Pts',(44.7396626834337,39.1936300858724,47.6561369687152));
#33054=CARTESIAN_POINT('Ctrl Pts',(44.7255281910292,39.1978518055544,47.5782073096548));
#33055=CARTESIAN_POINT('Ctrl Pts',(44.7113983233675,39.2020721439085,47.5003031488318));
#33056=CARTESIAN_POINT('Ctrl Pts',(44.6933443794085,39.2062924822627,47.4230812828554));
#33057=CARTESIAN_POINT('Ctrl Pts',(44.6714600219979,39.2105128206168,47.3469610965911));
#33058=CARTESIAN_POINT('Ctrl Pts',(44.6495759910263,39.2147330960181,47.2708420457771));
#33059=CARTESIAN_POINT('Ctrl Pts',(44.6238617911444,39.2189533714194,47.1958250927204));
#33060=CARTESIAN_POINT('Ctrl Pts',(44.5944611574601,39.2231736468207,47.1223151651653));
#33061=CARTESIAN_POINT('Ctrl Pts',(44.5650311162929,39.2273981434805,47.0487317105576));
#33062=CARTESIAN_POINT('Ctrl Pts',(44.5319074502033,39.2316226401404,46.976658729456));
#33063=CARTESIAN_POINT('Ctrl Pts',(44.495282130258,39.2358471368002,46.9064812596387));
#33064=CARTESIAN_POINT('Ctrl Pts',(44.4586392265924,39.2400736616298,46.8362700978017));
#33065=CARTESIAN_POINT('Ctrl Pts',(44.4184915581805,39.2443001864595,46.7679566653412));
#33066=CARTESIAN_POINT('Ctrl Pts',(44.3750758902299,39.2485267112891,46.701899207021));
#33067=CARTESIAN_POINT('Ctrl Pts',(44.3315808598937,39.2527609620645,46.6357209978816));
#33068=CARTESIAN_POINT('Ctrl Pts',(44.2848061708965,39.2569952128398,46.5718073830453));
#33069=CARTESIAN_POINT('Ctrl Pts',(44.2350304246718,39.2612294636151,46.510485387306));
#33070=CARTESIAN_POINT('Ctrl Pts',(44.1875574700924,39.2652678238605,46.4520003511339));
#33071=CARTESIAN_POINT('Ctrl Pts',(44.1373552608477,39.2693061841058,46.3958726848754));
#33072=CARTESIAN_POINT('Ctrl Pts',(44.0846956673817,39.2733445443511,46.3423537925102));
#33073=CARTESIAN_POINT('Ctrl Pts',(44.029465398511,39.2775800446174,46.286222276476));
#33074=CARTESIAN_POINT('Ctrl Pts',(43.9713217538187,39.2818155448836,46.2327473740915));
#33075=CARTESIAN_POINT('Ctrl Pts',(43.9105506083137,39.2860510451499,46.1822466337197));
#33076=CARTESIAN_POINT('Ctrl Pts',(43.8498675616802,39.2902804052851,46.131819103392));
#33077=CARTESIAN_POINT('Ctrl Pts',(43.7865649362458,39.2945097654204,46.0843574704553));
#33078=CARTESIAN_POINT('Ctrl Pts',(43.7209657534595,39.2987391255556,46.040142882992));
#33079=CARTESIAN_POINT('Ctrl Pts',(43.655443176918,39.3029635466751,45.9959799289997));
#33080=CARTESIAN_POINT('Ctrl Pts',(43.5876297596427,39.3071879677946,45.95505674628));
#33081=CARTESIAN_POINT('Ctrl Pts',(43.5178807313047,39.3114123889141,45.9176136017834));
#33082=CARTESIAN_POINT('Ctrl Pts',(43.448176306152,39.3156341085962,45.8801944014699));
#33083=CARTESIAN_POINT('Ctrl Pts',(43.3765391390938,39.3198558282782,45.8462510437949));
#33084=CARTESIAN_POINT('Ctrl Pts',(43.3033514685189,39.3240775479602,45.8159792663015));
#33085=CARTESIAN_POINT('Ctrl Pts',(43.2301877446238,39.3282978863144,45.785717393599));
#33086=CARTESIAN_POINT('Ctrl Pts',(43.1554749579643,39.3325182246685,45.7591248949027));
#33087=CARTESIAN_POINT('Ctrl Pts',(43.0796164937853,39.3367385630227,45.7363498807733));
#33088=CARTESIAN_POINT('Ctrl Pts',(43.0037591611525,39.340958838424,45.7135752063685));
#33089=CARTESIAN_POINT('Ctrl Pts',(42.9267566348827,39.3451791138253,45.6946180370235));
#33090=CARTESIAN_POINT('Ctrl Pts',(42.8490272300439,39.3493993892265,45.679576549942));
#33091=CARTESIAN_POINT('Ctrl Pts',(42.7712200776924,39.3536238858864,45.6645200178693));
#33092=CARTESIAN_POINT('Ctrl Pts',(42.6926850563059,39.3578483825462,45.6533870813348));
#33093=CARTESIAN_POINT('Ctrl Pts',(42.6138498481755,39.3620728792061,45.6462245894446));
#33094=CARTESIAN_POINT('Ctrl Pts',(42.5349767914677,39.3662994040357,45.6390586588607));
#33095=CARTESIAN_POINT('Ctrl Pts',(42.4558037305286,39.3705259288654,45.6358669892364));
#33096=CARTESIAN_POINT('Ctrl Pts',(42.3767600472215,39.374752453695,45.6366442617552));
#33097=CARTESIAN_POINT('Ctrl Pts',(42.2975718747112,39.3789867044704,45.6374229551021));
#33098=CARTESIAN_POINT('Ctrl Pts',(42.2185140221459,39.3832209552457,45.6421850596758));
#33099=CARTESIAN_POINT('Ctrl Pts',(42.1400122475599,39.387455206021,45.6508731814819));
#33100=CARTESIAN_POINT('Ctrl Pts',(42.0651422262749,39.3914935662664,45.6591593618641));
#33101=CARTESIAN_POINT('Ctrl Pts',(41.9907783157044,39.3955319265117,45.6710162390806));
#33102=CARTESIAN_POINT('Ctrl Pts',(41.9172790332476,39.399570286757,45.6863511698709));
#33103=CARTESIAN_POINT('Ctrl Pts',(41.8401917474427,39.4038057870233,45.7024347036568));
#33104=CARTESIAN_POINT('Ctrl Pts',(41.7637626367544,39.4080412872895,45.7224056736516));
#33105=CARTESIAN_POINT('Ctrl Pts',(41.6884134242154,39.4122767875558,45.7461954419109));
#33106=CARTESIAN_POINT('Ctrl Pts',(41.6131734441177,39.416506147691,45.7699507225575));
#33107=CARTESIAN_POINT('Ctrl Pts',(41.5390106971314,39.4207355078263,45.7975136677444));
#33108=CARTESIAN_POINT('Ctrl Pts',(41.4663363885392,39.4249648679616,45.8287647060869));
#33109=CARTESIAN_POINT('Ctrl Pts',(41.3937469484722,39.4291892890811,45.8599792496957));
#33110=CARTESIAN_POINT('Ctrl Pts',(41.322642921634,39.4334137102005,45.894873143343));
#33111=CARTESIAN_POINT('Ctrl Pts',(41.2534185555025,39.43763813132,45.9332776112806));
#33112=CARTESIAN_POINT('Ctrl Pts',(41.1842384570446,39.4418598510021,45.9716575202869));
#33113=CARTESIAN_POINT('Ctrl Pts',(41.1169360428785,39.4460815706841,46.0135433207662));
#33114=CARTESIAN_POINT('Ctrl Pts',(41.0518827214868,39.4503032903661,46.0587194318507));
#33115=CARTESIAN_POINT('Ctrl Pts',(40.9868506852523,39.4545236287203,46.1038807615127));
#33116=CARTESIAN_POINT('Ctrl Pts',(40.9240666657714,39.4587439670744,46.1523299965446));
#33117=CARTESIAN_POINT('Ctrl Pts',(40.8638734561672,39.4629643054286,46.2038080051864));
#33118=CARTESIAN_POINT('Ctrl Pts',(40.8036811444376,39.4671845808299,46.2552852459544));
#33119=CARTESIAN_POINT('Ctrl Pts',(40.746079921596,39.4714048562312,46.3097908644601));
#33120=CARTESIAN_POINT('Ctrl Pts',(40.6913786623178,39.4756251316324,46.3670261590224));
#33121=CARTESIAN_POINT('Ctrl Pts',(40.6366226890372,39.4798496282923,46.4243187022127));
#33122=CARTESIAN_POINT('Ctrl Pts',(40.5847727987724,39.4840741249521,46.4843460354835));
#33123=CARTESIAN_POINT('Ctrl Pts',(40.5360997654162,39.488298621612,46.5467738109921));
#33124=CARTESIAN_POINT('Ctrl Pts',(40.487403364264,39.4925251464416,46.6092315579124));
#33125=CARTESIAN_POINT('Ctrl Pts',(40.4418871283864,39.4967516712713,46.6740916581663));
#33126=CARTESIAN_POINT('Ctrl Pts',(40.399778876443,39.5009781961009,46.7409901121213));
#33127=CARTESIAN_POINT('Ctrl Pts',(40.3575936520267,39.5052124468762,46.8080108542076));
#33128=CARTESIAN_POINT('Ctrl Pts',(40.3188290902334,39.5094466976516,46.8770769851343));
#33129=CARTESIAN_POINT('Ctrl Pts',(40.2836672525762,39.5136809484269,46.9477993807826));
#33130=CARTESIAN_POINT('Ctrl Pts',(40.2501321185274,39.5177193086722,47.0152499230846));
#33131=CARTESIAN_POINT('Ctrl Pts',(40.2198738423221,39.5217576689175,47.0842065286689));
#33132=CARTESIAN_POINT('Ctrl Pts',(40.19300846324,39.5257960291628,47.154317555125));
#33133=CARTESIAN_POINT('Ctrl Pts',(40.1608768226732,39.5306260053,47.2381720317349));
#33134=CARTESIAN_POINT('Ctrl Pts',(40.1334962853768,39.5354559814371,47.3239427193908));
#33135=CARTESIAN_POINT('Ctrl Pts',(40.1110689014416,39.5402859575742,47.4111155741981));
#33136=CARTESIAN_POINT('Ctrl Pts',(40.088734546621,39.5450958989001,47.4979268347359));
#33137=CARTESIAN_POINT('Ctrl Pts',(40.0713124680133,39.5499058402259,47.5861284659829));
#33138=CARTESIAN_POINT('Ctrl Pts',(40.0589554590699,39.5547157815518,47.6751909818351));
#33139=CARTESIAN_POINT('Ctrl Pts',(40.0466851433725,39.5594919777029,47.7636286605089));
#33140=CARTESIAN_POINT('Ctrl Pts',(40.0394091884403,39.5642681738539,47.8529149815301));
#33141=CARTESIAN_POINT('Ctrl Pts',(40.0372292376017,39.569044370005,47.9425129122682));
#33142=CARTESIAN_POINT('Ctrl Pts',(40.036776046103,39.5700372967507,47.9611394885191));
#33143=CARTESIAN_POINT('Ctrl Pts',(40.0365429267318,39.5710302234965,47.9797794737281));
#33144=CARTESIAN_POINT('Ctrl Pts',(40.036530522818,39.5720231502423,47.9984279538409));
#33145=CARTESIAN_POINT('',(40.0365306476135,40.3657731503002,48.001749637055));
#33146=CARTESIAN_POINT('Ctrl Pts',(40.0365305228177,39.5720231502717,47.998427954393));
#33147=CARTESIAN_POINT('Ctrl Pts',(40.036477506972,39.5762670422148,48.0781338690935));
#33148=CARTESIAN_POINT('Ctrl Pts',(40.0404608398097,39.580510934158,48.1578629671102));
#33149=CARTESIAN_POINT('Ctrl Pts',(40.0484609932266,39.5847548261011,48.2371808182024));
#33150=CARTESIAN_POINT('Ctrl Pts',(40.056461639913,39.588998979712,48.3165035598345));
#33151=CARTESIAN_POINT('Ctrl Pts',(40.0684795521282,39.5932431333228,48.3954145447556));
#33152=CARTESIAN_POINT('Ctrl Pts',(40.0844433687405,39.5974872869337,48.473484876559));
#33153=CARTESIAN_POINT('Ctrl Pts',(40.1004129449128,39.601732971786,48.5515833752332));
#33154=CARTESIAN_POINT('Ctrl Pts',(40.1203311600012,39.6059786566383,48.6288401662839));
#33155=CARTESIAN_POINT('Ctrl Pts',(40.1440759360515,39.6102243414906,48.704838320892));
#33156=CARTESIAN_POINT('Ctrl Pts',(40.1678524071262,39.614475693572,48.780937919429));
#33157=CARTESIAN_POINT('Ctrl Pts',(40.1954654925946,39.6187270456533,48.8557750881277));
#33158=CARTESIAN_POINT('Ctrl Pts',(40.226743968526,39.6229783977347,48.9289503014488));
#33159=CARTESIAN_POINT('Ctrl Pts',(40.258047098849,39.6272331008265,49.0021831931035));
#33160=CARTESIAN_POINT('Ctrl Pts',(40.2930211668911,39.6314878039184,49.0737511082556));
#33161=CARTESIAN_POINT('Ctrl Pts',(40.3314488740314,39.6357425070102,49.1432789161679));
#33162=CARTESIAN_POINT('Ctrl Pts',(40.3699442393029,39.640004701188,49.2129291389184));
#33163=CARTESIAN_POINT('Ctrl Pts',(40.4119051337497,39.6442668953659,49.2805316962437));
#33164=CARTESIAN_POINT('Ctrl Pts',(40.4570711621342,39.6485290895437,49.3457406778015));
#33165=CARTESIAN_POINT('Ctrl Pts',(40.4694083581805,39.6496933168854,49.3635526488388));
#33166=CARTESIAN_POINT('Ctrl Pts',(40.4819844690065,39.650857544227,49.3811862268741));
#33167=CARTESIAN_POINT('Ctrl Pts',(40.494793690343,39.6520217715687,49.3986348195806));
#33168=CARTESIAN_POINT('Ctrl Pts',(40.5413940908316,39.656257271835,49.462113417282));
#33169=CARTESIAN_POINT('Ctrl Pts',(40.5912590564143,39.6604927721012,49.5233811397024));
#33170=CARTESIAN_POINT('Ctrl Pts',(40.6441512579066,39.6647282723675,49.582082689302));
#33171=CARTESIAN_POINT('Ctrl Pts',(40.6969667824954,39.6689576325027,49.6406991402873));
#33172=CARTESIAN_POINT('Ctrl Pts',(40.7528005166242,39.673186992638,49.696756460248));
#33173=CARTESIAN_POINT('Ctrl Pts',(40.8113731440476,39.6774163527732,49.7499300424437));
#33174=CARTESIAN_POINT('Ctrl Pts',(40.869877370786,39.6816407738927,49.8030415289198));
#33175=CARTESIAN_POINT('Ctrl Pts',(40.9311137891788,39.6858651950122,49.8532756558546));
#33176=CARTESIAN_POINT('Ctrl Pts',(40.9947653397528,39.6900896161317,49.9003436506432));
#33177=CARTESIAN_POINT('Ctrl Pts',(41.0583761863633,39.6943113358138,49.9473815463388));
#33178=CARTESIAN_POINT('Ctrl Pts',(41.1243987234273,39.6985330554958,49.9912570501427));
#33179=CARTESIAN_POINT('Ctrl Pts',(41.1924827701755,39.7027547751778,50.0317215804772));
#33180=CARTESIAN_POINT('Ctrl Pts',(41.2605445401268,39.706975113532,50.0721728709977));
#33181=CARTESIAN_POINT('Ctrl Pts',(41.33066607723,39.7111954518861,50.1092151645504));
#33182=CARTESIAN_POINT('Ctrl Pts',(41.4024694359028,39.7154157902403,50.1426439775642));
#33183=CARTESIAN_POINT('Ctrl Pts',(41.4742717235175,39.7196360656416,50.1760722919354));
#33184=CARTESIAN_POINT('Ctrl Pts',(41.5477553567728,39.7238563410429,50.2058870360244));
#33185=CARTESIAN_POINT('Ctrl Pts',(41.6225204468284,39.7280766164441,50.2319309992247));
#33186=CARTESIAN_POINT('Ctrl Pts',(41.6973603193916,39.732301113104,50.2580010124554));
#33187=CARTESIAN_POINT('Ctrl Pts',(41.7734837649345,39.7365256097638,50.280292555667));
#33188=CARTESIAN_POINT('Ctrl Pts',(41.8504742561262,39.7407501064237,50.2986978700386));
#33189=CARTESIAN_POINT('Ctrl Pts',(41.9275017102515,39.7449766312533,50.3171120207535));
#33190=CARTESIAN_POINT('Ctrl Pts',(42.0053965772456,39.749203156083,50.3316361396397));
#33191=CARTESIAN_POINT('Ctrl Pts',(42.0837331589628,39.7534296809126,50.3422138515004));
#33192=CARTESIAN_POINT('Ctrl Pts',(42.1622129373251,39.757663931688,50.3528108990638));
#33193=CARTESIAN_POINT('Ctrl Pts',(42.2411355749332,39.7618981824633,50.3594470851074));
#33194=CARTESIAN_POINT('Ctrl Pts',(42.3200714844046,39.7661324332387,50.3621180904635));
#33195=CARTESIAN_POINT('Ctrl Pts',(42.3953555560499,39.770170793484,50.3646655262241));
#33196=CARTESIAN_POINT('Ctrl Pts',(42.4706513420945,39.7742091537293,50.363606594462));
#33197=CARTESIAN_POINT('Ctrl Pts',(42.5455907392309,39.7782475139745,50.3589815127614));
#33198=CARTESIAN_POINT('Ctrl Pts',(42.6241884415766,39.7824830142408,50.3541306491474));
#33199=CARTESIAN_POINT('Ctrl Pts',(42.7026928376915,39.786718514507,50.3453381299536));
#33200=CARTESIAN_POINT('Ctrl Pts',(42.7806767193037,39.7909540147733,50.3326113427402));
#33201=CARTESIAN_POINT('Ctrl Pts',(42.8585475490406,39.7951833749086,50.3199030053286));
#33202=CARTESIAN_POINT('Ctrl Pts',(42.9358989034339,39.7994127350438,50.3032718008792));
#33203=CARTESIAN_POINT('Ctrl Pts',(43.0123066713929,39.8036420951791,50.2827770327099));
#33204=CARTESIAN_POINT('Ctrl Pts',(43.0886252109205,39.8078665162986,50.2623061981807));
#33205=CARTESIAN_POINT('Ctrl Pts',(43.1640019027486,39.812090937418,50.2379808867639));
#33206=CARTESIAN_POINT('Ctrl Pts',(43.238022354535,39.8163153585375,50.2099115308536));
#33207=CARTESIAN_POINT('Ctrl Pts',(43.3119954716417,39.8205370782196,50.1818601247658));
#33208=CARTESIAN_POINT('Ctrl Pts',(43.3846136324202,39.8247587979016,50.15006959222));
#33209=CARTESIAN_POINT('Ctrl Pts',(43.4554783279712,39.8289805175836,50.1146999645536));
#33210=CARTESIAN_POINT('Ctrl Pts',(43.5263198369095,39.8332008559378,50.0793419096719));
#33211=CARTESIAN_POINT('Ctrl Pts',(43.5954086002184,39.837421194292,50.0404072944587));
#33212=CARTESIAN_POINT('Ctrl Pts',(43.6623681761319,39.8416415326461,49.9981033578845));
#33213=CARTESIAN_POINT('Ctrl Pts',(43.7293267532398,39.8458618080474,49.955800052339));
#33214=CARTESIAN_POINT('Ctrl Pts',(43.7941558100022,39.8500820834487,49.9101277771519));
#33215=CARTESIAN_POINT('Ctrl Pts',(43.8565067914275,39.8543023588499,49.8613378004611));
#33216=CARTESIAN_POINT('Ctrl Pts',(43.9189201383598,39.8585268555098,49.8124990224274));
#33217=CARTESIAN_POINT('Ctrl Pts',(43.9788500880155,39.8627513521696,49.7605366033697));
#33218=CARTESIAN_POINT('Ctrl Pts',(44.0359806744609,39.8669758488295,49.7057425578588));
#33219=CARTESIAN_POINT('Ctrl Pts',(44.0931386891514,39.8712023736591,49.6509222058699));
#33220=CARTESIAN_POINT('Ctrl Pts',(44.1474943408743,39.8754288984888,49.5932678612009));
#33221=CARTESIAN_POINT('Ctrl Pts',(44.1987699174329,39.8796554233184,49.5331070494386));
#33222=CARTESIAN_POINT('Ctrl Pts',(44.2501392240265,39.8838896740938,49.4728362657293));
#33223=CARTESIAN_POINT('Ctrl Pts',(44.2984169179976,39.8881239248691,49.4100502325925));
#33224=CARTESIAN_POINT('Ctrl Pts',(44.3433669636869,39.8923581756444,49.345107908441));
#33225=CARTESIAN_POINT('Ctrl Pts',(44.3862374706948,39.8963965358898,49.2831700322952));
#33226=CARTESIAN_POINT('Ctrl Pts',(44.4260812587883,39.9004348961351,49.2192712898739));
#33227=CARTESIAN_POINT('Ctrl Pts',(44.4627330113282,39.9044732563804,49.1537430237608));
#33228=CARTESIAN_POINT('Ctrl Pts',(44.5011739869249,39.9087087566467,49.0850158741981));
#33229=CARTESIAN_POINT('Ctrl Pts',(44.5362494416739,39.912944256913,49.0142347956722));
#33230=CARTESIAN_POINT('Ctrl Pts',(44.5677344726814,39.9171797571792,48.9417630789369));
#33231=CARTESIAN_POINT('Ctrl Pts',(44.5991738603877,39.9214091173145,48.8693964231874));
#33232=CARTESIAN_POINT('Ctrl Pts',(44.6270329750745,39.9256384774498,48.7953444231009));
#33233=CARTESIAN_POINT('Ctrl Pts',(44.651132252006,39.929867837585,48.7199958505982));
#33234=CARTESIAN_POINT('Ctrl Pts',(44.6752033859784,39.9340922587045,48.6447352696063));
#33235=CARTESIAN_POINT('Ctrl Pts',(44.6955232651173,39.938316679824,48.5681815697724));
#33236=CARTESIAN_POINT('Ctrl Pts',(44.7119605834352,39.9425411009435,48.4907430096722));
#33237=CARTESIAN_POINT('Ctrl Pts',(44.7283873903987,39.9467628206255,48.4133539700674));
#33238=CARTESIAN_POINT('Ctrl Pts',(44.7409364672251,39.9509845403076,48.3350816511724));
#33239=CARTESIAN_POINT('Ctrl Pts',(44.7495268148379,39.9552062599896,48.2563477857479));
#33240=CARTESIAN_POINT('Ctrl Pts',(44.7581143517271,39.9594265983437,48.1776396816935));
#33241=CARTESIAN_POINT('Ctrl Pts',(44.762745680528,39.9636469366979,48.0984707972066));
#33242=CARTESIAN_POINT('Ctrl Pts',(44.7633914432395,39.9678672750521,48.0192698448972));
#33243=CARTESIAN_POINT('Ctrl Pts',(44.7640371963184,39.9720875504533,47.9400700739924));
#33244=CARTESIAN_POINT('Ctrl Pts',(44.7606974989907,39.9763078258546,47.8608387055626));
#33245=CARTESIAN_POINT('Ctrl Pts',(44.7533951095284,39.9805281012559,47.7820048180627));
#33246=CARTESIAN_POINT('Ctrl Pts',(44.7460854159755,39.9847525979158,47.70309207831));
#33247=CARTESIAN_POINT('Ctrl Pts',(44.7348051558609,39.9889770945756,47.6245780821575));
#33248=CARTESIAN_POINT('Ctrl Pts',(44.7196289867533,39.9932015912355,47.5468865432213));
#33249=CARTESIAN_POINT('Ctrl Pts',(44.7044455316066,39.9974281160651,47.4691577047805));
#33250=CARTESIAN_POINT('Ctrl Pts',(44.6853625545606,40.0016546408947,47.3922525663273));
#33251=CARTESIAN_POINT('Ctrl Pts',(44.6625052738913,40.0058811657244,47.3165818801686));
#33252=CARTESIAN_POINT('Ctrl Pts',(44.6396062108793,40.0101154164997,47.2407728705324));
#33253=CARTESIAN_POINT('Ctrl Pts',(44.6129192163879,40.0143496672751,47.1662032653489));
#33254=CARTESIAN_POINT('Ctrl Pts',(44.582618491234,40.0185839180504,47.0932657706783));
#33255=CARTESIAN_POINT('Ctrl Pts',(44.5537195784492,40.0226222782957,47.0237026072055));
#33256=CARTESIAN_POINT('Ctrl Pts',(44.5215340929191,40.026660638541,46.9556241873224));
#33257=CARTESIAN_POINT('Ctrl Pts',(44.4862512681615,40.0306989987863,46.8893488004803));
#33258=CARTESIAN_POINT('Ctrl Pts',(44.4492460470873,40.0349344990526,46.8198380581086));
#33259=CARTESIAN_POINT('Ctrl Pts',(44.408692695973,40.0391699993188,46.7520466551394));
#33260=CARTESIAN_POINT('Ctrl Pts',(44.3647750819876,40.043405499585,46.6863602784246));
#33261=CARTESIAN_POINT('Ctrl Pts',(44.3209211346025,40.0476348597203,46.6207691261064));
#33262=CARTESIAN_POINT('Ctrl Pts',(44.2737128680956,40.0518642198556,46.5572773269405));
#33263=CARTESIAN_POINT('Ctrl Pts',(44.2233801075699,40.0560935799908,46.4962462222097));
#33264=CARTESIAN_POINT('Ctrl Pts',(44.173106125273,40.0603180011103,46.4352863891558));
#33265=CARTESIAN_POINT('Ctrl Pts',(44.1197151967979,40.0645424222298,46.3767819004132));
#33266=CARTESIAN_POINT('Ctrl Pts',(44.0634796436432,40.0687668433493,46.3210640524175));
#33267=CARTESIAN_POINT('Ctrl Pts',(44.0072800520618,40.0729885630313,46.2653818349325));
#33268=CARTESIAN_POINT('Ctrl Pts',(43.9482397788051,40.0772102827133,46.2124830507483));
#33269=CARTESIAN_POINT('Ctrl Pts',(43.8866696931503,40.0814320023954,46.1626639761959));
#33270=CARTESIAN_POINT('Ctrl Pts',(43.8251197529534,40.0856523407495,46.1128612022228));
#33271=CARTESIAN_POINT('Ctrl Pts',(43.7610420085747,40.0898726791037,46.0661364319965));
#33272=CARTESIAN_POINT('Ctrl Pts',(43.6947811369232,40.0940930174578,46.0227462862931));
#33273=CARTESIAN_POINT('Ctrl Pts',(43.628521253655,40.0983132928591,45.9793567878207));
#33274=CARTESIAN_POINT('Ctrl Pts',(43.5600787012306,40.1025335682604,45.9393020710057));
#33275=CARTESIAN_POINT('Ctrl Pts',(43.4898266587049,40.1067538436617,45.9027951232948));
#33276=CARTESIAN_POINT('Ctrl Pts',(43.4195043477707,40.1109783403215,45.8662516601315));
#33277=CARTESIAN_POINT('Ctrl Pts',(43.3473693486783,40.1152028369814,45.8332632717804));
#33278=CARTESIAN_POINT('Ctrl Pts',(43.2738184055801,40.1194273336412,45.803996394591));
#33279=CARTESIAN_POINT('Ctrl Pts',(43.2002321508665,40.1236538584708,45.7747154664504));
#33280=CARTESIAN_POINT('Ctrl Pts',(43.1252290428012,40.1278803833005,45.7491597603559));
#33281=CARTESIAN_POINT('Ctrl Pts',(43.0492222776242,40.1321069081301,45.7274461777251));
#33282=CARTESIAN_POINT('Ctrl Pts',(42.9730765746287,40.1363411589055,45.7056929033931));
#33283=CARTESIAN_POINT('Ctrl Pts',(42.8959240068713,40.1405754096808,45.6877958930098));
#33284=CARTESIAN_POINT('Ctrl Pts',(42.8181890923301,40.1448096604561,45.6738210894353));
#33285=CARTESIAN_POINT('Ctrl Pts',(42.7440504535926,40.1488480207015,45.6604928067742));
#33286=CARTESIAN_POINT('Ctrl Pts',(42.6693825180014,40.1528863809468,45.6507318576801));
#33287=CARTESIAN_POINT('Ctrl Pts',(42.5945553496412,40.1569247411921,45.6445512833377));
#33288=CARTESIAN_POINT('Ctrl Pts',(42.5160753547276,40.1611602414584,45.6380689928331));
#33289=CARTESIAN_POINT('Ctrl Pts',(42.4371218643529,40.1653957417246,45.6355009272594));
#33290=CARTESIAN_POINT('Ctrl Pts',(42.358118722558,40.1696312419909,45.6369011024716));
#33291=CARTESIAN_POINT('Ctrl Pts',(42.2792301102423,40.1738606021261,45.6382992478742));
#33292=CARTESIAN_POINT('Ctrl Pts',(42.200292454752,40.1780899622614,45.6436542019903));
#33293=CARTESIAN_POINT('Ctrl Pts',(42.1217339876723,40.1823193223966,45.6529681580168));
#33294=CARTESIAN_POINT('Ctrl Pts',(42.0432672605946,40.1865437435161,45.6622712372736));
#33295=CARTESIAN_POINT('Ctrl Pts',(41.9651793056406,40.1907681646356,45.6755240761237));
#33296=CARTESIAN_POINT('Ctrl Pts',(41.8878960760243,40.1949925857551,45.6926768730954));
#33297=CARTESIAN_POINT('Ctrl Pts',(41.8106622675724,40.1992143054372,45.7098187011778));
#33298=CARTESIAN_POINT('Ctrl Pts',(41.7342326200377,40.2034360251192,45.7308554360035));
#33299=CARTESIAN_POINT('Ctrl Pts',(41.6590244877631,40.2076577448012,45.7556859107591));
#33300=CARTESIAN_POINT('Ctrl Pts',(41.5838409632544,40.2118780831554,45.780508261094));
#33301=CARTESIAN_POINT('Ctrl Pts',(41.5098786057367,40.2160984215096,45.8091217395229));
#33302=CARTESIAN_POINT('Ctrl Pts',(41.4375397077592,40.2203187598637,45.8413752927478));
#33303=CARTESIAN_POINT('Ctrl Pts',(41.3652018888285,40.224539035265,45.8736283648609));
#33304=CARTESIAN_POINT('Ctrl Pts',(41.2944879094299,40.2287593106663,45.9095212114892));
#33305=CARTESIAN_POINT('Ctrl Pts',(41.2257787846763,40.2329795860676,45.9488552029699));
#33306=CARTESIAN_POINT('Ctrl Pts',(41.1570009347914,40.2372040827274,45.9882285376053));
#33307=CARTESIAN_POINT('Ctrl Pts',(41.0902323537357,40.2414285793873,46.0310496590746));
#33308=CARTESIAN_POINT('Ctrl Pts',(41.0258276543604,40.2456530760471,46.0770749350588));
#33309=CARTESIAN_POINT('Ctrl Pts',(40.9613920344571,40.2498796008768,46.1231223076577));
#33310=CARTESIAN_POINT('Ctrl Pts',(40.8993229252437,40.2541061257064,46.172376607114));
#33311=CARTESIAN_POINT('Ctrl Pts',(40.8399421797426,40.2583326505361,46.2245535664646));
#33312=CARTESIAN_POINT('Ctrl Pts',(40.7804528882295,40.2625669013114,46.2768259035476));
#33313=CARTESIAN_POINT('Ctrl Pts',(40.7236621176619,40.2668011520868,46.3320312481309));
#33314=CARTESIAN_POINT('Ctrl Pts',(40.6698549884491,40.2710354028621,46.3898482432064));
#33315=CARTESIAN_POINT('Ctrl Pts',(40.6185371560732,40.2750737631074,46.4449904317077));
#33316=CARTESIAN_POINT('Ctrl Pts',(40.5699332062563,40.2791121233527,46.5025076708174));
#33317=CARTESIAN_POINT('Ctrl Pts',(40.5242543085212,40.283150483598,46.562095781424));
#33318=CARTESIAN_POINT('Ctrl Pts',(40.4762651280949,40.2873930903168,46.6246976552202));
#33319=CARTESIAN_POINT('Ctrl Pts',(40.4313198957796,40.2916356970356,46.6898264207477));
#33320=CARTESIAN_POINT('Ctrl Pts',(40.3896950661176,40.2958783037544,46.7571546702393));
#33321=CARTESIAN_POINT('Ctrl Pts',(40.3481300765327,40.3001148112792,46.8243861282804));
#33322=CARTESIAN_POINT('Ctrl Pts',(40.3098762568635,40.3043513188039,46.8938104002843));
#33323=CARTESIAN_POINT('Ctrl Pts',(40.2751690774718,40.3085878263287,46.9650681222574));
#33324=CARTESIAN_POINT('Ctrl Pts',(40.2405010940688,40.3128195494226,47.0362453704808));
#33325=CARTESIAN_POINT('Ctrl Pts',(40.2093720001794,40.3170512725164,47.1092515396943));
#33326=CARTESIAN_POINT('Ctrl Pts',(40.1819725145746,40.3212829956103,47.1837007198352));
#33327=CARTESIAN_POINT('Ctrl Pts',(40.154595210532,40.3255112928651,47.2580896288038));
#33328=CARTESIAN_POINT('Ctrl Pts',(40.1309416771006,40.3297395901198,47.3339187912001));
#33329=CARTESIAN_POINT('Ctrl Pts',(40.1111548526966,40.3339678873746,47.4107815917966));
#33330=CARTESIAN_POINT('Ctrl Pts',(40.0913774547657,40.3381941702622,47.4876077748389));
#33331=CARTESIAN_POINT('Ctrl Pts',(40.0754632205032,40.3424204531497,47.5654661658495));
#33332=CARTESIAN_POINT('Ctrl Pts',(40.0635050627558,40.3466467360373,47.6439356109743));
#33333=CARTESIAN_POINT('Ctrl Pts',(40.0515462945462,40.350873234676,47.7224090619528));
#33334=CARTESIAN_POINT('Ctrl Pts',(40.0435440831736,40.3550997333147,47.8014931688741));
#33335=CARTESIAN_POINT('Ctrl Pts',(40.0395399008274,40.3593262319534,47.8807583918517));
#33336=CARTESIAN_POINT('Ctrl Pts',(40.0375039652753,40.3614752047262,47.9210609733895));
#33337=CARTESIAN_POINT('Ctrl Pts',(40.0365007850733,40.3636241774989,47.9614102878016));
#33338=CARTESIAN_POINT('Ctrl Pts',(40.0365306476131,40.3657731502717,48.0017496365208));
#33339=CARTESIAN_POINT('',(40.0365301409399,41.1595231502254,48.0008162196351));
#33340=CARTESIAN_POINT('Ctrl Pts',(40.0365306476135,40.3657731503002,48.001749637055));
#33341=CARTESIAN_POINT('Ctrl Pts',(40.0365982547737,40.37063830587,48.0930756927361));
#33342=CARTESIAN_POINT('Ctrl Pts',(40.0419631966318,40.3755034614398,48.1841861615192));
#33343=CARTESIAN_POINT('Ctrl Pts',(40.052526975406,40.3803686170097,48.2745192884));
#33344=CARTESIAN_POINT('Ctrl Pts',(40.063191471508,40.385280158014,48.3657136706464));
#33345=CARTESIAN_POINT('Ctrl Pts',(40.0791543076126,40.3901916990183,48.4561156530629));
#33346=CARTESIAN_POINT('Ctrl Pts',(40.1002644889058,40.3951032400226,48.5451669651698));
#33347=CARTESIAN_POINT('Ctrl Pts',(40.1207132863672,40.3998609020164,48.631428291856));
#33348=CARTESIAN_POINT('Ctrl Pts',(40.1459915809743,40.4046185640101,48.7164222519164));
#33349=CARTESIAN_POINT('Ctrl Pts',(40.1759197402339,40.4093762260039,48.7996608274879));
#33350=CARTESIAN_POINT('Ctrl Pts',(40.2025632316544,40.4136117262702,48.8737638237618));
#33351=CARTESIAN_POINT('Ctrl Pts',(40.2329649197856,40.4178472265364,48.9466746320274));
#33352=CARTESIAN_POINT('Ctrl Pts',(40.2669982082182,40.4220827268027,49.017985165489));
#33353=CARTESIAN_POINT('Ctrl Pts',(40.3009821591852,40.426312086938,49.0891923213119));
#33354=CARTESIAN_POINT('Ctrl Pts',(40.3385870553058,40.4305414470732,49.1588033892228));
#33355=CARTESIAN_POINT('Ctrl Pts',(40.3796373233663,40.4347708072085,49.2264277784547));
#33356=CARTESIAN_POINT('Ctrl Pts',(40.4206396532244,40.438995228328,49.2939731964204));
#33357=CARTESIAN_POINT('Ctrl Pts',(40.4650791173327,40.4432196494475,49.3595361469052));
#33358=CARTESIAN_POINT('Ctrl Pts',(40.5127337732114,40.447444070567,49.4227496723328));
#33359=CARTESIAN_POINT('Ctrl Pts',(40.5603579548384,40.451665790249,49.4859227739057));
#33360=CARTESIAN_POINT('Ctrl Pts',(40.611192965633,40.4558875099311,49.5467490586181));
#33361=CARTESIAN_POINT('Ctrl Pts',(40.6649736873588,40.4601092296131,49.6048906926463));
#33362=CARTESIAN_POINT('Ctrl Pts',(40.718736812272,40.4643295679673,49.6630133029908));
#33363=CARTESIAN_POINT('Ctrl Pts',(40.7754434158152,40.4685499063214,49.7184526625828));
#33364=CARTESIAN_POINT('Ctrl Pts',(40.834789229615,40.4727702446756,49.7709053292514));
#33365=CARTESIAN_POINT('Ctrl Pts',(40.8941341581803,40.4769905200768,49.8233572135073));
#33366=CARTESIAN_POINT('Ctrl Pts',(40.9561178661875,40.4812107954781,49.8728221835688));
#33367=CARTESIAN_POINT('Ctrl Pts',(41.0204016146411,40.4854310708794,49.9190358871097));
#33368=CARTESIAN_POINT('Ctrl Pts',(41.0847496618188,40.4896555675393,49.9652958151203));
#33369=CARTESIAN_POINT('Ctrl Pts',(41.1514019631305,40.4938800641991,50.0082977056594));
#33370=CARTESIAN_POINT('Ctrl Pts',(41.219989776019,40.4981045608589,50.0478198925199));
#33371=CARTESIAN_POINT('Ctrl Pts',(41.288610517737,40.5023310856886,50.087361053879));
#33372=CARTESIAN_POINT('Ctrl Pts',(41.3591682036669,40.5065576105182,50.123418969649));
#33373=CARTESIAN_POINT('Ctrl Pts',(41.4312706986902,40.5107841353479,50.1558186337639));
#33374=CARTESIAN_POINT('Ctrl Pts',(41.5035049946572,40.5150183861232,50.1882775233787));
#33375=CARTESIAN_POINT('Ctrl Pts',(41.5772893040498,40.5192526368986,50.2170646277777));
#33376=CARTESIAN_POINT('Ctrl Pts',(41.6522129720365,40.5234868876739,50.2420537463918));
#33377=CARTESIAN_POINT('Ctrl Pts',(41.7236704218381,40.5275252479192,50.2658867852291));
#33378=CARTESIAN_POINT('Ctrl Pts',(41.796163786748,40.5315636081644,50.2862654205252));
#33379=CARTESIAN_POINT('Ctrl Pts',(41.869328707653,40.5356019684097,50.3031236224699));
#33380=CARTESIAN_POINT('Ctrl Pts',(41.94606530943,40.5398374686759,50.3208047887078));
#33381=CARTESIAN_POINT('Ctrl Pts',(42.0238324000669,40.5440729689422,50.3346802424668));
#33382=CARTESIAN_POINT('Ctrl Pts',(42.1022182795349,40.5483084692084,50.3446356833967));
#33383=CARTESIAN_POINT('Ctrl Pts',(42.1804905243584,40.5525378293437,50.3545766920972));
#33384=CARTESIAN_POINT('Ctrl Pts',(42.2593793149624,40.5567671894789,50.3606089143199));
#33385=CARTESIAN_POINT('Ctrl Pts',(42.3384611699351,40.5609965496142,50.3626687057847));
#33386=CARTESIAN_POINT('Ctrl Pts',(42.4174506736971,40.5652209707337,50.3647260918401));
#33387=CARTESIAN_POINT('Ctrl Pts',(42.4966323270434,40.5694453918532,50.3628202534882));
#33388=CARTESIAN_POINT('Ctrl Pts',(42.5755774393607,40.5736698129727,50.3569393296578));
#33389=CARTESIAN_POINT('Ctrl Pts',(42.6544720677708,40.5778915326547,50.3510621665669));
#33390=CARTESIAN_POINT('Ctrl Pts',(42.7331299885875,40.5821132523367,50.3412149980812));
#33391=CARTESIAN_POINT('Ctrl Pts',(42.8111236473736,40.5863349720188,50.327438030855));
#33392=CARTESIAN_POINT('Ctrl Pts',(42.8890917869819,40.5905553103729,50.3136655713911));
#33393=CARTESIAN_POINT('Ctrl Pts',(42.9663956342856,40.5947756487271,50.2959659479658));
#33394=CARTESIAN_POINT('Ctrl Pts',(43.042615379302,40.5989959870812,50.2744308991888));
#33395=CARTESIAN_POINT('Ctrl Pts',(43.118833987383,40.6032162624825,50.2528961716403));
#33396=CARTESIAN_POINT('Ctrl Pts',(43.1939680740145,40.6074365378838,50.2275262613617));
#33397=CARTESIAN_POINT('Ctrl Pts',(43.2676120565571,40.6116568132851,50.1984630449968));
#33398=CARTESIAN_POINT('Ctrl Pts',(43.3413297002385,40.6158813099449,50.169370758645));
#33399=CARTESIAN_POINT('Ctrl Pts',(43.4135538248403,40.6201058066047,50.1365779593506));
#33400=CARTESIAN_POINT('Ctrl Pts',(43.4838985162758,40.6243303032646,50.100274850422));
#33401=CARTESIAN_POINT('Ctrl Pts',(43.5542769800138,40.6285568280942,50.0639543124657));
#33402=CARTESIAN_POINT('Ctrl Pts',(43.6227738067827,40.6327833529239,50.0241203438456));
#33403=CARTESIAN_POINT('Ctrl Pts',(43.6890296698075,40.6370098777535,49.9810080644096));
#33404=CARTESIAN_POINT('Ctrl Pts',(43.7554066463287,40.6412441285289,49.9378169771722));
#33405=CARTESIAN_POINT('Ctrl Pts',(43.819534092501,40.6454783793042,49.8913358805884));
#33406=CARTESIAN_POINT('Ctrl Pts',(43.8810837093347,40.6497126300795,49.8418418734634));
#33407=CARTESIAN_POINT('Ctrl Pts',(43.9397858360921,40.6537509903249,49.7946376237956));
#33408=CARTESIAN_POINT('Ctrl Pts',(43.9961431337756,40.6577893505702,49.744693337531));
#33409=CARTESIAN_POINT('Ctrl Pts',(44.0499029542822,40.6618277108155,49.6922797293447));
#33410=CARTESIAN_POINT('Ctrl Pts',(44.1062871598103,40.6660632110818,49.6373074539799));
#33411=CARTESIAN_POINT('Ctrl Pts',(44.1600281400338,40.670298711348,49.5794096505003));
#33412=CARTESIAN_POINT('Ctrl Pts',(44.2108070389384,40.6745342116143,49.5188707346681));
#33413=CARTESIAN_POINT('Ctrl Pts',(44.2615123245573,40.6787635717495,49.4584195810482));
#33414=CARTESIAN_POINT('Ctrl Pts',(44.3092637570627,40.6829929318848,49.3953352749048));
#33415=CARTESIAN_POINT('Ctrl Pts',(44.3537787099889,40.68722229202,49.3299395449772));
#33416=CARTESIAN_POINT('Ctrl Pts',(44.3982416786794,40.6914467131395,49.2646201837036));
#33417=CARTESIAN_POINT('Ctrl Pts',(44.4394754156993,40.695671134259,49.1969951485624));
#33418=CARTESIAN_POINT('Ctrl Pts',(44.4772380275817,40.6998955553785,49.1274185636526));
#33419=CARTESIAN_POINT('Ctrl Pts',(44.5149764909875,40.7041172750605,49.0578864716538));
#33420=CARTESIAN_POINT('Ctrl Pts',(44.5492480116388,40.7083389947426,48.9864057182537));
#33421=CARTESIAN_POINT('Ctrl Pts',(44.5798551011486,40.7125607144246,48.9133576401917));
#33422=CARTESIAN_POINT('Ctrl Pts',(44.610452176155,40.7167810527787,48.8403334631356));
#33423=CARTESIAN_POINT('Ctrl Pts',(44.6373870195651,40.7210013911329,48.765743412272));
#33424=CARTESIAN_POINT('Ctrl Pts',(44.6605096724967,40.7252217294871,48.6899901893861));
#33425=CARTESIAN_POINT('Ctrl Pts',(44.6836319805181,40.7294420048883,48.6142380964766));
#33426=CARTESIAN_POINT('Ctrl Pts',(44.7029420753495,40.7336622802896,48.5373233153283));
#33427=CARTESIAN_POINT('Ctrl Pts',(44.7183398624741,40.7378825556909,48.4596637063808));
#33428=CARTESIAN_POINT('Ctrl Pts',(44.7337530509729,40.7421070523507,48.3819264197327));
#33429=CARTESIAN_POINT('Ctrl Pts',(44.7452460231156,40.7463315490106,48.3034432785405));
#33430=CARTESIAN_POINT('Ctrl Pts',(44.7527699689865,40.7505560456704,48.2246417457535));
#33431=CARTESIAN_POINT('Ctrl Pts',(44.7602975270842,40.7547825705001,48.1458023805566));
#33432=CARTESIAN_POINT('Ctrl Pts',(44.7638522417978,40.7590090953297,48.0666447887745));
#33433=CARTESIAN_POINT('Ctrl Pts',(44.7634374627916,40.7632356201594,47.9875983721466));
#33434=CARTESIAN_POINT('Ctrl Pts',(44.7630219255832,40.7674698709347,47.9084074613192));
#33435=CARTESIAN_POINT('Ctrl Pts',(44.758622421402,40.77170412171,47.8293286015956));
#33436=CARTESIAN_POINT('Ctrl Pts',(44.7502943911612,40.7759383724854,47.7507878097357));
#33437=CARTESIAN_POINT('Ctrl Pts',(44.7423516433102,40.7799767327307,47.675880576246));
#33438=CARTESIAN_POINT('Ctrl Pts',(44.7308359152055,40.784015092976,47.6014630733394));
#33439=CARTESIAN_POINT('Ctrl Pts',(44.7158382050134,40.7880534532213,47.5278942394968));
#33440=CARTESIAN_POINT('Ctrl Pts',(44.7001083538726,40.7922889534876,47.4507340070262));
#33441=CARTESIAN_POINT('Ctrl Pts',(44.6804880890839,40.7965244537538,47.3742141154112));
#33442=CARTESIAN_POINT('Ctrl Pts',(44.6570441138962,40.8007599540201,47.2987565980157));
#33443=CARTESIAN_POINT('Ctrl Pts',(44.6336341250311,40.8049893141553,47.2234084700693));
#33444=CARTESIAN_POINT('Ctrl Pts',(44.6064115715956,40.8092186742906,47.1491201023906));
#33445=CARTESIAN_POINT('Ctrl Pts',(44.5754941379767,40.8134480344259,47.0763032442792));
#33446=CARTESIAN_POINT('Ctrl Pts',(44.5446128095101,40.8176724555454,47.0035714211611));
#33447=CARTESIAN_POINT('Ctrl Pts',(44.5100453577583,40.8218968766648,46.9323081225715));
#33448=CARTESIAN_POINT('Ctrl Pts',(44.4719587487204,40.8261212977843,46.8629083658293));
#33449=CARTESIAN_POINT('Ctrl Pts',(44.4338964953491,40.8303430174664,46.7935529889197));
#33450=CARTESIAN_POINT('Ctrl Pts',(44.3923197765235,40.8345647371484,46.7260591989381));
#33451=CARTESIAN_POINT('Ctrl Pts',(44.3474424676075,40.8387864568304,46.6607993890911));
#33452=CARTESIAN_POINT('Ctrl Pts',(44.3025798423472,40.8430067951846,46.5955609319632));
#33453=CARTESIAN_POINT('Ctrl Pts',(44.254419037141,40.8472271335388,46.5325553899907));
#33454=CARTESIAN_POINT('Ctrl Pts',(44.2032176090137,40.8514474718929,46.4721267410407));
#33455=CARTESIAN_POINT('Ctrl Pts',(44.1520169446349,40.8556677472942,46.4116989934774));
#33456=CARTESIAN_POINT('Ctrl Pts',(44.0977760519236,40.8598880226955,46.3538484197605));
#33457=CARTESIAN_POINT('Ctrl Pts',(44.0407922129559,40.8641082980968,46.2988852611293));
#33458=CARTESIAN_POINT('Ctrl Pts',(43.9837513768743,40.8683327947566,46.2438671265351));
#33459=CARTESIAN_POINT('Ctrl Pts',(43.9239624525029,40.8725572914165,46.1917425029625));
#33460=CARTESIAN_POINT('Ctrl Pts',(43.8617585424306,40.8767817880763,46.142783694738));
#33461=CARTESIAN_POINT('Ctrl Pts',(43.7995247684237,40.881008312906,46.0938013815176));
#33462=CARTESIAN_POINT('Ctrl Pts',(43.7348740824683,40.8852348377356,46.0479881832126));
#33463=CARTESIAN_POINT('Ctrl Pts',(43.6681694356189,40.8894613625653,46.0055735853479));
#33464=CARTESIAN_POINT('Ctrl Pts',(43.6013428549113,40.8936956133406,45.9630814550202));
#33465=CARTESIAN_POINT('Ctrl Pts',(43.5324552201012,40.897929864116,45.9240005714261));
#33466=CARTESIAN_POINT('Ctrl Pts',(43.4618948163027,40.9021641148913,45.8885147786429));
#33467=CARTESIAN_POINT('Ctrl Pts',(43.3945987715684,40.9062024751366,45.8546706767102));
#33468=CARTESIAN_POINT('Ctrl Pts',(43.3257816520912,40.9102408353819,45.8240964915293));
#33469=CARTESIAN_POINT('Ctrl Pts',(43.2557945644409,40.9142791956273,45.7969098737515));
#33470=CARTESIAN_POINT('Ctrl Pts',(43.1823909277244,40.9185146958935,45.7683960909681));
#33471=CARTESIAN_POINT('Ctrl Pts',(43.1074211549665,40.9227501961598,45.7435006742057));
#33472=CARTESIAN_POINT('Ctrl Pts',(43.031276273961,40.926985696426,45.7223958406181));
#33473=CARTESIAN_POINT('Ctrl Pts',(42.9552417788638,40.9312150565613,45.7013216023402));
#33474=CARTESIAN_POINT('Ctrl Pts',(42.8780360069106,40.9354444166965,45.6840271591567));
#33475=CARTESIAN_POINT('Ctrl Pts',(42.8000689170705,40.9396737768318,45.6706362880619));
#33476=CARTESIAN_POINT('Ctrl Pts',(42.7221928766266,40.9438981979513,45.6572610547283));
#33477=CARTESIAN_POINT('Ctrl Pts',(42.643557745202,40.9481226190708,45.6477804138057));
#33478=CARTESIAN_POINT('Ctrl Pts',(42.5645860706328,40.9523470401903,45.6422676432102));
#33479=CARTESIAN_POINT('Ctrl Pts',(42.4856648969569,40.9565687598723,45.6367583979273));
#33480=CARTESIAN_POINT('Ctrl Pts',(42.4064080742356,40.9607904795543,45.6352120194146));
#33481=CARTESIAN_POINT('Ctrl Pts',(42.327244500359,40.9650121992364,45.6376500940437));
#33482=CARTESIAN_POINT('Ctrl Pts',(42.2481068284513,40.9692325375905,45.6400873709456));
#33483=CARTESIAN_POINT('Ctrl Pts',(42.1690628135786,40.9734528759447,45.6465064978454));
#33484=CARTESIAN_POINT('Ctrl Pts',(42.0905410869398,40.9776732142988,45.6568769511552));
#33485=CARTESIAN_POINT('Ctrl Pts',(42.0120205315739,40.9818934897001,45.6672472497738));
#33486=CARTESIAN_POINT('Ctrl Pts',(41.9340227140917,40.9861137651014,45.6815686948655));
#33487=CARTESIAN_POINT('Ctrl Pts',(41.8569693831561,40.9903340405027,45.6997591017309));
#33488=CARTESIAN_POINT('Ctrl Pts',(41.779838980939,40.9945585371625,45.7179677032408));
#33489=CARTESIAN_POINT('Ctrl Pts',(41.7036554103252,40.9987830338224,45.740052888968));
#33490=CARTESIAN_POINT('Ctrl Pts',(41.6288278925616,41.0030075304822,45.7658818246098));
#33491=CARTESIAN_POINT('Ctrl Pts',(41.5539644503024,41.0072340553119,45.791723160656));
#33492=CARTESIAN_POINT('Ctrl Pts',(41.4804587938383,41.0114605801415,45.8213116516826));
#33493=CARTESIAN_POINT('Ctrl Pts',(41.4087002803684,41.0156871049712,45.8544661953821));
#33494=CARTESIAN_POINT('Ctrl Pts',(41.3368105947416,41.0199213557465,45.8876813444759));
#33495=CARTESIAN_POINT('Ctrl Pts',(41.266674850631,41.0241556065219,45.9244753533669));
#33496=CARTESIAN_POINT('Ctrl Pts',(41.1986577250075,41.0283898572972,45.9646211214578));
#33497=CARTESIAN_POINT('Ctrl Pts',(41.1337872979375,41.0324282175425,46.0029096127346));
#33498=CARTESIAN_POINT('Ctrl Pts',(41.0708440741402,41.0364665777878,46.0442463676946));
#33499=CARTESIAN_POINT('Ctrl Pts',(41.0101169467817,41.0405049380331,46.0883997438594));
#33500=CARTESIAN_POINT('Ctrl Pts',(40.9469663954162,41.0447044562254,46.1343151390172));
#33501=CARTESIAN_POINT('Ctrl Pts',(40.8859635327625,41.0489039744176,46.183457914074));
#33502=CARTESIAN_POINT('Ctrl Pts',(40.8274614140943,41.0531034926098,46.2355984479893));
#33503=CARTESIAN_POINT('Ctrl Pts',(40.7690443249774,41.0572969070377,46.2876631985604));
#33504=CARTESIAN_POINT('Ctrl Pts',(40.7131211190808,41.0614903214655,46.3427167443031));
#33505=CARTESIAN_POINT('Ctrl Pts',(40.6600146796133,41.0656837358934,46.4004870973516));
#33506=CARTESIAN_POINT('Ctrl Pts',(40.6069695066388,41.069872312569,46.4581908033612));
#33507=CARTESIAN_POINT('Ctrl Pts',(40.5567349671245,41.0740608892447,46.5186047406997));
#33508=CARTESIAN_POINT('Ctrl Pts',(40.5095984934268,41.0782494659203,46.5814188127409));
#33509=CARTESIAN_POINT('Ctrl Pts',(40.4624910896804,41.0824354594218,46.6441941461604));
#33510=CARTESIAN_POINT('Ctrl Pts',(40.4184782474128,41.0866214529232,46.709366296129));
#33511=CARTESIAN_POINT('Ctrl Pts',(40.3778074617442,41.0908074464247,46.7765917365317));
#33512=CARTESIAN_POINT('Ctrl Pts',(40.3371485197186,41.094992220933,46.8437976003735));
#33513=CARTESIAN_POINT('Ctrl Pts',(40.2998299494773,41.0991769954412,46.9130551586631));
#33514=CARTESIAN_POINT('Ctrl Pts',(40.2660552989271,41.1033617699494,46.9839928870017));
#33515=CARTESIAN_POINT('Ctrl Pts',(40.232279489984,41.1075466879859,47.0549330483418));
#33516=CARTESIAN_POINT('Ctrl Pts',(40.2020480453447,41.1117316060223,47.1275530613374));
#33517=CARTESIAN_POINT('Ctrl Pts',(40.1755173132373,41.1159165240587,47.2014593202643));
#33518=CARTESIAN_POINT('Ctrl Pts',(40.1489607095979,41.1201055230319,47.2754376491261));
#33519=CARTESIAN_POINT('Ctrl Pts',(40.1261121823859,41.1242945220051,47.3507042762981));
#33520=CARTESIAN_POINT('Ctrl Pts',(40.1070786252969,41.1284835209783,47.4268490510088));
#33521=CARTESIAN_POINT('Ctrl Pts',(40.0880345971696,41.1326748244691,47.5030357156744));
#33522=CARTESIAN_POINT('Ctrl Pts',(40.0728098073642,41.13686612796,47.5801010200745));
#33523=CARTESIAN_POINT('Ctrl Pts',(40.0614597913776,41.1410574314508,47.6576257405177));
#33524=CARTESIAN_POINT('Ctrl Pts',(40.0500915413763,41.1452554683497,47.7352750058851));
#33525=CARTESIAN_POINT('Ctrl Pts',(40.0426105323222,41.1494535052486,47.8133846847294));
#33526=CARTESIAN_POINT('Ctrl Pts',(40.0390202890001,41.1536515421475,47.891532285233));
#33527=CARTESIAN_POINT('Ctrl Pts',(40.0373464509499,41.1556087448401,47.9279661465382));
#33528=CARTESIAN_POINT('Ctrl Pts',(40.0365175675292,41.1575659475328,47.9644082776245));
#33529=CARTESIAN_POINT('Ctrl Pts',(40.0365301409399,41.1595231502254,48.0008162196351));
#33530=CARTESIAN_POINT('',(40.0365310012703,41.953273150305,47.9978244670332));
#33531=CARTESIAN_POINT('Ctrl Pts',(40.0365301409402,41.1595231502717,48.0008162204963));
#33532=CARTESIAN_POINT('Ctrl Pts',(40.0365455750992,41.1619256603275,48.0455077831622));
#33533=CARTESIAN_POINT('Ctrl Pts',(40.0378285482484,41.1643281703832,48.0901759288546));
#33534=CARTESIAN_POINT('Ctrl Pts',(40.0403756299082,41.1667306804389,48.1347711874589));
#33535=CARTESIAN_POINT('Ctrl Pts',(40.0448660023929,41.1709661807051,48.2133903088399));
#33536=CARTESIAN_POINT('Ctrl Pts',(40.0532984169016,41.1752016809713,48.2919342009553));
#33537=CARTESIAN_POINT('Ctrl Pts',(40.0656674450805,41.1794371812375,48.369975626147));
#33538=CARTESIAN_POINT('Ctrl Pts',(40.0780185420946,41.1836665413727,48.4479039160434));
#33539=CARTESIAN_POINT('Ctrl Pts',(40.0942948471514,41.1878959015079,48.5253307258805));
#33540=CARTESIAN_POINT('Ctrl Pts',(40.1144390024818,41.1921252616431,48.6018316770691));
#33541=CARTESIAN_POINT('Ctrl Pts',(40.1345596336153,41.1963496827626,48.6782432910075));
#33542=CARTESIAN_POINT('Ctrl Pts',(40.158539020312,41.200574103882,48.7537307433428));
#33543=CARTESIAN_POINT('Ctrl Pts',(40.1862686316953,41.2047985250015,48.8278791396597));
#33544=CARTESIAN_POINT('Ctrl Pts',(40.2139805105162,41.2090202446835,48.9019801194787));
#33545=CARTESIAN_POINT('Ctrl Pts',(40.2454376901529,41.2132419643655,48.9747433044258));
#33546=CARTESIAN_POINT('Ctrl Pts',(40.2804819684672,41.2174636840476,49.0457694559066));
#33547=CARTESIAN_POINT('Ctrl Pts',(40.3155147804497,41.2216840224017,49.116772367947));
#33548=CARTESIAN_POINT('Ctrl Pts',(40.3541321530474,41.2259043607559,49.1860389544874));
#33549=CARTESIAN_POINT('Ctrl Pts',(40.396128575788,41.23012469911,49.2531918273458));
#33550=CARTESIAN_POINT('Ctrl Pts',(40.438124372087,41.2343449745113,49.3203436985154));
#33551=CARTESIAN_POINT('Ctrl Pts',(40.4834988683402,41.2385652499126,49.3853815214434));
#33552=CARTESIAN_POINT('Ctrl Pts',(40.5320023974853,41.2427855253139,49.4479555925163));
#33553=CARTESIAN_POINT('Ctrl Pts',(40.5805544414589,41.2470100219738,49.5105922522376));
#33554=CARTESIAN_POINT('Ctrl Pts',(40.6322414821881,41.2512345186336,49.5707598654583));
#33555=CARTESIAN_POINT('Ctrl Pts',(40.6867729571565,41.2554590152935,49.6281411304214));
#33556=CARTESIAN_POINT('Ctrl Pts',(40.7413306125435,41.2596855401231,49.6855499439798));
#33557=CARTESIAN_POINT('Ctrl Pts',(40.7987350821282,41.2639120649528,49.7401694204061));
#33558=CARTESIAN_POINT('Ctrl Pts',(40.8586601173245,41.2681385897825,49.7917203484288));
#33559=CARTESIAN_POINT('Ctrl Pts',(40.9186946934761,41.2723728405578,49.8433655098197));
#33560=CARTESIAN_POINT('Ctrl Pts',(40.9812586703905,41.2766070913331,49.8919306257449));
#33561=CARTESIAN_POINT('Ctrl Pts',(41.0459941758621,41.2808413421085,49.9371780168846));
#33562=CARTESIAN_POINT('Ctrl Pts',(41.1077348014509,41.284879702354,49.9803321131547));
#33563=CARTESIAN_POINT('Ctrl Pts',(41.171450152885,41.2889180625995,50.0204685146466));
#33564=CARTESIAN_POINT('Ctrl Pts',(41.236809649188,41.292956422845,50.0574203869598));
#33565=CARTESIAN_POINT('Ctrl Pts',(41.3053597901279,41.2971919231113,50.09617613323));
#33566=CARTESIAN_POINT('Ctrl Pts',(41.3759792723293,41.3014274233775,50.1315758131263));
#33567=CARTESIAN_POINT('Ctrl Pts',(41.4483058402374,41.3056629236438,50.1633928601097));
#33568=CARTESIAN_POINT('Ctrl Pts',(41.5205275575793,41.3098922837791,50.1951637824742));
#33569=CARTESIAN_POINT('Ctrl Pts',(41.5944510202613,41.3141216439143,50.2233621982639));
#33570=CARTESIAN_POINT('Ctrl Pts',(41.6696882839139,41.3183510040496,50.2478067617674));
#33571=CARTESIAN_POINT('Ctrl Pts',(41.7448376860415,41.3225754251691,50.2722227790889));
#33572=CARTESIAN_POINT('Ctrl Pts',(41.8212973962415,41.3267998462886,50.292893511118));
#33573=CARTESIAN_POINT('Ctrl Pts',(41.8986597623857,41.3310242674081,50.3096857810206));
#33574=CARTESIAN_POINT('Ctrl Pts',(41.975972656759,41.3352459870901,50.326467312584));
#33575=CARTESIAN_POINT('Ctrl Pts',(42.0541866039638,41.3394677067721,50.3393752054039));
#33576=CARTESIAN_POINT('Ctrl Pts',(42.1328802471267,41.3436894264542,50.348326527237));
#33577=CARTESIAN_POINT('Ctrl Pts',(42.2115481420801,41.3479097648083,50.3572749202374));
#33578=CARTESIAN_POINT('Ctrl Pts',(42.290694955341,41.3521301031625,50.3622692598365));
#33579=CARTESIAN_POINT('Ctrl Pts',(42.3698921134399,41.3563504415166,50.3632782223147));
#33580=CARTESIAN_POINT('Ctrl Pts',(42.4490880901907,41.3605707169179,50.3642871697427));
#33581=CARTESIAN_POINT('Ctrl Pts',(42.5283339409563,41.3647909923191,50.3613108535745));
#33582=CARTESIAN_POINT('Ctrl Pts',(42.6072004874271,41.3690112677204,50.3543700641382));
#33583=CARTESIAN_POINT('Ctrl Pts',(42.6861459188172,41.3732357643802,50.3474223322955));
#33584=CARTESIAN_POINT('Ctrl Pts',(42.7647108193664,41.3774602610401,50.3365022470497));
#33585=CARTESIAN_POINT('Ctrl Pts',(42.8424711375432,41.3816847576999,50.321682522082));
#33586=CARTESIAN_POINT('Ctrl Pts',(42.9202687882454,41.3859112825295,50.3068556822032));
#33587=CARTESIAN_POINT('Ctrl Pts',(42.9972606303851,41.3901378073592,50.288125584035));
#33588=CARTESIAN_POINT('Ctrl Pts',(43.073035341738,41.3943643321888,50.2656155608734));
#33589=CARTESIAN_POINT('Ctrl Pts',(43.1489485667229,41.3985985829641,50.2430643901441));
#33590=CARTESIAN_POINT('Ctrl Pts',(43.2236397713106,41.4028328337395,50.2167196439986));
#33591=CARTESIAN_POINT('Ctrl Pts',(43.2967154547051,41.4070670845148,50.1867537205166));
#33592=CARTESIAN_POINT('Ctrl Pts',(43.3664104138306,41.4111054447601,50.1581741203648));
#33593=CARTESIAN_POINT('Ctrl Pts',(43.4346357168277,41.4151438050053,50.1263011731616));
#33594=CARTESIAN_POINT('Ctrl Pts',(43.5010722097884,41.4191821652505,50.0913226507958));
#33595=CARTESIAN_POINT('Ctrl Pts',(43.5707519229727,41.4234176655168,50.0546365871968));
#33596=CARTESIAN_POINT('Ctrl Pts',(43.6387285861544,41.427653165783,50.0143945461722));
#33597=CARTESIAN_POINT('Ctrl Pts',(43.7046156733432,41.4318886660493,49.9707786242415));
#33598=CARTESIAN_POINT('Ctrl Pts',(43.770407245169,41.4361180261845,49.9272259315534));
#33599=CARTESIAN_POINT('Ctrl Pts',(43.8341148684436,41.4403473863198,49.8803093276203));
#33600=CARTESIAN_POINT('Ctrl Pts',(43.8953761517319,41.4445767464551,49.8302569780584));
#33601=CARTESIAN_POINT('Ctrl Pts',(43.9565658945426,41.4488011675746,49.7802630792635));
#33602=CARTESIAN_POINT('Ctrl Pts',(44.015314612821,41.453025588694,49.727141007136));
#33603=CARTESIAN_POINT('Ctrl Pts',(44.0712897647799,41.4572500098135,49.6711615610234));
#33604=CARTESIAN_POINT('Ctrl Pts',(44.127229121687,41.4614717294956,49.6152179127085));
#33605=CARTESIAN_POINT('Ctrl Pts',(44.1803981016048,41.4656934491776,49.5564208480802));
#33606=CARTESIAN_POINT('Ctrl Pts',(44.2304990057065,41.4699151688597,49.4950798744574));
#33607=CARTESIAN_POINT('Ctrl Pts',(44.2805835170155,41.4741355072138,49.433758971328));
#33608=CARTESIAN_POINT('Ctrl Pts',(44.327601649166,41.478355845568,49.3698961752223));
#33609=CARTESIAN_POINT('Ctrl Pts',(44.3712952034314,41.4825761839222,49.3038349825911));
#33610=CARTESIAN_POINT('Ctrl Pts',(44.4149881059399,41.4867964593235,49.2377747753647));
#33611=CARTESIAN_POINT('Ctrl Pts',(44.4553562713294,41.4910167347247,49.1695166290041));
#33612=CARTESIAN_POINT('Ctrl Pts',(44.4921850030362,41.495237010126,49.0994327419039));
#33613=CARTESIAN_POINT('Ctrl Pts',(44.5290505720545,41.4994615067859,49.0292787545897));
#33614=CARTESIAN_POINT('Ctrl Pts',(44.5623694164245,41.5036860034458,48.9572957950096));
#33615=CARTESIAN_POINT('Ctrl Pts',(44.5919732821235,41.5079105001056,48.8838798398859));
#33616=CARTESIAN_POINT('Ctrl Pts',(44.621591360561,41.5121370249353,48.8104286379541));
#33617=CARTESIAN_POINT('Ctrl Pts',(44.6474907536523,41.5163635497649,48.7355435141247));
#33618=CARTESIAN_POINT('Ctrl Pts',(44.6695526663381,41.5205900745946,48.6596371241962));
#33619=CARTESIAN_POINT('Ctrl Pts',(44.6916549074606,41.5248243253699,48.5835919799317));
#33620=CARTESIAN_POINT('Ctrl Pts',(44.7099055425513,41.5290585761453,48.506522297105));
#33621=CARTESIAN_POINT('Ctrl Pts',(44.7242366826522,41.5332928269206,48.4288522868238));
#33622=CARTESIAN_POINT('Ctrl Pts',(44.7379048165262,41.5373311871659,48.3547755496595));
#33623=CARTESIAN_POINT('Ctrl Pts',(44.7480080816397,41.5413695474113,48.2801531618215));
#33624=CARTESIAN_POINT('Ctrl Pts',(44.7545317398734,41.5454079076566,48.2053551236974));
#33625=CARTESIAN_POINT('Ctrl Pts',(44.7613738625438,41.5496434079228,48.1269056810659));
#33626=CARTESIAN_POINT('Ctrl Pts',(44.7643039728385,41.5538789081891,48.047964797762));
#33627=CARTESIAN_POINT('Ctrl Pts',(44.76326611177,41.5581144084553,47.9689560656592));
#33628=CARTESIAN_POINT('Ctrl Pts',(44.7622297552707,41.5623437685906,47.8900618711397));
#33629=CARTESIAN_POINT('Ctrl Pts',(44.757236856571,41.5665731287258,47.8111004884866));
#33630=CARTESIAN_POINT('Ctrl Pts',(44.7482832586759,41.5708024888611,47.7325001347245));
#33631=CARTESIAN_POINT('Ctrl Pts',(44.7393401167268,41.5750269099806,47.6539915698795));
#33632=CARTESIAN_POINT('Ctrl Pts',(44.7264455197113,41.5792513311001,47.5758436600272));
#33633=CARTESIAN_POINT('Ctrl Pts',(44.7096473152042,41.5834757522196,47.4984825822863));
#33634=CARTESIAN_POINT('Ctrl Pts',(44.6928598528313,41.5876974719016,47.4211709754925));
#33635=CARTESIAN_POINT('Ctrl Pts',(44.6721738368805,41.5919191915836,47.3446456595606));
#33636=CARTESIAN_POINT('Ctrl Pts',(44.6476885191618,41.5961409112656,47.2693244483847));
#33637=CARTESIAN_POINT('Ctrl Pts',(44.62321121293,41.6003612496198,47.1940278819736));
#33638=CARTESIAN_POINT('Ctrl Pts',(44.5949372183358,41.6045815879739,47.1199350840304));
#33639=CARTESIAN_POINT('Ctrl Pts',(44.5630157422213,41.6088019263281,47.0474490355876));
#33640=CARTESIAN_POINT('Ctrl Pts',(44.5310947422649,41.6130222017294,46.9749640683861));
#33641=CARTESIAN_POINT('Ctrl Pts',(44.4955265593229,41.6172424771306,46.9040862320499));
#33642=CARTESIAN_POINT('Ctrl Pts',(44.4565080736778,41.6214627525319,46.8351974485785));
#33643=CARTESIAN_POINT('Ctrl Pts',(44.4174505604573,41.6256872491918,46.7662397602752));
#33644=CARTESIAN_POINT('Ctrl Pts',(44.374936082379,41.6299117458516,46.6992755085151));
#33645=CARTESIAN_POINT('Ctrl Pts',(44.3292066429857,41.6341362425114,46.6346604196904));
#33646=CARTESIAN_POINT('Ctrl Pts',(44.2834552490081,41.6383627673411,46.5700143093305));
#33647=CARTESIAN_POINT('Ctrl Pts',(44.234486109346,41.6425892921707,46.5077199781744));
#33648=CARTESIAN_POINT('Ctrl Pts',(44.1825820119918,41.6468158170004,46.4481005794758));
#33649=CARTESIAN_POINT('Ctrl Pts',(44.1305830356877,41.6510500677757,46.3883721985152));
#33650=CARTESIAN_POINT('Ctrl Pts',(44.0756387076146,41.655284318551,46.3313288596858));
#33651=CARTESIAN_POINT('Ctrl Pts',(44.0180690738715,41.6595185693264,46.2772571541056));
#33652=CARTESIAN_POINT('Ctrl Pts',(43.963162802944,41.6635569295717,46.2256869855449));
#33653=CARTESIAN_POINT('Ctrl Pts',(43.9058690608256,41.667595289817,46.1768197792944));
#33654=CARTESIAN_POINT('Ctrl Pts',(43.84649105503,41.6716336500623,46.130868097587));
#33655=CARTESIAN_POINT('Ctrl Pts',(43.7842144021118,41.6758691503286,46.082673199588));
#33656=CARTESIAN_POINT('Ctrl Pts',(43.719408068394,41.6801046505948,46.0375025485721));
#33657=CARTESIAN_POINT('Ctrl Pts',(43.652398033195,41.6843401508611,45.9956323672167));
#33658=CARTESIAN_POINT('Ctrl Pts',(43.5854851412774,41.6885695109963,45.9538228843342));
#33659=CARTESIAN_POINT('Ctrl Pts',(43.5163752865965,41.6927988711316,45.91530461628));
#33660=CARTESIAN_POINT('Ctrl Pts',(43.4454263627895,41.6970282312668,45.8803127209693));
#33661=CARTESIAN_POINT('Ctrl Pts',(43.3745602926158,41.7012526523863,45.8453616889375));
#33662=CARTESIAN_POINT('Ctrl Pts',(43.3018598398523,41.7054770735058,45.8139290528015));
#33663=CARTESIAN_POINT('Ctrl Pts',(43.2277093165479,41.7097014946253,45.7862051296022));
#33664=CARTESIAN_POINT('Ctrl Pts',(43.1536062111015,41.7139232143074,45.7584989353277));
#33665=CARTESIAN_POINT('Ctrl Pts',(43.0780553140324,41.7181449339894,45.7344969106953));
#33666=CARTESIAN_POINT('Ctrl Pts',(43.0014617129366,41.7223666536714,45.7143416159077));
#33667=CARTESIAN_POINT('Ctrl Pts',(42.9248931729259,41.7265869920256,45.6941929158428));
#33668=CARTESIAN_POINT('Ctrl Pts',(42.8472830598909,41.7308073303798,45.6778885657465));
#33669=CARTESIAN_POINT('Ctrl Pts',(42.7690510118218,41.7350276687339,45.6655210877857));
#33670=CARTESIAN_POINT('Ctrl Pts',(42.6908201307046,41.7392479441352,45.6531537943049));
#33671=CARTESIAN_POINT('Ctrl Pts',(42.6119677967967,41.7434682195365,45.6447233281987));
#33672=CARTESIAN_POINT('Ctrl Pts',(42.532921727776,41.7476884949378,45.6402707241751));
#33673=CARTESIAN_POINT('Ctrl Pts',(42.4537965942717,41.7519129915976,45.6358136665102));
#33674=CARTESIAN_POINT('Ctrl Pts',(42.3744778082822,41.7561374882575,45.6353424455197));
#33675=CARTESIAN_POINT('Ctrl Pts',(42.2953954675445,41.7603619849173,45.6388459743825));
#33676=CARTESIAN_POINT('Ctrl Pts',(42.2162751595817,41.764588509747,45.6423511852804));
#33677=CARTESIAN_POINT('Ctrl Pts',(42.1373919909055,41.7688150345766,45.6498349031435));
#33678=CARTESIAN_POINT('Ctrl Pts',(42.0591707283695,41.7730415594063,45.6612341184933));
#33679=CARTESIAN_POINT('Ctrl Pts',(41.9808064799878,41.7772758101816,45.6726541712267));
#33680=CARTESIAN_POINT('Ctrl Pts',(41.9031070171583,41.781510060957,45.6880039324047));
#33681=CARTESIAN_POINT('Ctrl Pts',(41.8264865132704,41.7857443117323,45.707169277631));
#33682=CARTESIAN_POINT('Ctrl Pts',(41.7534107288416,41.7897826719776,45.7254479702158));
#33683=CARTESIAN_POINT('Ctrl Pts',(41.6813166099833,41.7938210322229,45.7471968726855));
#33684=CARTESIAN_POINT('Ctrl Pts',(41.6105469601833,41.7978593924682,45.7722759733701));
#33685=CARTESIAN_POINT('Ctrl Pts',(41.5363225590991,41.8020948927345,45.7985793567174));
#33686=CARTESIAN_POINT('Ctrl Pts',(41.4632730988246,41.8063303930007,45.8286463644956));
#33687=CARTESIAN_POINT('Ctrl Pts',(41.3918072424209,41.810565893267,45.8623522730663));
#33688=CARTESIAN_POINT('Ctrl Pts',(41.3204449888248,41.8147952534022,45.8960093187682));
#33689=CARTESIAN_POINT('Ctrl Pts',(41.250662201115,41.8190246135375,45.9332945910263));
#33690=CARTESIAN_POINT('Ctrl Pts',(41.18285027111,41.8232539736728,45.9740343096777));
#33691=CARTESIAN_POINT('Ctrl Pts',(41.1151175313799,41.8274783947922,46.0147264527842));
#33692=CARTESIAN_POINT('Ctrl Pts',(41.0493514759781,41.8317028159117,46.0588647853688));
#33693=CARTESIAN_POINT('Ctrl Pts',(40.9859200764249,41.8359272370312,46.1062290501115));
#33694=CARTESIAN_POINT('Ctrl Pts',(40.9225292400528,41.8401489567133,46.1535630263021));
#33695=CARTESIAN_POINT('Ctrl Pts',(40.8614704713665,41.8443706763953,46.2041185601328));
#33696=CARTESIAN_POINT('Ctrl Pts',(40.8030828164395,41.8485923960773,46.2576320854225));
#33697=CARTESIAN_POINT('Ctrl Pts',(40.7447142656932,41.8528127344315,46.311128101325));
#33698=CARTESIAN_POINT('Ctrl Pts',(40.6890154390263,41.8570330727856,46.3675798699888));
#33699=CARTESIAN_POINT('Ctrl Pts',(40.636291170759,41.8612534111398,46.4266845177915));
#33700=CARTESIAN_POINT('Ctrl Pts',(40.5835676889556,41.865473686541,46.4857882839569));
#33701=CARTESIAN_POINT('Ctrl Pts',(40.5338189887963,41.8696939619423,46.5475444994656));
#33702=CARTESIAN_POINT('Ctrl Pts',(40.4873109732458,41.8739142373436,46.6116156411736));
#33703=CARTESIAN_POINT('Ctrl Pts',(40.4407564388452,41.8781387340034,46.6757508689494));
#33704=CARTESIAN_POINT('Ctrl Pts',(40.3974493406097,41.8823632306633,46.7422052676186));
#33705=CARTESIAN_POINT('Ctrl Pts',(40.357613033427,41.8865877273231,46.8106111150374));
#33706=CARTESIAN_POINT('Ctrl Pts',(40.3177576009373,41.8908142521528,46.8790498039248));
#33707=CARTESIAN_POINT('Ctrl Pts',(40.2813764948038,41.8950407769824,46.9494413904245));
#33708=CARTESIAN_POINT('Ctrl Pts',(40.2486465175392,41.8992673018121,47.0213945460995));
#33709=CARTESIAN_POINT('Ctrl Pts',(40.2158567109735,41.9035015525874,47.0934792297308));
#33710=CARTESIAN_POINT('Ctrl Pts',(40.1867315428286,41.9077358033627,47.1671307488784));
#33711=CARTESIAN_POINT('Ctrl Pts',(40.161399095563,41.9119700541381,47.2419390317701));
#33712=CARTESIAN_POINT('Ctrl Pts',(40.1372386115997,41.9160084143834,47.3132864345762));
#33713=CARTESIAN_POINT('Ctrl Pts',(40.1165277442649,41.9200467746287,47.3856855830994));
#33714=CARTESIAN_POINT('Ctrl Pts',(40.0993341935841,41.924085134874,47.458772424863));
#33715=CARTESIAN_POINT('Ctrl Pts',(40.0751743144991,41.9297597216444,47.5614719365866));
#33716=CARTESIAN_POINT('Ctrl Pts',(40.0578822519074,41.9354343084147,47.6658441082782));
#33717=CARTESIAN_POINT('Ctrl Pts',(40.047639778813,41.9411088951851,47.7711073817772));
#33718=CARTESIAN_POINT('Ctrl Pts',(40.0403210634903,41.9451636468806,47.8463228034409));
#33719=CARTESIAN_POINT('Ctrl Pts',(40.0366008029736,41.9492183985762,47.9219928813227));
#33720=CARTESIAN_POINT('Ctrl Pts',(40.0365310012709,41.9532731502717,47.9978244664113));
#33721=CARTESIAN_POINT('',(40.0365300138095,42.7470231503245,48.0002554931331));
#33722=CARTESIAN_POINT('Ctrl Pts',(40.0365310012703,41.953273150305,47.9978244670332));
#33723=CARTESIAN_POINT('Ctrl Pts',(40.036459200662,41.957444018785,48.0758276573125));
#33724=CARTESIAN_POINT('Ctrl Pts',(40.040253223248,41.9616148872651,48.1539409988832));
#33725=CARTESIAN_POINT('Ctrl Pts',(40.0479190791829,41.9657857557452,48.2317450815622));
#33726=CARTESIAN_POINT('Ctrl Pts',(40.0555795272878,41.9699536819122,48.3094942778379));
#33727=CARTESIAN_POINT('Ctrl Pts',(40.0671063450249,41.9741216080792,48.3869341692086));
#33728=CARTESIAN_POINT('Ctrl Pts',(40.0824535028735,41.9782895342462,48.4636471444499));
#33729=CARTESIAN_POINT('Ctrl Pts',(40.0977949205481,41.9824559015173,48.5403314273542));
#33730=CARTESIAN_POINT('Ctrl Pts',(40.1169537485858,41.9866222687885,48.6162888607868));
#33731=CARTESIAN_POINT('Ctrl Pts',(40.1398325646431,41.9907886360596,48.6911104145157));
#33732=CARTESIAN_POINT('Ctrl Pts',(40.1627104054812,41.9949548257376,48.7659287789444));
#33733=CARTESIAN_POINT('Ctrl Pts',(40.1893077766097,41.9991210154155,48.8396108987954));
#33734=CARTESIAN_POINT('Ctrl Pts',(40.2194774146584,42.0032872050935,48.9117629602671));
#33735=CARTESIAN_POINT('Ctrl Pts',(40.2496759753692,42.0074573887636,48.9839841916007));
#33736=CARTESIAN_POINT('Ctrl Pts',(40.2834534545533,42.0116275724336,49.0546719894266));
#33737=CARTESIAN_POINT('Ctrl Pts',(40.3206147694229,42.0157977561037,49.1234533829927));
#33738=CARTESIAN_POINT('Ctrl Pts',(40.3577942885969,42.0199699826319,49.1922684706685));
#33739=CARTESIAN_POINT('Ctrl Pts',(40.3983606912674,42.0241422091601,49.2591748830298));
#33740=CARTESIAN_POINT('Ctrl Pts',(40.4420747218958,42.0283144356882,49.3238274231412));
#33741=CARTESIAN_POINT('Ctrl Pts',(40.4858650365847,42.0324939430454,49.3885927864859));
#33742=CARTESIAN_POINT('Ctrl Pts',(40.53281365624,42.0366734504025,49.451096038529));
#33743=CARTESIAN_POINT('Ctrl Pts',(40.5826404409023,42.0408529577597,49.5110243789748));
#33744=CARTESIAN_POINT('Ctrl Pts',(40.6202252309282,42.0440055975998,49.5562288630193));
#33745=CARTESIAN_POINT('Ctrl Pts',(40.6594467906287,42.0471582374399,49.5999689452227));
#33746=CARTESIAN_POINT('Ctrl Pts',(40.7001717981188,42.0503108772799,49.6421250028512));
#33747=CARTESIAN_POINT('Ctrl Pts',(40.7548849238852,42.0545463775462,49.6987607120874));
#33748=CARTESIAN_POINT('Ctrl Pts',(40.8125356685345,42.0587818778124,49.7527666399521));
#33749=CARTESIAN_POINT('Ctrl Pts',(40.8728410815323,42.0630173780787,49.8038226294856));
#33750=CARTESIAN_POINT('Ctrl Pts',(40.9330590708229,42.0672467382139,49.8548046040402));
#33751=CARTESIAN_POINT('Ctrl Pts',(40.9959237309831,42.0714760983492,49.9028448318794));
#33752=CARTESIAN_POINT('Ctrl Pts',(41.0611146327495,42.0757054584845,49.9476592140984));
#33753=CARTESIAN_POINT('Ctrl Pts',(41.1262294050587,42.079929879604,49.9924212624103));
#33754=CARTESIAN_POINT('Ctrl Pts',(41.1936646358799,42.0841543007234,50.0339646865659));
#33755=CARTESIAN_POINT('Ctrl Pts',(41.2630673141337,42.0883787218429,50.0720459716688));
#33756=CARTESIAN_POINT('Ctrl Pts',(41.3324256106866,42.092600441525,50.1101029045097));
#33757=CARTESIAN_POINT('Ctrl Pts',(41.4037484471551,42.096822161207,50.1447018673911));
#33758=CARTESIAN_POINT('Ctrl Pts',(41.4766553964691,42.101043880889,50.1756436252361));
#33759=CARTESIAN_POINT('Ctrl Pts',(41.549538490954,42.1052642192432,50.2065752590757));
#33760=CARTESIAN_POINT('Ctrl Pts',(41.6240042373583,42.1094845575973,50.2338518807473));
#33761=CARTESIAN_POINT('Ctrl Pts',(41.6996506258257,42.1137048959515,50.2573216862011));
#33762=CARTESIAN_POINT('Ctrl Pts',(41.7752958859104,42.1179251713528,50.2807911415664));
#33763=CARTESIAN_POINT('Ctrl Pts',(41.8521213043839,42.122145446754,50.3004537557839));
#33764=CARTESIAN_POINT('Ctrl Pts',(41.9297094842226,42.1263657221553,50.316207519129));
#33765=CARTESIAN_POINT('Ctrl Pts',(42.0073752703162,42.1305902188152,50.3319770399075));
#33766=CARTESIAN_POINT('Ctrl Pts',(42.0858048807772,42.134814715475,50.343829805956));
#33767=CARTESIAN_POINT('Ctrl Pts',(42.164571080988,42.1390392121349,50.3517150475755));
#33768=CARTESIAN_POINT('Ctrl Pts',(42.2433750966456,42.1432657369645,50.3596040748788));
#33769=CARTESIAN_POINT('Ctrl Pts',(42.3225155545501,42.1474922617941,50.3635217599245));
#33770=CARTESIAN_POINT('Ctrl Pts',(42.401563042116,42.1517187866238,50.3634694831538));
#33771=CARTESIAN_POINT('Ctrl Pts',(42.480755025839,42.1559530373991,50.3634171108229));
#33772=CARTESIAN_POINT('Ctrl Pts',(42.5598532296557,42.1601872881745,50.359380299558));
#33773=CARTESIAN_POINT('Ctrl Pts',(42.6384313870402,42.1644215389498,50.3514125360247));
#33774=CARTESIAN_POINT('Ctrl Pts',(42.7133742574011,42.1684598991951,50.3438133877446));
#33775=CARTESIAN_POINT('Ctrl Pts',(42.7878437876093,42.1724982594404,50.3326390509328));
#33776=CARTESIAN_POINT('Ctrl Pts',(42.8614806256514,42.1765366196857,50.3179788767477));
#33777=CARTESIAN_POINT('Ctrl Pts',(42.9387121820721,42.180772119952,50.302603039058));
#33778=CARTESIAN_POINT('Ctrl Pts',(43.015321245365,42.1850076202182,50.2833338920987));
#33779=CARTESIAN_POINT('Ctrl Pts',(43.0908854807103,42.1892431204845,50.2602362030203));
#33780=CARTESIAN_POINT('Ctrl Pts',(43.1663401718995,42.1934724806197,50.2371719982596));
#33781=CARTESIAN_POINT('Ctrl Pts',(43.240752597952,42.197701840755,50.2102904090784));
#33782=CARTESIAN_POINT('Ctrl Pts',(43.3137104742106,42.2019312008903,50.1797072303908));
#33783=CARTESIAN_POINT('Ctrl Pts',(43.386583150796,42.2061556220098,50.1491597665151));
#33784=CARTESIAN_POINT('Ctrl Pts',(43.4580042224367,42.2103800431293,50.1149194836282));
#33785=CARTESIAN_POINT('Ctrl Pts',(43.5275779102807,42.2146044642488,50.077151534469));
#33786=CARTESIAN_POINT('Ctrl Pts',(43.5971071070664,42.2188261839308,50.0394077371995));
#33787=CARTESIAN_POINT('Ctrl Pts',(43.6647908534378,42.2230479036128,49.9981409744052));
#33788=CARTESIAN_POINT('Ctrl Pts',(43.7302557792961,42.2272696232949,49.9535634114483));
#33789=CARTESIAN_POINT('Ctrl Pts',(43.7956992853222,42.231489961649,49.9090004340714));
#33790=CARTESIAN_POINT('Ctrl Pts',(43.8589250247505,42.2357103000032,49.861129071535));
#33791=CARTESIAN_POINT('Ctrl Pts',(43.9195878422038,42.2399306383573,49.8102053007121));
#33792=CARTESIAN_POINT('Ctrl Pts',(43.9802497547774,42.2441509137586,49.759282289496));
#33793=CARTESIAN_POINT('Ctrl Pts',(44.0383484627454,42.2483711891599,49.7053072632901));
#33794=CARTESIAN_POINT('Ctrl Pts',(44.0935723648291,42.2525914645612,49.6485760783134));
#33795=CARTESIAN_POINT('Ctrl Pts',(44.1488515036799,42.256815961221,49.5917881489356));
#33796=CARTESIAN_POINT('Ctrl Pts',(44.2012497643554,42.2610404578809,49.5322388908524));
#33797=CARTESIAN_POINT('Ctrl Pts',(44.2504933178218,42.2652649545407,49.4702601543934));
#33798=CARTESIAN_POINT('Ctrl Pts',(44.2997605129895,42.2694914793704,49.4082516621051));
#33799=CARTESIAN_POINT('Ctrl Pts',(44.345869710249,42.2737180042,49.3438117500821));
#33800=CARTESIAN_POINT('Ctrl Pts',(44.3885897620363,42.2779445290297,49.277302313168));
#33801=CARTESIAN_POINT('Ctrl Pts',(44.4313879046461,42.282178779805,49.210671299233));
#33802=CARTESIAN_POINT('Ctrl Pts',(44.470784288152,42.2864130305804,49.1419636092785));
#33803=CARTESIAN_POINT('Ctrl Pts',(44.5065932897786,42.2906472813557,49.0715666812476));
#33804=CARTESIAN_POINT('Ctrl Pts',(44.5407456478379,42.294685641601,49.0044265493482));
#33805=CARTESIAN_POINT('Ctrl Pts',(44.5716350990051,42.2987240018463,48.9357503632342));
#33806=CARTESIAN_POINT('Ctrl Pts',(44.5991423837312,42.3027623620916,48.8658886862507));
#33807=CARTESIAN_POINT('Ctrl Pts',(44.627992487413,42.3069978623579,48.7926165823545));
#33808=CARTESIAN_POINT('Ctrl Pts',(44.6532314452433,42.3112333626241,48.7177617654702));
#33809=CARTESIAN_POINT('Ctrl Pts',(44.6746852486706,42.3154688628904,48.6417144695116));
#33810=CARTESIAN_POINT('Ctrl Pts',(44.6961079508926,42.3196982230257,48.5657774179938));
#33811=CARTESIAN_POINT('Ctrl Pts',(44.713756269108,42.3239275831609,48.4886517682259));
#33812=CARTESIAN_POINT('Ctrl Pts',(44.7275045475989,42.3281569432962,48.4107469072391));
#33813=CARTESIAN_POINT('Ctrl Pts',(44.7412367709509,42.3323813644157,48.3329330229782));
#33814=CARTESIAN_POINT('Ctrl Pts',(44.7510779239492,42.3366057855352,48.2543421955609));
#33815=CARTESIAN_POINT('Ctrl Pts',(44.7569527916921,42.3408302066547,48.175396632336));
#33816=CARTESIAN_POINT('Ctrl Pts',(44.7628239025682,42.3450519263367,48.0965015533066));
#33817=CARTESIAN_POINT('Ctrl Pts',(44.7647337275928,42.3492736460187,48.0172526555051));
#33818=CARTESIAN_POINT('Ctrl Pts',(44.7626587137445,42.3534953657008,47.938078733319));
#33819=CARTESIAN_POINT('Ctrl Pts',(44.7605843788314,42.3577157040549,47.8589307164877));
#33820=CARTESIAN_POINT('Ctrl Pts',(44.7545278062901,42.3619360424091,47.7798580953953));
#33821=CARTESIAN_POINT('Ctrl Pts',(44.7445175537334,42.3661563807632,47.7012896367116));
#33822=CARTESIAN_POINT('Ctrl Pts',(44.7345074504951,42.3703766561645,47.6227223499979));
#33823=CARTESIAN_POINT('Ctrl Pts',(44.7205438451144,42.3745969315658,47.5446596761631));
#33824=CARTESIAN_POINT('Ctrl Pts',(44.7027069873352,42.378817206967,47.4675237363247));
#33825=CARTESIAN_POINT('Ctrl Pts',(44.6848522885429,42.3830417036269,47.3903106425766));
#33826=CARTESIAN_POINT('Ctrl Pts',(44.6631167042344,42.3872662002867,47.3140265929015));
#33827=CARTESIAN_POINT('Ctrl Pts',(44.6376311906737,42.3914906969466,47.2390814134061));
#33828=CARTESIAN_POINT('Ctrl Pts',(44.6121334415847,42.3957172217762,47.164100252926));
#33829=CARTESIAN_POINT('Ctrl Pts',(44.5828823502661,42.3999437466058,47.0904596799371));
#33830=CARTESIAN_POINT('Ctrl Pts',(44.5500572315736,42.4041702714355,47.0185498780589));
#33831=CARTESIAN_POINT('Ctrl Pts',(44.5171721096646,42.4084045222108,46.9465086274737));
#33832=CARTESIAN_POINT('Ctrl Pts',(44.4807001222147,42.4126387729862,46.8762048877178));
#33833=CARTESIAN_POINT('Ctrl Pts',(44.4408666950662,42.4168730237615,46.8080043733848));
#33834=CARTESIAN_POINT('Ctrl Pts',(44.4028760948004,42.4209113840068,46.7429590417773));
#33835=CARTESIAN_POINT('Ctrl Pts',(44.3618284249697,42.4249497442521,46.679826914187));
#33836=CARTESIAN_POINT('Ctrl Pts',(44.3179540007854,42.4289881044974,46.6188979430284));
#33837=CARTESIAN_POINT('Ctrl Pts',(44.2719377654755,42.4332236047637,46.5549946115054));
#33838=CARTESIAN_POINT('Ctrl Pts',(44.2226368249494,42.4374591050299,46.493272120739));
#33839=CARTESIAN_POINT('Ctrl Pts',(44.1702852397358,42.4416946052962,46.4340879300313));
#33840=CARTESIAN_POINT('Ctrl Pts',(44.1180095477037,42.4459239654315,46.3749895376144));
#33841=CARTESIAN_POINT('Ctrl Pts',(44.0626923015589,42.4501533255667,46.3184224865432));
#33842=CARTESIAN_POINT('Ctrl Pts',(44.0046098286107,42.454382685702,46.2647139317029));
#33843=CARTESIAN_POINT('Ctrl Pts',(43.9465951839488,42.4586071068215,46.2110680973194));
#33844=CARTESIAN_POINT('Ctrl Pts',(43.8858220723409,42.462831527941,46.1602744426767));
#33845=CARTESIAN_POINT('Ctrl Pts',(43.8226048913956,42.4670559490605,46.1126246362005));
#33846=CARTESIAN_POINT('Ctrl Pts',(43.7594281366426,42.4712776687425,46.0650053008749));
#33847=CARTESIAN_POINT('Ctrl Pts',(43.6938107884397,42.4754993884245,46.0205261051851));
#33848=CARTESIAN_POINT('Ctrl Pts',(43.6261007329175,42.4797211081066,45.9794388319976));
#33849=CARTESIAN_POINT('Ctrl Pts',(43.5584128318239,42.4839414464607,45.938365002383));
#33850=CARTESIAN_POINT('Ctrl Pts',(43.4886339839979,42.4881617848149,45.9006811348342));
#33851=CARTESIAN_POINT('Ctrl Pts',(43.4171402436681,42.492382123169,45.8665951707164));
#33852=CARTESIAN_POINT('Ctrl Pts',(43.3456475697777,42.4966023985703,45.8325097150432));
#33853=CARTESIAN_POINT('Ctrl Pts',(43.2724404784693,42.5008226739716,45.8020222569056));
#33854=CARTESIAN_POINT('Ctrl Pts',(43.1979173998788,42.5050429493729,45.7752936679484));
#33855=CARTESIAN_POINT('Ctrl Pts',(43.123319780849,42.5092674460328,45.7485383441756));
#33856=CARTESIAN_POINT('Ctrl Pts',(43.0474039879245,42.5134919426926,45.7255495589812));
#33857=CARTESIAN_POINT('Ctrl Pts',(42.9705855425879,42.5177164393525,45.7064388869076));
#33858=CARTESIAN_POINT('Ctrl Pts',(42.8937302169165,42.5219429641821,45.6873190398503));
#33859=CARTESIAN_POINT('Ctrl Pts',(42.8159718367486,42.5261694890118,45.6720811053743));
#33860=CARTESIAN_POINT('Ctrl Pts',(42.7377355652697,42.5303960138414,45.6607853606708));
#33861=CARTESIAN_POINT('Ctrl Pts',(42.6593562805094,42.5346302646167,45.6494689677247));
#33862=CARTESIAN_POINT('Ctrl Pts',(42.5804978273916,42.5388645153921,45.6421092079402));
#33863=CARTESIAN_POINT('Ctrl Pts',(42.5015897356161,42.5430987661674,45.6387143403397));
#33864=CARTESIAN_POINT('Ctrl Pts',(42.4263321947273,42.5471371264127,45.6354765306106));
#33865=CARTESIAN_POINT('Ctrl Pts',(42.3510298634973,42.551175486658,45.6358448292773));
#33866=CARTESIAN_POINT('Ctrl Pts',(42.2760511986137,42.5552138469033,45.6397823965713));
#33867=CARTESIAN_POINT('Ctrl Pts',(42.1974123115932,42.5594493471696,45.6439121834919));
#33868=CARTESIAN_POINT('Ctrl Pts',(42.1188305752909,42.5636848474358,45.6519843159781));
#33869=CARTESIAN_POINT('Ctrl Pts',(42.0407332477664,42.5679203477021,45.6639953249962));
#33870=CARTESIAN_POINT('Ctrl Pts',(41.9627491365777,42.5721497078373,45.6759889218637));
#33871=CARTESIAN_POINT('Ctrl Pts',(41.8852484996176,42.5763790679726,45.69190998523));
#33872=CARTESIAN_POINT('Ctrl Pts',(41.8086559740489,42.5806084281079,45.7117031040811));
#33873=CARTESIAN_POINT('Ctrl Pts',(41.7321528926706,42.5848328492274,45.731473108673));
#33874=CARTESIAN_POINT('Ctrl Pts',(41.6565562673637,42.5890572703469,45.7551060663524));
#33875=CARTESIAN_POINT('Ctrl Pts',(41.582281485891,42.5932816914663,45.7824953500425));
#33876=CARTESIAN_POINT('Ctrl Pts',(41.508054201737,42.5975034111484,45.8098671188033));
#33877=CARTESIAN_POINT('Ctrl Pts',(41.4351475228643,42.6017251308304,45.8409902839723));
#33878=CARTESIAN_POINT('Ctrl Pts',(41.3639614091661,42.6059468505124,45.8757084759377));
#33879=CARTESIAN_POINT('Ctrl Pts',(41.2927985872474,42.6101671888666,45.9104153082652));
#33880=CARTESIAN_POINT('Ctrl Pts',(41.2233556341836,42.6143875272207,45.9487146261067));
#33881=CARTESIAN_POINT('Ctrl Pts',(41.156010876636,42.6186078655749,45.9904026518101));
#33882=CARTESIAN_POINT('Ctrl Pts',(41.0886671236395,42.6228281409762,46.0320900556722));
#33883=CARTESIAN_POINT('Ctrl Pts',(41.0234219023212,42.6270484163774,46.0771658187454));
#33884=CARTESIAN_POINT('Ctrl Pts',(40.9606260575622,42.6312686917787,46.1253818802937));
#33885=CARTESIAN_POINT('Ctrl Pts',(40.8977674023296,42.6354931884386,46.173646169136));
#33886=CARTESIAN_POINT('Ctrl Pts',(40.8373633908965,42.6397176850984,46.225056744535));
#33887=CARTESIAN_POINT('Ctrl Pts',(40.7797326541702,42.6439421817583,46.2793245021395));
#33888=CARTESIAN_POINT('Ctrl Pts',(40.7220742490777,42.6481687065879,46.3336183135525));
#33889=CARTESIAN_POINT('Ctrl Pts',(40.6671920966208,42.6523952314176,46.3907717008113));
#33890=CARTESIAN_POINT('Ctrl Pts',(40.6153669012738,42.6566217562472,46.4504596991911));
#33891=CARTESIAN_POINT('Ctrl Pts',(40.5634469712073,42.6608560070225,46.5102568052308));
#33892=CARTESIAN_POINT('Ctrl Pts',(40.5145954546749,42.6650902577979,46.5725974101743));
#33893=CARTESIAN_POINT('Ctrl Pts',(40.4690516696586,42.6693245085732,46.6371247355493));
#33894=CARTESIAN_POINT('Ctrl Pts',(40.4256148916807,42.6733628688185,46.6986668121424));
#33895=CARTESIAN_POINT('Ctrl Pts',(40.3851867208811,42.6774012290638,46.7621974326211));
#33896=CARTESIAN_POINT('Ctrl Pts',(40.3479355059124,42.6814395893091,46.8273867845684));
#33897=CARTESIAN_POINT('Ctrl Pts',(40.3071963122816,42.6858560772042,46.8986800734954));
#33898=CARTESIAN_POINT('Ctrl Pts',(40.270113103662,42.6902725650992,46.9722089595395));
#33899=CARTESIAN_POINT('Ctrl Pts',(40.2369265036252,42.6946890529942,47.0475801922571));
#33900=CARTESIAN_POINT('Ctrl Pts',(40.2038270381793,42.6990939449781,47.1227535305983));
#33901=CARTESIAN_POINT('Ctrl Pts',(40.1746039716191,42.703498836962,47.19975920718));
#33902=CARTESIAN_POINT('Ctrl Pts',(40.1494521309674,42.7079037289459,47.2781795721282));
#33903=CARTESIAN_POINT('Ctrl Pts',(40.1243392761471,42.7123017932634,47.3564783840195));
#33904=CARTESIAN_POINT('Ctrl Pts',(40.1032852240893,42.7166998575809,47.4361871338538));
#33905=CARTESIAN_POINT('Ctrl Pts',(40.0864369623797,42.7210979218985,47.5168680181803));
#33906=CARTESIAN_POINT('Ctrl Pts',(40.0696202029547,42.7254877628707,47.597398048239));
#33907=CARTESIAN_POINT('Ctrl Pts',(40.0569936581839,42.7298776038429,47.6788961913138));
#33908=CARTESIAN_POINT('Ctrl Pts',(40.048654264041,42.7342674448151,47.7609107470266));
#33909=CARTESIAN_POINT('Ctrl Pts',(40.040576913324,42.738519346634,47.8403482120316));
#33910=CARTESIAN_POINT('Ctrl Pts',(40.0365213673141,42.7427712484528,47.9202697353209));
#33911=CARTESIAN_POINT('Ctrl Pts',(40.0365300138094,42.7470231502717,48.0002554921404));
#33912=CARTESIAN_POINT('',(40.0365309117291,43.5407731502446,48.0020759787561));
#33913=CARTESIAN_POINT('Ctrl Pts',(40.0365300138095,42.7470231503245,48.0002554931331));
#33914=CARTESIAN_POINT('Ctrl Pts',(40.0365390801091,42.751481472945,48.0841243885452));
#33915=CARTESIAN_POINT('Ctrl Pts',(40.0410166138422,42.7559397955656,48.1678918268366));
#33916=CARTESIAN_POINT('Ctrl Pts',(40.0499047771218,42.7603981181862,48.2510834210075));
#33917=CARTESIAN_POINT('Ctrl Pts',(40.0588211874745,42.7648706096019,48.3345394026533));
#33918=CARTESIAN_POINT('Ctrl Pts',(40.0721762090108,42.7693431010177,48.4174154972645));
#33919=CARTESIAN_POINT('Ctrl Pts',(40.0898604967801,42.7738155924335,48.4992453470619));
#33920=CARTESIAN_POINT('Ctrl Pts',(40.1075743816014,42.7782955691697,48.5812121502019));
#33921=CARTESIAN_POINT('Ctrl Pts',(40.1296318840185,42.7827755459059,48.6621288448638));
#33922=CARTESIAN_POINT('Ctrl Pts',(40.1558739613116,42.7872555226421,48.7415448492038));
#33923=CARTESIAN_POINT('Ctrl Pts',(40.1821907867162,42.7917482601746,48.821187062631));
#33924=CARTESIAN_POINT('Ctrl Pts',(40.2127158766436,42.7962409977071,48.8993196805187));
#33925=CARTESIAN_POINT('Ctrl Pts',(40.2472419462328,42.8007337352395,48.9755117645834));
#33926=CARTESIAN_POINT('Ctrl Pts',(40.264998067866,42.803044267398,49.0146959499898));
#33927=CARTESIAN_POINT('Ctrl Pts',(40.2838116483987,42.8053547995565,49.0533673052659));
#33928=CARTESIAN_POINT('Ctrl Pts',(40.3036499480538,42.807665331715,49.0914700639985));
#33929=CARTESIAN_POINT('Ctrl Pts',(40.3400160826526,42.8119008319812,49.1613172825985));
#33930=CARTESIAN_POINT('Ctrl Pts',(40.3799459672787,42.8161363322475,49.2294777764117));
#33931=CARTESIAN_POINT('Ctrl Pts',(40.4232592798914,42.8203718325137,49.2955641884386));
#33932=CARTESIAN_POINT('Ctrl Pts',(40.466509801949,42.824601192649,49.3615547961446));
#33933=CARTESIAN_POINT('Ctrl Pts',(40.5131337566303,42.8288305527842,49.4254769037269));
#33934=CARTESIAN_POINT('Ctrl Pts',(40.5629046426042,42.8330599129195,49.4869670772195));
#33935=CARTESIAN_POINT('Ctrl Pts',(40.6126174065022,42.837284334039,49.5483854429382));
#33936=CARTESIAN_POINT('Ctrl Pts',(40.6654695051001,42.8415087551585,49.6073771552396));
#33937=CARTESIAN_POINT('Ctrl Pts',(40.7211916668968,42.8457331762779,49.6636084339782));
#33938=CARTESIAN_POINT('Ctrl Pts',(40.7768781954243,42.84995489596,49.7198037538769));
#33939=CARTESIAN_POINT('Ctrl Pts',(40.8354308148945,42.854176615642,49.77324181136));
#33940=CARTESIAN_POINT('Ctrl Pts',(40.8965413864561,42.858398335324,49.8236234913657));
#33941=CARTESIAN_POINT('Ctrl Pts',(40.9576319629109,42.8626186736782,49.8739886867101));
#33942=CARTESIAN_POINT('Ctrl Pts',(41.0212784676792,42.8668390120323,49.9212991919717));
#33943=CARTESIAN_POINT('Ctrl Pts',(41.0871385919924,42.8710593503865,49.9652952359034));
#33944=CARTESIAN_POINT('Ctrl Pts',(41.1529977339001,42.8752796257877,50.009290623566));
#33945=CARTESIAN_POINT('Ctrl Pts',(41.2210700386964,42.879499901189,50.0499713885688));
#33946=CARTESIAN_POINT('Ctrl Pts',(41.2909842964744,42.8837201765903,50.0871211297463));
#33947=CARTESIAN_POINT('Ctrl Pts',(41.3609684847975,42.8879446732501,50.1243080293194));
#33948=CARTESIAN_POINT('Ctrl Pts',(41.4327978910302,42.89216916991,50.1579566289978));
#33949=CARTESIAN_POINT('Ctrl Pts',(41.5060773142077,42.8963936665698,50.1878968606234));
#33950=CARTESIAN_POINT('Ctrl Pts',(41.5793919186447,42.9006201913995,50.217851466476));
#33951=CARTESIAN_POINT('Ctrl Pts',(41.6541574833693,42.9048467162291,50.2440940018879));
#33952=CARTESIAN_POINT('Ctrl Pts',(41.7299619017027,42.9090732410587,50.2665037806565));
#33953=CARTESIAN_POINT('Ctrl Pts',(41.8059048879714,42.9133074918341,50.2889545237493));
#33954=CARTESIAN_POINT('Ctrl Pts',(41.8828900650561,42.9175417426094,50.3075583997282));
#33955=CARTESIAN_POINT('Ctrl Pts',(41.9604935376409,42.9217759933847,50.322245574965));
#33956=CARTESIAN_POINT('Ctrl Pts',(42.0345068153651,42.9258143536301,50.3362532726051));
#33957=CARTESIAN_POINT('Ctrl Pts',(42.109082086108,42.9298527138755,50.346698641262));
#33958=CARTESIAN_POINT('Ctrl Pts',(42.1838494209599,42.9338910741208,50.3535652461915));
#33959=CARTESIAN_POINT('Ctrl Pts',(42.2622666614811,42.9381265743871,50.3607670571347));
#33960=CARTESIAN_POINT('Ctrl Pts',(42.3411932775508,42.9423620746533,50.3640591505288));
#33961=CARTESIAN_POINT('Ctrl Pts',(42.4202059383712,42.9465975749196,50.3633836254308));
#33962=CARTESIAN_POINT('Ctrl Pts',(42.4991040559129,42.9508269350548,50.3627090796298));
#33963=CARTESIAN_POINT('Ctrl Pts',(42.5780875051341,42.9550562951901,50.3580783413496));
#33964=CARTESIAN_POINT('Ctrl Pts',(42.6567280925766,42.9592856553253,50.3494852898842));
#33965=CARTESIAN_POINT('Ctrl Pts',(42.7352768441173,42.9635100764448,50.3409022733213));
#33966=CARTESIAN_POINT('Ctrl Pts',(42.8134830653811,42.9677344975643,50.3283661893197));
#33967=CARTESIAN_POINT('Ctrl Pts',(42.8909203643071,42.9719589186838,50.3119229305512));
#33968=CARTESIAN_POINT('Ctrl Pts',(42.9683081435441,42.9761806383658,50.295490186936));
#33969=CARTESIAN_POINT('Ctrl Pts',(43.0449275185103,42.9804023580479,50.2751553248965));
#33970=CARTESIAN_POINT('Ctrl Pts',(43.1203602245478,42.9846240777299,50.2510156791523));
#33971=CARTESIAN_POINT('Ctrl Pts',(43.1957682493397,42.988844416084,50.2268839317927));
#33972=CARTESIAN_POINT('Ctrl Pts',(43.2699899295026,42.9930647544382,50.1989500156484));
#33973=CARTESIAN_POINT('Ctrl Pts',(43.3426216039958,42.9972850927923,50.1673612879676));
#33974=CARTESIAN_POINT('Ctrl Pts',(43.4152521950753,43.0015053681936,50.1357730314814));
#33975=CARTESIAN_POINT('Ctrl Pts',(43.4862923977552,43.0057256435949,50.1005302602413));
#33976=CARTESIAN_POINT('Ctrl Pts',(43.5553593911814,43.0099459189962,50.0618281010087));
#33977=CARTESIAN_POINT('Ctrl Pts',(43.6244954676909,43.014170415656,50.0230872306007));
#33978=CARTESIAN_POINT('Ctrl Pts',(43.6916539818663,43.0183949123159,49.9808802900125));
#33979=CARTESIAN_POINT('Ctrl Pts',(43.756478101255,43.0226194089757,49.9354476489215));
#33980=CARTESIAN_POINT('Ctrl Pts',(43.821333342534,43.0268459338054,49.8899931957382));
#33981=CARTESIAN_POINT('Ctrl Pts',(43.8838515855544,43.031072458635,49.8413102457139));
#33982=CARTESIAN_POINT('Ctrl Pts',(43.9437083836268,43.0352989834646,49.7896801019234));
#33983=CARTESIAN_POINT('Ctrl Pts',(44.0036745979194,43.03953323424,49.7379555799608));
#33984=CARTESIAN_POINT('Ctrl Pts',(44.0609693053627,43.0437674850153,49.6832734239026));
#33985=CARTESIAN_POINT('Ctrl Pts',(44.1153044501575,43.0480017357906,49.625952362208));
#33986=CARTESIAN_POINT('Ctrl Pts',(44.1671258703585,43.052040096036,49.5712831635585));
#33987=CARTESIAN_POINT('Ctrl Pts',(44.2162553053429,43.0560784562813,49.5142141233452));
#33988=CARTESIAN_POINT('Ctrl Pts',(44.2624788046377,43.0601168165267,49.4550474711072));
#33989=CARTESIAN_POINT('Ctrl Pts',(44.3109587895019,43.064352316793,49.3929924893615));
#33990=CARTESIAN_POINT('Ctrl Pts',(44.3564261600119,43.0685878170593,49.3283939845637));
#33991=CARTESIAN_POINT('Ctrl Pts',(44.398603201491,43.0728233173255,49.2615766658789));
#33992=CARTESIAN_POINT('Ctrl Pts',(44.4407190996474,43.0770526774608,49.1948562110975));
#33993=CARTESIAN_POINT('Ctrl Pts',(44.4795538926046,43.0812820375961,49.1259237235177));
#33994=CARTESIAN_POINT('Ctrl Pts',(44.5148707836607,43.0855113977314,49.0551360146058));
#33995=CARTESIAN_POINT('Ctrl Pts',(44.5501464319103,43.0897358188509,48.9844309710616));
#33996=CARTESIAN_POINT('Ctrl Pts',(44.5819121335306,43.0939602399704,48.9118754292533));
#33997=CARTESIAN_POINT('Ctrl Pts',(44.6099758110708,43.0981846610899,48.8378528244162));
#33998=CARTESIAN_POINT('Ctrl Pts',(44.6380215424196,43.102406380772,48.7638775556357));
#33999=CARTESIAN_POINT('Ctrl Pts',(44.6623697824841,43.106628100454,48.6884375235558));
#34000=CARTESIAN_POINT('Ctrl Pts',(44.6828761148751,43.1108498201361,48.611937157748));
#34001=CARTESIAN_POINT('Ctrl Pts',(44.7033757376855,43.1150701584902,48.5354618225191));
#34002=CARTESIAN_POINT('Ctrl Pts',(44.7200358274869,43.1192904968444,48.4579272954668));
#34003=CARTESIAN_POINT('Ctrl Pts',(44.7327619386732,43.1235108351986,48.3797527858724));
#34004=CARTESIAN_POINT('Ctrl Pts',(44.7454878600298,43.1277311105999,48.3015794423715));
#34005=CARTESIAN_POINT('Ctrl Pts',(44.7542798453204,43.1319513860012,48.2227665987723));
#34006=CARTESIAN_POINT('Ctrl Pts',(44.7590948988036,43.1361716614025,48.1437417800744));
#34007=CARTESIAN_POINT('Ctrl Pts',(44.763914768462,43.1403961580624,48.0646379181482));
#34008=CARTESIAN_POINT('Ctrl Pts',(44.7647497314263,43.1446206547222,47.9853221271795));
#34009=CARTESIAN_POINT('Ctrl Pts',(44.7616089020215,43.1488451513821,47.9062245512258));
#34010=CARTESIAN_POINT('Ctrl Pts',(44.7584665647128,43.1530716762118,47.8270890007326));
#34011=CARTESIAN_POINT('Ctrl Pts',(44.7513446747799,43.1572982010414,47.7481723420521));
#34012=CARTESIAN_POINT('Ctrl Pts',(44.7403042931064,43.1615247258711,47.6698996265256));
#34013=CARTESIAN_POINT('Ctrl Pts',(44.7292437299852,43.1657589766465,47.5914838310992));
#34014=CARTESIAN_POINT('Ctrl Pts',(44.7142504511103,43.1699932274218,47.5137147930387));
#34015=CARTESIAN_POINT('Ctrl Pts',(44.6954366803258,43.1742274781972,47.43700720474));
#34016=CARTESIAN_POINT('Ctrl Pts',(44.6774932971803,43.1782658384423,47.3638483647189));
#34017=CARTESIAN_POINT('Ctrl Pts',(44.6560752388336,43.1823041986874,47.2916552659579));
#34018=CARTESIAN_POINT('Ctrl Pts',(44.6313209434258,43.1863425589325,47.2207713504179));
#34019=CARTESIAN_POINT('Ctrl Pts',(44.6053582213241,43.1905780591987,47.1464271054972));
#34020=CARTESIAN_POINT('Ctrl Pts',(44.5756265262222,43.194813559465,47.0732405294778));
#34021=CARTESIAN_POINT('Ctrl Pts',(44.5422487063644,43.1990490597312,47.0016208530922));
#34022=CARTESIAN_POINT('Ctrl Pts',(44.5089192737509,43.2032784198664,46.9301050025045));
#34023=CARTESIAN_POINT('Ctrl Pts',(44.471954409482,43.2075077800017,46.8601519625604));
#34024=CARTESIAN_POINT('Ctrl Pts',(44.4315260970149,43.2117371401369,46.7921539178988));
#34025=CARTESIAN_POINT('Ctrl Pts',(44.3911449964349,43.2159615612564,46.7242352808553));
#34026=CARTESIAN_POINT('Ctrl Pts',(44.3473087236237,43.2201859823759,46.6582675036271));
#34027=CARTESIAN_POINT('Ctrl Pts',(44.3002358461097,43.2244104034953,46.5946195639402));
#34028=CARTESIAN_POINT('Ctrl Pts',(44.2531930708112,43.2286321231773,46.5310123259077));
#34029=CARTESIAN_POINT('Ctrl Pts',(44.2029180771509,43.2328538428593,46.4697223573419));
#34030=CARTESIAN_POINT('Ctrl Pts',(44.1496728737119,43.2370755625414,46.4110899094358));
#34031=CARTESIAN_POINT('Ctrl Pts',(44.0964450918662,43.2412959008955,46.3524766458054));
#34032=CARTESIAN_POINT('Ctrl Pts',(44.0402493452888,43.2455162392496,46.2965195234357));
#34033=CARTESIAN_POINT('Ctrl Pts',(43.9813871064818,43.2497365776038,46.2435247623855));
#34034=CARTESIAN_POINT('Ctrl Pts',(43.9225257456961,43.253956853005,46.190530791834));
#34035=CARTESIAN_POINT('Ctrl Pts',(43.8609983214482,43.2581771284063,46.1404994078151));
#34036=CARTESIAN_POINT('Ctrl Pts',(43.7971411339319,43.2623974038076,46.0936980583403));
#34037=CARTESIAN_POINT('Ctrl Pts',(43.7332200743519,43.2666219004674,46.0468498966131));
#34038=CARTESIAN_POINT('Ctrl Pts',(43.6669649758922,43.2708463971272,46.0032385014496));
#34039=CARTESIAN_POINT('Ctrl Pts',(43.59874253255,43.275070893787,45.9630889117206));
#34040=CARTESIAN_POINT('Ctrl Pts',(43.5304873357912,43.2792974186167,45.9229200462786));
#34041=CARTESIAN_POINT('Ctrl Pts',(43.4602633290897,43.2835239434463,45.886216514893));
#34042=CARTESIAN_POINT('Ctrl Pts',(43.3884610259716,43.2877504682759,45.8531569128054));
#34043=CARTESIAN_POINT('Ctrl Pts',(43.3165274706505,43.2919847190512,45.8200368788735));
#34044=CARTESIAN_POINT('Ctrl Pts',(43.2430102906739,43.2962189698265,45.7905742594983));
#34045=CARTESIAN_POINT('Ctrl Pts',(43.1683189661304,43.3004532206019,45.7648990163341));
#34046=CARTESIAN_POINT('Ctrl Pts',(43.0970831107861,43.3044915808474,45.7404115953498));
#34047=CARTESIAN_POINT('Ctrl Pts',(43.0247797012346,43.3085299410929,45.7193689315346));
#34048=CARTESIAN_POINT('Ctrl Pts',(42.9517724756598,43.3125683013385,45.7018403937054));
#34049=CARTESIAN_POINT('Ctrl Pts',(42.8752012674076,43.3168038016047,45.6834561678988));
#34050=CARTESIAN_POINT('Ctrl Pts',(42.7975647088768,43.3210393018709,45.6688680431903));
#34051=CARTESIAN_POINT('Ctrl Pts',(42.7192734344537,43.3252748021371,45.6581940911015));
#34052=CARTESIAN_POINT('Ctrl Pts',(42.641095657528,43.3295041622723,45.6475356128552));
#34053=CARTESIAN_POINT('Ctrl Pts',(42.5622655106308,43.3337335224075,45.6407801019222));
#34054=CARTESIAN_POINT('Ctrl Pts',(42.4832058736375,43.3379628825428,45.6379950839399));
#34055=CARTESIAN_POINT('Ctrl Pts',(42.4042385619087,43.3421873036622,45.6352133182812));
#34056=CARTESIAN_POINT('Ctrl Pts',(42.3250427592673,43.3464117247817,45.636392848));
#34057=CARTESIAN_POINT('Ctrl Pts',(42.2460470295097,43.3506361459011,45.6415494654801));
#34058=CARTESIAN_POINT('Ctrl Pts',(42.167101816028,43.3548578655831,45.6467027854008));
#34059=CARTESIAN_POINT('Ctrl Pts',(42.0883568885804,43.3590795852651,45.6558281147404));
#34060=CARTESIAN_POINT('Ctrl Pts',(42.010240152383,43.3633013049471,45.6688891699266));
#34061=CARTESIAN_POINT('Ctrl Pts',(41.9321489756339,43.3675216433012,45.6819459515936));
#34062=CARTESIAN_POINT('Ctrl Pts',(41.8546860445732,43.3717419816554,45.6989358247166));
#34063=CARTESIAN_POINT('Ctrl Pts',(41.7782719929229,43.3759623200095,45.7197709049054));
#34064=CARTESIAN_POINT('Ctrl Pts',(41.7018590811062,43.3801825954107,45.7406056743068));
#34065=CARTESIAN_POINT('Ctrl Pts',(41.62649547007,43.384402870812,45.7652854120072));
#34066=CARTESIAN_POINT('Ctrl Pts',(41.5525880266408,43.3886231462132,45.7936719672027));
#34067=CARTESIAN_POINT('Ctrl Pts',(41.4786066585505,43.392847642873,45.8220869155663));
#34068=CARTESIAN_POINT('Ctrl Pts',(41.4060848068154,43.3970721395328,45.8542159192995));
#34069=CARTESIAN_POINT('Ctrl Pts',(41.3354101137736,43.4012966361926,45.8898723225728));
#34070=CARTESIAN_POINT('Ctrl Pts',(41.2647014899964,43.4055231610223,45.9255458443921));
#34071=CARTESIAN_POINT('Ctrl Pts',(41.1958421999975,43.4097496858519,45.9647499068625));
#34072=CARTESIAN_POINT('Ctrl Pts',(41.1291937118813,43.4139762106815,46.0072526956541));
#34073=CARTESIAN_POINT('Ctrl Pts',(41.0624233925633,43.4182104614568,46.0498331781186));
#34074=CARTESIAN_POINT('Ctrl Pts',(40.9978723340775,43.4224447122321,46.095724163513));
#34075=CARTESIAN_POINT('Ctrl Pts',(40.9358713630654,43.4266789630074,46.144651575739));
#34076=CARTESIAN_POINT('Ctrl Pts',(40.8767387632706,43.430717323253,46.1913154430772));
#34077=CARTESIAN_POINT('Ctrl Pts',(40.819925763197,43.4347556834987,46.2407407377773));
#34078=CARTESIAN_POINT('Ctrl Pts',(40.7656874832283,43.4387940437443,46.2926590737573));
#34079=CARTESIAN_POINT('Ctrl Pts',(40.7086184111207,43.4430431731818,46.34728711988));
#34080=CARTESIAN_POINT('Ctrl Pts',(40.6541653394365,43.4472923026193,46.40490063856));
#34081=CARTESIAN_POINT('Ctrl Pts',(40.6026626588428,43.4515414320569,46.4652137207474));
#34082=CARTESIAN_POINT('Ctrl Pts',(40.5521635800498,43.4557077612614,46.5243515181305));
#34083=CARTESIAN_POINT('Ctrl Pts',(40.5045013028056,43.4598740904658,46.5860842540786));
#34084=CARTESIAN_POINT('Ctrl Pts',(40.4599566629003,43.4640404196703,46.6501028590759));
#34085=CARTESIAN_POINT('Ctrl Pts',(40.4154544564735,43.4682027800058,46.7140604795843));
#34086=CARTESIAN_POINT('Ctrl Pts',(40.3740642728014,43.4723651403413,46.7802992556056));
#34087=CARTESIAN_POINT('Ctrl Pts',(40.3360268850936,43.4765275006768,46.8484769121534));
#34088=CARTESIAN_POINT('Ctrl Pts',(40.298013037963,43.4806872850109,46.9166123749156));
#34089=CARTESIAN_POINT('Ctrl Pts',(40.2633481050394,43.484847069345,46.9866839154094));
#34090=CARTESIAN_POINT('Ctrl Pts',(40.2322287563103,43.489006853679,47.0583215644755));
#34091=CARTESIAN_POINT('Ctrl Pts',(40.1999567820551,43.4933207117262,47.1326125911449));
#34092=CARTESIAN_POINT('Ctrl Pts',(40.1714984602697,43.4976345697733,47.2085875394332));
#34093=CARTESIAN_POINT('Ctrl Pts',(40.1470194300474,43.5019484278204,47.2858088544962));
#34094=CARTESIAN_POINT('Ctrl Pts',(40.123410782464,43.5061089012311,47.360284468795));
#34095=CARTESIAN_POINT('Ctrl Pts',(40.1035033133508,43.5102693746418,47.4359188077746));
#34096=CARTESIAN_POINT('Ctrl Pts',(40.0873947493397,43.5144298480525,47.5123039927183));
#34097=CARTESIAN_POINT('Ctrl Pts',(40.0712812845998,43.5185915872093,47.588712416424));
#34098=CARTESIAN_POINT('Ctrl Pts',(40.0589691050863,43.5227533263661,47.6658716630413));
#34099=CARTESIAN_POINT('Ctrl Pts',(40.0505044774577,43.5269150655229,47.7433655704048));
#34100=CARTESIAN_POINT('Ctrl Pts',(40.0420309912486,43.5310811601107,47.8209405783258));
#34101=CARTESIAN_POINT('Ctrl Pts',(40.0374131159821,43.5352472546985,47.8988504628412));
#34102=CARTESIAN_POINT('Ctrl Pts',(40.0366450790482,43.5394133492862,47.9766770818087));
#34103=CARTESIAN_POINT('Ctrl Pts',(40.0365615173866,43.5398666162724,47.9851445412663));
#34104=CARTESIAN_POINT('Ctrl Pts',(40.0365234764394,43.5403198832585,47.9936110186486));
#34105=CARTESIAN_POINT('Ctrl Pts',(40.0365309117291,43.5407731502446,48.0020759787561));
#34106=CARTESIAN_POINT('',(40.0365303613413,44.3345231503005,47.9986930805401));
#34107=CARTESIAN_POINT('Ctrl Pts',(40.0365309117295,43.5407731502717,48.0020759792626));
#34108=CARTESIAN_POINT('Ctrl Pts',(40.0366326946382,43.546977995395,48.1179541880231));
#34109=CARTESIAN_POINT('Ctrl Pts',(40.0452598640996,43.5531828405182,48.233471756771));
#34110=CARTESIAN_POINT('Ctrl Pts',(40.0622349480595,43.5593876856415,48.3476276784514));
#34111=CARTESIAN_POINT('Ctrl Pts',(40.0673710085148,43.5612650524777,48.3821672257353));
#34112=CARTESIAN_POINT('Ctrl Pts',(40.0732709855902,43.5631424193139,48.4165823443543));
#34113=CARTESIAN_POINT('Ctrl Pts',(40.0799291996866,43.5650197861502,48.4508457856444));
#34114=CARTESIAN_POINT('Ctrl Pts',(40.0949507005634,43.5692552864162,48.5281470417959));
#34115=CARTESIAN_POINT('Ctrl Pts',(40.1138683244528,43.5734907866822,48.6048436656388));
#34116=CARTESIAN_POINT('Ctrl Pts',(40.1366192416652,43.5777262869483,48.6805130297796));
#34117=CARTESIAN_POINT('Ctrl Pts',(40.159337177269,43.5819556470833,48.7560726973607));
#34118=CARTESIAN_POINT('Ctrl Pts',(40.1858772368616,43.5861850072183,48.8306076168557));
#34119=CARTESIAN_POINT('Ctrl Pts',(40.2161255174371,43.5904143673534,48.9037049769203));
#34120=CARTESIAN_POINT('Ctrl Pts',(40.2463384742922,43.5946387884726,48.9767169744236));
#34121=CARTESIAN_POINT('Ctrl Pts',(40.2802508682226,43.5988632095919,49.0482943170942));
#34122=CARTESIAN_POINT('Ctrl Pts',(40.3176993632225,43.6030876307111,49.1180404728702));
#34123=CARTESIAN_POINT('Ctrl Pts',(40.3551239106177,43.6073093503929,49.187742027298));
#34124=CARTESIAN_POINT('Ctrl Pts',(40.3960798495183,43.6115310700747,49.2556143066362));
#34125=CARTESIAN_POINT('Ctrl Pts',(40.4403567290258,43.6157527897565,49.3212829717458));
#34126=CARTESIAN_POINT('Ctrl Pts',(40.4846191213355,43.6199731281105,49.3869301503607));
#34127=CARTESIAN_POINT('Ctrl Pts',(40.5322000344415,43.6241934664644,49.4503747575766));
#34128=CARTESIAN_POINT('Ctrl Pts',(40.5828450770055,43.6284138048183,49.5112704677644));
#34129=CARTESIAN_POINT('Ctrl Pts',(40.6334893641205,43.6326340802194,49.5721652695987));
#34130=CARTESIAN_POINT('Ctrl Pts',(40.6871973886971,43.6368543556204,49.630510889974));
#34131=CARTESIAN_POINT('Ctrl Pts',(40.7436747265954,43.6410746310215,49.685994374125));
#34132=CARTESIAN_POINT('Ctrl Pts',(40.8002085549886,43.6452991276811,49.7415333546857));
#34133=CARTESIAN_POINT('Ctrl Pts',(40.8595168944304,43.6495236243407,49.7942041505038));
#34134=CARTESIAN_POINT('Ctrl Pts',(40.9212691538297,43.6537481210003,49.843731413597));
#34135=CARTESIAN_POINT('Ctrl Pts',(40.9830510603273,43.6579746458298,49.8932824545998));
#34136=CARTESIAN_POINT('Ctrl Pts',(41.0472788432116,43.6622011706592,49.9396866811162));
#34137=CARTESIAN_POINT('Ctrl Pts',(41.1135916714608,43.6664276954886,49.9827112884041));
#34138=CARTESIAN_POINT('Ctrl Pts',(41.1800257173371,43.6706619462637,50.0258145432318));
#34139=CARTESIAN_POINT('Ctrl Pts',(41.2485520174761,43.6748961970388,50.0655255981262));
#34140=CARTESIAN_POINT('Ctrl Pts',(41.3187839892539,43.679130447814,50.1016570555174));
#34141=CARTESIAN_POINT('Ctrl Pts',(41.3857667963626,43.6831688080613,50.1361169514841));
#34142=CARTESIAN_POINT('Ctrl Pts',(41.4543006048555,43.6872071683086,50.1673210190355));
#34143=CARTESIAN_POINT('Ctrl Pts',(41.5240354019836,43.691245528556,50.1951483922328));
#34144=CARTESIAN_POINT('Ctrl Pts',(41.5971744321095,43.695481028822,50.2243342100801));
#34145=CARTESIAN_POINT('Ctrl Pts',(41.6719127188849,43.6997165290881,50.2499161781902));
#34146=CARTESIAN_POINT('Ctrl Pts',(41.7478608304828,43.7039520293542,50.2717185002727));
#34147=CARTESIAN_POINT('Ctrl Pts',(41.8236988414257,43.7081813894892,50.2934892159086));
#34148=CARTESIAN_POINT('Ctrl Pts',(41.9007427470158,43.7124107496243,50.3114910380031));
#34149=CARTESIAN_POINT('Ctrl Pts',(41.9785837407698,43.7166401097594,50.3255964347574));
#34150=CARTESIAN_POINT('Ctrl Pts',(42.0563338323817,43.7208645308787,50.3396853593327));
#34151=CARTESIAN_POINT('Ctrl Pts',(42.1348787029864,43.725088951998,50.3498868174432));
#34152=CARTESIAN_POINT('Ctrl Pts',(42.2137964946016,43.7293133731173,50.3561236587831));
#34153=CARTESIAN_POINT('Ctrl Pts',(42.2926638197806,43.7335350927991,50.3623565117808));
#34154=CARTESIAN_POINT('Ctrl Pts',(42.3719031260178,43.7377568124809,50.364629743154));
#34155=CARTESIAN_POINT('Ctrl Pts',(42.4510857314457,43.7419785321628,50.3629178337265));
#34156=CARTESIAN_POINT('Ctrl Pts',(42.5302424286777,43.7461988705167,50.3612064844281));
#34157=CARTESIAN_POINT('Ctrl Pts',(42.6093419930523,43.7504192088707,50.3555125936196));
#34158=CARTESIAN_POINT('Ctrl Pts',(42.6879555314468,43.7546395472246,50.3458627523385));
#34159=CARTESIAN_POINT('Ctrl Pts',(42.7665678971988,43.7588598226257,50.3362130549997));
#34160=CARTESIAN_POINT('Ctrl Pts',(42.8446937856893,43.7630800980268,50.3226075829935));
#34161=CARTESIAN_POINT('Ctrl Pts',(42.9219107122232,43.7673003734279,50.3051246494206));
#34162=CARTESIAN_POINT('Ctrl Pts',(42.9992048736722,43.7715248700875,50.2876242288414));
#34163=CARTESIAN_POINT('Ctrl Pts',(43.0755877981171,43.7757493667472,50.2662387030641));
#34164=CARTESIAN_POINT('Ctrl Pts',(43.1506490632099,43.7799738634068,50.2410971475601));
#34165=CARTESIAN_POINT('Ctrl Pts',(43.2257463650198,43.7842003882363,50.2159435216611));
#34166=CARTESIAN_POINT('Ctrl Pts',(43.2995203058357,43.7884269130657,50.1870304452184));
#34167=CARTESIAN_POINT('Ctrl Pts',(43.3715798838236,43.7926534378952,50.1545354418643));
#34168=CARTESIAN_POINT('Ctrl Pts',(43.4437711843042,43.7968876886703,50.1219810387335));
#34169=CARTESIAN_POINT('Ctrl Pts',(43.5142414411835,43.8011219394454,50.0858318397518));
#34170=CARTESIAN_POINT('Ctrl Pts',(43.5826239099361,43.8053561902206,50.0463115912655));
#34171=CARTESIAN_POINT('Ctrl Pts',(43.6478427781782,43.8093945504677,50.0086196809566));
#34172=CARTESIAN_POINT('Ctrl Pts',(43.7111624818923,43.8134329107148,49.9678619594898));
#34173=CARTESIAN_POINT('Ctrl Pts',(43.7722920155135,43.8174712709618,49.9242674099662));
#34174=CARTESIAN_POINT('Ctrl Pts',(43.836405700318,43.8217067712294,49.8785447119219));
#34175=CARTESIAN_POINT('Ctrl Pts',(43.8983536305805,43.825942271497,49.8295273421116));
#34176=CARTESIAN_POINT('Ctrl Pts',(43.9577772773827,43.8301777717645,49.7774477193353));
#34177=CARTESIAN_POINT('Ctrl Pts',(44.0171147787588,43.8344071319011,49.7254435954812));
#34178=CARTESIAN_POINT('Ctrl Pts',(44.073934913626,43.8386364920377,49.6703863410523));
#34179=CARTESIAN_POINT('Ctrl Pts',(44.1279092633336,43.8428658521743,49.6125507801573));
#34180=CARTESIAN_POINT('Ctrl Pts',(44.1818205821912,43.8470902732951,49.5547827592063));
#34181=CARTESIAN_POINT('Ctrl Pts',(44.232892401313,43.8513146944159,49.4942432205423));
#34182=CARTESIAN_POINT('Ctrl Pts',(44.2808316135483,43.8555391155367,49.4312452209098));
#34183=CARTESIAN_POINT('Ctrl Pts',(44.3287401695636,43.85976083522,49.3682875073074));
#34184=CARTESIAN_POINT('Ctrl Pts',(44.3735198112441,43.8639825549034,49.3028748255943));
#34185=CARTESIAN_POINT('Ctrl Pts',(44.4149171630047,43.8682042745867,49.2353539035958));
#34186=CARTESIAN_POINT('Ctrl Pts',(44.456300969736,43.8724246129422,49.1678550741423));
#34187=CARTESIAN_POINT('Ctrl Pts',(44.4943044388895,43.8766449512977,49.098249773962));
#34188=CARTESIAN_POINT('Ctrl Pts',(44.5287179067445,43.8808652896531,49.026913099734));
#34189=CARTESIAN_POINT('Ctrl Pts',(44.5631308612694,43.8850855650557,48.9555774896029));
#34190=CARTESIAN_POINT('Ctrl Pts',(44.5939537182137,43.8893058404583,48.8825109800734));
#34191=CARTESIAN_POINT('Ctrl Pts',(44.6210237804686,43.8935261158609,48.8081112593529));
#34192=CARTESIAN_POINT('Ctrl Pts',(44.6481209190919,43.897750612522,48.7336371215798));
#34193=CARTESIAN_POINT('Ctrl Pts',(44.6714576037361,43.9019751091832,48.6578275508552));
#34194=CARTESIAN_POINT('Ctrl Pts',(44.6909203554978,43.9061996058443,48.5810975526244));
#34195=CARTESIAN_POINT('Ctrl Pts',(44.7103924512756,43.9104261306752,48.5043307165222));
#34196=CARTESIAN_POINT('Ctrl Pts',(44.7259868165942,43.9146526555062,48.4266430334096));
#34197=CARTESIAN_POINT('Ctrl Pts',(44.7376412251462,43.9188791803371,48.3484593855776));
#34198=CARTESIAN_POINT('Ctrl Pts',(44.7493169375662,43.9231134311137,48.270132820659));
#34199=CARTESIAN_POINT('Ctrl Pts',(44.7570382558388,43.9273476818903,48.191308947752));
#34200=CARTESIAN_POINT('Ctrl Pts',(44.7607949512539,43.9315819326669,48.1124172541651));
#34201=CARTESIAN_POINT('Ctrl Pts',(44.7643778494276,43.9356202929005,48.0371753530702));
#34202=CARTESIAN_POINT('Ctrl Pts',(44.7643548825488,43.9396586531341,47.9618721249029));
#34203=CARTESIAN_POINT('Ctrl Pts',(44.7607612002978,43.9436970133677,47.886876191416));
#34204=CARTESIAN_POINT('Ctrl Pts',(44.7569920857951,43.9479325136319,47.8082191926045));
#34205=CARTESIAN_POINT('Ctrl Pts',(44.7492804050985,43.9521680138961,47.7296012647612));
#34206=CARTESIAN_POINT('Ctrl Pts',(44.737627667848,43.9564035141602,47.6514496773612));
#34207=CARTESIAN_POINT('Ctrl Pts',(44.7259918233678,43.9606328742934,47.5734113849567));
#34208=CARTESIAN_POINT('Ctrl Pts',(44.7104263365325,43.9648622344266,47.4958385507813));
#34209=CARTESIAN_POINT('Ctrl Pts',(44.6909846704357,43.9690915945598,47.4191560616409));
#34210=CARTESIAN_POINT('Ctrl Pts',(44.6715657081741,43.9733160156772,47.3425631217491));
#34211=CARTESIAN_POINT('Ctrl Pts',(44.6482796765435,43.9775404367947,47.2668589133324));
#34212=CARTESIAN_POINT('Ctrl Pts',(44.6212312965784,43.9817648579121,47.1924593087648));
#34213=CARTESIAN_POINT('Ctrl Pts',(44.594200213541,43.9859865775921,47.1181072813378));
#34214=CARTESIAN_POINT('Ctrl Pts',(44.5634117173996,43.9902082972721,47.0450586418268));
#34215=CARTESIAN_POINT('Ctrl Pts',(44.529020341951,43.9944300169521,46.9737140630122));
#34216=CARTESIAN_POINT('Ctrl Pts',(44.4946402192072,43.9986503553042,46.9023928278259));
#34217=CARTESIAN_POINT('Ctrl Pts',(44.4566597616052,44.0028706936563,46.8327749686778));
#34218=CARTESIAN_POINT('Ctrl Pts',(44.4152810096909,44.0070910320084,46.765239742752));
#34219=CARTESIAN_POINT('Ctrl Pts',(44.3739028750046,44.0113113074077,46.6977055242182));
#34220=CARTESIAN_POINT('Ctrl Pts',(44.3291267931115,44.015531582807,46.632254276664));
#34221=CARTESIAN_POINT('Ctrl Pts',(44.2811992132045,44.0197518582062,46.5692379788592));
#34222=CARTESIAN_POINT('Ctrl Pts',(44.2332236945518,44.0239763548641,46.5061586500757));
#34223=CARTESIAN_POINT('Ctrl Pts',(44.1820906657114,44.028200851522,46.4455195107658));
#34224=CARTESIAN_POINT('Ctrl Pts',(44.1280877667894,44.0324253481799,46.3876405142857));
#34225=CARTESIAN_POINT('Ctrl Pts',(44.0740589412166,44.0366518730075,46.3297337302505));
#34226=CARTESIAN_POINT('Ctrl Pts',(44.0171578382906,44.0408783978352,46.2745900559656));
#34227=CARTESIAN_POINT('Ctrl Pts',(43.95770813204,44.0451049226629,46.2224916832047));
#34228=CARTESIAN_POINT('Ctrl Pts',(43.8981497537186,44.0493391734364,46.1702980763643));
#34229=CARTESIAN_POINT('Ctrl Pts',(43.8360338318456,44.0535734242098,46.1211611865935));
#34230=CARTESIAN_POINT('Ctrl Pts',(43.771716043656,44.0578076749833,46.0753219655027));
#34231=CARTESIAN_POINT('Ctrl Pts',(43.7103738100583,44.0618460352467,46.0316034190904));
#34232=CARTESIAN_POINT('Ctrl Pts',(43.6470292563365,44.0658843955101,45.9908843290108));
#34233=CARTESIAN_POINT('Ctrl Pts',(43.5820114194165,44.0699227557735,45.9533345546307));
#34234=CARTESIAN_POINT('Ctrl Pts',(43.5138196169086,44.0741582560391,45.9139517187806));
#34235=CARTESIAN_POINT('Ctrl Pts',(43.443527779424,44.0783937563046,45.8779058288163));
#34236=CARTESIAN_POINT('Ctrl Pts',(43.3714960692856,44.0826292565701,45.8454267642378));
#34237=CARTESIAN_POINT('Ctrl Pts',(43.2995687822636,44.0868586167047,45.812994783994));
#34238=CARTESIAN_POINT('Ctrl Pts',(43.2259070556054,44.0910879768392,45.7841195522038));
#34239=CARTESIAN_POINT('Ctrl Pts',(43.1508971541187,44.0953173369737,45.7589859650514));
#34240=CARTESIAN_POINT('Ctrl Pts',(43.0759748486458,44.0995417580924,45.7338817287181));
#34241=CARTESIAN_POINT('Ctrl Pts',(42.9997079396694,44.1037661792111,45.7125106024248));
#34242=CARTESIAN_POINT('Ctrl Pts',(42.9225028407167,44.1079906003299,45.6950094962575));
#34243=CARTESIAN_POINT('Ctrl Pts',(42.8453471129659,44.1122123200111,45.6775195817169));
#34244=CARTESIAN_POINT('Ctrl Pts',(42.7672548425226,44.1164340396924,45.6638948788254));
#34245=CARTESIAN_POINT('Ctrl Pts',(42.6886466079096,44.1206557593736,45.6542221808871));
#34246=CARTESIAN_POINT('Ctrl Pts',(42.6100640935613,44.1248760977269,45.6445526478124));
#34247=CARTESIAN_POINT('Ctrl Pts',(42.5309664157519,44.1290964360803,45.6388326093437));
#34248=CARTESIAN_POINT('Ctrl Pts',(42.4517818426335,44.1333167744336,45.6370973186199));
#34249=CARTESIAN_POINT('Ctrl Pts',(42.3725984506758,44.1375370498341,45.6353620537806));
#34250=CARTESIAN_POINT('Ctrl Pts',(42.2933286352536,44.1417573252345,45.6376114274847));
#34251=CARTESIAN_POINT('Ctrl Pts',(42.2144017473073,44.145977600635,45.6438285865631));
#34252=CARTESIAN_POINT('Ctrl Pts',(42.1353959140864,44.150202097294,45.6500519642489));
#34253=CARTESIAN_POINT('Ctrl Pts',(42.0567341625618,44.154426593953,45.6602510183619));
#34254=CARTESIAN_POINT('Ctrl Pts',(41.9788411933351,44.158651090612,45.6743569275427));
#34255=CARTESIAN_POINT('Ctrl Pts',(41.9009108278979,44.1628776154408,45.6884696089336));
#34256=CARTESIAN_POINT('Ctrl Pts',(41.8237504377088,44.1671041402696,45.7064927750539));
#34257=CARTESIAN_POINT('Ctrl Pts',(41.7477724588646,44.1713306650983,45.7283068703092));
#34258=CARTESIAN_POINT('Ctrl Pts',(41.6716555948225,44.1755649158728,45.7501608409993));
#34259=CARTESIAN_POINT('Ctrl Pts',(41.5967259063327,44.1797991666473,45.7758194355191));
#34260=CARTESIAN_POINT('Ctrl Pts',(41.5233784588197,44.1840334174217,45.8051138721021));
#34261=CARTESIAN_POINT('Ctrl Pts',(41.4534243081469,44.1880717776743,45.8330530506295));
#34262=CARTESIAN_POINT('Ctrl Pts',(41.3849095462803,44.1921101379269,45.8642989169101));
#34263=CARTESIAN_POINT('Ctrl Pts',(41.3181550358887,44.1961484981794,45.898666634128));
#34264=CARTESIAN_POINT('Ctrl Pts',(41.2481417806304,44.2003839984554,45.9347120750144));
#34265=CARTESIAN_POINT('Ctrl Pts',(41.1797988894822,44.2046194987314,45.9743289635968));
#34266=CARTESIAN_POINT('Ctrl Pts',(41.1135145423081,44.2088549990074,46.017338756104));
#34267=CARTESIAN_POINT('Ctrl Pts',(41.0473262863973,44.2130843591525,46.0602861980643));
#34268=CARTESIAN_POINT('Ctrl Pts',(40.9831910386942,44.2173137192975,46.1066165230949));
#34269=CARTESIAN_POINT('Ctrl Pts',(40.9214732680534,44.2215430794425,46.1561048989112));
#34270=CARTESIAN_POINT('Ctrl Pts',(40.8598275709725,44.2257675005718,46.2055354825652));
#34271=CARTESIAN_POINT('Ctrl Pts',(40.8005941051742,44.2299919217011,46.2581164962757));
#34272=CARTESIAN_POINT('Ctrl Pts',(40.7441078821434,44.2342163428303,46.3135802020492));
#34273=CARTESIAN_POINT('Ctrl Pts',(40.6876577809846,44.2384380625221,46.3690084398312));
#34274=CARTESIAN_POINT('Ctrl Pts',(40.6339517696957,44.242659782214,46.4273153829194));
#34275=CARTESIAN_POINT('Ctrl Pts',(40.5832903732837,44.2468815019058,46.4881942674086));
#34276=CARTESIAN_POINT('Ctrl Pts',(40.532645553055,44.2511018402697,46.5490532325979));
#34277=CARTESIAN_POINT('Ctrl Pts',(40.4850436696072,44.2553221786336,46.6124821076934));
#34278=CARTESIAN_POINT('Ctrl Pts',(40.4407460612456,44.2595425169975,46.6781397788059));
#34279=CARTESIAN_POINT('Ctrl Pts',(40.3964491136516,44.2637627924085,46.7437964705323));
#34280=CARTESIAN_POINT('Ctrl Pts',(40.3554566045661,44.2679830678196,46.8116815023639));
#34281=CARTESIAN_POINT('Ctrl Pts',(40.3179866352061,44.2722033432306,46.8814246606869));
#34282=CARTESIAN_POINT('Ctrl Pts',(40.2804791871488,44.2764278399,46.9512375784136));
#34283=CARTESIAN_POINT('Ctrl Pts',(40.2465015398371,44.2806523365695,47.0229119208925));
#34284=CARTESIAN_POINT('Ctrl Pts',(40.2162255719881,44.284876833239,47.0960532712261));
#34285=CARTESIAN_POINT('Ctrl Pts',(40.1859350687264,44.2891033580782,47.1692297365297));
#34286=CARTESIAN_POINT('Ctrl Pts',(40.1593499429503,44.2933298829174,47.2438741699996));
#34287=CARTESIAN_POINT('Ctrl Pts',(40.1365927694682,44.2975564077566,47.319575022742));
#34288=CARTESIAN_POINT('Ctrl Pts',(40.1137939966372,44.3017906585413,47.3954142541016));
#34289=CARTESIAN_POINT('Ctrl Pts',(40.0948372711182,44.3060249093261,47.4723133066147));
#34290=CARTESIAN_POINT('Ctrl Pts',(40.0797943697413,44.3102591601108,47.5498486096703));
#34291=CARTESIAN_POINT('Ctrl Pts',(40.0654474033776,44.3142975202689,47.6237968698538));
#34292=CARTESIAN_POINT('Ctrl Pts',(40.0546601511491,44.3183358804271,47.6983234535545));
#34293=CARTESIAN_POINT('Ctrl Pts',(40.0474507440786,44.3223742405853,47.7730585111452));
#34294=CARTESIAN_POINT('Ctrl Pts',(40.0402212060184,44.3264238771474,47.84800225312));
#34295=CARTESIAN_POINT('Ctrl Pts',(40.0365720529249,44.3304735137096,47.9232968877507));
#34296=CARTESIAN_POINT('Ctrl Pts',(40.0365303613416,44.3345231502717,47.9986930800047));
#34297=CARTESIAN_POINT('',(40.0365304116029,45.1282731502432,47.9986051444044));
#34298=CARTESIAN_POINT('Ctrl Pts',(40.0365303613413,44.3345231503005,47.9986930805401));
#34299=CARTESIAN_POINT('Ctrl Pts',(40.0364873138526,44.3387044920006,48.0765413609645));
#34300=CARTESIAN_POINT('Ctrl Pts',(40.0402947576141,44.3428858337008,48.1545451941626));
#34301=CARTESIAN_POINT('Ctrl Pts',(40.047972454677,44.347067175401,48.2322861746675));
#34302=CARTESIAN_POINT('Ctrl Pts',(40.0557404770259,44.3512977090506,48.3109417492561));
#34303=CARTESIAN_POINT('Ctrl Pts',(40.0674704954214,44.3555282427002,48.3893277508716));
#34304=CARTESIAN_POINT('Ctrl Pts',(40.0831286024023,44.3597587763497,48.4670089591152));
#34305=CARTESIAN_POINT('Ctrl Pts',(40.0985691505288,44.3639305295825,48.5436108392703));
#34306=CARTESIAN_POINT('Ctrl Pts',(40.1178292293051,44.3681022828153,48.6195268984098));
#34307=CARTESIAN_POINT('Ctrl Pts',(40.140824253703,44.3722740360481,48.6943452946794));
#34308=CARTESIAN_POINT('Ctrl Pts',(40.1638081619622,44.376443772593,48.7691275226171));
#34309=CARTESIAN_POINT('Ctrl Pts',(40.1905232926915,44.3806135091379,48.842812680392));
#34310=CARTESIAN_POINT('Ctrl Pts',(40.2208346617081,44.3847832456828,48.9150021143622));
#34311=CARTESIAN_POINT('Ctrl Pts',(40.2511413964841,44.3889523447255,48.9871805114433));
#34312=CARTESIAN_POINT('Ctrl Pts',(40.2850430906621,44.3931214437682,49.0578631947279));
#34313=CARTESIAN_POINT('Ctrl Pts',(40.3223564941723,44.397290542811,49.1266711603622));
#34314=CARTESIAN_POINT('Ctrl Pts',(40.3606247512086,44.4015663294926,49.197239928347));
#34315=CARTESIAN_POINT('Ctrl Pts',(40.4024815024921,44.4058421161743,49.2658362304326));
#34316=CARTESIAN_POINT('Ctrl Pts',(40.4476797591311,44.410117902856,49.3320796214918));
#34317=CARTESIAN_POINT('Ctrl Pts',(40.4918069478713,44.4142923657655,49.3967532358614));
#34318=CARTESIAN_POINT('Ctrl Pts',(40.5391186654831,44.418466828675,49.4591838745681));
#34319=CARTESIAN_POINT('Ctrl Pts',(40.5893433779465,44.4226412915845,49.5190500445719));
#34320=CARTESIAN_POINT('Ctrl Pts',(40.6413966935497,44.4269677401523,49.5810958480881));
#34321=CARTESIAN_POINT('Ctrl Pts',(40.6965788149973,44.43129418872,49.6403864316954));
#34322=CARTESIAN_POINT('Ctrl Pts',(40.7545465108049,44.4356206372878,49.6966063938921));
#34323=CARTESIAN_POINT('Ctrl Pts',(40.8125142066124,44.4399470858555,49.7528263560887));
#34324=CARTESIAN_POINT('Ctrl Pts',(40.8732669979703,44.4442735344233,49.8059753825312));
#34325=CARTESIAN_POINT('Ctrl Pts',(40.936426713427,44.448599982991,49.8557865382985));
#34326=CARTESIAN_POINT('Ctrl Pts',(40.9982587189332,44.4528354832578,49.9045505904384));
#34327=CARTESIAN_POINT('Ctrl Pts',(41.0626480362529,44.4570709835245,49.950313724215));
#34328=CARTESIAN_POINT('Ctrl Pts',(41.1292712332043,44.4613064837913,49.9927967387915));
#34329=CARTESIAN_POINT('Ctrl Pts',(41.1957978476641,44.4655358439268,50.0352181664795));
#34330=CARTESIAN_POINT('Ctrl Pts',(41.2645515184387,44.4697652040624,50.0743686676054));
#34331=CARTESIAN_POINT('Ctrl Pts',(41.3351765237371,44.473994564198,50.1100098116595));
#34332=CARTESIAN_POINT('Ctrl Pts',(41.4057190536672,44.4782189853175,50.1456093342444));
#34333=CARTESIAN_POINT('Ctrl Pts',(41.4781281586208,44.482443406437,50.1777074332868));
#34334=CARTESIAN_POINT('Ctrl Pts',(41.5520212882403,44.4866678275565,50.2061102749641));
#34335=CARTESIAN_POINT('Ctrl Pts',(41.6258671645971,44.4908895472384,50.23449495356));
#34336=CARTESIAN_POINT('Ctrl Pts',(41.7011947451277,44.4951112669203,50.2591888969931));
#34337=CARTESIAN_POINT('Ctrl Pts',(41.777600266791,44.4993329866022,50.2800458357238));
#34338=CARTESIAN_POINT('Ctrl Pts',(41.8539807889048,44.503553324956,50.3008959501562));
#34339=CARTESIAN_POINT('Ctrl Pts',(41.9314380993689,44.5077736633099,50.3179114292895));
#34340=CARTESIAN_POINT('Ctrl Pts',(42.0095534264271,44.5119940016637,50.3309959060636));
#34341=CARTESIAN_POINT('Ctrl Pts',(42.0876675882715,44.5162142770645,50.344080187662));
#34342=CARTESIAN_POINT('Ctrl Pts',(42.1664392840762,44.5204345524653,50.3532335072376));
#34343=CARTESIAN_POINT('Ctrl Pts',(42.2454411905109,44.5246548278662,50.3584109089193));
#34344=CARTESIAN_POINT('Ctrl Pts',(42.3245221172514,44.5288793245253,50.3635934892084));
#34345=CARTESIAN_POINT('Ctrl Pts',(42.403833245138,44.5331038211844,50.36479217659));
#34346=CARTESIAN_POINT('Ctrl Pts',(42.4829443928394,44.5373283178435,50.3620141127005));
#34347=CARTESIAN_POINT('Ctrl Pts',(42.5620935215933,44.5415548426723,50.35923471507));
#34348=CARTESIAN_POINT('Ctrl Pts',(42.6410420106153,44.545781367501,50.3524748028493));
#34349=CARTESIAN_POINT('Ctrl Pts',(42.7193645330155,44.5500078923298,50.3417934870419));
#34350=CARTESIAN_POINT('Ctrl Pts',(42.7978302263567,44.5542421431041,50.3310926461478));
#34351=CARTESIAN_POINT('Ctrl Pts',(42.8756672041234,44.5584763938783,50.3164561648982));
#34352=CARTESIAN_POINT('Ctrl Pts',(42.9524602636344,44.5627106446525,50.2979943642239));
#34353=CARTESIAN_POINT('Ctrl Pts',(43.0257006207594,44.5667490049007,50.2803866678624));
#34354=CARTESIAN_POINT('Ctrl Pts',(43.0979911812455,44.5707873651488,50.2592999040496));
#34355=CARTESIAN_POINT('Ctrl Pts',(43.1689878718805,44.574825725397,50.2348709344839));
#34356=CARTESIAN_POINT('Ctrl Pts',(43.2434503984069,44.5790612257338,50.2092494191986));
#34357=CARTESIAN_POINT('Ctrl Pts',(43.3167725522144,44.5832967260707,50.1798536614904));
#34358=CARTESIAN_POINT('Ctrl Pts',(43.3885445434963,44.5875322264075,50.1468046316383));
#34359=CARTESIAN_POINT('Ctrl Pts',(43.4602124881788,44.5917615866137,50.1138035123863));
#34360=CARTESIAN_POINT('Ctrl Pts',(43.5303343102457,44.5959909468198,50.0771598327297));
#34361=CARTESIAN_POINT('Ctrl Pts',(43.5985170404772,44.600220307026,50.0370437758148));
#34362=CARTESIAN_POINT('Ctrl Pts',(43.666620147419,44.6044447282165,49.9969745661354));
#34363=CARTESIAN_POINT('Ctrl Pts',(43.7327882599967,44.608669149407,49.9534412740424));
#34364=CARTESIAN_POINT('Ctrl Pts',(43.796651402031,44.6128935705975,49.9066607726874));
#34365=CARTESIAN_POINT('Ctrl Pts',(43.8604737047943,44.6171152903506,49.8599101865778));
#34366=CARTESIAN_POINT('Ctrl Pts',(43.9219935849465,44.6213370101036,49.8099167892779));
#34367=CARTESIAN_POINT('Ctrl Pts',(43.9808695933246,44.6255587298567,49.7569410262731));
#34368=CARTESIAN_POINT('Ctrl Pts',(44.0397263377345,44.6297790682818,49.7039825967025));
#34369=CARTESIAN_POINT('Ctrl Pts',(44.0959405794593,44.6339994067069,49.6480440527762));
#34370=CARTESIAN_POINT('Ctrl Pts',(44.1492047191353,44.6382197451321,49.5894254595465));
#34371=CARTESIAN_POINT('Ctrl Pts',(44.2024680642923,44.6424400206042,49.5308077407061));
#34372=CARTESIAN_POINT('Ctrl Pts',(44.2527810802238,44.6466602960763,49.4695104002925));
#34373=CARTESIAN_POINT('Ctrl Pts',(44.2998747794902,44.6508805715483,49.4058685084875));
#34374=CARTESIAN_POINT('Ctrl Pts',(44.3470155834178,44.6551050682783,49.3421629599771));
#34375=CARTESIAN_POINT('Ctrl Pts',(44.3909303583399,44.6593295650082,49.2761085536373));
#34376=CARTESIAN_POINT('Ctrl Pts',(44.4313923861292,44.6635540617381,49.2080709476171));
#34377=CARTESIAN_POINT('Ctrl Pts',(44.471873839629,44.6677805866375,49.1400006769254));
#34378=CARTESIAN_POINT('Ctrl Pts',(44.5088990241303,44.6720071115369,49.0699457253269));
#34379=CARTESIAN_POINT('Ctrl Pts',(44.5422875554129,44.6762336364363,48.998295783234));
#34380=CARTESIAN_POINT('Ctrl Pts',(44.5757371197999,44.6804678872801,48.9265148674738));
#34381=CARTESIAN_POINT('Ctrl Pts',(44.6055365702878,44.6847021381238,48.8531335711954));
#34382=CARTESIAN_POINT('Ctrl Pts',(44.631554068754,44.6889363889676,48.7785607742029));
#34383=CARTESIAN_POINT('Ctrl Pts',(44.6563679068757,44.6929747485793,48.7074379752427));
#34384=CARTESIAN_POINT('Ctrl Pts',(44.6777419208073,44.6970131081911,48.635231836396));
#34385=CARTESIAN_POINT('Ctrl Pts',(44.6956050744272,44.7010514678028,48.5623057737249));
#34386=CARTESIAN_POINT('Ctrl Pts',(44.7143402531728,44.7052869679152,48.4858196812667));
#34387=CARTESIAN_POINT('Ctrl Pts',(44.7292842565899,44.7095224680277,48.4082508412591));
#34388=CARTESIAN_POINT('Ctrl Pts',(44.7403171312684,44.7137579681401,48.3300093422795));
#34389=CARTESIAN_POINT('Ctrl Pts',(44.7513340117802,44.7179873281217,48.251881268641));
#34390=CARTESIAN_POINT('Ctrl Pts',(44.7584509579835,44.7222166881032,48.1730829333129));
#34391=CARTESIAN_POINT('Ctrl Pts',(44.7615985056644,44.7264460480847,48.0940369020325));
#34392=CARTESIAN_POINT('Ctrl Pts',(44.7647423776626,44.7306704690514,48.0150831801147));
#34393=CARTESIAN_POINT('Ctrl Pts',(44.7639260440308,44.7348948900181,47.9358828035966));
#34394=CARTESIAN_POINT('Ctrl Pts',(44.7591317471986,44.7391193109847,47.8568642593213));
#34395=CARTESIAN_POINT('Ctrl Pts',(44.7543405162281,44.7433410305145,47.7778962459021));
#34396=CARTESIAN_POINT('Ctrl Pts',(44.7455763993675,44.7475627500444,47.6991103011625));
#34397=CARTESIAN_POINT('Ctrl Pts',(44.7328737174753,44.7517844695742,47.6209344921877));
#34398=CARTESIAN_POINT('Ctrl Pts',(44.7201751918418,44.7560048077769,47.5427842619756));
#34399=CARTESIAN_POINT('Ctrl Pts',(44.7035407352886,44.7602251459796,47.4652442340471));
#34400=CARTESIAN_POINT('Ctrl Pts',(44.6830563022954,44.7644454841824,47.3887354407056));
#34401=CARTESIAN_POINT('Ctrl Pts',(44.6625721748543,44.7686657594332,47.3122277885927));
#34402=CARTESIAN_POINT('Ctrl Pts',(44.6382383078035,44.7728860346841,47.2367517935278));
#34403=CARTESIAN_POINT('Ctrl Pts',(44.6101909846418,44.777106309935,47.1627149515796));
#34404=CARTESIAN_POINT('Ctrl Pts',(44.5821156076045,44.781330806447,47.0886040554932));
#34405=CARTESIAN_POINT('Ctrl Pts',(44.5503195212965,44.7855553029591,47.015935628046));
#34406=CARTESIAN_POINT('Ctrl Pts',(44.5149876018931,44.7897797994711,46.9450981634586));
#34407=CARTESIAN_POINT('Ctrl Pts',(44.4796387197172,44.7940063241541,46.8742266899686));
#34408=CARTESIAN_POINT('Ctrl Pts',(44.4407508533913,44.7982328488372,46.8051883399968));
#34409=CARTESIAN_POINT('Ctrl Pts',(44.3985541571483,44.8024593735202,46.7383456408964));
#34410=CARTESIAN_POINT('Ctrl Pts',(44.3562803267192,44.8066936241527,46.6713807555194));
#34411=CARTESIAN_POINT('Ctrl Pts',(44.3106858510907,44.8109278747852,46.6066199258715));
#34412=CARTESIAN_POINT('Ctrl Pts',(44.2620432863374,44.8151621254177,46.544395231972));
#34413=CARTESIAN_POINT('Ctrl Pts',(44.215651071391,44.8192004870146,46.4850492375945));
#34414=CARTESIAN_POINT('Ctrl Pts',(44.1664868188274,44.8232388486116,46.4280101564727));
#34415=CARTESIAN_POINT('Ctrl Pts',(44.1148177422448,44.8272772102086,46.3735343373491));
#34416=CARTESIAN_POINT('Ctrl Pts',(44.0606263616456,44.8315127105267,46.3163991988324));
#34417=CARTESIAN_POINT('Ctrl Pts',(44.0034733661707,44.8357482108448,46.2618667882227));
#34418=CARTESIAN_POINT('Ctrl Pts',(43.9436387580783,44.8399837111628,46.210259844151));
#34419=CARTESIAN_POINT('Ctrl Pts',(43.8838908911942,44.8442130713485,46.1587277137837));
#34420=CARTESIAN_POINT('Ctrl Pts',(43.8214694839679,44.8484424315342,46.1101129320315));
#34421=CARTESIAN_POINT('Ctrl Pts',(43.7566923465237,44.8526717917199,46.0647025247306));
#34422=CARTESIAN_POINT('Ctrl Pts',(43.6919908553802,44.8568962128875,46.0193451473947));
#34423=CARTESIAN_POINT('Ctrl Pts',(43.6249394831052,44.8611206340551,45.9771849763871));
#34424=CARTESIAN_POINT('Ctrl Pts',(43.5558889924924,44.8653450552227,45.9384687540726));
#34425=CARTESIAN_POINT('Ctrl Pts',(43.4868826583859,44.8695667749514,45.8997772900633));
#34426=CARTESIAN_POINT('Ctrl Pts',(43.4158801515753,44.8737884946802,45.8645256324937));
#34427=CARTESIAN_POINT('Ctrl Pts',(43.3432600558127,44.8780102144089,45.832916497223));
#34428=CARTESIAN_POINT('Ctrl Pts',(43.2706637210468,44.8822305528083,45.8013177043314));
#34429=CARTESIAN_POINT('Ctrl Pts',(43.1964512783069,44.8864508912077,45.773359254359));
#34430=CARTESIAN_POINT('Ctrl Pts',(43.1210233282464,44.8906712296071,45.7491966320834));
#34431=CARTESIAN_POINT('Ctrl Pts',(43.0455965033378,44.8948915050521,45.7250343702396));
#34432=CARTESIAN_POINT('Ctrl Pts',(42.9689546545346,44.8991117804971,45.7046679654549));
#34433=CARTESIAN_POINT('Ctrl Pts',(42.8915142257092,44.903332055942,45.6882032514026));
#34434=CARTESIAN_POINT('Ctrl Pts',(42.8139963384641,44.9075565526429,45.6717220688112));
#34435=CARTESIAN_POINT('Ctrl Pts',(42.7356787357484,44.9117810493438,45.659150470723));
#34436=CARTESIAN_POINT('Ctrl Pts',(42.6569881685724,44.9160055460447,45.6505431431682));
#34437=CARTESIAN_POINT('Ctrl Pts',(42.5782598222871,44.920232070914,45.6419316832609));
#34438=CARTESIAN_POINT('Ctrl Pts',(42.4991586240225,44.9244585957833,45.6372883129055));
#34439=CARTESIAN_POINT('Ctrl Pts',(42.4201139809706,44.9286851206526,45.6366155901611));
#34440=CARTESIAN_POINT('Ctrl Pts',(42.3409248470153,44.9329193714647,45.6359416377026));
#34441=CARTESIAN_POINT('Ctrl Pts',(42.2617929450269,44.9371536222769,45.6392528167839));
#34442=CARTESIAN_POINT('Ctrl Pts',(42.1831450141727,44.9413878730891,45.6464995525767));
#34443=CARTESIAN_POINT('Ctrl Pts',(42.1081356064422,44.9454262329309,45.653411029508));
#34444=CARTESIAN_POINT('Ctrl Pts',(42.0335667283851,44.9494645927727,45.6639018852172));
#34445=CARTESIAN_POINT('Ctrl Pts',(41.9597985362927,44.9535029526145,45.6778860682021));
#34446=CARTESIAN_POINT('Ctrl Pts',(41.8824291967322,44.9577384533772,45.692552918116));
#34447=CARTESIAN_POINT('Ctrl Pts',(41.805646616342,44.9619739541399,45.7111186237424));
#34448=CARTESIAN_POINT('Ctrl Pts',(41.7298737062781,44.9662094549025,45.7335222940954));
#34449=CARTESIAN_POINT('Ctrl Pts',(41.6542106428243,44.9704388155368,45.7558934862549));
#34450=CARTESIAN_POINT('Ctrl Pts',(41.5795547893287,44.974668176171,45.7820914624098));
#34451=CARTESIAN_POINT('Ctrl Pts',(41.5063194752089,44.9788975368052,45.8120042137817));
#34452=CARTESIAN_POINT('Ctrl Pts',(41.4331696847166,44.9831219584251,45.8418820332763));
#34453=CARTESIAN_POINT('Ctrl Pts',(41.361437569315,44.9873463800451,45.8754658308542));
#34454=CARTESIAN_POINT('Ctrl Pts',(41.2915204059977,44.991570801665,45.9125940906042));
#34455=CARTESIAN_POINT('Ctrl Pts',(41.2216479533683,44.9957925218481,45.9496986075427));
#34456=CARTESIAN_POINT('Ctrl Pts',(41.1535885626358,45.0000142420313,45.990342868372));
#34457=CARTESIAN_POINT('Ctrl Pts',(41.0877175341625,45.0042359622144,46.0343181410118));
#34458=CARTESIAN_POINT('Ctrl Pts',(41.0218680583941,45.0084563010697,46.0782790251398));
#34459=CARTESIAN_POINT('Ctrl Pts',(40.958205913163,45.012676639925,46.1255684965106));
#34460=CARTESIAN_POINT('Ctrl Pts',(40.8970785871185,45.0168969787802,46.1759337546015));
#34461=CARTESIAN_POINT('Ctrl Pts',(40.8359521728926,45.0211172546819,46.2262982614084));
#34462=CARTESIAN_POINT('Ctrl Pts',(40.7773608640782,45.0253375305836,46.2797381642466));
#34463=CARTESIAN_POINT('Ctrl Pts',(40.7216189623958,45.0295578064853,46.3359604771789));
#34464=CARTESIAN_POINT('Ctrl Pts',(40.6658213058933,45.033782303641,46.3922390254539));
#34465=CARTESIAN_POINT('Ctrl Pts',(40.6128790811359,45.0380068007966,46.4513052092275));
#34466=CARTESIAN_POINT('Ctrl Pts',(40.5630691493132,45.0422312979523,46.5128297035326));
#34467=CARTESIAN_POINT('Ctrl Pts',(40.5132353038953,45.046457823276,46.5743837355584));
#34468=CARTESIAN_POINT('Ctrl Pts',(40.4665370241649,45.0506843485998,46.6383980495722));
#34469=CARTESIAN_POINT('Ctrl Pts',(40.4232087671965,45.0549108739235,46.7045128858954));
#34470=CARTESIAN_POINT('Ctrl Pts',(40.3798013077261,45.0591451251842,46.7707485777715));
#34471=CARTESIAN_POINT('Ctrl Pts',(40.3397764185185,45.0633793764449,46.8390920584642));
#34472=CARTESIAN_POINT('Ctrl Pts',(40.303323268048,45.0676136277056,46.9091576087302));
#34473=CARTESIAN_POINT('Ctrl Pts',(40.2685566041134,45.0716519834771,46.9759816118151));
#34474=CARTESIAN_POINT('Ctrl Pts',(40.2370386144975,45.0756903392487,47.0443715272226));
#34475=CARTESIAN_POINT('Ctrl Pts',(40.2088917686089,45.0797286950203,47.1139779013873));
#34476=CARTESIAN_POINT('Ctrl Pts',(40.1757163997721,45.0844885158097,47.1960196742183));
#34477=CARTESIAN_POINT('Ctrl Pts',(40.1471176123712,45.0892483365991,47.2800134669348));
#34478=CARTESIAN_POINT('Ctrl Pts',(40.1233014859866,45.0940081573885,47.3654652750329));
#34479=CARTESIAN_POINT('Ctrl Pts',(40.0995701814865,45.0987510259261,47.450612743824));
#34480=CARTESIAN_POINT('Ctrl Pts',(40.0805876735128,45.1034938944638,47.5372076374993));
#34481=CARTESIAN_POINT('Ctrl Pts',(40.066511289221,45.1082367630015,47.6247389207938));
#34482=CARTESIAN_POINT('Ctrl Pts',(40.052520392988,45.112950827365,47.7117386130679));
#34483=CARTESIAN_POINT('Ctrl Pts',(40.0433763266751,45.1176648917286,47.7996631151682));
#34484=CARTESIAN_POINT('Ctrl Pts',(40.0391855935731,45.1223789560921,47.8879920569462));
#34485=CARTESIAN_POINT('Ctrl Pts',(40.0374389765965,45.1243436874758,47.9248058614714));
#34486=CARTESIAN_POINT('Ctrl Pts',(40.036552198086,45.1263084188595,47.9616897171321));
#34487=CARTESIAN_POINT('Ctrl Pts',(40.0365304116029,45.1282731502432,47.9986051444044));
#34488=CARTESIAN_POINT('',(40.0365307523589,45.9220231503247,48.0018858300131));
#34489=CARTESIAN_POINT('Ctrl Pts',(40.0365304116026,45.1282731502717,47.9986051449398));
#34490=CARTESIAN_POINT('Ctrl Pts',(40.0364831607206,45.132534293567,48.0786679599995));
#34491=CARTESIAN_POINT('Ctrl Pts',(40.0405084554841,45.1367954368622,48.1587400086586));
#34492=CARTESIAN_POINT('Ctrl Pts',(40.048582621628,45.1410565801575,48.2383836269337));
#34493=CARTESIAN_POINT('Ctrl Pts',(40.0566584521647,45.1453186018365,48.3180436627888));
#34494=CARTESIAN_POINT('Ctrl Pts',(40.0687847659602,45.1495806235155,48.3972746385648));
#34495=CARTESIAN_POINT('Ctrl Pts',(40.0848861177655,45.1538426451946,48.4756449865026));
#34496=CARTESIAN_POINT('Ctrl Pts',(40.1012920702124,45.1581852945472,48.5554979216514));
#34497=CARTESIAN_POINT('Ctrl Pts',(40.1218249154472,45.1625279438999,48.6344568465592));
#34498=CARTESIAN_POINT('Ctrl Pts',(40.146351044666,45.1668705932525,48.7120792280512));
#34499=CARTESIAN_POINT('Ctrl Pts',(40.1704688745975,45.1711409482525,48.7884093892029));
#34500=CARTESIAN_POINT('Ctrl Pts',(40.1984478103584,45.1754113032524,48.8634467624919));
#34501=CARTESIAN_POINT('Ctrl Pts',(40.230111961434,45.1796816582524,48.9367904466786));
#34502=CARTESIAN_POINT('Ctrl Pts',(40.2625801929569,45.1840604547813,49.0119966226859));
#34503=CARTESIAN_POINT('Ctrl Pts',(40.2989231194113,45.1884392513103,49.0854214593619));
#34504=CARTESIAN_POINT('Ctrl Pts',(40.3389017872644,45.1928180478393,49.1566609694972));
#34505=CARTESIAN_POINT('Ctrl Pts',(40.3788804551175,45.1971968443683,49.2279004796325));
#34506=CARTESIAN_POINT('Ctrl Pts',(40.4224945307587,45.2015756408973,49.2969542716546));
#34507=CARTESIAN_POINT('Ctrl Pts',(40.4694596645134,45.2059544374263,49.3634531359601));
#34508=CARTESIAN_POINT('Ctrl Pts',(40.5148878710121,45.2101899384678,49.4277758344831));
#34509=CARTESIAN_POINT('Ctrl Pts',(40.5636206474227,45.2144254395093,49.4899479095042));
#34510=CARTESIAN_POINT('Ctrl Pts',(40.6154272214919,45.2186609405509,49.5496097699446));
#34511=CARTESIAN_POINT('Ctrl Pts',(40.6671586923627,45.2228903014513,49.6091851394982));
#34512=CARTESIAN_POINT('Ctrl Pts',(40.7219548068612,45.2271196623518,49.6662571695286));
#34513=CARTESIAN_POINT('Ctrl Pts',(40.7795422497894,45.2313490232522,49.7204961844429));
#34514=CARTESIAN_POINT('Ctrl Pts',(40.8370624422827,45.2355734451183,49.7746718592058));
#34515=CARTESIAN_POINT('Ctrl Pts',(40.8973671456749,45.2397978669843,49.8260207731037));
#34516=CARTESIAN_POINT('Ctrl Pts',(40.9601446506006,45.2440222888504,49.8742483863421));
#34517=CARTESIAN_POINT('Ctrl Pts',(41.0228820103333,45.2482440092674,49.9224451588065));
#34518=CARTESIAN_POINT('Ctrl Pts',(41.0880886618312,45.2524657296844,49.9675243071242));
#34519=CARTESIAN_POINT('Ctrl Pts',(41.1554190427955,45.2566874501014,50.0092308682339));
#34520=CARTESIAN_POINT('Ctrl Pts',(41.2227273933636,45.260907789178,50.0509237830215));
#34521=CARTESIAN_POINT('Ctrl Pts',(41.2921576948924,45.2651281282547,50.0892460548279));
#34522=CARTESIAN_POINT('Ctrl Pts',(41.3633358160648,45.2693484673313,50.123986301897));
#34523=CARTESIAN_POINT('Ctrl Pts',(41.4345128752798,45.2735687434417,50.1587260306514));
#34524=CARTESIAN_POINT('Ctrl Pts',(41.5074372799248,45.277789019552,50.1898836362334));
#34525=CARTESIAN_POINT('Ctrl Pts',(41.5817120920012,45.2820092956624,50.2172945993988));
#34526=CARTESIAN_POINT('Ctrl Pts',(41.6560611957255,45.2862337930055,50.2447329797406));
#34527=CARTESIAN_POINT('Ctrl Pts',(41.7317629637269,45.2904582903486,50.2684170686901));
#34528=CARTESIAN_POINT('Ctrl Pts',(41.8084029152355,45.2946827876917,50.2882314852738));
#34529=CARTESIAN_POINT('Ctrl Pts',(41.8850796611432,45.2989093131916,50.3080554146446));
#34530=CARTESIAN_POINT('Ctrl Pts',(41.9626950274675,45.3031358386915,50.3240058760595));
#34531=CARTESIAN_POINT('Ctrl Pts',(42.0408244216449,45.3073623641914,50.3360186953048));
#34532=CARTESIAN_POINT('Ctrl Pts',(42.119096633161,45.3115966156072,50.3480534734925));
#34533=CARTESIAN_POINT('Ctrl Pts',(42.1978842819863,45.3158308670229,50.3561361784949));
#34534=CARTESIAN_POINT('Ctrl Pts',(42.2767579321219,45.3200651184387,50.3602546120292));
#34535=CARTESIAN_POINT('Ctrl Pts',(42.3519824932765,45.3241034722365,50.3641825062592));
#34536=CARTESIAN_POINT('Ctrl Pts',(42.4272849167069,45.3281418260342,50.3645048659867));
#34537=CARTESIAN_POINT('Ctrl Pts',(42.5022964251498,45.332180179832,50.3612551497671));
#34538=CARTESIAN_POINT('Ctrl Pts',(42.5809699470928,45.3364156834596,50.357846784496));
#34539=CARTESIAN_POINT('Ctrl Pts',(42.6596224767622,45.3406511870872,50.3504957088366));
#34540=CARTESIAN_POINT('Ctrl Pts',(42.7378267416534,45.3448866907148,50.3392014734785));
#34541=CARTESIAN_POINT('Ctrl Pts',(42.8159176356725,45.3491160542331,50.3279236111061));
#34542=CARTESIAN_POINT('Ctrl Pts',(42.8935610947764,45.3533454177513,50.3127140071283));
#34543=CARTESIAN_POINT('Ctrl Pts',(42.9703319909164,45.3575747812695,50.2936241760666));
#34544=CARTESIAN_POINT('Ctrl Pts',(43.0470132349386,45.3617992057885,50.2745566378773));
#34545=CARTESIAN_POINT('Ctrl Pts',(43.1228234877626,45.3660236303075,50.2516179897764));
#34546=CARTESIAN_POINT('Ctrl Pts',(43.1973464006665,45.3702480548265,50.2249110450183));
#34547=CARTESIAN_POINT('Ctrl Pts',(43.2718216577657,45.3744697779167,50.1982211787786));
#34548=CARTESIAN_POINT('Ctrl Pts',(43.3450107682317,45.3786915010068,50.1677679566239));
#34549=CARTESIAN_POINT('Ctrl Pts',(43.4165123543819,45.3829132240969,50.1337040737387));
#34550=CARTESIAN_POINT('Ctrl Pts',(43.4879905456159,45.387133565863,50.099651336364));
#34551=CARTESIAN_POINT('Ctrl Pts',(43.557781885516,45.3913539076292,50.0619904858153));
#34552=CARTESIAN_POINT('Ctrl Pts',(43.625506193939,45.3955742493953,50.0209218217232));
#34553=CARTESIAN_POINT('Ctrl Pts',(43.6932294921368,45.3997945282077,49.9798537702414));
#34554=CARTESIAN_POINT('Ctrl Pts',(43.7588854195137,45.4040148070201,49.9353782507703));
#34555=CARTESIAN_POINT('Ctrl Pts',(43.8221208704177,45.4082350858325,49.8877400962056));
#34556=CARTESIAN_POINT('Ctrl Pts',(43.8854195710733,45.4124595858781,49.8400542927131));
#34557=CARTESIAN_POINT('Ctrl Pts',(43.9462925831825,45.4166840859238,49.7891998180229));
#34558=CARTESIAN_POINT('Ctrl Pts',(44.004418637284,45.4209085859694,49.7354628423668));
#34559=CARTESIAN_POINT('Ctrl Pts',(44.0625725974162,45.4251351141766,49.6817000678549));
#34560=CARTESIAN_POINT('Ctrl Pts',(44.1179766436995,45.4293616423837,49.6250523715345));
#34561=CARTESIAN_POINT('Ctrl Pts',(44.1703471026072,45.4335881705909,49.5658421303536));
#34562=CARTESIAN_POINT('Ctrl Pts',(44.2228132922078,45.4378224246894,49.5065236556851));
#34563=CARTESIAN_POINT('Ctrl Pts',(44.2722345200738,45.4420566787879,49.4446336437347));
#34564=CARTESIAN_POINT('Ctrl Pts',(44.318368205642,45.4462909328864,49.3805266634448));
#34565=CARTESIAN_POINT('Ctrl Pts',(44.3623672269892,45.4503292626703,49.3193859945487));
#34566=CARTESIAN_POINT('Ctrl Pts',(44.4033760505672,45.4543675924541,49.2562293028178));
#34567=CARTESIAN_POINT('Ctrl Pts',(44.4412233136354,45.458405922238,49.1913848348756));
#34568=CARTESIAN_POINT('Ctrl Pts',(44.4809183637648,45.4626414122104,49.1233745166407));
#34569=CARTESIAN_POINT('Ctrl Pts',(44.5172861515701,45.4668769021828,49.053248888801));
#34570=CARTESIAN_POINT('Ctrl Pts',(44.5500951483325,45.4711123921553,48.9813670536639));
#34571=CARTESIAN_POINT('Ctrl Pts',(44.5828565822975,45.4753417419902,48.9095894247354));
#34572=CARTESIAN_POINT('Ctrl Pts',(44.6120692771118,45.4795710918251,48.8360610676888));
#34573=CARTESIAN_POINT('Ctrl Pts',(44.6375465671233,45.48380044166,48.7611673934522));
#34574=CARTESIAN_POINT('Ctrl Pts',(44.6629941050983,45.4880248525171,48.6863611790406));
#34575=CARTESIAN_POINT('Ctrl Pts',(44.6847147563111,45.4922492633742,48.6101932578452));
#34576=CARTESIAN_POINT('Ctrl Pts',(44.7025697482568,45.4964736742313,48.53306940947));
#34577=CARTESIAN_POINT('Ctrl Pts',(44.7204133223606,45.5006953836784,48.4559948799579));
#34578=CARTESIAN_POINT('Ctrl Pts',(44.7343960380072,45.5049170931254,48.3779660925758));
#34579=CARTESIAN_POINT('Ctrl Pts',(44.7444291739671,45.5091388025724,48.2994032216792));
#34580=CARTESIAN_POINT('Ctrl Pts',(44.7544590272192,45.5133591307326,48.2208660555029));
#34581=CARTESIAN_POINT('Ctrl Pts',(44.7605418073509,45.5175794588928,48.141795618018));
#34582=CARTESIAN_POINT('Ctrl Pts',(44.7626402974864,45.521799787053,48.0626200095295));
#34583=CARTESIAN_POINT('Ctrl Pts',(44.7647387563468,45.526020052315,47.9834455810443));
#34584=CARTESIAN_POINT('Ctrl Pts',(44.7628530321443,45.530240317577,47.9041664538956));
#34585=CARTESIAN_POINT('Ctrl Pts',(44.7569980087985,45.534460582839,47.8252120501289));
#34586=CARTESIAN_POINT('Ctrl Pts',(44.7511371288338,45.5386850695163,47.7461786704446));
#34587=CARTESIAN_POINT('Ctrl Pts',(44.7412990531836,45.5429095561935,47.6674711321817));
#34588=CARTESIAN_POINT('Ctrl Pts',(44.7275506547398,45.5471340428707,47.5895144454181));
#34589=CARTESIAN_POINT('Ctrl Pts',(44.7137956554857,45.5513605577868,47.5115203304913));
#34590=CARTESIAN_POINT('Ctrl Pts',(44.6961266982247,45.5555870727028,47.4342782433785));
#34591=CARTESIAN_POINT('Ctrl Pts',(44.6746614457831,45.5598135876188,47.358201162382));
#34592=CARTESIAN_POINT('Ctrl Pts',(44.6531569542943,45.5640478287155,47.2819850104764));
#34593=CARTESIAN_POINT('Ctrl Pts',(44.6278424508328,45.5682820698122,47.2069385661546));
#34594=CARTESIAN_POINT('Ctrl Pts',(44.5988849035263,45.5725163109089,47.1334576629246));
#34595=CARTESIAN_POINT('Ctrl Pts',(44.5712663432456,45.5765547621538,47.0633744913818));
#34596=CARTESIAN_POINT('Ctrl Pts',(44.5403343790282,45.5805932133988,46.9947155913935));
#34597=CARTESIAN_POINT('Ctrl Pts',(44.5062723882212,45.5846316646438,46.9278026918907));
#34598=CARTESIAN_POINT('Ctrl Pts',(44.4705483286529,45.5888671737677,46.8576247501119));
#34599=CARTESIAN_POINT('Ctrl Pts',(44.4312451870556,45.5931026828915,46.7891007845917));
#34600=CARTESIAN_POINT('Ctrl Pts',(44.3885397261206,45.5973381920153,46.7226197909235));
#34601=CARTESIAN_POINT('Ctrl Pts',(44.3458961751394,45.6015675609368,46.6562351745138));
#34602=CARTESIAN_POINT('Ctrl Pts',(44.2998603510811,45.6057969298582,46.591888040118));
#34603=CARTESIAN_POINT('Ctrl Pts',(44.2506554133761,45.6100262987796,46.5299438847983));
#34604=CARTESIAN_POINT('Ctrl Pts',(44.2015079384275,45.6142507285383,46.4680720694119));
#34605=CARTESIAN_POINT('Ctrl Pts',(44.1491989947642,45.6184751582969,46.4085980221448));
#34606=CARTESIAN_POINT('Ctrl Pts',(44.0939947821361,45.6226995880556,46.3518579797251));
#34607=CARTESIAN_POINT('Ctrl Pts',(44.0388258726987,45.626921316284,46.2951542226621));
#34608=CARTESIAN_POINT('Ctrl Pts',(43.9807656955991,45.6311430445124,46.241181335737));
#34609=CARTESIAN_POINT('Ctrl Pts',(43.9201196342383,45.6353647727409,46.1902412485352));
#34610=CARTESIAN_POINT('Ctrl Pts',(43.8594934174458,45.6395851195379,46.1393178299187));
#34611=CARTESIAN_POINT('Ctrl Pts',(43.7962833556874,45.6438054663349,46.0914255421101));
#34612=CARTESIAN_POINT('Ctrl Pts',(43.7308293617135,45.6480258131319,46.0468272859521));
#34613=CARTESIAN_POINT('Ctrl Pts',(43.6653763458594,45.6522460968616,46.0022296962537));
#34614=CARTESIAN_POINT('Ctrl Pts',(43.5976798530667,45.6564663805913,45.960926303538));
#34615=CARTESIAN_POINT('Ctrl Pts',(43.5281090938304,45.6606866643211,45.9231369054949));
#34616=CARTESIAN_POINT('Ctrl Pts',(43.4584687516683,45.6649111690725,45.8853097114452));
#34617=CARTESIAN_POINT('Ctrl Pts',(43.3869508117429,45.669135673824,45.8510037575045));
#34618=CARTESIAN_POINT('Ctrl Pts',(43.3139488995933,45.6733601785755,45.8203927303681));
#34619=CARTESIAN_POINT('Ctrl Pts',(43.2409119414849,45.677586711381,45.7897670078249));
#34620=CARTESIAN_POINT('Ctrl Pts',(43.1663900339697,45.6818132441865,45.7628399054713));
#34621=CARTESIAN_POINT('Ctrl Pts',(43.0907941606151,45.686039776992,45.7397358852205));
#34622=CARTESIAN_POINT('Ctrl Pts',(43.0150601059946,45.6902740354527,45.7165896332628));
#34623=CARTESIAN_POINT('Ctrl Pts',(42.9382486191926,45.6945082939134,45.6972805421796));
#34624=CARTESIAN_POINT('Ctrl Pts',(42.8607829384152,45.6987425523741,45.6818823315963));
#34625=CARTESIAN_POINT('Ctrl Pts',(42.7869025904808,45.7027808372659,45.6671967941551));
#34626=CARTESIAN_POINT('Ctrl Pts',(42.7124276233734,45.7068191221578,45.6560681495653));
#34627=CARTESIAN_POINT('Ctrl Pts',(42.6377277782365,45.7108574070496,45.6485162249433));
#34628=CARTESIAN_POINT('Ctrl Pts',(42.5593794600486,45.7150929289448,45.6405954509159));
#34629=CARTESIAN_POINT('Ctrl Pts',(42.4804859357017,45.7193284508399,45.6365796021642));
#34630=CARTESIAN_POINT('Ctrl Pts',(42.4014699915066,45.723563972735,45.6365304571404));
#34631=CARTESIAN_POINT('Ctrl Pts',(42.3225685914181,45.7277933546786,45.6364813833589));
#34632=CARTESIAN_POINT('Ctrl Pts',(42.2435455892698,45.7320227366221,45.6403875945823));
#34633=CARTESIAN_POINT('Ctrl Pts',(42.1648291082892,45.7362521185657,45.6482591357482));
#34634=CARTESIAN_POINT('Ctrl Pts',(42.0862045482709,45.7404765616596,45.6561214849427));
#34635=CARTESIAN_POINT('Ctrl Pts',(42.0078862627192,45.7447010047536,45.6679399159463));
#34636=CARTESIAN_POINT('Ctrl Pts',(41.9303010502155,45.7489254478476,45.6836724459889));
#34637=CARTESIAN_POINT('Ctrl Pts',(41.8527654500533,45.7531471895955,45.6993949157682));
#34638=CARTESIAN_POINT('Ctrl Pts',(41.7759624512762,45.7573689313433,45.7190264238513));
#34639=CARTESIAN_POINT('Ctrl Pts',(41.7003111969052,45.7615906730912,45.7424734730853));
#34640=CARTESIAN_POINT('Ctrl Pts',(41.6246846940734,45.7658110335717,45.7659128509255));
#34641=CARTESIAN_POINT('Ctrl Pts',(41.5502096353618,45.7700313940522,45.7931651522315));
#34642=CARTESIAN_POINT('Ctrl Pts',(41.4772910193502,45.7742517545327,45.8240867255499));
#34643=CARTESIAN_POINT('Ctrl Pts',(41.4043734905107,45.7784720520902,45.8550078378465));
#34644=CARTESIAN_POINT('Ctrl Pts',(41.3330127898229,45.7826923496478,45.8895979289479));
#34645=CARTESIAN_POINT('Ctrl Pts',(41.2635935145341,45.7869126472053,45.9276653888209));
#34646=CARTESIAN_POINT('Ctrl Pts',(41.1941048059683,45.7911371659116,45.9657709238319));
#34647=CARTESIAN_POINT('Ctrl Pts',(41.1265618143403,45.7953616846179,46.0073605492878));
#34648=CARTESIAN_POINT('Ctrl Pts',(41.0613235644421,45.7995862033242,46.0521971758461));
#34649=CARTESIAN_POINT('Ctrl Pts',(40.9960539943587,45.8038127501767,46.0970553279887));
#34650=CARTESIAN_POINT('Ctrl Pts',(40.9330917437077,45.8080392970292,46.1451633013083));
#34651=CARTESIAN_POINT('Ctrl Pts',(40.872763828304,45.8122658438817,46.1962427777655));
#34652=CARTESIAN_POINT('Ctrl Pts',(40.8123256404039,45.8165001163761,46.2474156216355));
#34653=CARTESIAN_POINT('Ctrl Pts',(40.7545317531609,45.8207343888705,46.3015705004234));
#34654=CARTESIAN_POINT('Ctrl Pts',(40.6996731362859,45.8249686613649,46.3583913385242));
#34655=CARTESIAN_POINT('Ctrl Pts',(40.6473552893458,45.8290068240618,46.4125805266612));
#34656=CARTESIAN_POINT('Ctrl Pts',(40.5977070470928,45.8330449867586,46.4691939018447));
#34657=CARTESIAN_POINT('Ctrl Pts',(40.5509450912843,45.8370831494555,46.527931256546));
#34658=CARTESIAN_POINT('Ctrl Pts',(40.5019863988631,45.8413110129399,46.5894279162287));
#34659=CARTESIAN_POINT('Ctrl Pts',(40.456001613711,45.8455388764243,46.6534920074066));
#34660=CARTESIAN_POINT('Ctrl Pts',(40.4132720529381,45.8497667399087,46.7198037239302));
#34661=CARTESIAN_POINT('Ctrl Pts',(40.3706026233879,45.8539886537274,46.7860221232156));
#34662=CARTESIAN_POINT('Ctrl Pts',(40.3311795791544,45.8582105675462,46.8544814788692));
#34663=CARTESIAN_POINT('Ctrl Pts',(40.2952439087338,45.8624324813649,46.924829205578));
#34664=CARTESIAN_POINT('Ctrl Pts',(40.259347505455,45.8666497818708,46.9951000628667));
#34665=CARTESIAN_POINT('Ctrl Pts',(40.2269311231829,45.8708670823768,47.0672547778774));
#34666=CARTESIAN_POINT('Ctrl Pts',(40.1981915184993,45.8750843828827,47.140913361941));
#34667=CARTESIAN_POINT('Ctrl Pts',(40.1694724175153,45.8792986746394,47.2145193957521));
#34668=CARTESIAN_POINT('Ctrl Pts',(40.1444250573977,45.8835129663961,47.289626731564));
#34669=CARTESIAN_POINT('Ctrl Pts',(40.1231988235759,45.8877272581529,47.3658337410947));
#34670=CARTESIAN_POINT('Ctrl Pts',(40.101981865698,45.8919397082483,47.4420074478764));
#34671=CARTESIAN_POINT('Ctrl Pts',(40.0845828410875,45.8961521583437,47.5192794202338));
#34672=CARTESIAN_POINT('Ctrl Pts',(40.0711013561075,45.9003646084391,47.5972326386414));
#34673=CARTESIAN_POINT('Ctrl Pts',(40.0576170767114,45.9045779316831,47.6752020150418));
#34674=CARTESIAN_POINT('Ctrl Pts',(40.0480520456333,45.908791254927,47.7538524565879));
#34675=CARTESIAN_POINT('Ctrl Pts',(40.0424545776666,45.913004578171,47.832757593492));
#34676=CARTESIAN_POINT('Ctrl Pts',(40.038460804777,45.9160107688712,47.8890561196266));
#34677=CARTESIAN_POINT('Ctrl Pts',(40.0364857490142,45.9190169595715,47.9454840988405));
#34678=CARTESIAN_POINT('Ctrl Pts',(40.0365307523581,45.9220231502717,48.001885829018));
#34679=CARTESIAN_POINT('Ctrl Pts',(40.0365307523589,45.9220231503247,48.0018858300131));
#34680=CARTESIAN_POINT('Ctrl Pts',(40.036604800625,45.9269695181273,48.0946888920839));
#34681=CARTESIAN_POINT('Ctrl Pts',(40.0421487212102,45.9319158859298,48.1872613527968));
#34682=CARTESIAN_POINT('Ctrl Pts',(40.0530579116337,45.9368622537323,48.2790219969011));
#34683=CARTESIAN_POINT('Ctrl Pts',(40.0640877371016,45.9418633190216,48.3717973404419));
#34684=CARTESIAN_POINT('Ctrl Pts',(40.0806020526626,45.946864384311,48.4637427056642));
#34685=CARTESIAN_POINT('Ctrl Pts',(40.1024434110274,45.9518654496003,48.5542780542008));
#34686=CARTESIAN_POINT('Ctrl Pts',(40.1191025498901,45.955679930354,48.6233324105306));
#34687=CARTESIAN_POINT('Ctrl Pts',(40.138859746909,45.9594944111076,48.6915668875298));
#34688=CARTESIAN_POINT('Ctrl Pts',(40.1616266405747,45.9633088918613,48.7587325910458));
#34689=CARTESIAN_POINT('Ctrl Pts',(40.1869069439293,45.9675444820129,48.8333132248749));
#34690=CARTESIAN_POINT('Ctrl Pts',(40.2159668137028,45.9717800721645,48.9067707372094));
#34691=CARTESIAN_POINT('Ctrl Pts',(40.2486871505458,45.9760156623161,48.9786947760529));
#34692=CARTESIAN_POINT('Ctrl Pts',(40.281360050537,45.9802451118505,49.0505145418265));
#34693=CARTESIAN_POINT('Ctrl Pts',(40.3176826864701,45.9844745613849,49.1208048253659));
#34694=CARTESIAN_POINT('Ctrl Pts',(40.3574866697458,45.9887040109194,49.1891718700987));
#34695=CARTESIAN_POINT('Ctrl Pts',(40.3972441604984,45.9929285203005,49.2574590595971));
#34696=CARTESIAN_POINT('Ctrl Pts',(40.4404746830861,45.9971530296815,49.3238270708495));
#34697=CARTESIAN_POINT('Ctrl Pts',(40.4869630542426,46.0013775390626,49.3879049265231));
#34698=CARTESIAN_POINT('Ctrl Pts',(40.5334216895834,46.0055993462791,49.4519417954454));
#34699=CARTESIAN_POINT('Ctrl Pts',(40.5831337626294,46.0098211534956,49.5136910373979));
#34700=CARTESIAN_POINT('Ctrl Pts',(40.6358403875421,46.0140429607121,49.5728100020893));
#34701=CARTESIAN_POINT('Ctrl Pts',(40.6885297569592,46.0182633857612,49.6319096119647));
#34702=CARTESIAN_POINT('Ctrl Pts',(40.7442114194451,46.0224838108103,49.6883803044246));
#34703=CARTESIAN_POINT('Ctrl Pts',(40.8025867147373,46.0267042358594,49.7419130968468));
#34704=CARTESIAN_POINT('Ctrl Pts',(40.8609611261152,46.0309245970032,49.7954450786794));
#34705=CARTESIAN_POINT('Ctrl Pts',(40.9220287424196,46.035144958147,49.8460389326746));
#34706=CARTESIAN_POINT('Ctrl Pts',(40.9854557212912,46.0393653192907,49.8934241269384));
#34707=CARTESIAN_POINT('Ctrl Pts',(41.0489461092583,46.0435898996057,49.9408566930359));
#34708=CARTESIAN_POINT('Ctrl Pts',(41.1148001947032,46.0478144799207,49.9850739099351));
#34709=CARTESIAN_POINT('Ctrl Pts',(41.1826533535065,46.0520390602356,50.0258473741057));
#34710=CARTESIAN_POINT('Ctrl Pts',(41.2505390717185,46.0562656677198,50.0666404034654));
#34711=CARTESIAN_POINT('Ctrl Pts',(41.320425359749,46.0604922752041,50.1039861666234));
#34712=CARTESIAN_POINT('Ctrl Pts',(41.3919233481216,46.0647188826883,50.1377024827692));
#34713=CARTESIAN_POINT('Ctrl Pts',(41.4635519846217,46.0689532134437,50.1714804086704));
#34714=CARTESIAN_POINT('Ctrl Pts',(41.5367977712082,46.0731875441991,50.2016154560557));
#34715=CARTESIAN_POINT('Ctrl Pts',(41.611252425834,46.0774218749545,50.2279739013613));
#34716=CARTESIAN_POINT('Ctrl Pts',(41.682247612818,46.0814594613921,50.2531076255387));
#34717=CARTESIAN_POINT('Ctrl Pts',(41.7543414734322,46.0854970478296,50.2748078360182));
#34718=CARTESIAN_POINT('Ctrl Pts',(41.8271711395766,46.0895346342672,50.2930018616578));
#34719=CARTESIAN_POINT('Ctrl Pts',(41.9035730842204,46.0937702633979,50.3120883001018));
#34720=CARTESIAN_POINT('Ctrl Pts',(41.9810751446395,46.0980058925286,50.3273882921773));
#34721=CARTESIAN_POINT('Ctrl Pts',(42.0592677571527,46.1022415216593,50.338780019494));
#34722=CARTESIAN_POINT('Ctrl Pts',(42.1373470455186,46.1064710121146,50.3501552368394));
#34723=CARTESIAN_POINT('Ctrl Pts',(42.2161144380453,46.11070050257,50.3576333705177));
#34724=CARTESIAN_POINT('Ctrl Pts',(42.2951476654467,46.1149299930254,50.361143034388));
#34725=CARTESIAN_POINT('Ctrl Pts',(42.3740886304944,46.119154546029,50.3646486011226));
#34726=CARTESIAN_POINT('Ctrl Pts',(42.4532943473058,46.1233790990327,50.3641948834675));
#34727=CARTESIAN_POINT('Ctrl Pts',(42.5323363909304,46.1276036520363,50.3597621745709));
#34728=CARTESIAN_POINT('Ctrl Pts',(42.611327906917,46.1318255044939,50.3553322992841));
#34729=CARTESIAN_POINT('Ctrl Pts',(42.6901554900649,46.1360473569514,50.3469285074188));
#34730=CARTESIAN_POINT('Ctrl Pts',(42.7683908985587,46.1402692094089,50.3345831719515));
#34731=CARTESIAN_POINT('Ctrl Pts',(42.8466007226081,46.1444896812416,50.3222418736402));
#34732=CARTESIAN_POINT('Ctrl Pts',(42.9242182933021,46.1487101530743,50.3059616642739));
#34733=CARTESIAN_POINT('Ctrl Pts',(43.000822168485,46.1529306249069,50.2858265819517));
#34734=CARTESIAN_POINT('Ctrl Pts',(43.0774249103957,46.1571510343023,50.2656917975065));
#34735=CARTESIAN_POINT('Ctrl Pts',(43.1530135330446,46.1613714436976,50.2417023740636));
#34736=CARTESIAN_POINT('Ctrl Pts',(43.2271799008161,46.1655918530929,50.2139927399578));
#34737=CARTESIAN_POINT('Ctrl Pts',(43.3014204473718,46.1698164836041,50.186255391579));
#34738=CARTESIAN_POINT('Ctrl Pts',(43.3742354567555,46.1740411141154,50.1547905643507));
#34739=CARTESIAN_POINT('Ctrl Pts',(43.4452355730499,46.1782657446267,50.1197813655495));
#34740=CARTESIAN_POINT('Ctrl Pts',(43.5162697776245,46.1824924034499,50.0847553582776));
#34741=CARTESIAN_POINT('Ctrl Pts',(43.5854869427322,46.1867190622732,50.0461818181882));
#34742=CARTESIAN_POINT('Ctrl Pts',(43.6525234717276,46.1909457210965,50.0042892490036));
#34743=CARTESIAN_POINT('Ctrl Pts',(43.7196825156794,46.1951801044981,49.962320117587));
#34744=CARTESIAN_POINT('Ctrl Pts',(43.7846525739653,46.1994144878997,49.9170201052931));
#34745=CARTESIAN_POINT('Ctrl Pts',(43.8471003027147,46.2036488713014,49.8686602566499));
#34746=CARTESIAN_POINT('Ctrl Pts',(43.9066395500663,46.2076860397586,49.8225527512544));
#34747=CARTESIAN_POINT('Ctrl Pts',(43.9638859411231,46.2117232082158,49.7736643427086));
#34748=CARTESIAN_POINT('Ctrl Pts',(44.0185821359781,46.215760376673,49.7222608135798));
#34749=CARTESIAN_POINT('Ctrl Pts',(44.0759567971213,46.2199952447991,49.6683400596197));
#34750=CARTESIAN_POINT('Ctrl Pts',(44.1307433138437,46.2242301129252,49.6114464648617));
#34751=CARTESIAN_POINT('Ctrl Pts',(44.1826177016614,46.2284649810513,49.5518584248003));
#34752=CARTESIAN_POINT('Ctrl Pts',(44.2344168621055,46.2326937078421,49.4923567983224));
#34753=CARTESIAN_POINT('Ctrl Pts',(44.2833119742782,46.236922434633,49.4301688370739));
#34754=CARTESIAN_POINT('Ctrl Pts',(44.3290145857132,46.2411511614238,49.3656109142087));
#34755=CARTESIAN_POINT('Ctrl Pts',(44.3746638302279,46.2453749503321,49.3011283756031));
#34756=CARTESIAN_POINT('Ctrl Pts',(44.4171277120583,46.2495987392405,49.2342817558782));
#34757=CARTESIAN_POINT('Ctrl Pts',(44.456157905618,46.2538225281488,49.1654205713238));
#34758=CARTESIAN_POINT('Ctrl Pts',(44.4951631451948,46.2580436165746,49.0966034132181));
#34759=CARTESIAN_POINT('Ctrl Pts',(44.5307388228312,46.2622647050004,49.0257746540407));
#34760=CARTESIAN_POINT('Ctrl Pts',(44.5626805084814,46.2664857934262,48.9533118372992));
#34761=CARTESIAN_POINT('Ctrl Pts',(44.5946117550196,46.2707055023251,48.8808727026973));
#34762=CARTESIAN_POINT('Ctrl Pts',(44.6229111785989,46.274925211224,48.806801000239));
#34763=CARTESIAN_POINT('Ctrl Pts',(44.6474214773925,46.2791449201229,48.7314965098038));
#34764=CARTESIAN_POINT('Ctrl Pts',(44.6719314259048,46.2833645687172,48.6561930955591));
#34765=CARTESIAN_POINT('Ctrl Pts',(44.6926522132296,46.2875842173114,48.5796573752252));
#34766=CARTESIAN_POINT('Ctrl Pts',(44.7094761151086,46.2918038659056,48.5023052006926));
#34767=CARTESIAN_POINT('Ctrl Pts',(44.7263168813563,46.2960277442981,48.4248754879294));
#34768=CARTESIAN_POINT('Ctrl Pts',(44.7392528589133,46.3002516226905,48.3466281459569));
#34769=CARTESIAN_POINT('Ctrl Pts',(44.7482274233652,46.3044755010829,48.2679895689311));
#34770=CARTESIAN_POINT('Ctrl Pts',(44.7572063048397,46.3087014112819,48.189313164496));
#34771=CARTESIAN_POINT('Ctrl Pts',(44.7622199474325,46.3129273214809,48.1102456193126));
#34772=CARTESIAN_POINT('Ctrl Pts',(44.7632638423439,46.3171532316798,48.0312162196629));
#34773=CARTESIAN_POINT('Ctrl Pts',(44.7643096490701,46.3213868813149,47.9520420836223));
#34774=CARTESIAN_POINT('Ctrl Pts',(44.761371197878,46.32562053095,47.872906703128));
#34775=CARTESIAN_POINT('Ctrl Pts',(44.7544961246778,46.3298541805851,47.794236932912));
#34776=CARTESIAN_POINT('Ctrl Pts',(44.7479290590336,46.333898160083,47.7190916173384));
#34777=CARTESIAN_POINT('Ctrl Pts',(44.7377706425223,46.3379421395809,47.6443714367161));
#34778=CARTESIAN_POINT('Ctrl Pts',(44.7241057095372,46.3419861190788,47.5704384889254));
#34779=CARTESIAN_POINT('Ctrl Pts',(44.7097907356966,46.3462224706795,47.492988550844));
#34780=CARTESIAN_POINT('Ctrl Pts',(44.6915728757931,46.3504588222802,47.4161079843623));
#34781=CARTESIAN_POINT('Ctrl Pts',(44.6695111642325,46.3546951738808,47.3402201000908));
#34782=CARTESIAN_POINT('Ctrl Pts',(44.6474814451446,46.3589253821973,47.26444226354));
#34783=CARTESIAN_POINT('Ctrl Pts',(44.6216190735712,46.3631555905138,47.189654697226));
#34784=CARTESIAN_POINT('Ctrl Pts',(44.592034243633,46.3673857988303,47.1162713563314));
#34785=CARTESIAN_POINT('Ctrl Pts',(44.5624840160413,46.3716110595052,47.0429738444173));
#34786=CARTESIAN_POINT('Ctrl Pts',(44.5292201564919,46.3758363201802,46.971077727025));
#34787=CARTESIAN_POINT('Ctrl Pts',(44.492402437075,46.3800615808551,46.9009811274493));
#34788=CARTESIAN_POINT('Ctrl Pts',(44.4556083059308,46.384284134502,46.8309294371654));
#34789=CARTESIAN_POINT('Ctrl Pts',(44.4152650516619,46.3885066881488,46.7626753906071));
#34790=CARTESIAN_POINT('Ctrl Pts',(44.3715797613306,46.3927292417956,46.696595348477));
#34791=CARTESIAN_POINT('Ctrl Pts',(44.3279088308731,46.396950407439,46.6305370276418));
#34792=CARTESIAN_POINT('Ctrl Pts',(44.2808983043025,46.4011715730822,46.5666516832776));
#34793=CARTESIAN_POINT('Ctrl Pts',(44.230799463836,46.4053927387255,46.5052880665098));
#34794=CARTESIAN_POINT('Ctrl Pts',(44.1807014627008,46.4096138336495,46.443925477798));
#34795=CARTESIAN_POINT('Ctrl Pts',(44.1275155482453,46.4138349285735,46.3850848952801));
#34796=CARTESIAN_POINT('Ctrl Pts',(44.0715333412382,46.4180560234974,46.3290820696309));
#34797=CARTESIAN_POINT('Ctrl Pts',(44.0154953868851,46.4222813218076,46.2730234761036));
#34798=CARTESIAN_POINT('Ctrl Pts',(43.9566559099006,46.4265066201179,46.2198086170687));
#34799=CARTESIAN_POINT('Ctrl Pts',(43.8953430429374,46.4307319184281,46.1697159715392));
#34800=CARTESIAN_POINT('Ctrl Pts',(43.8340008677528,46.4349592364771,46.1195993811769));
#34801=CARTESIAN_POINT('Ctrl Pts',(43.7701833255224,46.4391865545262,46.0726082561226));
#34802=CARTESIAN_POINT('Ctrl Pts',(43.7042491842033,46.4434138725752,46.028978816348));
#34803=CARTESIAN_POINT('Ctrl Pts',(43.6381949096214,46.4476488928784,45.9852698829021));
#34804=CARTESIAN_POINT('Ctrl Pts',(43.5700167345931,46.4518839131816,45.9449351136142));
#34805=CARTESIAN_POINT('Ctrl Pts',(43.5000995997961,46.4561189334847,45.9081655630934));
#34806=CARTESIAN_POINT('Ctrl Pts',(43.4335510894747,46.4601499094847,45.8731675784154));
#34807=CARTESIAN_POINT('Ctrl Pts',(43.3654276541714,46.4641808854847,45.8413993118555));
#34808=CARTESIAN_POINT('Ctrl Pts',(43.2960761658031,46.4682118614847,45.8129842373729));
#34809=CARTESIAN_POINT('Ctrl Pts',(43.2231943976194,46.4724480309643,45.7831227171648));
#34810=CARTESIAN_POINT('Ctrl Pts',(43.1486802469155,46.4766842004438,45.7568517691367));
#34811=CARTESIAN_POINT('Ctrl Pts',(43.0729216966716,46.4809203699234,45.7343506822439));
#34812=CARTESIAN_POINT('Ctrl Pts',(42.9972727479057,46.485150410848,45.7118821481438));
#34813=CARTESIAN_POINT('Ctrl Pts',(42.9203834206851,46.4893804517726,45.6931727769525));
#34814=CARTESIAN_POINT('Ctrl Pts',(42.84266149648,46.4936104926973,45.678353765012));
#34815=CARTESIAN_POINT('Ctrl Pts',(42.7650300620964,46.497835608684,45.663552006501));
#34816=CARTESIAN_POINT('Ctrl Pts',(42.6865684155536,46.5020607246708,45.6526316937259));
#34817=CARTESIAN_POINT('Ctrl Pts',(42.6076978358981,46.5062858406575,45.6456737588297));
#34818=CARTESIAN_POINT('Ctrl Pts',(42.5288775305307,46.5105082634385,45.6387202591135));
#34819=CARTESIAN_POINT('Ctrl Pts',(42.4496492755223,46.5147306862195,45.6357241653015));
#34820=CARTESIAN_POINT('Ctrl Pts',(42.3704416321956,46.5189531090005,45.6367148407793));
#34821=CARTESIAN_POINT('Ctrl Pts',(42.2912597658661,46.5231741576543,45.637705193856));
#34822=CARTESIAN_POINT('Ctrl Pts',(42.21209896668,46.527395206308,45.6426797340462));
#34823=CARTESIAN_POINT('Ctrl Pts',(42.1333884725642,46.5316162549618,45.651615718342));
#34824=CARTESIAN_POINT('Ctrl Pts',(42.0546790371533,46.5358372468398,45.6605515824433));
#34825=CARTESIAN_POINT('Ctrl Pts',(41.9764203607963,46.5400582387179,45.673448730472));
#34826=CARTESIAN_POINT('Ctrl Pts',(41.8990357375915,46.5442792305959,45.6902326418686));
#34827=CARTESIAN_POINT('Ctrl Pts',(41.8215736413307,46.5485044482894,45.7070333563567));
#34828=CARTESIAN_POINT('Ctrl Pts',(41.744987805847,46.552729665983,45.7277285076792));
#34829=CARTESIAN_POINT('Ctrl Pts',(41.6696899214558,46.5569548836765,45.7521927061964));
#34830=CARTESIAN_POINT('Ctrl Pts',(41.5943558275568,46.5611821332074,45.7766686691422));
#34831=CARTESIAN_POINT('Ctrl Pts',(41.520311357542,46.5654093827383,45.8049171225106));
#34832=CARTESIAN_POINT('Ctrl Pts',(41.447949221445,46.5696366322692,45.8367640544885));
#34833=CARTESIAN_POINT('Ctrl Pts',(41.3754548756137,46.5738716052251,45.8686691726208));
#34834=CARTESIAN_POINT('Ctrl Pts',(41.3046494261874,46.5781065781811,45.9041856961053));
#34835=CARTESIAN_POINT('Ctrl Pts',(41.2359017471559,46.582341551137,45.9430931721088));
#34836=CARTESIAN_POINT('Ctrl Pts',(41.1704487079906,46.5863735687216,45.9801360597606));
#34837=CARTESIAN_POINT('Ctrl Pts',(41.1068610136877,46.5904055863061,46.0202521262543));
#34838=CARTESIAN_POINT('Ctrl Pts',(41.0454303341048,46.5944376038906,46.0632162069202));
#34839=CARTESIAN_POINT('Ctrl Pts',(40.9813670517248,46.5986424129996,46.1080215069851));
#34840=CARTESIAN_POINT('Ctrl Pts',(40.9193984368704,46.6028472221085,46.1561003933127));
#34841=CARTESIAN_POINT('Ctrl Pts',(40.8598822810811,46.6070520312174,46.2072290015811));
#34842=CARTESIAN_POINT('Ctrl Pts',(40.8004528399889,46.6112507139437,46.2582831157609));
#34843=CARTESIAN_POINT('Ctrl Pts',(40.7434691234988,46.6154493966699,46.3123778236317));
#34844=CARTESIAN_POINT('Ctrl Pts',(40.6892595063388,46.6196480793961,46.3692463692367));
#34845=CARTESIAN_POINT('Ctrl Pts',(40.6351126114818,46.6238419041089,46.4260491160713));
#34846=CARTESIAN_POINT('Ctrl Pts',(40.5837337673293,46.6280357288216,46.4856189820183));
#34847=CARTESIAN_POINT('Ctrl Pts',(40.5354165933514,46.6322295535344,46.5476504688778));
#34848=CARTESIAN_POINT('Ctrl Pts',(40.4871295028087,46.636420767071,46.609643333441));
#34849=CARTESIAN_POINT('Ctrl Pts',(40.4419005926706,46.6406119806076,46.6740944028798));
#34850=CARTESIAN_POINT('Ctrl Pts',(40.399984167694,46.6448031941441,46.7406640196416));
#34851=CARTESIAN_POINT('Ctrl Pts',(40.3580802737597,46.6489931547047,46.8072137352147));
#34852=CARTESIAN_POINT('Ctrl Pts',(40.3194871530234,46.6531831152653,46.8758803375015));
#34853=CARTESIAN_POINT('Ctrl Pts',(40.2844156950254,46.6573730758259,46.9462953499936));
#34854=CARTESIAN_POINT('Ctrl Pts',(40.2493433702582,46.6615631399387,47.0167121027487));
#34855=CARTESIAN_POINT('Ctrl Pts',(40.2177930917328,46.6657532040516,47.0888769236911));
#34856=CARTESIAN_POINT('Ctrl Pts',(40.1899289772536,46.6699432681644,47.1623983552328));
#34857=CARTESIAN_POINT('Ctrl Pts',(40.162036879065,46.6741375403254,47.2359936237658));
#34858=CARTESIAN_POINT('Ctrl Pts',(40.1378385045712,46.6783318124865,47.3109477759341));
#34859=CARTESIAN_POINT('Ctrl Pts',(40.1174488569127,46.6825260846475,47.3868517959816));
#34860=CARTESIAN_POINT('Ctrl Pts',(40.0970482647868,46.6867226081508,47.4627965587186));
#34861=CARTESIAN_POINT('Ctrl Pts',(40.0804605684087,46.6909191316541,47.5396917377188));
#34862=CARTESIAN_POINT('Ctrl Pts',(40.0677495871925,46.6951156551574,47.6171182260029));
#34863=CARTESIAN_POINT('Ctrl Pts',(40.0550169035634,46.6993193437005,47.6946769103458));
#34864=CARTESIAN_POINT('Ctrl Pts',(40.0461742027216,46.7035230322435,47.7727682411818));
#34865=CARTESIAN_POINT('Ctrl Pts',(40.0412333527236,46.7077267207866,47.850968645593));
#34866=CARTESIAN_POINT('Ctrl Pts',(40.0380808672715,46.7104088639365,47.9008640355258));
#34867=CARTESIAN_POINT('Ctrl Pts',(40.0365157731703,46.7130910070864,47.9508038052924));
#34868=CARTESIAN_POINT('Ctrl Pts',(40.0365300974769,46.7157731502363,48.000678798438));
#34869=CARTESIAN_POINT('Origin',(42.4,48.4493818343519,48.));
#34870=CARTESIAN_POINT('',(40.4708708151857,32.1775068343172,48.0017734705773));
#34871=CARTESIAN_POINT('Ctrl Pts',(41.794138831786,32.3337813919524,49.8315225365117));
#34872=CARTESIAN_POINT('Ctrl Pts',(41.7886782500385,32.3333951108295,49.8297161954099));
#34873=CARTESIAN_POINT('Ctrl Pts',(41.7832256701112,32.333010105823,49.8278854083931));
#34874=CARTESIAN_POINT('Ctrl Pts',(41.7717294671852,32.3321999839773,49.8239680839032));
#34875=CARTESIAN_POINT('Ctrl Pts',(41.7656878576262,32.331775190185,49.8218758306898));
#34876=CARTESIAN_POINT('Ctrl Pts',(41.7549590389245,32.3310226658072,49.818100524036));
#34877=CARTESIAN_POINT('Ctrl Pts',(41.750267836368,32.3306942574116,49.8164293199577));
#34878=CARTESIAN_POINT('Ctrl Pts',(41.740062550579,32.329981234195,49.8127491712764));
#34879=CARTESIAN_POINT('Ctrl Pts',(41.7345511388645,32.3295970385137,49.8107332245768));
#34880=CARTESIAN_POINT('Ctrl Pts',(41.719807971515,32.3285714368358,49.8052641102468));
#34881=CARTESIAN_POINT('Ctrl Pts',(41.7105931909916,32.3279326625102,49.8017652358244));
#34882=CARTESIAN_POINT('Ctrl Pts',(41.6549588428836,32.324087358939,49.7801514297329));
#34883=CARTESIAN_POINT('Ctrl Pts',(41.6092242731332,32.3209740058822,49.7603125122545));
#34884=CARTESIAN_POINT('Ctrl Pts',(41.4367611911365,32.3092305662373,49.6774203503844));
#34885=CARTESIAN_POINT('Ctrl Pts',(41.3163440513153,32.3009949294976,49.602267998054));
#34886=CARTESIAN_POINT('Ctrl Pts',(41.1418884809709,32.2875473795785,49.4646521162385));
#34887=CARTESIAN_POINT('Ctrl Pts',(41.0817544458631,32.2825785173526,49.4107716797351));
#34888=CARTESIAN_POINT('Ctrl Pts',(41.0126677973322,32.2763154243633,49.3405855876347));
#34889=CARTESIAN_POINT('Ctrl Pts',(41.0003391713107,32.2751744139912,49.327708510472));
#34890=CARTESIAN_POINT('Ctrl Pts',(40.9811716296557,32.2733619595949,49.3071245959298));
#34891=CARTESIAN_POINT('Ctrl Pts',(40.9742127639004,32.2726956732212,49.2995304553285));
#34892=CARTESIAN_POINT('Ctrl Pts',(40.9613827771837,32.2714515228676,49.2853021119403));
#34893=CARTESIAN_POINT('Ctrl Pts',(40.9554958680582,32.2708743482146,49.2786824629801));
#34894=CARTESIAN_POINT('Ctrl Pts',(40.9425244019797,32.2695883164697,49.2638925503667));
#34895=CARTESIAN_POINT('Ctrl Pts',(40.9354625748005,32.268878539553,49.2557028389643));
#34896=CARTESIAN_POINT('Ctrl Pts',(40.9160472984658,32.2668998177003,49.232800068835));
#34897=CARTESIAN_POINT('Ctrl Pts',(40.9038444957099,32.2656247932808,49.2179615312213));
#34898=CARTESIAN_POINT('Ctrl Pts',(40.8350337196072,32.2582493481227,49.131693242776));
#34899=CARTESIAN_POINT('Ctrl Pts',(40.78333075363,32.2519582845867,49.0565156218265));
#34900=CARTESIAN_POINT('Ctrl Pts',(40.6973836322991,32.240006539079,48.9103789886614));
#34901=CARTESIAN_POINT('Ctrl Pts',(40.6617881943141,32.2343928873117,48.8404232095297));
#34902=CARTESIAN_POINT('Ctrl Pts',(40.5920584116766,32.2219013084359,48.6798721347924));
#34903=CARTESIAN_POINT('Ctrl Pts',(40.5602747001927,32.2150479309445,48.5884676141541));
#34904=CARTESIAN_POINT('Ctrl Pts',(40.5327816114671,32.207814182667,48.4849206391801));
#34905=CARTESIAN_POINT('Ctrl Pts',(40.530173009105,32.2071101367896,48.4747626489807));
#34906=CARTESIAN_POINT('Ctrl Pts',(40.5260985363842,32.2059815621403,48.4583418160482));
#34907=CARTESIAN_POINT('Ctrl Pts',(40.5245809627852,32.2055542574737,48.4520921957861));
#34908=CARTESIAN_POINT('Ctrl Pts',(40.5219404904334,32.2047983045004,48.4409761623109));
#34909=CARTESIAN_POINT('Ctrl Pts',(40.52080520832,32.2044689657767,48.4361128684041));
#34910=CARTESIAN_POINT('Ctrl Pts',(40.5183764236116,32.2037548602556,48.425522900488));
#34911=CARTESIAN_POINT('Ctrl Pts',(40.5170901699271,32.2033705065886,48.4197947071277));
#34912=CARTESIAN_POINT('Ctrl Pts',(40.5144844887396,32.2025786931522,48.4079376366705));
#34913=CARTESIAN_POINT('Ctrl Pts',(40.5131687454796,32.2021714395008,48.4018080115956));
#34914=CARTESIAN_POINT('Ctrl Pts',(40.5098570521573,32.2011265739235,48.3860048585975));
#34915=CARTESIAN_POINT('Ctrl Pts',(40.5079054436263,32.2004912822652,48.3763220871882));
#34916=CARTESIAN_POINT('Ctrl Pts',(40.5023681338805,32.1986277657745,48.3477165039367));
#34917=CARTESIAN_POINT('Ctrl Pts',(40.4989912261293,32.1974095732903,48.3287539631835));
#34918=CARTESIAN_POINT('Ctrl Pts',(40.4793365194097,32.189737888435,48.2079295422149));
#34919=CARTESIAN_POINT('Ctrl Pts',(40.4709658658183,32.1835991181717,48.1049438817111));
#34920=CARTESIAN_POINT('Ctrl Pts',(40.4708708187116,32.1774426331651,48.0017773017898));
#34921=CARTESIAN_POINT('',(43.9476533605231,31.6998,49.1516560391721));
#34922=CARTESIAN_POINT('Ctrl Pts',(40.4708708151857,32.1775068343172,48.0017734705773));
#34923=CARTESIAN_POINT('Ctrl Pts',(40.4708092245439,32.1731176722038,47.9347769800571));
#34924=CARTESIAN_POINT('Ctrl Pts',(40.4742419471142,32.1687285100904,47.8676805505439));
#34925=CARTESIAN_POINT('Ctrl Pts',(40.4811735403552,32.164339347977,47.8008830126105));
#34926=CARTESIAN_POINT('Ctrl Pts',(40.4881000068995,32.1599534321451,47.7341348790066));
#34927=CARTESIAN_POINT('Ctrl Pts',(40.4985201638095,32.1555675163132,47.6676857020333));
#34928=CARTESIAN_POINT('Ctrl Pts',(40.512386543448,32.1511816004813,47.6019321721817));
#34929=CARTESIAN_POINT('Ctrl Pts',(40.5262477497833,32.1467973209578,47.5362031738203));
#34930=CARTESIAN_POINT('Ctrl Pts',(40.5435525244123,32.1424130414343,47.4711698040497));
#34931=CARTESIAN_POINT('Ctrl Pts',(40.5642021288926,32.1380287619108,47.4072194897456));
#34932=CARTESIAN_POINT('Ctrl Pts',(40.5848515974943,32.1336445112367,47.3432695962476));
#34933=CARTESIAN_POINT('Ctrl Pts',(40.6088456934916,32.1292602605626,47.2804032260941));
#34934=CARTESIAN_POINT('Ctrl Pts',(40.636036159954,32.1248760098885,47.2189915954934));
#34935=CARTESIAN_POINT('Ctrl Pts',(40.6632540336694,32.1204873400087,47.1575180636339));
#34936=CARTESIAN_POINT('Ctrl Pts',(40.6936744995961,32.1160986701287,47.097502661538));
#34937=CARTESIAN_POINT('Ctrl Pts',(40.7271021030885,32.1117100002489,47.0392944345904));
#34938=CARTESIAN_POINT('Ctrl Pts',(40.7605491529565,32.1073187772777,46.9810523452378));
#34939=CARTESIAN_POINT('Ctrl Pts',(40.7970065427126,32.1029275543065,46.9246199469879));
#34940=CARTESIAN_POINT('Ctrl Pts',(40.8362356319982,32.0985363313353,46.8703170540952));
#34941=CARTESIAN_POINT('Ctrl Pts',(40.8755312425507,32.0941376621114,46.815922079095));
#34942=CARTESIAN_POINT('Ctrl Pts',(40.9176076082244,32.0897389928874,46.7636642053333));
#34943=CARTESIAN_POINT('Ctrl Pts',(40.9621867732401,32.0853403236635,46.7138290619617));
#34944=CARTESIAN_POINT('Ctrl Pts',(40.9796790097263,32.0836143478122,46.6942744535954));
#34945=CARTESIAN_POINT('Ctrl Pts',(40.99755621004,32.0818883719608,46.6750924473109));
#34946=CARTESIAN_POINT('Ctrl Pts',(41.0158001753889,32.0801623961095,46.6562986185739));
#34947=CARTESIAN_POINT('Ctrl Pts',(41.0628485759409,32.0757113679671,46.607832204315));
#34948=CARTESIAN_POINT('Ctrl Pts',(41.1125409804307,32.0712603398248,46.5617415422288));
#34949=CARTESIAN_POINT('Ctrl Pts',(41.1646076147278,32.0668093116824,46.5183292500318));
#34950=CARTESIAN_POINT('Ctrl Pts',(41.2165950871786,32.0623650508606,46.4749829616632));
#34951=CARTESIAN_POINT('Ctrl Pts',(41.270949249308,32.0579207900388,46.4343072768261));
#34952=CARTESIAN_POINT('Ctrl Pts',(41.3273631296451,32.0534765292169,46.3965684606897));
#34953=CARTESIAN_POINT('Ctrl Pts',(41.3837102631183,32.0490375266839,46.3588742957563));
#34954=CARTESIAN_POINT('Ctrl Pts',(41.4421118661863,32.0445985241508,46.3241103733826));
#34955=CARTESIAN_POINT('Ctrl Pts',(41.5022289657174,32.0401595216177,46.2925019101319));
#34956=CARTESIAN_POINT('Ctrl Pts',(41.5623082273727,32.0357233130057,46.2609133413392));
#34957=CARTESIAN_POINT('Ctrl Pts',(41.6241004068553,32.0312871043936,46.2324765224017));
#34958=CARTESIAN_POINT('Ctrl Pts',(41.6872400822758,32.0268508957815,46.2073718019105));
#34959=CARTESIAN_POINT('Ctrl Pts',(41.7503619725508,32.022415936758,46.1822741529016));
#34960=CARTESIAN_POINT('Ctrl Pts',(41.8148301456332,32.0179809777345,46.1605069221356));
#34961=CARTESIAN_POINT('Ctrl Pts',(41.8802589664987,32.0135460187109,46.1422024289512));
#34962=CARTESIAN_POINT('Ctrl Pts',(41.9456921080106,32.0091107668212,46.1238967270143));
#34963=CARTESIAN_POINT('Ctrl Pts',(42.012085545857,32.0046755149315,46.1090543474025));
#34964=CARTESIAN_POINT('Ctrl Pts',(42.0790400437406,32.0002402630417,46.0977573069196));
#34965=CARTESIAN_POINT('Ctrl Pts',(42.146067428378,31.995800182931,46.0864479684636));
#34966=CARTESIAN_POINT('Ctrl Pts',(42.2136566028683,31.9913601028203,46.0786917534496));
#34967=CARTESIAN_POINT('Ctrl Pts',(42.2814007672019,31.9869200227096,46.074519078547));
#34968=CARTESIAN_POINT('Ctrl Pts',(42.3491864044555,31.9824772243856,46.0703438491363));
#34969=CARTESIAN_POINT('Ctrl Pts',(42.4171267253904,31.9780344260616,46.0697565293414));
#34970=CARTESIAN_POINT('Ctrl Pts',(42.484815352849,31.9735916277376,46.072735380696));
#34971=CARTESIAN_POINT('Ctrl Pts',(42.5526229951648,31.9691410177762,46.0757194696744));
#34972=CARTESIAN_POINT('Ctrl Pts',(42.620177568542,31.9646904078149,46.0822821953618));
#34973=CARTESIAN_POINT('Ctrl Pts',(42.6870791397067,31.9602397978536,46.0923501043312));
#34974=CARTESIAN_POINT('Ctrl Pts',(42.7186620950456,31.9581387498036,46.0971029720711));
#34975=CARTESIAN_POINT('Ctrl Pts',(42.7500996918463,31.9560377017536,46.1026362702326));
#34976=CARTESIAN_POINT('Ctrl Pts',(42.7813509885611,31.9539366537035,46.1089383985646));
#34977=CARTESIAN_POINT('Ctrl Pts',(42.8477518181369,31.949472476272,46.1223287725116));
#34978=CARTESIAN_POINT('Ctrl Pts',(42.9135772124744,31.9450082988405,46.1392470232286));
#34979=CARTESIAN_POINT('Ctrl Pts',(42.9784249626804,31.940544121409,46.1596285376457));
#34980=CARTESIAN_POINT('Ctrl Pts',(43.0431742857848,31.9360867197876,46.1799791166273));
#34981=CARTESIAN_POINT('Ctrl Pts',(43.106948444429,31.9316293181663,46.2037823800547));
#34982=CARTESIAN_POINT('Ctrl Pts',(43.1693558339415,31.9271719165449,46.2309227948786));
#34983=CARTESIAN_POINT('Ctrl Pts',(43.2316885407987,31.922719849077,46.2580307308845));
#34984=CARTESIAN_POINT('Ctrl Pts',(43.2926572782625,31.9182677816091,46.2884676911477));
#34985=CARTESIAN_POINT('Ctrl Pts',(43.3518877729144,31.9138157141411,46.3220690643903));
#34986=CARTESIAN_POINT('Ctrl Pts',(43.4110803695575,31.9093664952817,46.3556489381478));
#34987=CARTESIAN_POINT('Ctrl Pts',(43.4685365029924,31.9049172764223,46.3923889661042));
#34988=CARTESIAN_POINT('Ctrl Pts',(43.5239053920692,31.9004680575629,46.4320780546922));
#34989=CARTESIAN_POINT('Ctrl Pts',(43.5792578099748,31.8960201622598,46.4717553365456));
#34990=CARTESIAN_POINT('Ctrl Pts',(43.6325238167008,31.8915722669568,46.5143796509825));
#34991=CARTESIAN_POINT('Ctrl Pts',(43.6833821151811,31.8871243716537,46.5596969404555));
#34992=CARTESIAN_POINT('Ctrl Pts',(43.7342426953449,31.8826762768023,46.6050162630226));
#34993=CARTESIAN_POINT('Ctrl Pts',(43.782694987332,31.878228181951,46.6530284714022));
#34994=CARTESIAN_POINT('Ctrl Pts',(43.8284526329951,31.8737800870996,46.7034408489431));
#34995=CARTESIAN_POINT('Ctrl Pts',(43.8742576062804,31.8693273915361,46.7539053685451));
#34996=CARTESIAN_POINT('Ctrl Pts',(43.9173620398033,31.8648746959727,46.8067746468774));
#34997=CARTESIAN_POINT('Ctrl Pts',(43.9575188633162,31.8604220004092,46.8617216740559));
#34998=CARTESIAN_POINT('Ctrl Pts',(43.9976991946313,31.855966698238,46.9167008672208));
#34999=CARTESIAN_POINT('Ctrl Pts',(44.0349282123254,31.8515113960668,46.9737598184123));
#35000=CARTESIAN_POINT('Ctrl Pts',(44.0690028814936,31.8470560938957,47.0325435728334));
#35001=CARTESIAN_POINT('Ctrl Pts',(44.1031349884786,31.8425932816639,47.0914264158325));
#35002=CARTESIAN_POINT('Ctrl Pts',(44.1341019109925,31.8381304694322,47.1520394271205));
#35003=CARTESIAN_POINT('Ctrl Pts',(44.1617475480732,31.8336676572004,47.2140050039865));
#35004=CARTESIAN_POINT('Ctrl Pts',(44.174047567796,31.8316820752328,47.2415745555713));
#35005=CARTESIAN_POINT('Ctrl Pts',(44.1856907859411,31.8296964932652,47.2694116151986));
#35006=CARTESIAN_POINT('Ctrl Pts',(44.1966666295966,31.8277109112976,47.2974819724776));
#35007=CARTESIAN_POINT('Ctrl Pts',(44.221315821241,31.8232517560854,47.3605214651867));
#35008=CARTESIAN_POINT('Ctrl Pts',(44.2426914939263,31.8187926008732,47.4249833216754));
#35009=CARTESIAN_POINT('Ctrl Pts',(44.2606307944358,31.814333445661,47.4904947461534));
#35010=CARTESIAN_POINT('Ctrl Pts',(44.2785433129736,31.8098809476185,47.5559083672021));
#35011=CARTESIAN_POINT('Ctrl Pts',(44.2930295119248,31.805428449576,47.622367974857));
#35012=CARTESIAN_POINT('Ctrl Pts',(44.303975115198,31.8009759515335,47.6894821782782));
#35013=CARTESIAN_POINT('Ctrl Pts',(44.3149080885458,31.7965285911446,47.756518939885));
#35014=CARTESIAN_POINT('Ctrl Pts',(44.3223085006713,31.7920812307556,47.8242083130688));
#35015=CARTESIAN_POINT('Ctrl Pts',(44.3261127378193,31.7876338703667,47.8921469605884));
#35016=CARTESIAN_POINT('Ctrl Pts',(44.3299146448619,31.7831892339979,47.9600439955047));
#35017=CARTESIAN_POINT('Ctrl Pts',(44.3301247188218,31.7787445976292,48.0281895108933));
#35018=CARTESIAN_POINT('Ctrl Pts',(44.3267311582565,31.7742999612604,48.0961748444436));
#35019=CARTESIAN_POINT('Ctrl Pts',(44.323338508612,31.7698565179488,48.164141928944));
#35020=CARTESIAN_POINT('Ctrl Pts',(44.3163441693474,31.7654130746372,48.2319484249721));
#35021=CARTESIAN_POINT('Ctrl Pts',(44.3057884235369,31.7609696313256,48.299187301891));
#35022=CARTESIAN_POINT('Ctrl Pts',(44.2952318793074,31.7565258519194,48.3664312646459));
#35023=CARTESIAN_POINT('Ctrl Pts',(44.2811134727428,31.7520820725132,48.4331070366154));
#35024=CARTESIAN_POINT('Ctrl Pts',(44.2635248878602,31.747638293107,48.4988161477195));
#35025=CARTESIAN_POINT('Ctrl Pts',(44.2459171715654,31.7431896801241,48.5645967317758));
#35026=CARTESIAN_POINT('Ctrl Pts',(44.2248318721696,31.7387410671411,48.6294080797517));
#35027=CARTESIAN_POINT('Ctrl Pts',(44.2004107481887,31.7342924541581,48.6928662891976));
#35028=CARTESIAN_POINT('Ctrl Pts',(44.1759746161275,31.7298411072657,48.7563634970905));
#35029=CARTESIAN_POINT('Ctrl Pts',(44.1481987808603,31.7253897603733,48.8185054616234));
#35030=CARTESIAN_POINT('Ctrl Pts',(44.1172722746545,31.7209384134809,48.8789303110048));
#35031=CARTESIAN_POINT('Ctrl Pts',(44.0862919625275,31.7164793221372,48.9394602875111));
#35032=CARTESIAN_POINT('Ctrl Pts',(44.0521502870094,31.7120202307936,48.9982667608184));
#35033=CARTESIAN_POINT('Ctrl Pts',(44.015080659964,31.7075611394499,49.055015174635));
#35034=CARTESIAN_POINT('Ctrl Pts',(43.9982436001863,31.7055358159306,49.0807903580366));
#35035=CARTESIAN_POINT('Ctrl Pts',(43.9808030739588,31.7035104924113,49.106141402521));
#35036=CARTESIAN_POINT('Ctrl Pts',(43.9627836415489,31.701485168892,49.1310392772168));
#35037=CARTESIAN_POINT('Ctrl Pts',(43.9577859565441,31.700923445928,49.1379446964436));
#35038=CARTESIAN_POINT('Ctrl Pts',(43.9527424375441,31.700361722964,49.144817081284));
#35039=CARTESIAN_POINT('Ctrl Pts',(43.9476533605231,31.6998,49.1516560391721));
#35040=CARTESIAN_POINT('',(43.8578594651099,31.6998,46.7365965264851));
#35041=CARTESIAN_POINT('Origin',(42.4,31.6998,48.));
#35042=CARTESIAN_POINT('',(40.470870167032,32.0064681656139,47.9991972218753));
#35043=CARTESIAN_POINT('Ctrl Pts',(40.470870167032,32.0064681656139,47.9991972218753));
#35044=CARTESIAN_POINT('Ctrl Pts',(40.4709011975406,32.0016092260085,47.9246288223946));
#35045=CARTESIAN_POINT('Ctrl Pts',(40.475259964132,31.996750286403,47.8501996671079));
#35046=CARTESIAN_POINT('Ctrl Pts',(40.483873195406,31.9918913467975,47.7763918033335));
#35047=CARTESIAN_POINT('Ctrl Pts',(40.492513155862,31.9870173285907,47.7023548938321));
#35048=CARTESIAN_POINT('Ctrl Pts',(40.5054338919586,31.9821433103839,47.6289434528292));
#35049=CARTESIAN_POINT('Ctrl Pts',(40.5225112662355,31.9772692921771,47.5566281340821));
#35050=CARTESIAN_POINT('Ctrl Pts',(40.5396666955009,31.9723729964569,47.4839822861055));
#35051=CARTESIAN_POINT('Ctrl Pts',(40.5610166993639,31.9674767007366,47.4124429092672));
#35052=CARTESIAN_POINT('Ctrl Pts',(40.5863869842789,31.9625804050164,47.3424664372772));
#35053=CARTESIAN_POINT('Ctrl Pts',(40.6042268414166,31.9591374316148,47.29326043634));
#35054=CARTESIAN_POINT('Ctrl Pts',(40.6240535527847,31.9556944582133,47.2448268014045));
#35055=CARTESIAN_POINT('Ctrl Pts',(40.6457929214645,31.9522514848117,47.1973169476587));
#35056=CARTESIAN_POINT('Ctrl Pts',(40.6736626774029,31.9478376110779,47.1364095658451));
#35057=CARTESIAN_POINT('Ctrl Pts',(40.7047702000245,31.9434237373442,47.0768205595951));
#35058=CARTESIAN_POINT('Ctrl Pts',(40.7389679731072,31.9390098636104,47.0189214289689));
#35059=CARTESIAN_POINT('Ctrl Pts',(40.7731133247939,31.9346027558559,46.9611110512929));
#35060=CARTESIAN_POINT('Ctrl Pts',(40.8103392783329,31.9301956481014,46.9049858417072));
#35061=CARTESIAN_POINT('Ctrl Pts',(40.8504509007865,31.9257885403469,46.8508959376859));
#35062=CARTESIAN_POINT('Ctrl Pts',(40.8905162115877,31.9213865209042,46.7968684842135));
#35063=CARTESIAN_POINT('Ctrl Pts',(40.9334602813578,31.9169845014615,46.7448720758815));
#35064=CARTESIAN_POINT('Ctrl Pts',(40.9790440695699,31.9125824820188,46.6952292152736));
#35065=CARTESIAN_POINT('Ctrl Pts',(41.0246001405321,31.9081831392267,46.6456165400371));
#35066=CARTESIAN_POINT('Ctrl Pts',(41.0727924085359,31.9037837964345,46.5983549464344));
#35067=CARTESIAN_POINT('Ctrl Pts',(41.1233417319082,31.8993844536424,46.5537336955412));
#35068=CARTESIAN_POINT('Ctrl Pts',(41.1738785930472,31.8949861954471,46.5091234453974));
#35069=CARTESIAN_POINT('Ctrl Pts',(41.2267709791414,31.8905879372519,46.4671525800915));
#35070=CARTESIAN_POINT('Ctrl Pts',(41.281704532659,31.8861896790566,46.4280719467404));
#35071=CARTESIAN_POINT('Ctrl Pts',(41.3366444025176,31.8817909151431,46.3889868198405));
#35072=CARTESIAN_POINT('Ctrl Pts',(41.3936254931727,31.8773921512296,46.35279287411));
#35073=CARTESIAN_POINT('Ctrl Pts',(41.4523037936787,31.8729933873161,46.3196981052727));
#35074=CARTESIAN_POINT('Ctrl Pts',(41.5110540263297,31.8685892310766,46.2865627664514));
#35075=CARTESIAN_POINT('Ctrl Pts',(41.5715051800388,31.8641850748372,46.2565344326099));
#35076=CARTESIAN_POINT('Ctrl Pts',(41.6332888846635,31.8597809185977,46.2297749796934));
#35077=CARTESIAN_POINT('Ctrl Pts',(41.6951143419729,31.8553737860824,46.2029974430605));
#35078=CARTESIAN_POINT('Ctrl Pts',(41.7582736681009,31.8509666535671,46.1794933537636));
#35079=CARTESIAN_POINT('Ctrl Pts',(41.8223816805205,31.8465595210518,46.1593752055615));
#35080=CARTESIAN_POINT('Ctrl Pts',(41.8866147410499,31.8421437920512,46.1392178152068));
#35081=CARTESIAN_POINT('Ctrl Pts',(41.9517996925201,31.8377280630505,46.1224596681049));
#35082=CARTESIAN_POINT('Ctrl Pts',(42.0175403705868,31.8333123340499,46.1091623050169));
#35083=CARTESIAN_POINT('Ctrl Pts',(42.0537009136062,31.8308834701685,46.101848114106));
#35084=CARTESIAN_POINT('Ctrl Pts',(42.0900294839137,31.8284546062872,46.0955800777092));
#35085=CARTESIAN_POINT('Ctrl Pts',(42.1264598712172,31.8260257424059,46.0903617214652));
#35086=CARTESIAN_POINT('Ctrl Pts',(42.1951041302893,31.8214491355164,46.0805289904826));
#35087=CARTESIAN_POINT('Ctrl Pts',(42.2643926296832,31.8168725286268,46.074385533138));
#35088=CARTESIAN_POINT('Ctrl Pts',(42.3339066447597,31.8122959217373,46.072002534936));
#35089=CARTESIAN_POINT('Ctrl Pts',(42.4051024326407,31.8076085916649,46.0695618841648));
#35090=CARTESIAN_POINT('Ctrl Pts',(42.4765343220368,31.8029212615926,46.0710661782557));
#35091=CARTESIAN_POINT('Ctrl Pts',(42.5477432913384,31.7982339315202,46.0765358134957));
#35092=CARTESIAN_POINT('Ctrl Pts',(42.6170367640556,31.7936726890015,46.0818583174443));
#35093=CARTESIAN_POINT('Ctrl Pts',(42.6861186630357,31.7891114464829,46.0909354908467));
#35094=CARTESIAN_POINT('Ctrl Pts',(42.7545645738241,31.7845502039642,46.1037335314126));
#35095=CARTESIAN_POINT('Ctrl Pts',(42.8229452737836,31.7799933071019,46.1165193788347));
#35096=CARTESIAN_POINT('Ctrl Pts',(42.8906907376217,31.7754364102396,46.1330189646288));
#35097=CARTESIAN_POINT('Ctrl Pts',(42.957383288383,31.7708795133773,46.1531468854477));
#35098=CARTESIAN_POINT('Ctrl Pts',(43.0240307330039,31.7663256984788,46.1732611931598));
#35099=CARTESIAN_POINT('Ctrl Pts',(43.0896262391683,31.7617718835803,46.1969988247196));
#35100=CARTESIAN_POINT('Ctrl Pts',(43.1537653134501,31.7572180686819,46.2242239980393));
#35101=CARTESIAN_POINT('Ctrl Pts',(43.2211582915429,31.752433229625,46.252830358977));
#35102=CARTESIAN_POINT('Ctrl Pts',(43.2869426173446,31.7476483905682,46.2852873672686));
#35103=CARTESIAN_POINT('Ctrl Pts',(43.3506717289978,31.7428635515114,46.3213797866747));
#35104=CARTESIAN_POINT('Ctrl Pts',(43.4113091777405,31.7383108372883,46.3557212701029));
#35105=CARTESIAN_POINT('Ctrl Pts',(43.4700857694018,31.7337581230652,46.393353355447));
#35106=CARTESIAN_POINT('Ctrl Pts',(43.5266429201655,31.7292054088421,46.4340439701764));
#35107=CARTESIAN_POINT('Ctrl Pts',(43.5832059084648,31.7246522247115,46.4747387847798));
#35108=CARTESIAN_POINT('Ctrl Pts',(43.6375486304879,31.7200990405808,46.5184924801764));
#35109=CARTESIAN_POINT('Ctrl Pts',(43.6893437163278,31.7155458564502,46.565031241432));
#35110=CARTESIAN_POINT('Ctrl Pts',(43.7411749505203,31.7109894946029,46.6116024825943));
#35111=CARTESIAN_POINT('Ctrl Pts',(43.7904546638894,31.7064331327557,46.6609623523788));
#35112=CARTESIAN_POINT('Ctrl Pts',(43.8368913921465,31.7018767709084,46.7127992836875));
#35113=CARTESIAN_POINT('Ctrl Pts',(43.8439466151188,31.7011845139389,46.7206749700744));
#35114=CARTESIAN_POINT('Ctrl Pts',(43.8509362865415,31.7004922569695,46.7286077710193));
#35115=CARTESIAN_POINT('Ctrl Pts',(43.8578594651099,31.6998,46.7365965264851));
#35116=CARTESIAN_POINT('Ctrl Pts',(40.4708701307726,32.004994408738,47.9992896799358));
#35117=CARTESIAN_POINT('Ctrl Pts',(40.4708627806638,32.006246742668,48.019251546574));
#35118=CARTESIAN_POINT('Ctrl Pts',(40.4711652667494,32.0075076083347,48.0392118611536));
#35119=CARTESIAN_POINT('Ctrl Pts',(40.4722595512005,32.0097780261629,48.0748761664676));
#35120=CARTESIAN_POINT('Ctrl Pts',(40.4729336918832,32.0107839605529,48.0905820021913));
#35121=CARTESIAN_POINT('Ctrl Pts',(40.4742865346698,32.0123646478213,48.1151012709811));
#35122=CARTESIAN_POINT('Ctrl Pts',(40.4748340034472,32.012935338653,48.1239214856286));
#35123=CARTESIAN_POINT('Ctrl Pts',(40.4760361467134,32.0140673468661,48.1413513319663));
#35124=CARTESIAN_POINT('Ctrl Pts',(40.4766880604071,32.0146285658266,48.1499609509146));
#35125=CARTESIAN_POINT('Ctrl Pts',(40.4782001442076,32.0158281715614,48.1682948913855));
#35126=CARTESIAN_POINT('Ctrl Pts',(40.4790763729743,32.016467042734,48.1780176099576));
#35127=CARTESIAN_POINT('Ctrl Pts',(40.4815310931312,32.0181238404701,48.2031223876356));
#35128=CARTESIAN_POINT('Ctrl Pts',(40.4832207742616,32.01914519036,48.2184926253707));
#35129=CARTESIAN_POINT('Ctrl Pts',(40.4908944015245,32.0233503744575,48.2813314655605));
#35130=CARTESIAN_POINT('Ctrl Pts',(40.4984580254018,32.0265824797393,48.3285864122701));
#35131=CARTESIAN_POINT('Ctrl Pts',(40.5385013013827,32.0406916259529,48.5303692624794));
#35132=CARTESIAN_POINT('Ctrl Pts',(40.5881266008019,32.0520648312043,48.6808605516744));
#35133=CARTESIAN_POINT('Ctrl Pts',(40.6737664730247,32.0662119589922,48.8622577614324));
#35134=CARTESIAN_POINT('Ctrl Pts',(40.6933016176098,32.069201237967,48.9003064586181));
#35135=CARTESIAN_POINT('Ctrl Pts',(40.7224301145485,32.0733186864852,48.9526786002534));
#35136=CARTESIAN_POINT('Ctrl Pts',(40.7309741434781,32.0744896615469,48.967569103407));
#35137=CARTESIAN_POINT('Ctrl Pts',(40.7463153549934,32.0765266631546,48.9934976615909));
#35138=CARTESIAN_POINT('Ctrl Pts',(40.7530270446214,32.0773970370017,49.0045847971862));
#35139=CARTESIAN_POINT('Ctrl Pts',(40.7632177908763,32.0786870647035,49.021042347508));
#35140=CARTESIAN_POINT('Ctrl Pts',(40.7666125005188,32.079111738868,49.0264642004913));
#35141=CARTESIAN_POINT('Ctrl Pts',(40.7724859266638,32.079837752799,49.0357420084307));
#35142=CARTESIAN_POINT('Ctrl Pts',(40.7749515128934,32.0801399266426,49.0396061673923));
#35143=CARTESIAN_POINT('Ctrl Pts',(40.7805996582828,32.0808262099835,49.0483889592649));
#35144=CARTESIAN_POINT('Ctrl Pts',(40.7837908817173,32.0812097457134,49.0533019343326));
#35145=CARTESIAN_POINT('Ctrl Pts',(40.7926643282636,32.0822648566423,49.066827566897));
#35146=CARTESIAN_POINT('Ctrl Pts',(40.7983934424351,32.082933435362,49.0754094407244));
#35147=CARTESIAN_POINT('Ctrl Pts',(40.8297882516345,32.0865318647349,49.1216295926669));
#35148=CARTESIAN_POINT('Ctrl Pts',(40.8567143551735,32.0893859367888,49.1583989078264));
#35149=CARTESIAN_POINT('Ctrl Pts',(40.9936490432383,32.1030102574597,49.3321302540539));
#35150=CARTESIAN_POINT('Ctrl Pts',(41.1207104482148,32.1131255583394,49.4545860986199));
#35151=CARTESIAN_POINT('Ctrl Pts',(41.29172446324,32.1261562670014,49.5794202035729));
#35152=CARTESIAN_POINT('Ctrl Pts',(41.3214387021441,32.1283986821038,49.5998587870614));
#35153=CARTESIAN_POINT('Ctrl Pts',(41.3670653712595,32.1318229677713,49.6293935461119));
#35154=CARTESIAN_POINT('Ctrl Pts',(41.382564013842,32.1329829233396,49.6391159978181));
#35155=CARTESIAN_POINT('Ctrl Pts',(41.4080311090721,32.1348852155009,49.6545913889043));
#35156=CARTESIAN_POINT('Ctrl Pts',(41.4179171073616,32.1356227606144,49.6604782827849));
#35157=CARTESIAN_POINT('Ctrl Pts',(41.4370348504081,32.1370476868972,49.6716320262033));
#35158=CARTESIAN_POINT('Ctrl Pts',(41.4462586410076,32.1377345776486,49.6769117219052));
#35159=CARTESIAN_POINT('Ctrl Pts',(41.4631418143845,32.1389910156643,49.6863912933081));
#35160=CARTESIAN_POINT('Ctrl Pts',(41.4707870415153,32.1395596585546,49.6906159018776));
#35161=CARTESIAN_POINT('Ctrl Pts',(41.4874912159891,32.1408015587082,49.6996987792366));
#35162=CARTESIAN_POINT('Ctrl Pts',(41.4965607920905,32.1414755120483,49.7045368320232));
#35163=CARTESIAN_POINT('Ctrl Pts',(41.5212500645083,32.1433094770585,49.7174546159945));
#35164=CARTESIAN_POINT('Ctrl Pts',(41.5369419645521,32.1444743813436,49.7253934622963));
#35165=CARTESIAN_POINT('Ctrl Pts',(41.6200254063973,32.150640158119,49.7660100611101));
#35166=CARTESIAN_POINT('Ctrl Pts',(41.6891609547765,32.1557676430686,49.7949532734779));
#35167=CARTESIAN_POINT('Ctrl Pts',(41.7712093451674,32.1618454763861,49.8238177671504));
#35168=CARTESIAN_POINT('Ctrl Pts',(41.7826573950548,32.1626932439883,49.8277245182302));
#35169=CARTESIAN_POINT('Ctrl Pts',(41.7941388784248,32.1635431008229,49.8315225519397));
#35170=CARTESIAN_POINT('Origin',(42.4,31.6998,48.));
#35171=CARTESIAN_POINT('',(40.2836156024077,31.6998,46.9479032732073));
#35172=CARTESIAN_POINT('Origin',(42.4,31.6998,48.));
#35173=CARTESIAN_POINT('Ctrl Pts',(40.2836156024078,31.6998,46.9479032732073));
#35174=CARTESIAN_POINT('Ctrl Pts',(40.3278926679427,31.6998,46.8769610634086));
#35175=CARTESIAN_POINT('Ctrl Pts',(40.3762433003066,31.6998,46.8085972732121));
#35176=CARTESIAN_POINT('Ctrl Pts',(40.4283168746136,31.6998,46.7430091960712));
#35177=CARTESIAN_POINT('Ctrl Pts',(40.4725499800367,31.6998,46.6872964018317));
#35178=CARTESIAN_POINT('Ctrl Pts',(40.5194704001647,31.6998,46.6335868254742));
#35179=CARTESIAN_POINT('Ctrl Pts',(40.5688802061001,31.6998,46.5820255156089));
#35180=CARTESIAN_POINT('Ctrl Pts',(40.5804814395833,31.6998,46.5699191172306));
#35181=CARTESIAN_POINT('Ctrl Pts',(40.5922183828339,31.6998,46.5579330154579));
#35182=CARTESIAN_POINT('Ctrl Pts',(40.6040806009517,31.6998,46.5460766914988));
#35183=CARTESIAN_POINT('Ctrl Pts',(40.6628239074511,31.6998,46.4873625736696));
#35184=CARTESIAN_POINT('Ctrl Pts',(40.7246897231953,31.6998,46.4317723406803));
#35185=CARTESIAN_POINT('Ctrl Pts',(40.7893476148646,31.6998,46.3795180785659));
#35186=CARTESIAN_POINT('Ctrl Pts',(40.8357795880102,31.6998,46.3419933707134));
#35187=CARTESIAN_POINT('Ctrl Pts',(40.8836521335364,31.6998,46.3061898568887));
#35188=CARTESIAN_POINT('Ctrl Pts',(40.9328489705532,31.6998,46.2722015277962));
#35189=CARTESIAN_POINT('Ctrl Pts',(40.9448895535959,31.6998,46.2638831210909));
#35190=CARTESIAN_POINT('Ctrl Pts',(40.9570094754657,31.6998,46.2556735073344));
#35191=CARTESIAN_POINT('Ctrl Pts',(40.9692070552756,31.6998,46.2475741931581));
#35192=CARTESIAN_POINT('Ctrl Pts',(40.9813625143741,31.6998,46.2395028475525));
#35193=CARTESIAN_POINT('Ctrl Pts',(40.9935877226732,31.6998,46.2315459621755));
#35194=CARTESIAN_POINT('Ctrl Pts',(41.0058778593767,31.6998,46.2237064435508));
#35195=CARTESIAN_POINT('Ctrl Pts',(41.0743104083663,31.6998,46.1800553227145));
#35196=CARTESIAN_POINT('Ctrl Pts',(41.1447837982158,31.6998,46.1400195296668));
#35197=CARTESIAN_POINT('Ctrl Pts',(41.2169884141849,31.6998,46.1037900354922));
#35198=CARTESIAN_POINT('Ctrl Pts',(41.2875858943175,31.6998,46.0683669401558));
#35199=CARTESIAN_POINT('Ctrl Pts',(41.3598393097106,31.6998,46.0365823804477));
#35200=CARTESIAN_POINT('Ctrl Pts',(41.4334713794664,31.6998,46.0086619738273));
#35201=CARTESIAN_POINT('Ctrl Pts',(41.5055827727076,31.6998,45.9813181896864));
#35202=CARTESIAN_POINT('Ctrl Pts',(41.5790172237879,31.6998,45.9576804264826));
#35203=CARTESIAN_POINT('Ctrl Pts',(41.6535138228268,31.6998,45.9380090899685));
#35204=CARTESIAN_POINT('Ctrl Pts',(41.6874584785425,31.6998,45.9290457714539));
#35205=CARTESIAN_POINT('Ctrl Pts',(41.7216235827886,31.6998,45.9209066525431));
#35206=CARTESIAN_POINT('Ctrl Pts',(41.7559837827323,31.6998,45.9136199602272));
#35207=CARTESIAN_POINT('Ctrl Pts',(41.7681538566628,31.6998,45.9110390793144));
#35208=CARTESIAN_POINT('Ctrl Pts',(41.7803434987159,31.6998,45.9085662449037));
#35209=CARTESIAN_POINT('Ctrl Pts',(41.7925438080729,31.6998,45.9062038693017));
#35210=CARTESIAN_POINT('Ctrl Pts',(41.8673941835534,31.6998,45.8917104088767));
#35211=CARTESIAN_POINT('Ctrl Pts',(41.9427350306394,31.6998,45.8813514036828));
#35212=CARTESIAN_POINT('Ctrl Pts',(42.0183083661715,31.6998,45.8753295077184));
#35213=CARTESIAN_POINT('Ctrl Pts',(42.0438483937305,31.6998,45.8732944064779));
#35214=CARTESIAN_POINT('Ctrl Pts',(42.069414977119,31.6998,45.8717550820673));
#35215=CARTESIAN_POINT('Ctrl Pts',(42.0949980865043,31.6998,45.8707207179083));
#35216=CARTESIAN_POINT('Ctrl Pts',(42.1725910153043,31.6998,45.8675835173696));
#35217=CARTESIAN_POINT('Ctrl Pts',(42.2503372664716,31.6998,45.8690877185585));
#35218=CARTESIAN_POINT('Ctrl Pts',(42.3278997019256,31.6998,45.87507693665));
#35219=CARTESIAN_POINT('Ctrl Pts',(42.4026205805095,31.6998,45.8808467353317));
#35220=CARTESIAN_POINT('Ctrl Pts',(42.4771715618792,31.6998,45.8907797086975));
#35221=CARTESIAN_POINT('Ctrl Pts',(42.5512293212772,31.6998,45.9047761999135));
#35222=CARTESIAN_POINT('Ctrl Pts',(42.5694631410037,31.6998,45.9082222871258));
#35223=CARTESIAN_POINT('Ctrl Pts',(42.5876734448574,31.6998,45.9119164301344));
#35224=CARTESIAN_POINT('Ctrl Pts',(42.6058197878003,31.6998,45.9158493587107));
#35225=CARTESIAN_POINT('Ctrl Pts',(42.6799748837184,31.6998,45.9319212855299));
#35226=CARTESIAN_POINT('Ctrl Pts',(42.7531518432347,31.6998,45.9519905284711));
#35227=CARTESIAN_POINT('Ctrl Pts',(42.82504465412,31.6998,45.9758841810461));
#35228=CARTESIAN_POINT('Ctrl Pts',(42.8966173594445,31.6998,45.9996714461958));
#35229=CARTESIAN_POINT('Ctrl Pts',(42.966918187902,31.6998,46.027249759349));
#35230=CARTESIAN_POINT('Ctrl Pts',(43.0356198557269,31.6998,46.0584926500212));
#35231=CARTESIAN_POINT('Ctrl Pts',(43.1037385474373,31.6998,46.0894704254554));
#35232=CARTESIAN_POINT('Ctrl Pts',(43.1702858755638,31.6998,46.1240514433707));
#35233=CARTESIAN_POINT('Ctrl Pts',(43.2349057444967,31.6998,46.162146870017));
#35234=CARTESIAN_POINT('Ctrl Pts',(43.2584962714637,31.6998,46.1760542208745));
#35235=CARTESIAN_POINT('Ctrl Pts',(43.2818295034026,31.6998,46.1904302386159));
#35236=CARTESIAN_POINT('Ctrl Pts',(43.3048865617406,31.6998,46.2052715243424));
#35237=CARTESIAN_POINT('Ctrl Pts',(43.3148243102554,31.6998,46.2116682191429));
#35238=CARTESIAN_POINT('Ctrl Pts',(43.3247094403455,31.6998,46.2181505929569));
#35239=CARTESIAN_POINT('Ctrl Pts',(43.3345306217168,31.6998,46.2247115366551));
#35240=CARTESIAN_POINT('Ctrl Pts',(43.3953085048616,31.6998,46.2653136041996));
#35241=CARTESIAN_POINT('Ctrl Pts',(43.4537463558528,31.6998,46.308989429215));
#35242=CARTESIAN_POINT('Ctrl Pts',(43.5095482320819,31.6998,46.3556161784622));
#35243=CARTESIAN_POINT('Ctrl Pts',(43.5644246533789,31.6998,46.401469639104));
#35244=CARTESIAN_POINT('Ctrl Pts',(43.6167524175643,31.6998,46.4501775666));
#35245=CARTESIAN_POINT('Ctrl Pts',(43.6662103729083,31.6998,46.501653076856));
#35246=CARTESIAN_POINT('Ctrl Pts',(43.7140843356336,31.6998,46.5514799781526));
#35247=CARTESIAN_POINT('Ctrl Pts',(43.7592697324565,31.6998,46.6039005799531));
#35248=CARTESIAN_POINT('Ctrl Pts',(43.8014309498606,31.6998,46.6588558401277));
#35249=CARTESIAN_POINT('Ctrl Pts',(43.8208980948003,31.6998,46.6842303924031));
#35250=CARTESIAN_POINT('Ctrl Pts',(43.8397198334818,31.6998,46.710145554351));
#35251=CARTESIAN_POINT('Ctrl Pts',(43.8578594651099,31.6998,46.7365965264851));
#35252=CARTESIAN_POINT('Ctrl Pts',(43.9504717140164,31.6998,49.1537532619121));
#35253=CARTESIAN_POINT('Ctrl Pts',(43.91517156945,31.6998,49.2142805813239));
#35254=CARTESIAN_POINT('Ctrl Pts',(43.876313406039,31.6998,49.2725892970532));
#35255=CARTESIAN_POINT('Ctrl Pts',(43.8342551647323,31.6998,49.3285785621835));
#35256=CARTESIAN_POINT('Ctrl Pts',(43.7956027712495,31.6998,49.3800338546398));
#35257=CARTESIAN_POINT('Ctrl Pts',(43.7542466023904,31.6998,49.4295303540662));
#35258=CARTESIAN_POINT('Ctrl Pts',(43.710427710391,31.6998,49.4769775792939));
#35259=CARTESIAN_POINT('Ctrl Pts',(43.6962200999558,31.6998,49.4923616216899));
#35260=CARTESIAN_POINT('Ctrl Pts',(43.6817503327117,31.6998,49.5075329290985));
#35261=CARTESIAN_POINT('Ctrl Pts',(43.6670459663506,31.6998,49.5224684275058));
#35262=CARTESIAN_POINT('Ctrl Pts',(43.6155359597312,31.6998,49.5747880992909));
#35263=CARTESIAN_POINT('Ctrl Pts',(43.5611098000689,31.6998,49.6242627199654));
#35264=CARTESIAN_POINT('Ctrl Pts',(43.5041269281797,31.6998,49.6707695142619));
#35265=CARTESIAN_POINT('Ctrl Pts',(43.4585949524133,31.6998,49.707930614794));
#35266=CARTESIAN_POINT('Ctrl Pts',(43.4114293717005,31.6998,49.7431966047481));
#35267=CARTESIAN_POINT('Ctrl Pts',(43.3627930380821,31.6998,49.776492738111));
#35268=CARTESIAN_POINT('Ctrl Pts',(43.3508526583872,31.6998,49.784667048244));
#35269=CARTESIAN_POINT('Ctrl Pts',(43.3388230033905,31.6998,49.7927228207283));
#35270=CARTESIAN_POINT('Ctrl Pts',(43.3267198102625,31.6998,49.8006503503805));
#35271=CARTESIAN_POINT('Ctrl Pts',(43.2630423735884,31.6998,49.8423587460136));
#35272=CARTESIAN_POINT('Ctrl Pts',(43.1972476615927,31.6998,49.8805790577778));
#35273=CARTESIAN_POINT('Ctrl Pts',(43.1297134118621,31.6998,49.91518907178));
#35274=CARTESIAN_POINT('Ctrl Pts',(43.0621791621316,31.6998,49.9497990857822));
#35275=CARTESIAN_POINT('Ctrl Pts',(42.9929045405879,31.6998,49.9807994335801));
#35276=CARTESIAN_POINT('Ctrl Pts',(42.9222254461525,31.6998,50.0080367038729));
#35277=CARTESIAN_POINT('Ctrl Pts',(42.8709659946502,31.6998,50.0277903176789));
#35278=CARTESIAN_POINT('Ctrl Pts',(42.8189669079838,31.6998,50.04556403106));
#35279=CARTESIAN_POINT('Ctrl Pts',(42.7663463649455,31.6998,50.0612861622637));
#35280=CARTESIAN_POINT('Ctrl Pts',(42.7262965849615,31.6998,50.0732523613797));
#35281=CARTESIAN_POINT('Ctrl Pts',(42.6858866223729,31.6998,50.0840299036639));
#35282=CARTESIAN_POINT('Ctrl Pts',(42.6451663824038,31.6998,50.0935820856434));
#35283=CARTESIAN_POINT('Ctrl Pts',(42.6267637139364,31.6998000000001,50.0978989963061));
#35284=CARTESIAN_POINT('Ctrl Pts',(42.6082907905384,31.6998,50.1019668307642));
#35285=CARTESIAN_POINT('Ctrl Pts',(42.5897891748184,31.6998,50.1057747222131));
#35286=CARTESIAN_POINT('Ctrl Pts',(42.5127566104579,31.6998,50.1216291020441));
#35287=CARTESIAN_POINT('Ctrl Pts',(42.4351379902024,31.6998000000001,50.1330052928323));
#35288=CARTESIAN_POINT('Ctrl Pts',(42.3572965076711,31.6998,50.1397510062613));
#35289=CARTESIAN_POINT('Ctrl Pts',(42.33214112474,31.6998,50.1419309622299));
#35290=CARTESIAN_POINT('Ctrl Pts',(42.3069622193782,31.6998,50.1436270192556));
#35291=CARTESIAN_POINT('Ctrl Pts',(42.2817714200905,31.6998,50.1448330571849));
#35292=CARTESIAN_POINT('Ctrl Pts',(42.2057610810024,31.6998,50.1484721379029));
#35293=CARTESIAN_POINT('Ctrl Pts',(42.1296433545669,31.6998,50.1476538965692));
#35294=CARTESIAN_POINT('Ctrl Pts',(42.0536890631274,31.6998,50.1425994759693));
#35295=CARTESIAN_POINT('Ctrl Pts',(41.9777347716879,31.6998,50.1375450553693));
#35296=CARTESIAN_POINT('Ctrl Pts',(41.901943126711,31.6998,50.1282542163723));
#35297=CARTESIAN_POINT('Ctrl Pts',(41.8265789334743,31.6998,50.1148961512031));
#35298=CARTESIAN_POINT('Ctrl Pts',(41.8136579892345,31.6998,50.112605954655));
#35299=CARTESIAN_POINT('Ctrl Pts',(41.8007475854246,31.6998,50.1101956878563));
#35300=CARTESIAN_POINT('Ctrl Pts',(41.7878555222505,31.6998,50.1076673315445));
#35301=CARTESIAN_POINT('Ctrl Pts',(41.7108587708215,31.6998,50.0925669383931));
#35302=CARTESIAN_POINT('Ctrl Pts',(41.6347686710189,31.6998,50.07330942136));
#35303=CARTESIAN_POINT('Ctrl Pts',(41.559869491234,31.6998,50.0501532594334));
#35304=CARTESIAN_POINT('Ctrl Pts',(41.4830476814102,31.6998,50.0264026886945));
#35305=CARTESIAN_POINT('Ctrl Pts',(41.4074778770195,31.6998,49.9985506735256));
#35306=CARTESIAN_POINT('Ctrl Pts',(41.3334597411236,31.6998,49.9668200521561));
#35307=CARTESIAN_POINT('Ctrl Pts',(41.2594416052277,31.6998,49.9350894307866));
#35308=CARTESIAN_POINT('Ctrl Pts',(41.1869742146367,31.6998,49.8994798787782));
#35309=CARTESIAN_POINT('Ctrl Pts',(41.1163636595774,31.6998,49.8601622832682));
#35310=CARTESIAN_POINT('Ctrl Pts',(41.0932456719035,31.6998,49.8472896512998));
#35311=CARTESIAN_POINT('Ctrl Pts',(41.0703268321719,31.6998,49.8340191546822));
#35312=CARTESIAN_POINT('Ctrl Pts',(41.0476182929131,31.6998,49.8203556713237));
#35313=CARTESIAN_POINT('Ctrl Pts',(41.0335607423107,31.6998,49.8118973946143));
#35314=CARTESIAN_POINT('Ctrl Pts',(41.0195837865544,31.6998,49.8032885094608));
#35315=CARTESIAN_POINT('Ctrl Pts',(41.0056901258032,31.6998,49.7945300723272));
#35316=CARTESIAN_POINT('Ctrl Pts',(40.9940648543958,31.6998,49.7872016071657));
#35317=CARTESIAN_POINT('Ctrl Pts',(40.982497025284,31.6998,49.7797677651481));
#35318=CARTESIAN_POINT('Ctrl Pts',(40.9710026743328,31.6998,49.7722388696788));
#35319=CARTESIAN_POINT('Ctrl Pts',(40.901156575791,31.6998,49.7264890942377));
#35320=CARTESIAN_POINT('Ctrl Pts',(40.8338981111519,31.6998,49.6771563319653));
#35321=CARTESIAN_POINT('Ctrl Pts',(40.7695370495458,31.6998,49.6244758840085));
#35322=CARTESIAN_POINT('Ctrl Pts',(40.7050594972812,31.6998,49.5717000867843));
#35323=CARTESIAN_POINT('Ctrl Pts',(40.6434888697281,31.6998,49.51556410536));
#35324=CARTESIAN_POINT('Ctrl Pts',(40.5851503766946,31.6998,49.4562541551619));
#35325=CARTESIAN_POINT('Ctrl Pts',(40.5280447210914,31.6998,49.3981975716997));
#35326=CARTESIAN_POINT('Ctrl Pts',(40.4740352031396,31.6998,49.337099242441));
#35327=CARTESIAN_POINT('Ctrl Pts',(40.4234532661656,31.6998,49.2730923705311));
#35328=CARTESIAN_POINT('Ctrl Pts',(40.3963290195265,31.6998,49.2387690866844));
#35329=CARTESIAN_POINT('Ctrl Pts',(40.3701909267342,31.6998,49.203608761589));
#35330=CARTESIAN_POINT('Ctrl Pts',(40.3450946017473,31.6998,49.167627614067));
#35331=CARTESIAN_POINT('Ctrl Pts',(41.5114521803192,47.2275992105786,49.7083478852713));
#35332=CARTESIAN_POINT('Ctrl Pts',(40.9424693995619,47.18552396311,49.4124079226697));
#35333=CARTESIAN_POINT('Ctrl Pts',(40.1335936552416,47.1013734681727,48.2118988144355));
#35334=CARTESIAN_POINT('Ctrl Pts',(40.9966811811913,46.975147725767,46.2047778501544));
#35335=CARTESIAN_POINT('Ctrl Pts',(43.1502053828948,46.848921983361,45.8504054458902));
#35336=CARTESIAN_POINT('Ctrl Pts',(44.6139419964807,46.7226962409553,47.467111741601));
#35337=CARTESIAN_POINT('Ctrl Pts',(44.0457885266063,46.5964704985493,49.5741617337718));
#35338=CARTESIAN_POINT('Ctrl Pts',(41.966498311004,46.4702447561435,50.2355298325241));
#35339=CARTESIAN_POINT('Ctrl Pts',(40.2853083124169,46.3440190137377,48.8449325541533));
#35340=CARTESIAN_POINT('Ctrl Pts',(40.5453717036046,46.2177932713318,46.6785273809893));
#35341=CARTESIAN_POINT('Ctrl Pts',(42.5080504436644,46.091567528926,45.7253297325292));
#35342=CARTESIAN_POINT('Ctrl Pts',(44.3715194260783,45.9653417865201,46.8602812964785));
#35343=CARTESIAN_POINT('Ctrl Pts',(44.4251088775567,45.8391160441143,49.041532550479));
#35344=CARTESIAN_POINT('Ctrl Pts',(42.6196094511424,45.7128903017084,50.2666298767135));
#35345=CARTESIAN_POINT('Ctrl Pts',(40.6125070533099,45.5866645593025,49.4109270826402));
#35346=CARTESIAN_POINT('Ctrl Pts',(40.2463524779982,45.4604388168967,47.2599668519521));
#35347=CARTESIAN_POINT('Ctrl Pts',(41.8572835539691,45.3342130744908,45.7883708343257));
#35348=CARTESIAN_POINT('Ctrl Pts',(43.966437279631,45.2079873320851,46.3470874390647));
#35349=CARTESIAN_POINT('Ctrl Pts',(44.637575063142,45.081761589679,48.4232062102119));
#35350=CARTESIAN_POINT('Ctrl Pts',(43.2545807794454,44.9555358472734,50.1108143256454));
#35351=CARTESIAN_POINT('Ctrl Pts',(41.0870668303238,44.8293101048674,49.860659036887));
#35352=CARTESIAN_POINT('Ctrl Pts',(40.1248478607906,44.7030843624616,47.9023870427558));
#35353=CARTESIAN_POINT('Ctrl Pts',(41.251257290822,44.5768586200558,46.0337254241421));
#35354=CARTESIAN_POINT('Ctrl Pts',(43.4322320766004,44.4506328776498,45.9701373254779));
#35355=CARTESIAN_POINT('Ctrl Pts',(44.665600248225,44.324407135244,47.769997718258));
#35356=CARTESIAN_POINT('Ctrl Pts',(43.8191088268314,44.1981813928382,49.7810041182161));
#35357=CARTESIAN_POINT('Ctrl Pts',(41.6698513475981,44.0719556504323,50.1570184234761));
#35358=CARTESIAN_POINT('Ctrl Pts',(40.1908827592175,43.9457299080265,48.5528530996183));
#35359=CARTESIAN_POINT('Ctrl Pts',(40.7399214005723,43.8195041656206,46.4411592202193));
#35360=CARTESIAN_POINT('Ctrl Pts',(42.8129404531986,43.6932784232148,45.7605077103516));
#35361=CARTESIAN_POINT('Ctrl Pts',(44.5068731409494,43.5670526808089,47.1357482420377));
#35362=CARTESIAN_POINT('Ctrl Pts',(44.2666604230926,43.4408269384031,49.3043865983774));
#35363=CARTESIAN_POINT('Ctrl Pts',(42.3128216634364,43.3146011959972,50.2755758547758));
#35364=CARTESIAN_POINT('Ctrl Pts',(40.4390141006492,43.1883754535914,49.1577477427049));
#35365=CARTESIAN_POINT('Ctrl Pts',(40.3654249724418,43.0621497111855,46.9770874962022));
#35366=CARTESIAN_POINT('Ctrl Pts',(42.1596103511045,42.9359239687796,45.7354783397155));
#35367=CARTESIAN_POINT('Ctrl Pts',(44.1744775192528,42.8096982263738,46.5727386129868));
#35368=CARTESIAN_POINT('Ctrl Pts',(44.5603441204102,42.6834724839679,48.7202491337033));
#35369=CARTESIAN_POINT('Ctrl Pts',(42.9629780466766,42.557246741562,50.2065586899405));
#35370=CARTESIAN_POINT('Ctrl Pts',(40.848788543348,42.4310209991563,49.6672098098151));
#35371=CARTESIAN_POINT('Ctrl Pts',(40.1586375612129,42.3047952567503,47.5973339458232));
#35372=CARTESIAN_POINT('Ctrl Pts',(41.5260954492946,42.1785695143446,45.8971123735567));
#35373=CARTESIAN_POINT('Ctrl Pts',(43.6958125901134,42.0523437719386,46.1273774367225));
#35374=CARTESIAN_POINT('Ctrl Pts',(44.6759517164996,41.9261180295328,48.0767418878717));
#35375=CARTESIAN_POINT('Ctrl Pts',(43.5667284269667,41.799892287127,49.9556559796906));
#35376=CARTESIAN_POINT('Ctrl Pts',(41.3864285819795,41.6736665447211,50.0392445939032));
#35377=CARTESIAN_POINT('Ctrl Pts',(40.1366045512679,41.5474408023153,48.2507719598567));
#35378=CARTESIAN_POINT('Ctrl Pts',(40.964616068938,41.4212150599094,46.2320863981401));
#35379=CARTESIAN_POINT('Ctrl Pts',(43.1103344677488,41.2949893175036,45.8363756155191));
#35380=CARTESIAN_POINT('Ctrl Pts',(44.6039537341892,41.1687635750977,47.4269088460414));
#35381=CARTESIAN_POINT('Ctrl Pts',(44.0743059579869,41.0425378326919,49.543549510784));
#35382=CARTESIAN_POINT('Ctrl Pts',(42.0076168131093,40.916312090286,50.2431854510578));
#35383=CARTESIAN_POINT('Ctrl Pts',(40.3011421127583,40.7900863478802,48.88353896482));
#35384=CARTESIAN_POINT('Ctrl Pts',(40.5214546786603,40.6638606054743,46.7127886696953));
#35385=CARTESIAN_POINT('Ctrl Pts',(42.4663038252612,40.5376348630684,45.7237202860924));
#35386=CARTESIAN_POINT('Ctrl Pts',(44.3502849316801,40.4114091206626,46.8243154256119));
#35387=CARTESIAN_POINT('Ctrl Pts',(44.4438712739898,40.2851833782568,49.0042090163662));
#35388=CARTESIAN_POINT('Ctrl Pts',(42.6611489969678,40.1589576358509,50.2622216369255));
#35389=CARTESIAN_POINT('Ctrl Pts',(40.6386874955747,40.032731893445,49.4434762883218));
#35390=CARTESIAN_POINT('Ctrl Pts',(40.2331408534716,39.9065061510392,47.2995951368686));
#35391=CARTESIAN_POINT('Ctrl Pts',(41.8168077911319,39.7802804086334,45.79869757173));
#35392=CARTESIAN_POINT('Ctrl Pts',(43.9358551033548,39.6540546662275,46.3186331052709));
#35393=CARTESIAN_POINT('Ctrl Pts',(44.6449612880996,39.5278289238216,48.3820920676043));
#35394=CARTESIAN_POINT('Ctrl Pts',(43.2931547977007,39.4016031814158,50.0947840080867));
#35395=CARTESIAN_POINT('Ctrl Pts',(41.1214170001545,39.2753774390099,49.8844285727238));
#35396=CARTESIAN_POINT('Ctrl Pts',(40.1234401599009,39.1491516966041,47.9441356317494));
#35397=CARTESIAN_POINT('Ctrl Pts',(41.2153840033819,39.0229259541982,46.0551271317259));
#35398=CARTESIAN_POINT('Ctrl Pts',(43.3948254957311,38.8967002117924,45.9515450294831));
#35399=CARTESIAN_POINT('Ctrl Pts',(44.6610002495504,38.7704744693865,47.7284794580054));
#35400=CARTESIAN_POINT('Ctrl Pts',(43.8515382886068,38.6442487269807,49.7546743657729));
#35401=CARTESIAN_POINT('Ctrl Pts',(41.7095394713246,38.5180229845748,50.1700483385246));
#35402=CARTESIAN_POINT('Ctrl Pts',(40.2013951720587,38.391797242169,48.5932809989753));
#35403=CARTESIAN_POINT('Ctrl Pts',(40.7116075284533,38.2655714997631,46.4718716038183));
#35404=CARTESIAN_POINT('Ctrl Pts',(42.7717929127451,38.1393457573573,45.7533100874343));
#35405=CARTESIAN_POINT('Ctrl Pts',(44.4906660746539,38.0131200149514,47.0972481528774));
#35406=CARTESIAN_POINT('Ctrl Pts',(44.2902721937023,37.8868942725456,49.2699277801937));
#35407=CARTESIAN_POINT('Ctrl Pts',(42.3545762636138,37.7606685301397,50.2767920891826));
#35408=CARTESIAN_POINT('Ctrl Pts',(40.460580096709,37.6344427877339,49.193522505825));
#35409=CARTESIAN_POINT('Ctrl Pts',(40.3470044129129,37.508217045328,47.014578946545));
#35410=CARTESIAN_POINT('Ctrl Pts',(42.1181136231814,37.3819913029222,45.7402686877073));
#35411=CARTESIAN_POINT('Ctrl Pts',(44.147999325506,37.2557655605163,46.5404302376307));
#35412=CARTESIAN_POINT('Ctrl Pts',(44.5731918933992,37.1295398181104,48.6805016735148));
#35413=CARTESIAN_POINT('Ctrl Pts',(43.0033573121084,37.0033140757046,50.1958609899347));
#35414=CARTESIAN_POINT('Ctrl Pts',(40.8796304482396,36.8770883332987,49.6953825406888));
#35415=CARTESIAN_POINT('Ctrl Pts',(40.1516287118976,36.7508625908929,47.6385140610914));
#35416=CARTESIAN_POINT('Ctrl Pts',(41.487670088745,36.624636848487,45.9134958264548));
#35417=CARTESIAN_POINT('Ctrl Pts',(43.6612458533724,36.4984111060812,46.1039239386188));
#35418=CARTESIAN_POINT('Ctrl Pts',(44.6769764562741,36.3721853636753,48.0349821492397));
#35419=CARTESIAN_POINT('Ctrl Pts',(43.6024039147009,36.2459596212695,49.933926151409));
#35420=CARTESIAN_POINT('Ctrl Pts',(41.4240041126824,36.1197338788636,50.0574930282095));
#35421=CARTESIAN_POINT('Ctrl Pts',(40.1415851481607,35.9935081364578,48.2922462834413));
#35422=CARTESIAN_POINT('Ctrl Pts',(40.9324294592972,35.8672823940519,46.2587124759964));
#35423=CARTESIAN_POINT('Ctrl Pts',(43.0705285070869,35.7410566516461,45.823710254958));
#35424=CARTESIAN_POINT('Ctrl Pts',(44.5930709719577,35.6148309092402,47.386579063643));
#35425=CARTESIAN_POINT('Ctrl Pts',(44.1023369551445,35.4886051668344,49.5125787332619));
#35426=CARTESIAN_POINT('Ctrl Pts',(42.0488286371567,35.3623794244285,50.2500053793523));
#35427=CARTESIAN_POINT('Ctrl Pts',(40.3177016076886,35.2361536820227,48.9218887886614));
#35428=CARTESIAN_POINT('Ctrl Pts',(40.4981599463454,35.1099279396168,46.7474625980434));
#35429=CARTESIAN_POINT('Ctrl Pts',(42.4245398263078,34.983702197211,45.7228870624835));
#35430=CARTESIAN_POINT('Ctrl Pts',(44.3283917283527,34.8574764548051,46.7887399635747));
#35431=CARTESIAN_POINT('Ctrl Pts',(44.4619471989263,34.7312507123993,48.9665501954546));
#35432=CARTESIAN_POINT('Ctrl Pts',(42.7026000447332,34.6050249699934,50.2570508960347));
#35433=CARTESIAN_POINT('Ctrl Pts',(40.6654608961038,34.4787992275875,49.475540455032));
#35434=CARTESIAN_POINT('Ctrl Pts',(40.2206581746343,34.3525734851817,47.3394587614941));
#35435=CARTESIAN_POINT('Ctrl Pts',(41.7765283340811,34.2263477427758,45.8097651660685));
#35436=CARTESIAN_POINT('Ctrl Pts',(43.9047561161392,34.10012200037,46.2907444338171));
#35437=CARTESIAN_POINT('Ctrl Pts',(44.6515921288771,33.9738962579641,48.3408493965467));
#35438=CARTESIAN_POINT('Ctrl Pts',(43.3314283241735,33.8476705155583,50.0780488291867));
#35439=CARTESIAN_POINT('Ctrl Pts',(41.1561972997618,33.7214447731524,49.9075640298549));
#35440=CARTESIAN_POINT('Ctrl Pts',(40.12279865113,33.5952190307466,47.9859030514586));
#35441=CARTESIAN_POINT('Ctrl Pts',(41.1799089551562,33.4689932883407,46.0771831726539));
#35442=CARTESIAN_POINT('Ctrl Pts',(43.3570848922405,33.3427675459349,45.9336421471489));
#35443=CARTESIAN_POINT('Ctrl Pts',(44.6556380509762,33.216541803529,47.6870522535155));
#35444=CARTESIAN_POINT('Ctrl Pts',(43.8834821652962,33.0903160611232,49.7277548104157));
#35445=CARTESIAN_POINT('Ctrl Pts',(41.7494543021213,32.9640903187173,50.1823468710386));
#35446=CARTESIAN_POINT('Ctrl Pts',(40.2126585350139,32.8378645763115,48.6335116728557));
#35447=CARTESIAN_POINT('Ctrl Pts',(40.6838395690534,32.7116388339056,46.503093397757));
#35448=CARTESIAN_POINT('Ctrl Pts',(42.7305643873577,32.5854130914998,45.7468779126706));
#35449=CARTESIAN_POINT('Ctrl Pts',(44.4736678592443,32.4591873490939,47.0590329676311));
#35450=CARTESIAN_POINT('Ctrl Pts',(44.3134222176753,32.332961606688,49.2350791291602));
#35451=CARTESIAN_POINT('Ctrl Pts',(42.3959996514303,32.2067358642822,50.2771677709232));
#35452=CARTESIAN_POINT('Ctrl Pts',(40.4834883240295,32.0805101218763,49.2290434733774));
#35453=CARTESIAN_POINT('Ctrl Pts',(40.3278918291434,31.9542843794705,47.052110764494));
#35454=CARTESIAN_POINT('Ctrl Pts',(42.079842082062,31.8280415161295,45.7461934776559));
#35455=CARTESIAN_POINT('Ctrl Pts',(43.4357287145305,31.7438739002569,46.2544404205575));
#35456=CARTESIAN_POINT('Ctrl Pts',(43.8557111658903,31.701781531853,46.7394942770224));
#35457=CARTESIAN_POINT('Ctrl Pts',(41.4436260057576,47.1427351163746,49.8387524614932));
#35458=CARTESIAN_POINT('Ctrl Pts',(40.8312106437082,47.1006598689058,49.5202222959576));
#35459=CARTESIAN_POINT('Ctrl Pts',(39.9605903919818,47.0165093739687,48.2280738425644));
#35460=CARTESIAN_POINT('Ctrl Pts',(40.8895606131567,46.8902836315629,46.067741836768));
#35461=CARTESIAN_POINT('Ctrl Pts',(43.2074713624294,46.764057889157,45.6863188630025));
#35462=CARTESIAN_POINT('Ctrl Pts',(44.7829404600371,46.6378321467512,47.4264343900444));
#35463=CARTESIAN_POINT('Ctrl Pts',(44.1714177132687,46.5116064043452,49.6943233797499));
#35464=CARTESIAN_POINT('Ctrl Pts',(41.9334075075836,46.3853806619395,50.4061761762548));
#35465=CARTESIAN_POINT('Ctrl Pts',(40.1238859957233,46.2591549195336,48.909429412557));
#35466=CARTESIAN_POINT('Ctrl Pts',(40.4038009971191,46.1329291771276,46.5776544391508));
#35467=CARTESIAN_POINT('Ctrl Pts',(42.5162983376901,46.0067034347219,45.5516956531759));
#35468=CARTESIAN_POINT('Ctrl Pts',(44.5220128691805,45.8804776923159,46.7732823100154));
#35469=CARTESIAN_POINT('Ctrl Pts',(44.5796930036929,45.7542519499102,49.1210366210712));
#35470=CARTESIAN_POINT('Ctrl Pts',(42.6363730609772,45.6280262075043,50.4396502030025));
#35471=CARTESIAN_POINT('Ctrl Pts',(40.4760610388754,45.5018004650984,49.5186284178764));
#35472=CARTESIAN_POINT('Ctrl Pts',(40.0819565169301,45.3755747226925,47.2034773571056));
#35473=CARTESIAN_POINT('Ctrl Pts',(41.8158559801338,45.2493489802868,45.619548917785));
#35474=CARTESIAN_POINT('Ctrl Pts',(44.0860092891672,45.1231232378808,46.2209144482476));
#35475=CARTESIAN_POINT('Ctrl Pts',(44.8083775269665,44.996897495475,48.4555111212743));
#35476=CARTESIAN_POINT('Ctrl Pts',(43.31981412293,44.8706717530692,50.2719406688171));
#35477=CARTESIAN_POINT('Ctrl Pts',(40.9868457365551,44.7444460106634,50.0026900923241));
#35478=CARTESIAN_POINT('Ctrl Pts',(39.9511769983675,44.6182202682575,47.8949358810616));
#35479=CARTESIAN_POINT('Ctrl Pts',(41.1635694682946,44.4919945258517,45.8836323400513));
#35480=CARTESIAN_POINT('Ctrl Pts',(43.5110262072764,44.3657687834457,45.8151903242601));
#35481=CARTESIAN_POINT('Ctrl Pts',(44.8385419791249,44.23954304104,47.7524407848375));
#35482=CARTESIAN_POINT('Ctrl Pts',(43.9274347051677,44.1133172986341,49.9169548161318));
#35483=CARTESIAN_POINT('Ctrl Pts',(41.6141163732311,43.9870915562282,50.321671698047));
#35484=CARTESIAN_POINT('Ctrl Pts',(40.0222525872881,43.8608658138223,48.595054442091));
#35485=CARTESIAN_POINT('Ctrl Pts',(40.6132013992659,43.7346400714165,46.3221670798963));
#35486=CARTESIAN_POINT('Ctrl Pts',(42.8444617406766,43.6084143290108,45.5895588974655));
#35487=CARTESIAN_POINT('Ctrl Pts',(44.6676986387696,43.4821885866047,47.0697766766335));
#35488=CARTESIAN_POINT('Ctrl Pts',(44.4091495867591,43.355962844199,49.4039553004303));
#35489=CARTESIAN_POINT('Ctrl Pts',(42.306167015321,43.229737101793,50.4492790609911));
#35490=CARTESIAN_POINT('Ctrl Pts',(40.2893247209937,43.1035113593872,49.2461229530827));
#35491=CARTESIAN_POINT('Ctrl Pts',(40.2101182597121,42.9772856169814,46.899004763335));
#35492=CARTESIAN_POINT('Ctrl Pts',(42.1412605111437,42.8510598745756,45.5626189414625));
#35493=CARTESIAN_POINT('Ctrl Pts',(44.309930017487,42.7248341321696,46.4637904192753));
#35494=CARTESIAN_POINT('Ctrl Pts',(44.7252512578526,42.5986083897639,48.7752284408247));
#35495=CARTESIAN_POINT('Ctrl Pts',(43.0059522641835,42.472382647358,50.374993558126));
#35496=CARTESIAN_POINT('Ctrl Pts',(40.7303787777615,42.3461569049521,49.7944741630515));
#35497=CARTESIAN_POINT('Ctrl Pts',(39.9875459928562,42.2199311625463,47.5665969416062));
#35498=CARTESIAN_POINT('Ctrl Pts',(41.459387050159,42.0937054201404,45.7365911049481));
#35499=CARTESIAN_POINT('Ctrl Pts',(43.794726806084,41.9674796777346,45.9844331606221));
#35500=CARTESIAN_POINT('Ctrl Pts',(44.8496836136446,41.8412539353288,48.0825998828696));
#35501=CARTESIAN_POINT('Ctrl Pts',(43.6557891665248,41.7150281929229,50.1049385066667));
#35502=CARTESIAN_POINT('Ctrl Pts',(41.3090588890865,41.5888024505171,50.194907752077));
#35503=CARTESIAN_POINT('Ctrl Pts',(39.96383112095,41.4625767081111,48.2699143204002));
#35504=CARTESIAN_POINT('Ctrl Pts',(40.8550478510946,41.3363509657054,46.0971349482422));
#35505=CARTESIAN_POINT('Ctrl Pts',(43.1645569513782,41.2101252232995,45.6712180832658));
#35506=CARTESIAN_POINT('Ctrl Pts',(44.7721897563704,41.0838994808936,47.3831626572747));
#35507=CARTESIAN_POINT('Ctrl Pts',(44.2021119867235,40.9576737384876,49.6613744114186));
#35508=CARTESIAN_POINT('Ctrl Pts',(41.9776647385675,40.831447996082,50.4144161767515));
#35509=CARTESIAN_POINT('Ctrl Pts',(40.1409284491974,40.705222253676,48.9509827947776));
#35510=CARTESIAN_POINT('Ctrl Pts',(40.3780582963104,40.5789965112702,46.6145310200189));
#35511=CARTESIAN_POINT('Ctrl Pts',(42.4713650439449,40.4527707688644,45.5499633516799));
#35512=CARTESIAN_POINT('Ctrl Pts',(44.4991574664958,40.3265450264584,46.7345710298625));
#35513=CARTESIAN_POINT('Ctrl Pts',(44.5998876039393,40.2003192840526,49.0808640421642));
#35514=CARTESIAN_POINT('Ctrl Pts',(42.681083475521,40.0740935416469,50.4349054658031));
#35515=CARTESIAN_POINT('Ctrl Pts',(40.5042399321047,39.947867799241,49.5536622260268));
#35516=CARTESIAN_POINT('Ctrl Pts',(40.0677363997466,39.821642056835,47.2461306170551));
#35517=CARTESIAN_POINT('Ctrl Pts',(41.7722905511079,39.6954163144293,45.6306639336346));
#35518=CARTESIAN_POINT('Ctrl Pts',(44.053092661125,39.5691905720234,46.1902880888541));
#35519=CARTESIAN_POINT('Ctrl Pts',(44.816327570069,39.4429648296175,48.411258582565));
#35520=CARTESIAN_POINT('Ctrl Pts',(43.3613326401056,39.3167390872117,50.2546866972324));
#35521=CARTESIAN_POINT('Ctrl Pts',(41.0238179831763,39.1905133448058,50.0282740456309));
#35522=CARTESIAN_POINT('Ctrl Pts',(39.9496618424098,39.0642876024,47.9398712958198));
#35523=CARTESIAN_POINT('Ctrl Pts',(41.1249578388071,38.9380618599941,45.9066677199284));
#35524=CARTESIAN_POINT('Ctrl Pts',(43.4707642423434,38.8118361175882,45.7951788088538));
#35525=CARTESIAN_POINT('Ctrl Pts',(44.8335908453665,38.6856103751823,47.7077532806737));
#35526=CARTESIAN_POINT('Ctrl Pts',(43.9623396289119,38.5593846327765,49.8886152153205));
#35527=CARTESIAN_POINT('Ctrl Pts',(41.6568340397108,38.4331588903706,50.3356962351891));
#35528=CARTESIAN_POINT('Ctrl Pts',(40.0335674518741,38.3069331479648,48.6385683540385));
#35529=CARTESIAN_POINT('Ctrl Pts',(40.5827262235116,38.180707405559,46.3552238544726));
#35530=CARTESIAN_POINT('Ctrl Pts',(42.8001732547391,38.0544816631531,45.5818118531015));
#35531=CARTESIAN_POINT('Ctrl Pts',(44.6502544265565,37.9282559207474,47.0283377318369));
#35532=CARTESIAN_POINT('Ctrl Pts',(44.4345637320296,37.8020301783415,49.3668661119213));
#35533=CARTESIAN_POINT('Ctrl Pts',(42.351108900119,37.6758044359356,50.450588135114));
#35534=CARTESIAN_POINT('Ctrl Pts',(40.3125369301003,37.5495786935296,49.2846285375211));
#35535=CARTESIAN_POINT('Ctrl Pts',(40.1902915900575,37.4233529511239,46.9393580761451));
#35536=CARTESIAN_POINT('Ctrl Pts',(42.0965961829524,37.2971272087181,45.5677749546126));
#35537=CARTESIAN_POINT('Ctrl Pts',(44.281430644293,37.1709014663122,46.4290158249288));
#35538=CARTESIAN_POINT('Ctrl Pts',(44.739079749351,37.0446757239063,48.7324469085092));
#35539=CARTESIAN_POINT('Ctrl Pts',(43.0494138297966,36.9184499815005,50.3634792627137));
#35540=CARTESIAN_POINT('Ctrl Pts',(40.7635749604744,36.7922242390946,49.8247974237219));
#35541=CARTESIAN_POINT('Ctrl Pts',(39.9800021318887,36.6659984966887,47.6109204889157));
#35542=CARTESIAN_POINT('Ctrl Pts',(41.4180285382873,36.5397727542828,45.7542251680121));
#35543=CARTESIAN_POINT('Ctrl Pts',(43.7575214611913,36.413547011877,45.9591893693892));
#35544=CARTESIAN_POINT('Ctrl Pts',(44.8507865756343,36.2873212694711,48.0376524673795));
#35545=CARTESIAN_POINT('Ctrl Pts',(43.6941878975161,36.1610955270653,50.0815499594128));
#35546=CARTESIAN_POINT('Ctrl Pts',(41.3495027004248,36.0348697846594,50.2145491575474));
#35547=CARTESIAN_POINT('Ctrl Pts',(39.9691919054106,35.9086440422536,48.314554534046));
#35548=CARTESIAN_POINT('Ctrl Pts',(40.8204043172953,35.7824182998477,46.1257934940924));
#35549=CARTESIAN_POINT('Ctrl Pts',(43.12171245303,35.6561925574419,45.6575859284171));
#35550=CARTESIAN_POINT('Ctrl Pts',(44.7604762722412,35.5299668150361,47.3397543519194));
#35551=CARTESIAN_POINT('Ctrl Pts',(44.2322826946139,35.4037410726303,49.6280395187459));
#35552=CARTESIAN_POINT('Ctrl Pts',(42.0220224151058,35.2775153302245,50.421756695651));
#35553=CARTESIAN_POINT('Ctrl Pts',(40.1587519922397,35.1512895878186,48.9922600039424));
#35554=CARTESIAN_POINT('Ctrl Pts',(40.3529853900521,35.0250638454127,46.6518517388546));
#35555=CARTESIAN_POINT('Ctrl Pts',(42.4264130429271,34.8988381030069,45.5490665250003));
#35556=CARTESIAN_POINT('Ctrl Pts',(44.4755930731687,34.772612360601,46.6962799599032));
#35557=CARTESIAN_POINT('Ctrl Pts',(44.6193433317553,34.6463866181951,49.0403305827646));
#35558=CARTESIAN_POINT('Ctrl Pts',(42.7256986366174,34.5201608757894,50.4293400229428));
#35559=CARTESIAN_POINT('Ctrl Pts',(40.5330570463177,34.3939351333834,49.5881739703691));
#35560=CARTESIAN_POINT('Ctrl Pts',(40.0543008714003,34.2677093909775,47.289037181073));
#35561=CARTESIAN_POINT('Ctrl Pts',(41.728936412622,34.1414836485718,45.6425763587958));
#35562=CARTESIAN_POINT('Ctrl Pts',(44.019619772034,34.0152579061658,46.1602705709202));
#35563=CARTESIAN_POINT('Ctrl Pts',(44.8234645676949,33.8890321637599,48.3668677043488));
#35564=CARTESIAN_POINT('Ctrl Pts',(43.4025277278384,33.7628064213541,50.2366740596067));
#35565=CARTESIAN_POINT('Ctrl Pts',(41.0612531929868,33.6365806789483,50.0531755186354));
#35566=CARTESIAN_POINT('Ctrl Pts',(39.9489713648778,33.5103549365424,47.9848269787123));
#35567=CARTESIAN_POINT('Ctrl Pts',(41.0867748476205,33.3841291941365,45.9304073808587));
#35568=CARTESIAN_POINT('Ctrl Pts',(43.4301427575952,33.2579034517307,45.7759093326285));
#35569=CARTESIAN_POINT('Ctrl Pts',(44.8278193301428,33.1316777093248,47.663163782899));
#35570=CARTESIAN_POINT('Ctrl Pts',(43.9967219010468,33.0054519669191,49.8596407897353));
#35571=CARTESIAN_POINT('Ctrl Pts',(41.6997957186581,32.8792262245131,50.3489335606354));
#35572=CARTESIAN_POINT('Ctrl Pts',(40.0456905894021,32.7530004821074,48.6818699855523));
#35573=CARTESIAN_POINT('Ctrl Pts',(40.5528386320335,32.6267747397014,46.3888289245825));
#35574=CARTESIAN_POINT('Ctrl Pts',(42.7557976019851,32.5005489972957,45.5748886864084));
#35575=CARTESIAN_POINT('Ctrl Pts',(44.6319586738618,32.3743232548897,46.9872054387344));
#35576=CARTESIAN_POINT('Ctrl Pts',(44.4594808838175,32.248097512484,49.3293573331649));
#35577=CARTESIAN_POINT('Ctrl Pts',(42.3956942898794,32.1218717700782,50.4509924940452));
#35578=CARTESIAN_POINT('Ctrl Pts',(40.3371938279938,31.9956460276723,49.322860953228));
#35579=CARTESIAN_POINT('Ctrl Pts',(40.1697200713673,31.8694202852663,46.9797548379716));
#35580=CARTESIAN_POINT('Ctrl Pts',(42.0554032321223,31.7431774219253,45.574152005912));
#35581=CARTESIAN_POINT('Ctrl Pts',(43.5147897566423,31.6590098060527,46.121195336702));
#35582=CARTESIAN_POINT('Ctrl Pts',(43.9668310375078,31.6169174376488,46.6432751661215));
#35583=CARTESIAN_POINT('Ctrl Pts',(41.375799831196,47.0578710221704,49.9691570377152));
#35584=CARTESIAN_POINT('Ctrl Pts',(40.7199518878545,47.0157957747018,49.6280366692455));
#35585=CARTESIAN_POINT('Ctrl Pts',(39.7875871287221,46.9316452797646,48.2442488706934));
#35586=CARTESIAN_POINT('Ctrl Pts',(40.7824400451221,46.8054195373585,45.9307058233814));
#35587=CARTESIAN_POINT('Ctrl Pts',(43.2647373419639,46.6791937949528,45.5222322801147));
#35588=CARTESIAN_POINT('Ctrl Pts',(44.9519389235938,46.5529680525469,47.3857570384877));
#35589=CARTESIAN_POINT('Ctrl Pts',(44.2970468999311,46.4267423101412,49.8144850257279));
#35590=CARTESIAN_POINT('Ctrl Pts',(41.9003167041634,46.3005165677351,50.5768225199857));
#35591=CARTESIAN_POINT('Ctrl Pts',(39.9624636790296,46.1742908253294,48.9739262709606));
#35592=CARTESIAN_POINT('Ctrl Pts',(40.2622302906338,46.0480650829236,46.4767814973122));
#35593=CARTESIAN_POINT('Ctrl Pts',(42.5245462317156,45.9218393405177,45.3780615738228));
#35594=CARTESIAN_POINT('Ctrl Pts',(44.6725063122828,45.7956135981119,46.6862833235523));
#35595=CARTESIAN_POINT('Ctrl Pts',(44.7342771298289,45.669387855706,49.2005406916632));
#35596=CARTESIAN_POINT('Ctrl Pts',(42.6531366708118,45.5431621133002,50.6126705292915));
#35597=CARTESIAN_POINT('Ctrl Pts',(40.339615024441,45.4169363708943,49.6263297531126));
#35598=CARTESIAN_POINT('Ctrl Pts',(39.917560555862,45.2907106284885,47.1469878622588));
#35599=CARTESIAN_POINT('Ctrl Pts',(41.7744284062985,45.1644848860825,45.4507270012443));
#35600=CARTESIAN_POINT('Ctrl Pts',(44.2055812987032,45.0382591436767,46.0947414574306));
#35601=CARTESIAN_POINT('Ctrl Pts',(44.979179990791,44.9120334012709,48.4878160323366));
#35602=CARTESIAN_POINT('Ctrl Pts',(43.3850474664145,44.7858076588651,50.4330670119889));
#35603=CARTESIAN_POINT('Ctrl Pts',(40.8866246427863,44.6595819164592,50.1447211477612));
#35604=CARTESIAN_POINT('Ctrl Pts',(39.7775061359443,44.5333561740533,47.8874847193674));
#35605=CARTESIAN_POINT('Ctrl Pts',(41.0758816457674,44.4071304316475,45.7335392559602));
#35606=CARTESIAN_POINT('Ctrl Pts',(43.5898203379522,44.2809046892416,45.6602433230422));
#35607=CARTESIAN_POINT('Ctrl Pts',(45.0114837100247,44.1546789468357,47.7348838514171));
#35608=CARTESIAN_POINT('Ctrl Pts',(44.035760583504,44.02845320443,50.0529055140476));
#35609=CARTESIAN_POINT('Ctrl Pts',(41.5583813988641,43.9022274620241,50.486324972618));
#35610=CARTESIAN_POINT('Ctrl Pts',(39.8536224153584,43.7760017196182,48.6372557845636));
#35611=CARTESIAN_POINT('Ctrl Pts',(40.4864813979593,43.6497759772124,46.2031749395733));
#35612=CARTESIAN_POINT('Ctrl Pts',(42.8759830281547,43.5235502348065,45.4186100845792));
#35613=CARTESIAN_POINT('Ctrl Pts',(44.8285241365898,43.3973244924007,47.0038051112294));
#35614=CARTESIAN_POINT('Ctrl Pts',(44.5516387504256,43.2710987499948,49.503524002483));
#35615=CARTESIAN_POINT('Ctrl Pts',(42.2995123672055,43.144873007589,50.6229822672065));
#35616=CARTESIAN_POINT('Ctrl Pts',(40.1396353413383,43.0186472651831,49.3344981634606));
#35617=CARTESIAN_POINT('Ctrl Pts',(40.0548115469822,42.8924215227773,46.8209220304679));
#35618=CARTESIAN_POINT('Ctrl Pts',(42.1229106711827,42.7661957803713,45.3897595432095));
#35619=CARTESIAN_POINT('Ctrl Pts',(44.4453825157214,42.6399700379655,46.3548422255637));
#35620=CARTESIAN_POINT('Ctrl Pts',(44.8901583952948,42.5137442955597,48.8302077479463));
#35621=CARTESIAN_POINT('Ctrl Pts',(43.0489264816905,42.3875185531538,50.5434284263114));
#35622=CARTESIAN_POINT('Ctrl Pts',(40.6119690121749,42.261292810748,49.921738516288));
#35623=CARTESIAN_POINT('Ctrl Pts',(39.8164544244997,42.1350670683421,47.5358599373892));
#35624=CARTESIAN_POINT('Ctrl Pts',(41.3926786510233,42.0088413259363,45.5760698363395));
#35625=CARTESIAN_POINT('Ctrl Pts',(43.8936410220548,41.8826155835305,45.8414888845218));
#35626=CARTESIAN_POINT('Ctrl Pts',(45.0234155107894,41.7563898411245,48.0884578778673));
#35627=CARTESIAN_POINT('Ctrl Pts',(43.7448499060829,41.6301640987188,50.2542210336426));
#35628=CARTESIAN_POINT('Ctrl Pts',(41.2316891961937,41.5039383563129,50.3505709102508));
#35629=CARTESIAN_POINT('Ctrl Pts',(39.7910576906322,41.377712613907,48.2890566809437));
#35630=CARTESIAN_POINT('Ctrl Pts',(40.7454796332511,41.2514868715012,45.9621834983442));
#35631=CARTESIAN_POINT('Ctrl Pts',(43.2187794350078,41.1252611290953,45.5060605510125));
#35632=CARTESIAN_POINT('Ctrl Pts',(44.9404257785515,40.9990353866895,47.3394164685078));
#35633=CARTESIAN_POINT('Ctrl Pts',(44.3299180154603,40.8728096442837,49.7791993120531));
#35634=CARTESIAN_POINT('Ctrl Pts',(41.9477126640256,40.7465839018778,50.5856469024452));
#35635=CARTESIAN_POINT('Ctrl Pts',(39.9807147856365,40.6203581594719,49.0184266247355));
#35636=CARTESIAN_POINT('Ctrl Pts',(40.2346619139606,40.4941324170661,46.5162733703425));
#35637=CARTESIAN_POINT('Ctrl Pts',(42.4764262626284,40.3679066746601,45.3762064172675));
#35638=CARTESIAN_POINT('Ctrl Pts',(44.6480300013119,40.2416809322544,46.6448266341129));
#35639=CARTESIAN_POINT('Ctrl Pts',(44.7559039338887,40.1154551898485,49.1575190679622));
#35640=CARTESIAN_POINT('Ctrl Pts',(42.7010179540743,39.9892294474426,50.6075892946806));
#35641=CARTESIAN_POINT('Ctrl Pts',(40.3697923686348,39.8630037050366,49.6638481637318));
#35642=CARTESIAN_POINT('Ctrl Pts',(39.9023319460215,39.736777962631,47.1926660972417));
#35643=CARTESIAN_POINT('Ctrl Pts',(41.7277733110837,39.610552220225,45.462630295539));
#35644=CARTESIAN_POINT('Ctrl Pts',(44.1703302188954,39.4843264778193,46.0619430724373));
#35645=CARTESIAN_POINT('Ctrl Pts',(44.9876938520384,39.3581007354134,48.4404250975257));
#35646=CARTESIAN_POINT('Ctrl Pts',(43.4295104825105,39.2318749930075,50.4145893863779));
#35647=CARTESIAN_POINT('Ctrl Pts',(40.9262189661981,39.1056492506017,50.1721195185379));
#35648=CARTESIAN_POINT('Ctrl Pts',(39.7758835249186,38.9794235081958,47.9356069598901));
#35649=CARTESIAN_POINT('Ctrl Pts',(41.0345316742323,38.85319776579,45.7582083081311));
#35650=CARTESIAN_POINT('Ctrl Pts',(43.5467029889559,38.7269720233841,45.6388125882245));
#35651=CARTESIAN_POINT('Ctrl Pts',(45.0061814411827,38.6007462809783,47.687027103342));
#35652=CARTESIAN_POINT('Ctrl Pts',(44.0731409692172,38.4745205385724,50.0225560648681));
#35653=CARTESIAN_POINT('Ctrl Pts',(41.6041286080969,38.3482947961665,50.5013441318535));
#35654=CARTESIAN_POINT('Ctrl Pts',(39.8657397316897,38.2220690537607,48.6838557091019));
#35655=CARTESIAN_POINT('Ctrl Pts',(40.4538449185697,38.0958433113549,46.2385761051266));
#35656=CARTESIAN_POINT('Ctrl Pts',(42.8285535967332,37.969617568949,45.4103136187687));
#35657=CARTESIAN_POINT('Ctrl Pts',(44.8098427784591,37.8433918265431,46.9594273107965));
#35658=CARTESIAN_POINT('Ctrl Pts',(44.5788552703569,37.7171660841372,49.4638044436488));
#35659=CARTESIAN_POINT('Ctrl Pts',(42.347641536624,37.5909403417315,50.6243841810452));
#35660=CARTESIAN_POINT('Ctrl Pts',(40.1644937634915,37.4647145993256,49.3757345692172));
#35661=CARTESIAN_POINT('Ctrl Pts',(40.0335787672024,37.3384888569198,46.8641372057452));
#35662=CARTESIAN_POINT('Ctrl Pts',(42.0750787427234,37.2122631145138,45.3952812215179));
#35663=CARTESIAN_POINT('Ctrl Pts',(44.4148619630801,37.0860373721079,46.3176014122269));
#35664=CARTESIAN_POINT('Ctrl Pts',(44.9049676053029,36.9598116297022,48.7843921435038));
#35665=CARTESIAN_POINT('Ctrl Pts',(43.0954703474852,36.8335858872964,50.5310975354926));
#35666=CARTESIAN_POINT('Ctrl Pts',(40.647519472709,36.7073601448905,49.9542123067552));
#35667=CARTESIAN_POINT('Ctrl Pts',(39.8083755518798,36.5811344024847,47.5833269167399));
#35668=CARTESIAN_POINT('Ctrl Pts',(41.3483869878293,36.4549086600788,45.5949545095694));
#35669=CARTESIAN_POINT('Ctrl Pts',(43.8537970690102,36.3286829176729,45.8144548001597));
#35670=CARTESIAN_POINT('Ctrl Pts',(45.0245966949945,36.2024571752671,48.0403227855192));
#35671=CARTESIAN_POINT('Ctrl Pts',(43.7859718803313,36.0762314328613,50.2291737674166));
#35672=CARTESIAN_POINT('Ctrl Pts',(41.2750012881672,35.9500056904552,50.3716052868853));
#35673=CARTESIAN_POINT('Ctrl Pts',(39.7967986626603,35.8237799480496,48.3368627846507));
#35674=CARTESIAN_POINT('Ctrl Pts',(40.7083791752934,35.6975542056437,45.9928745121884));
#35675=CARTESIAN_POINT('Ctrl Pts',(43.1728963989727,35.5713284632378,45.4914616018761));
#35676=CARTESIAN_POINT('Ctrl Pts',(44.927881572525,35.4451027208319,47.2929296401959));
#35677=CARTESIAN_POINT('Ctrl Pts',(44.3622284340833,35.3188769784261,49.7435003042299));
#35678=CARTESIAN_POINT('Ctrl Pts',(41.9952161930549,35.1926512360203,50.5935080119497));
#35679=CARTESIAN_POINT('Ctrl Pts',(39.9998023767907,35.0664254936144,49.0626312192234));
#35680=CARTESIAN_POINT('Ctrl Pts',(40.2078108337589,34.9401997512085,46.5562408796657));
#35681=CARTESIAN_POINT('Ctrl Pts',(42.4282862595464,34.8139740088026,45.3752459875171));
#35682=CARTESIAN_POINT('Ctrl Pts',(44.6227944179848,34.6877482663969,46.6038199562315));
#35683=CARTESIAN_POINT('Ctrl Pts',(44.776739464584,34.561522523991,49.1141109700746));
#35684=CARTESIAN_POINT('Ctrl Pts',(42.7487972285017,34.435296781585,50.601629149851));
#35685=CARTESIAN_POINT('Ctrl Pts',(40.4006531965316,34.3090710391792,49.7008074857061));
#35686=CARTESIAN_POINT('Ctrl Pts',(39.8879435681661,34.1828452967733,47.2386156006519));
#35687=CARTESIAN_POINT('Ctrl Pts',(41.6813444911631,34.0566195543676,45.4753875515231));
#35688=CARTESIAN_POINT('Ctrl Pts',(44.1344834279288,33.9303938119617,46.0297967080234));
#35689=CARTESIAN_POINT('Ctrl Pts',(44.9953370065128,33.8041680695559,48.3928860121509));
#35690=CARTESIAN_POINT('Ctrl Pts',(43.4736271315033,33.6779423271499,50.3952992900265));
#35691=CARTESIAN_POINT('Ctrl Pts',(40.9663090862117,33.5517165847442,50.1987870074159));
#35692=CARTESIAN_POINT('Ctrl Pts',(39.7751440786257,33.4254908423384,47.9837509059659));
#35693=CARTESIAN_POINT('Ctrl Pts',(40.9936407400849,33.2992650999325,45.7836315890635));
#35694=CARTESIAN_POINT('Ctrl Pts',(43.5032006229498,33.1730393575266,45.6181765181081));
#35695=CARTESIAN_POINT('Ctrl Pts',(45.0000006093094,33.0468136151207,47.6392753122826));
#35696=CARTESIAN_POINT('Ctrl Pts',(44.1099616367975,32.9205878727149,49.9915267690549));
#35697=CARTESIAN_POINT('Ctrl Pts',(41.650137135195,32.7943621303091,50.5155202502322));
#35698=CARTESIAN_POINT('Ctrl Pts',(39.8787226437902,32.6681363879032,48.7302282982488));
#35699=CARTESIAN_POINT('Ctrl Pts',(40.4218376950136,32.5419106454973,46.274564451408));
#35700=CARTESIAN_POINT('Ctrl Pts',(42.7810308166128,32.4156849030914,45.4028994601463));
#35701=CARTESIAN_POINT('Ctrl Pts',(44.7902494884793,32.2894591606857,46.9153779098378));
#35702=CARTESIAN_POINT('Ctrl Pts',(44.6055395499598,32.1632334182798,49.4236355371696));
#35703=CARTESIAN_POINT('Ctrl Pts',(42.3953889283282,32.0370076758738,50.6248172171673));
#35704=CARTESIAN_POINT('Ctrl Pts',(40.1908993319584,31.9107819334682,49.4166784330786));
#35705=CARTESIAN_POINT('Ctrl Pts',(40.0115483135911,31.7845561910622,46.9073989114492));
#35706=CARTESIAN_POINT('Ctrl Pts',(42.0309643821828,31.6583133277211,45.4021105341682));
#35707=CARTESIAN_POINT('Ctrl Pts',(43.5938507987542,31.5741457118486,45.9879502528466));
#35708=CARTESIAN_POINT('Ctrl Pts',(44.0779509091253,31.5320533434447,46.5470560552206));
#35709=CARTESIAN_POINT('Ctrl Pts',(41.3079736566343,46.9730069279662,50.0995616139371));
#35710=CARTESIAN_POINT('Ctrl Pts',(40.6086931320009,46.9309316804976,49.7358510425334));
#35711=CARTESIAN_POINT('Ctrl Pts',(39.6145838654623,46.8467811855604,48.2604238988224));
#35712=CARTESIAN_POINT('Ctrl Pts',(40.6753194770875,46.7205554431545,45.7936698099951));
#35713=CARTESIAN_POINT('Ctrl Pts',(43.3220033214984,46.5943297007486,45.358145697227));
#35714=CARTESIAN_POINT('Ctrl Pts',(45.1209373871503,46.4681039583428,47.3450796869312));
#35715=CARTESIAN_POINT('Ctrl Pts',(44.4226760865935,46.341878215937,49.9346466717058));
#35716=CARTESIAN_POINT('Ctrl Pts',(41.8672259007431,46.2156524735311,50.7474688637164));
#35717=CARTESIAN_POINT('Ctrl Pts',(39.8010413623359,46.0894267311253,49.0384231293642));
#35718=CARTESIAN_POINT('Ctrl Pts',(40.1206595841484,45.9632009887194,46.3759085554738));
#35719=CARTESIAN_POINT('Ctrl Pts',(42.5327941257413,45.8369752463135,45.2044274944695));
#35720=CARTESIAN_POINT('Ctrl Pts',(44.8229997553851,45.7107495039077,46.5992843370893));
#35721=CARTESIAN_POINT('Ctrl Pts',(44.888861255965,45.5845237615018,49.2800447622554));
#35722=CARTESIAN_POINT('Ctrl Pts',(42.6699002806466,45.458298019096,50.7856908555805));
#35723=CARTESIAN_POINT('Ctrl Pts',(40.2031690100066,45.3320722766902,49.7340310883488));
#35724=CARTESIAN_POINT('Ctrl Pts',(39.7531645947938,45.2058465342842,47.0904983674123));
#35725=CARTESIAN_POINT('Ctrl Pts',(41.7330008324632,45.0796207918785,45.2819050847036));
#35726=CARTESIAN_POINT('Ctrl Pts',(44.3251533082391,44.9533950494725,45.9685684666135));
#35727=CARTESIAN_POINT('Ctrl Pts',(45.1499824546155,44.8271693070668,48.5201209433989));
#35728=CARTESIAN_POINT('Ctrl Pts',(43.4502808098991,44.7009435646609,50.5941933551607));
#35729=CARTESIAN_POINT('Ctrl Pts',(40.7864035490177,44.5747178222551,50.2867522031983));
#35730=CARTESIAN_POINT('Ctrl Pts',(39.6038352735211,44.4484920798491,47.8800335576731));
#35731=CARTESIAN_POINT('Ctrl Pts',(40.9881938232402,44.3222663374434,45.5834461718693));
#35732=CARTESIAN_POINT('Ctrl Pts',(43.6686144686279,44.1960405950374,45.5052963218242));
#35733=CARTESIAN_POINT('Ctrl Pts',(45.1844254409248,44.0698148526316,47.7173269179967));
#35734=CARTESIAN_POINT('Ctrl Pts',(44.14408646184,43.9435891102256,50.1888562119632));
#35735=CARTESIAN_POINT('Ctrl Pts',(41.5026464244972,43.8173633678199,50.650978247189));
#35736=CARTESIAN_POINT('Ctrl Pts',(39.6849922434289,43.6911376254141,48.6794571270361));
#35737=CARTESIAN_POINT('Ctrl Pts',(40.359761396653,43.5649118830082,46.0841827992503));
#35738=CARTESIAN_POINT('Ctrl Pts',(42.9075043156328,43.4386861406023,45.2476612716929));
#35739=CARTESIAN_POINT('Ctrl Pts',(44.9893496344101,43.3124603981964,46.9378335458254));
#35740=CARTESIAN_POINT('Ctrl Pts',(44.694127914092,43.1862346557907,49.6030927045356));
#35741=CARTESIAN_POINT('Ctrl Pts',(42.29285771909,43.0600089133848,50.7966854734219));
#35742=CARTESIAN_POINT('Ctrl Pts',(39.9899459616828,42.9337831709789,49.4228733738384));
#35743=CARTESIAN_POINT('Ctrl Pts',(39.8995048342524,42.8075574285731,46.7428392976006));
#35744=CARTESIAN_POINT('Ctrl Pts',(42.1045608312217,42.6813316861672,45.2169001449566));
#35745=CARTESIAN_POINT('Ctrl Pts',(44.5808350139558,42.5551059437613,46.245894031852));
#35746=CARTESIAN_POINT('Ctrl Pts',(45.0550655327371,42.4288802013556,48.8851870550678));
#35747=CARTESIAN_POINT('Ctrl Pts',(43.0919006991974,42.3026544589497,50.7118632944967));
#35748=CARTESIAN_POINT('Ctrl Pts',(40.4935592465884,42.1764287165438,50.0490028695245));
#35749=CARTESIAN_POINT('Ctrl Pts',(39.6453628561431,42.050202974138,47.505122933172));
#35750=CARTESIAN_POINT('Ctrl Pts',(41.3259702518877,41.9239772317321,45.4155485677308));
#35751=CARTESIAN_POINT('Ctrl Pts',(43.9925552380253,41.7977514893263,45.6985446084214));
#35752=CARTESIAN_POINT('Ctrl Pts',(45.1971474079345,41.6715257469204,48.094315872865));
#35753=CARTESIAN_POINT('Ctrl Pts',(43.8339106456409,41.5453000045146,50.4035035606187));
#35754=CARTESIAN_POINT('Ctrl Pts',(41.154319503301,41.4190742621087,50.5062340684245));
#35755=CARTESIAN_POINT('Ctrl Pts',(39.6182842603143,41.2928485197029,48.3081990414871));
#35756=CARTESIAN_POINT('Ctrl Pts',(40.6359114154075,41.166622777297,45.8272320484462));
#35757=CARTESIAN_POINT('Ctrl Pts',(43.2730019186371,41.0403970348911,45.3409030187592));
#35758=CARTESIAN_POINT('Ctrl Pts',(45.1086618007328,40.9141712924853,47.2956702797409));
#35759=CARTESIAN_POINT('Ctrl Pts',(44.4577240441967,40.7879455500795,49.8970242126877));
#35760=CARTESIAN_POINT('Ctrl Pts',(41.9177605894838,40.6617198076736,50.756877628139));
#35761=CARTESIAN_POINT('Ctrl Pts',(39.8205011220756,40.5354940652678,49.0858704546932));
#35762=CARTESIAN_POINT('Ctrl Pts',(40.0912655316106,40.4092683228619,46.4180157206662));
#35763=CARTESIAN_POINT('Ctrl Pts',(42.4814874813122,40.283042580456,45.202449482855));
#35764=CARTESIAN_POINT('Ctrl Pts',(44.7969025361278,40.1568168380502,46.5550822383634));
#35765=CARTESIAN_POINT('Ctrl Pts',(44.9119202638379,40.0305910956443,49.2341740937601));
#35766=CARTESIAN_POINT('Ctrl Pts',(42.7209524326276,39.9043653532385,50.780273123558));
#35767=CARTESIAN_POINT('Ctrl Pts',(40.2353448051647,39.7781396108327,49.7740341014369));
#35768=CARTESIAN_POINT('Ctrl Pts',(39.7369274922965,39.6519138684268,47.1392015774281));
#35769=CARTESIAN_POINT('Ctrl Pts',(41.6832560710595,39.525688126021,45.2945966574436));
#35770=CARTESIAN_POINT('Ctrl Pts',(44.2875677766657,39.3994623836151,45.9335980560206));
#35771=CARTESIAN_POINT('Ctrl Pts',(45.1590601340077,39.2732366412092,48.4695916124862));
#35772=CARTESIAN_POINT('Ctrl Pts',(43.4976883249155,39.1470108988034,50.5744920755234));
#35773=CARTESIAN_POINT('Ctrl Pts',(40.8286199492197,39.0207851563975,50.3159649914449));
#35774=CARTESIAN_POINT('Ctrl Pts',(39.6021052074275,38.8945594139917,47.9313426239604));
#35775=CARTESIAN_POINT('Ctrl Pts',(40.9441055096574,38.7683336715858,45.6097488963336));
#35776=CARTESIAN_POINT('Ctrl Pts',(43.6226417355683,38.64210792918,45.4824463675952));
#35777=CARTESIAN_POINT('Ctrl Pts',(45.1787720369989,38.515882186774,47.6663009260103));
#35778=CARTESIAN_POINT('Ctrl Pts',(44.1839423095224,38.3896564443681,50.1564969144156));
#35779=CARTESIAN_POINT('Ctrl Pts',(41.5514231764831,38.2634307019625,50.666992028518));
#35780=CARTESIAN_POINT('Ctrl Pts',(39.6979120115051,38.1372049595565,48.7291430641652));
#35781=CARTESIAN_POINT('Ctrl Pts',(40.324963613628,38.0109792171507,46.1219283557807));
#35782=CARTESIAN_POINT('Ctrl Pts',(42.8569339387272,37.8847534747447,45.2388153844359));
#35783=CARTESIAN_POINT('Ctrl Pts',(44.9694311303618,37.758527732339,46.8905168897562));
#35784=CARTESIAN_POINT('Ctrl Pts',(44.723146808684,37.6323019899332,49.5607427753764));
#35785=CARTESIAN_POINT('Ctrl Pts',(42.3441741731293,37.5060762475273,50.7981802269766));
#35786=CARTESIAN_POINT('Ctrl Pts',(40.0164505968826,37.3798505051215,49.4668406009133));
#35787=CARTESIAN_POINT('Ctrl Pts',(39.8768659443472,37.2536247627156,46.7889163353453));
#35788=CARTESIAN_POINT('Ctrl Pts',(42.0535613024942,37.1273990203097,45.2227874884231));
#35789=CARTESIAN_POINT('Ctrl Pts',(44.5482932818671,37.0011732779039,46.206186999525));
#35790=CARTESIAN_POINT('Ctrl Pts',(45.0708554612549,36.874947535498,48.8363373784985));
#35791=CARTESIAN_POINT('Ctrl Pts',(43.1415268651735,36.7487217930922,50.6987158082714));
#35792=CARTESIAN_POINT('Ctrl Pts',(40.5314639849437,36.6224960506863,50.0836271897885));
#35793=CARTESIAN_POINT('Ctrl Pts',(39.6367489718709,36.4962703082805,47.5557333445642));
#35794=CARTESIAN_POINT('Ctrl Pts',(41.2787454373714,36.3700445658746,45.4356838511265));
#35795=CARTESIAN_POINT('Ctrl Pts',(43.9500726768291,36.2438188234688,45.6697202309303));
#35796=CARTESIAN_POINT('Ctrl Pts',(45.1984068143546,36.1175930810629,48.0429931036587));
#35797=CARTESIAN_POINT('Ctrl Pts',(43.8777558631465,35.991367338657,50.3767975754204));
#35798=CARTESIAN_POINT('Ctrl Pts',(41.2004998759096,35.8651415962512,50.528661416223));
#35799=CARTESIAN_POINT('Ctrl Pts',(39.6244054199101,35.7389158538454,48.3591710352555));
#35800=CARTESIAN_POINT('Ctrl Pts',(40.5963540332916,35.6126901114394,45.8599555302844));
#35801=CARTESIAN_POINT('Ctrl Pts',(43.2240803449157,35.4864643690335,45.3253372753352));
#35802=CARTESIAN_POINT('Ctrl Pts',(45.0952868728086,35.3602386266278,47.2461049284724));
#35803=CARTESIAN_POINT('Ctrl Pts',(44.4921741735526,35.234012884222,49.858961089714));
#35804=CARTESIAN_POINT('Ctrl Pts',(41.968409971004,35.1077871418161,50.7652593282483));
#35805=CARTESIAN_POINT('Ctrl Pts',(39.8408527613417,34.9815613994102,49.1330024345044));
#35806=CARTESIAN_POINT('Ctrl Pts',(40.0626362774657,34.8553356570044,46.4606300204769));
#35807=CARTESIAN_POINT('Ctrl Pts',(42.4301594761657,34.7291099145985,45.2014254500338));
#35808=CARTESIAN_POINT('Ctrl Pts',(44.7699957628009,34.6028841721927,46.5113599525599));
#35809=CARTESIAN_POINT('Ctrl Pts',(44.9341355974128,34.4766584297868,49.1878913573846));
#35810=CARTESIAN_POINT('Ctrl Pts',(42.7718958203859,34.350432687381,50.773918276759));
#35811=CARTESIAN_POINT('Ctrl Pts',(40.2682493467455,34.2242069449751,49.8134410010433));
#35812=CARTESIAN_POINT('Ctrl Pts',(39.7215862649318,34.0979812025693,47.1881940202308));
#35813=CARTESIAN_POINT('Ctrl Pts',(41.633752569704,33.9717554601635,45.3081987442505));
#35814=CARTESIAN_POINT('Ctrl Pts',(44.2493470838237,33.8455297177575,45.8993228451264));
#35815=CARTESIAN_POINT('Ctrl Pts',(45.1672094453306,33.7193039753518,48.4189043199531));
#35816=CARTESIAN_POINT('Ctrl Pts',(43.5447265351681,33.5930782329459,50.5539245204464));
#35817=CARTESIAN_POINT('Ctrl Pts',(40.8713649794366,33.46685249054,50.3443984961964));
#35818=CARTESIAN_POINT('Ctrl Pts',(39.6013167923734,33.3406267481341,47.9826748332197));
#35819=CARTESIAN_POINT('Ctrl Pts',(40.9005066325494,33.2144010057282,45.6368557972682));
#35820=CARTESIAN_POINT('Ctrl Pts',(43.5762584883044,33.0881752633225,45.4604437035877));
#35821=CARTESIAN_POINT('Ctrl Pts',(45.1721818884761,32.9619495209166,47.6153868416661));
#35822=CARTESIAN_POINT('Ctrl Pts',(44.223201372548,32.8357237785108,50.1234127483746));
#35823=CARTESIAN_POINT('Ctrl Pts',(41.6004785517319,32.7094980361049,50.6821069398291));
#35824=CARTESIAN_POINT('Ctrl Pts',(39.7117546981783,32.583272293699,48.7785866109453));
#35825=CARTESIAN_POINT('Ctrl Pts',(40.2908367579938,32.4570465512932,46.1602999782335));
#35826=CARTESIAN_POINT('Ctrl Pts',(42.8062640312401,32.3308208088874,45.2309102338841));
#35827=CARTESIAN_POINT('Ctrl Pts',(44.9485403030968,32.2045950664815,46.843550380941));
#35828=CARTESIAN_POINT('Ctrl Pts',(44.7515982161019,32.0783693240757,49.5179137411743));
#35829=CARTESIAN_POINT('Ctrl Pts',(42.3950835667773,31.9521435816698,50.7986419402894));
#35830=CARTESIAN_POINT('Ctrl Pts',(40.0446048359227,31.8259178392639,49.510495912929));
#35831=CARTESIAN_POINT('Ctrl Pts',(39.8533765558149,31.6996920968581,46.8350429849268));
#35832=CARTESIAN_POINT('Ctrl Pts',(42.0065255322431,31.5734492335169,45.2300690624244));
#35833=CARTESIAN_POINT('Ctrl Pts',(43.6729118408661,31.4892816176444,45.8547051689911));
#35834=CARTESIAN_POINT('Ctrl Pts',(44.1890707807428,31.4471892492405,46.4508369443197));
#35835=CARTESIAN_POINT('Ctrl Pts',(40.2631768443428,31.6998,46.9876066983108));
#35836=CARTESIAN_POINT('Ctrl Pts',(40.2699897636978,31.6998,46.9743722232763));
#35837=CARTESIAN_POINT('Ctrl Pts',(40.2768026830528,31.6998,46.9611377482418));
#35838=CARTESIAN_POINT('Ctrl Pts',(40.2836156024077,31.6998,46.9479032732073));
#35839=CARTESIAN_POINT('Ctrl Pts',(41.1894856841367,46.9748,46.4934199857144));
#35840=CARTESIAN_POINT('Ctrl Pts',(41.1303103774516,46.9748,46.5309428133167));
#35841=CARTESIAN_POINT('Ctrl Pts',(41.0734841647242,46.9748,46.5719388529248));
#35842=CARTESIAN_POINT('Ctrl Pts',(41.0190945497751,46.9748,46.6160466749811));
#35843=CARTESIAN_POINT('Ctrl Pts',(40.9691207710807,46.9748,46.6565734288513));
#35844=CARTESIAN_POINT('Ctrl Pts',(40.9212038267111,46.9748,46.6997281928621));
#35845=CARTESIAN_POINT('Ctrl Pts',(40.8754251407322,46.9748,46.7452668914558));
#35846=CARTESIAN_POINT('Ctrl Pts',(40.8605791100933,46.9748,46.7600350941711));
#35847=CARTESIAN_POINT('Ctrl Pts',(40.8459553825702,46.9748,46.7750573691295));
#35848=CARTESIAN_POINT('Ctrl Pts',(40.831575992807,46.9748,46.7903053231744));
#35849=CARTESIAN_POINT('Ctrl Pts',(40.7812255431889,46.9748,46.8436971120169));
#35850=CARTESIAN_POINT('Ctrl Pts',(40.7338237459469,46.9748,46.8998950177031));
#35851=CARTESIAN_POINT('Ctrl Pts',(40.6894798075503,46.9748,46.9585357637079));
#35852=CARTESIAN_POINT('Ctrl Pts',(40.6540114853422,46.9748,47.0054393304417));
#35853=CARTESIAN_POINT('Ctrl Pts',(40.620499707712,46.9748,47.0539069081057));
#35854=CARTESIAN_POINT('Ctrl Pts',(40.5890132394166,46.9748,47.1037727021388));
#35855=CARTESIAN_POINT('Ctrl Pts',(40.5812875236016,46.9748,47.1160080836993));
#35856=CARTESIAN_POINT('Ctrl Pts',(40.5736835750194,46.9748,47.1283282812167));
#35857=CARTESIAN_POINT('Ctrl Pts',(40.5662105083118,46.9748,47.1407172084176));
#35858=CARTESIAN_POINT('Ctrl Pts',(40.526893031703,46.9748,47.2058981273756));
#35859=CARTESIAN_POINT('Ctrl Pts',(40.4911397818449,46.9748000000001,47.2730654660139));
#35860=CARTESIAN_POINT('Ctrl Pts',(40.4590588766433,46.9748,47.3418372106352));
#35861=CARTESIAN_POINT('Ctrl Pts',(40.4269779714417,46.9748,47.4106089552565));
#35862=CARTESIAN_POINT('Ctrl Pts',(40.3985688107134,46.9748,47.480985962799));
#35863=CARTESIAN_POINT('Ctrl Pts',(40.3739722403437,46.9748,47.5526268721434));
#35864=CARTESIAN_POINT('Ctrl Pts',(40.35613377041,46.9748,47.6045838803019));
#35865=CARTESIAN_POINT('Ctrl Pts',(40.3403012776577,46.9748,47.6572065634792));
#35866=CARTESIAN_POINT('Ctrl Pts',(40.3265420108385,46.9748,47.7103741641063));
#35867=CARTESIAN_POINT('Ctrl Pts',(40.3160697598934,46.9748,47.7508403069054));
#35868=CARTESIAN_POINT('Ctrl Pts',(40.3067987099654,46.9748,47.7916222866019));
#35869=CARTESIAN_POINT('Ctrl Pts',(40.2987636881035,46.9748,47.8326688703311));
#35870=CARTESIAN_POINT('Ctrl Pts',(40.295132423041,46.9748,47.8512190408216));
#35871=CARTESIAN_POINT('Ctrl Pts',(40.291752669636,46.9748,47.8698301774986));
#35872=CARTESIAN_POINT('Ctrl Pts',(40.2886337454123,46.9748,47.8884603431078));
#35873=CARTESIAN_POINT('Ctrl Pts',(40.2756479319583,46.9748,47.9660280677026));
#35874=CARTESIAN_POINT('Ctrl Pts',(40.2671589705433,46.9748,48.0440153075512));
#35875=CARTESIAN_POINT('Ctrl Pts',(40.2633055724053,46.9748,48.1220534670357));
#35876=CARTESIAN_POINT('Ctrl Pts',(40.2620603022212,46.9748,48.1472724010129));
#35877=CARTESIAN_POINT('Ctrl Pts',(40.2612994708194,46.9748,48.1724968887305));
#35878=CARTESIAN_POINT('Ctrl Pts',(40.2610287627922,46.9748,48.1977150825715));
#35879=CARTESIAN_POINT('Ctrl Pts',(40.260220477777,46.9748,48.2730120303637));
#35880=CARTESIAN_POINT('Ctrl Pts',(40.2637777325354,46.9748,48.3482521489875));
#35881=CARTESIAN_POINT('Ctrl Pts',(40.2714763918892,46.9748,48.4231811150368));
#35882=CARTESIAN_POINT('Ctrl Pts',(40.2793378346931,46.9748,48.4996944083113));
#35883=CARTESIAN_POINT('Ctrl Pts',(40.2915177567416,46.9748,48.5758840323195));
#35884=CARTESIAN_POINT('Ctrl Pts',(40.3078313114295,46.9748,48.6514834531951));
#35885=CARTESIAN_POINT('Ctrl Pts',(40.3105992632564,46.9748,48.6643105506073));
#35886=CARTESIAN_POINT('Ctrl Pts',(40.3134868120037,46.9748,48.6771226603303));
#35887=CARTESIAN_POINT('Ctrl Pts',(40.3164916889436,46.9748,48.6899120610965));
#35888=CARTESIAN_POINT('Ctrl Pts',(40.334438038668,46.9748,48.7662955747993));
#35889=CARTESIAN_POINT('Ctrl Pts',(40.3565050181593,46.9748,48.8416188377461));
#35890=CARTESIAN_POINT('Ctrl Pts',(40.3824237798636,46.9748,48.9156073690414));
#35891=CARTESIAN_POINT('Ctrl Pts',(40.4090078674698,46.9748,48.9914951610683));
#35892=CARTESIAN_POINT('Ctrl Pts',(40.4396441318805,46.9748,49.0659796543946));
#35893=CARTESIAN_POINT('Ctrl Pts',(40.4740987705517,46.9748,49.138769661897));
#35894=CARTESIAN_POINT('Ctrl Pts',(40.5085534092228,46.9748,49.2115596693994));
#35895=CARTESIAN_POINT('Ctrl Pts',(40.5468267806189,46.9748,49.2826561015899));
#35896=CARTESIAN_POINT('Ctrl Pts',(40.5887367591054,46.9748,49.3517594213202));
#35897=CARTESIAN_POINT('Ctrl Pts',(40.6024581151758,46.9748,49.3743838962045));
#35898=CARTESIAN_POINT('Ctrl Pts',(40.6165696726842,46.9748,49.3967946016751));
#35899=CARTESIAN_POINT('Ctrl Pts',(40.6310661433443,46.9748,49.4189805740005));
#35900=CARTESIAN_POINT('Ctrl Pts',(40.640039849335,46.9748,49.4327142887392));
#35901=CARTESIAN_POINT('Ctrl Pts',(40.6491610622686,46.9748,49.4463618817698));
#35902=CARTESIAN_POINT('Ctrl Pts',(40.6584286263235,46.9748,49.4599206942245));
#35903=CARTESIAN_POINT('Ctrl Pts',(40.6661836146128,46.9748,49.471266548559));
#35904=CARTESIAN_POINT('Ctrl Pts',(40.6740417848548,46.9748,49.4825510866558));
#35905=CARTESIAN_POINT('Ctrl Pts',(40.6819922247109,46.9748,49.4937586649968));
#35906=CARTESIAN_POINT('Ctrl Pts',(40.7302234805214,46.9748,49.5617493155483));
#35907=CARTESIAN_POINT('Ctrl Pts',(40.7819280150356,46.9748,49.6270299832024));
#35908=CARTESIAN_POINT('Ctrl Pts',(40.8368603491323,46.9748,49.6893013090378));
#35909=CARTESIAN_POINT('Ctrl Pts',(40.8917630700629,46.9748,49.751539065371));
#35910=CARTESIAN_POINT('Ctrl Pts',(40.9498905292052,46.9748,49.8107716637567));
#35911=CARTESIAN_POINT('Ctrl Pts',(41.0110467528271,46.9748,49.8666848752274));
#35912=CARTESIAN_POINT('Ctrl Pts',(41.0714906757508,46.9748,49.9219468525765));
#35913=CARTESIAN_POINT('Ctrl Pts',(41.1348936992962,46.9748,49.9739671882265));
#35914=CARTESIAN_POINT('Ctrl Pts',(41.201107808354,46.9748,50.0224141023343));
#35915=CARTESIAN_POINT('Ctrl Pts',(41.2364136632063,46.9748,50.0482463568473));
#35916=CARTESIAN_POINT('Ctrl Pts',(41.2725193969755,46.9748,50.07306209005));
#35917=CARTESIAN_POINT('Ctrl Pts',(41.309406738763,46.9748,50.0968063285493));
#35918=CARTESIAN_POINT('Origin',(42.4,46.9748,48.));
#35919=CARTESIAN_POINT('',(43.5298844544276,46.9748,50.0758977721803));
#35920=CARTESIAN_POINT('',(42.4,46.9748,45.63653));
#35921=CARTESIAN_POINT('Origin',(42.4,46.9748,48.));
#35922=CARTESIAN_POINT('Ctrl Pts',(43.5298844544276,46.9748,50.0758977721802));
#35923=CARTESIAN_POINT('Ctrl Pts',(43.5991352573157,46.9748,50.029019463505));
#35924=CARTESIAN_POINT('Ctrl Pts',(43.6656582922104,46.9748,49.9781660525874));
#35925=CARTESIAN_POINT('Ctrl Pts',(43.7292694101079,46.9748,49.9236952395323));
#35926=CARTESIAN_POINT('Ctrl Pts',(43.783302831196,46.9748,49.877425900522));
#35927=CARTESIAN_POINT('Ctrl Pts',(43.8352347245068,46.9748,49.8285454219465));
#35928=CARTESIAN_POINT('Ctrl Pts',(43.8849274853458,46.9748,49.7772569750236));
#35929=CARTESIAN_POINT('Ctrl Pts',(43.8965951848529,46.9748,49.7652146135855));
#35930=CARTESIAN_POINT('Ctrl Pts',(43.9081376356664,46.9748,49.7530410983771));
#35931=CARTESIAN_POINT('Ctrl Pts',(43.9195457502883,46.9748,49.7407472087553));
#35932=CARTESIAN_POINT('Ctrl Pts',(43.9760402133417,46.9748,49.6798662730318));
#35933=CARTESIAN_POINT('Ctrl Pts',(44.0292971033833,46.9748,49.6159808674749));
#35934=CARTESIAN_POINT('Ctrl Pts',(44.0791167399533,46.9748,49.5494290633886));
#35935=CARTESIAN_POINT('Ctrl Pts',(44.1148930930423,46.9748,49.501637047918));
#35936=CARTESIAN_POINT('Ctrl Pts',(44.1488959960298,46.9748,49.4524693038681));
#35937=CARTESIAN_POINT('Ctrl Pts',(44.1810358371969,46.9748,49.4020455179199));
#35938=CARTESIAN_POINT('Ctrl Pts',(44.1889018950558,46.9748,49.3897045603006));
#35939=CARTESIAN_POINT('Ctrl Pts',(44.1966562900803,46.9748,49.3772883533));
#35940=CARTESIAN_POINT('Ctrl Pts',(44.2042975790103,46.9748,49.3647986325625));
#35941=CARTESIAN_POINT('Ctrl Pts',(44.2119123601123,46.9748,49.3523522389879));
#35942=CARTESIAN_POINT('Ctrl Pts',(44.2194101741558,46.9748,49.3398403918988));
#35943=CARTESIAN_POINT('Ctrl Pts',(44.2267882958736,46.9748,49.3272680159029));
#35944=CARTESIAN_POINT('Ctrl Pts',(44.2678706899769,46.9748,49.2572633012563));
#35945=CARTESIAN_POINT('Ctrl Pts',(44.3052645362015,46.9748,49.1853532663675));
#35946=CARTESIAN_POINT('Ctrl Pts',(44.3387904821095,46.9748,49.1118543951674));
#35947=CARTESIAN_POINT('Ctrl Pts',(44.3715702155164,46.9748,49.0399914442977));
#35948=CARTESIAN_POINT('Ctrl Pts',(44.400652486977,46.9748,48.9666086718443));
#35949=CARTESIAN_POINT('Ctrl Pts',(44.4258221217546,46.9748,48.8919915357821));
#35950=CARTESIAN_POINT('Ctrl Pts',(44.450471949,46.9748,48.8189154053683));
#35951=CARTESIAN_POINT('Ctrl Pts',(44.4713692237863,46.9748,48.7446546031674));
#35952=CARTESIAN_POINT('Ctrl Pts',(44.4882633994834,46.9748,48.6694795181181));
#35953=CARTESIAN_POINT('Ctrl Pts',(44.4959612735851,46.9748,48.6352257995188));
#35954=CARTESIAN_POINT('Ctrl Pts',(44.5028273418609,46.9748,48.6007823587082));
#35955=CARTESIAN_POINT('Ctrl Pts',(44.5088343375696,46.9748,48.56617557783));
#35956=CARTESIAN_POINT('Ctrl Pts',(44.5109619703709,46.9748,48.5539181157449));
#35957=CARTESIAN_POINT('Ctrl Pts',(44.5129809047883,46.9748,48.5416451070528));
#35958=CARTESIAN_POINT('Ctrl Pts',(44.5148890604002,46.9748,48.5293655357747));
#35959=CARTESIAN_POINT('Ctrl Pts',(44.5265958064881,46.9748000000001,48.4540290055026));
#35960=CARTESIAN_POINT('Ctrl Pts',(44.5341527504262,46.9748000000001,48.378355707931));
#35961=CARTESIAN_POINT('Ctrl Pts',(44.5373669491418,46.9748000000001,48.30261096484));
#35962=CARTESIAN_POINT('Ctrl Pts',(44.5384531833379,46.9748000000001,48.2770131292999));
#35963=CARTESIAN_POINT('Ctrl Pts',(44.5390430018181,46.9748,48.2514071468793));
#35964=CARTESIAN_POINT('Ctrl Pts',(44.5391275997232,46.9748,48.2258033809724));
#35965=CARTESIAN_POINT('Ctrl Pts',(44.5393841841558,46.9748,48.1481474657363));
#35966=CARTESIAN_POINT('Ctrl Pts',(44.5349968811804,46.9748,48.0705105032779));
#35967=CARTESIAN_POINT('Ctrl Pts',(44.5261344730417,46.9748,47.9932236009828));
#35968=CARTESIAN_POINT('Ctrl Pts',(44.5175967452688,46.9748,47.9187681570591));
#35969=CARTESIAN_POINT('Ctrl Pts',(44.504905015825,46.9748,47.8446369257264));
#35970=CARTESIAN_POINT('Ctrl Pts',(44.4881708657763,46.9748,47.7711493147464));
#35971=CARTESIAN_POINT('Ctrl Pts',(44.4840507442499,46.9748,47.7530559017529));
#35972=CARTESIAN_POINT('Ctrl Pts',(44.4796836110545,46.9748,47.7349951900705));
#35973=CARTESIAN_POINT('Ctrl Pts',(44.4750802303516,46.9748,47.717007252933));
#35974=CARTESIAN_POINT('Ctrl Pts',(44.4562684669595,46.9748000000001,47.6434993596734));
#35975=CARTESIAN_POINT('Ctrl Pts',(44.433498427294,46.9748,47.5711172123902));
#35976=CARTESIAN_POINT('Ctrl Pts',(44.4069542493271,46.9748,47.5001602010979));
#35977=CARTESIAN_POINT('Ctrl Pts',(44.3805282755863,46.9748000000001,47.4295191694009));
#35978=CARTESIAN_POINT('Ctrl Pts',(44.3503610512703,46.9748000000001,47.3602897711562));
#35979=CARTESIAN_POINT('Ctrl Pts',(44.3165910991924,46.9748,47.292794375311));
#35980=CARTESIAN_POINT('Ctrl Pts',(44.283107711654,46.9748,47.2258717308571));
#35981=CARTESIAN_POINT('Ctrl Pts',(44.2460818591245,46.9748,47.1606530350058));
#35982=CARTESIAN_POINT('Ctrl Pts',(44.2056155224222,46.9748,47.0974908446937));
#35983=CARTESIAN_POINT('Ctrl Pts',(44.1908426060719,46.9748,47.0744324255229));
#35984=CARTESIAN_POINT('Ctrl Pts',(44.1756108890014,46.9748,47.0516485112693));
#35985=CARTESIAN_POINT('Ctrl Pts',(44.1599244680382,46.9748,47.0291578416167));
#35986=CARTESIAN_POINT('Ctrl Pts',(44.1531635220926,46.9748,47.0194642217554));
#35987=CARTESIAN_POINT('Ctrl Pts',(44.14631890799,46.9748,47.0098263625416));
#35988=CARTESIAN_POINT('Ctrl Pts',(44.1393981503246,46.9748,47.0002553228382));
#35989=CARTESIAN_POINT('Ctrl Pts',(44.0965694162336,46.9748000000001,46.9410254618529));
#35990=CARTESIAN_POINT('Ctrl Pts',(44.0507558491961,46.9748,46.8842480501475));
#35991=CARTESIAN_POINT('Ctrl Pts',(44.0020911747138,46.9748,46.8302142717846));
#35992=CARTESIAN_POINT('Ctrl Pts',(43.9547299363546,46.9748,46.7776277357865));
#35993=CARTESIAN_POINT('Ctrl Pts',(43.9046676139366,46.9748,46.7276393346297));
#35994=CARTESIAN_POINT('Ctrl Pts',(43.8520000209609,46.9748,46.6805567605905));
#35995=CARTESIAN_POINT('Ctrl Pts',(43.799933010938,46.9748,46.6340110820073));
#35996=CARTESIAN_POINT('Ctrl Pts',(43.745319295441,46.9748,46.5903048219264));
#35997=CARTESIAN_POINT('Ctrl Pts',(43.6882327293054,46.9748,46.5497817346553));
#35998=CARTESIAN_POINT('Ctrl Pts',(43.6621533214997,46.9748,46.5312691810016));
#35999=CARTESIAN_POINT('Ctrl Pts',(43.6355576110044,46.9748,46.5134216543318));
#36000=CARTESIAN_POINT('Ctrl Pts',(43.6084517554458,46.9748,46.4962756530335));
#36001=CARTESIAN_POINT('Origin',(42.4,46.9748,48.));
#36002=CARTESIAN_POINT('Ctrl Pts',(43.8816454908891,47.2273349779972,46.1547938147578));
#36003=CARTESIAN_POINT('Ctrl Pts',(44.4964807713991,47.1852426082705,46.6484554351011));
#36004=CARTESIAN_POINT('Ctrl Pts',(45.1824651975149,47.1010749910753,48.2904339462144));
#36005=CARTESIAN_POINT('Ctrl Pts',(43.6585580275758,46.9748321264113,50.5015145553006));
#36006=CARTESIAN_POINT('Ctrl Pts',(40.9780001174031,46.8486063840055,50.4096758350311));
#36007=CARTESIAN_POINT('Ctrl Pts',(39.6036218446586,46.7223806415996,48.1087275911241));
#36008=CARTESIAN_POINT('Ctrl Pts',(40.7959828223584,46.5961548991938,45.7064576286955));
#36009=CARTESIAN_POINT('Ctrl Pts',(43.4610518931062,46.4699291567879,45.410456497768));
#36010=CARTESIAN_POINT('Ctrl Pts',(45.1519601603745,46.3437034143821,47.4913191856257));
#36011=CARTESIAN_POINT('Ctrl Pts',(44.3165710055188,46.2174776719761,50.0393512686995));
#36012=CARTESIAN_POINT('Ctrl Pts',(41.7217124725944,46.0912519295704,50.7151277184636));
#36013=CARTESIAN_POINT('Ctrl Pts',(39.7495457958656,45.9650261871645,48.8984192274595));
#36014=CARTESIAN_POINT('Ctrl Pts',(40.2105349755461,45.8388004447587,46.2569221858256));
#36015=CARTESIAN_POINT('Ctrl Pts',(42.6814934434515,45.7125747023527,45.2156125251515));
#36016=CARTESIAN_POINT('Ctrl Pts',(44.8940345654646,45.586348959947,46.7304117848254));
#36017=CARTESIAN_POINT('Ctrl Pts',(44.8170102955553,45.460123217541,49.4107177431346));
#36018=CARTESIAN_POINT('Ctrl Pts',(42.5211290349961,45.3338974751353,50.7959592378664));
#36019=CARTESIAN_POINT('Ctrl Pts',(40.1140494587796,45.2076717327294,49.6144633468875));
#36020=CARTESIAN_POINT('Ctrl Pts',(39.8055112890285,45.0814459903235,46.9508622273783));
#36021=CARTESIAN_POINT('Ctrl Pts',(41.8787579687848,44.9552202479177,45.2503876399901));
#36022=CARTESIAN_POINT('Ctrl Pts',(44.4305136800393,44.8289945055118,46.0741039016234));
#36023=CARTESIAN_POINT('Ctrl Pts',(45.1182232833989,44.702768763106,48.6658256135953));
#36024=CARTESIAN_POINT('Ctrl Pts',(43.3105576378377,44.5765430207001,50.6463080535969));
#36025=CARTESIAN_POINT('Ctrl Pts',(40.6669845849055,44.4503172782943,50.1974346689313));
#36026=CARTESIAN_POINT('Ctrl Pts',(39.6143491799657,44.3240915358884,47.7312788480869));
#36027=CARTESIAN_POINT('Ctrl Pts',(41.1189886446677,44.1978657934826,45.511813621966));
#36028=CARTESIAN_POINT('Ctrl Pts',(43.7996183379206,44.0716400510767,45.5765458419894));
#36029=CARTESIAN_POINT('Ctrl Pts',(45.1953745735294,43.9454143086709,47.8660502307715));
#36030=CARTESIAN_POINT('Ctrl Pts',(44.0249293689912,43.819188566265,50.2785227873245));
#36031=CARTESIAN_POINT('Ctrl Pts',(41.3627713449932,43.6929628238591,50.599272641384));
#36032=CARTESIAN_POINT('Ctrl Pts',(39.6528068814801,43.5667370814533,48.5338459669609));
#36033=CARTESIAN_POINT('Ctrl Pts',(40.4648124622021,43.4405113390474,45.9783396080465));
#36034=CARTESIAN_POINT('Ctrl Pts',(43.0533531424619,43.3142855966417,45.2787519006654));
#36035=CARTESIAN_POINT('Ctrl Pts',(45.0421045168773,43.1880598542357,47.0773162682832));
#36036=CARTESIAN_POINT('Ctrl Pts',(44.6053589721454,43.0618341118299,49.7229200070962));
#36037=CARTESIAN_POINT('Ctrl Pts',(42.1440563524087,42.935608369424,50.7868538526695));
#36038=CARTESIAN_POINT('Ctrl Pts',(39.917714357712,42.8093826270182,49.2924084249837));
#36039=CARTESIAN_POINT('Ctrl Pts',(39.9701528349268,42.6831568846123,46.6115100643995));
#36040=CARTESIAN_POINT('Ctrl Pts',(42.2532323693868,42.5569311422065,45.2052690989143));
#36041=CARTESIAN_POINT('Ctrl Pts',(44.6710470869588,42.4307053998006,46.3646386712122));
#36042=CARTESIAN_POINT('Ctrl Pts',(45.0040019220144,42.3044796573948,49.0252977796835));
#36043=CARTESIAN_POINT('Ctrl Pts',(42.946438668573,42.1782539149889,50.7447160742719));
#36044=CARTESIAN_POINT('Ctrl Pts',(40.3872354161611,42.0520281725831,49.9444382934213));
#36045=CARTESIAN_POINT('Ctrl Pts',(39.6757843120393,41.9258024301772,47.3591330619018));
#36046=CARTESIAN_POINT('Ctrl Pts',(41.4652095797749,41.7995766877714,45.3621545880901));
#36047=CARTESIAN_POINT('Ctrl Pts',(44.1127883648371,41.6733509453655,45.7867631025674));
#36048=CARTESIAN_POINT('Ctrl Pts',(45.1879982767062,41.5471252029597,48.2431607615583));
#36049=CARTESIAN_POINT('Ctrl Pts',(43.7037783145724,41.4208994605538,50.4763327024714));
#36050=CARTESIAN_POINT('Ctrl Pts',(41.0226676673639,41.294673718148,50.4361890715529));
#36051=CARTESIAN_POINT('Ctrl Pts',(39.6059715458142,41.1684479757421,48.1595824052919));
#36052=CARTESIAN_POINT('Ctrl Pts',(40.7542411038366,41.0422222333363,45.7364763746368));
#36053=CARTESIAN_POINT('Ctrl Pts',(43.4133453418658,40.9159964909304,45.3913235606926));
#36054=CARTESIAN_POINT('Ctrl Pts',(45.1421813073775,40.7897707485246,47.4409801216879));
#36055=CARTESIAN_POINT('Ctrl Pts',(44.3536481566047,40.6635450061187,50.0038264463454));
#36056=CARTESIAN_POINT('Ctrl Pts',(41.771632743995,40.5373192637129,50.7271259850728));
#36057=CARTESIAN_POINT('Ctrl Pts',(39.7664691681677,40.411093521307,48.946877449656));
#36058=CARTESIAN_POINT('Ctrl Pts',(40.1789317226774,40.2848677789012,46.2973792981554));
#36059=CARTESIAN_POINT('Ctrl Pts',(42.6303727617419,40.1586420364953,45.2109159321516));
#36060=CARTESIAN_POINT('Ctrl Pts',(44.8703276842312,40.0324162940895,46.6848792149011));
#36061=CARTESIAN_POINT('Ctrl Pts',(44.8424797438481,39.9061905516836,49.3661457637348));
#36062=CARTESIAN_POINT('Ctrl Pts',(42.5723938238785,39.7799648092778,50.7932672475736));
#36063=CARTESIAN_POINT('Ctrl Pts',(40.1440474391825,39.6537390668719,49.6561218524672));
#36064=CARTESIAN_POINT('Ctrl Pts',(39.7867039050733,39.527513324466,46.998628407074));
#36065=CARTESIAN_POINT('Ctrl Pts',(41.8284106683955,39.4012875820602,45.2604111288599));
#36066=CARTESIAN_POINT('Ctrl Pts',(44.3948461674537,39.2750618396543,46.0371830663371));
#36067=CARTESIAN_POINT('Ctrl Pts',(45.1299789294624,39.1488360972485,48.6158543590574));
#36068=CARTESIAN_POINT('Ctrl Pts',(43.3589445658158,39.0226103548426,50.6291608673817));
#36069=CARTESIAN_POINT('Ctrl Pts',(40.7075827680497,38.8963846124368,50.228852947118));
#36070=CARTESIAN_POINT('Ctrl Pts',(39.6098887967391,38.7701588700309,47.7824200829205));
#36071=CARTESIAN_POINT('Ctrl Pts',(41.0735644019736,38.6439331276251,45.5357292861443));
#36072=CARTESIAN_POINT('Ctrl Pts',(43.7549304641552,38.5177073852192,45.5512809503369));
#36073=CARTESIAN_POINT('Ctrl Pts',(45.1924472972574,38.3914816428134,47.8147983830566));
#36074=CARTESIAN_POINT('Ctrl Pts',(44.0664499797616,38.2652559004075,50.2483340525446));
#36075=CARTESIAN_POINT('Ctrl Pts',(41.4106232153221,38.1390301580017,50.6178607917188));
#36076=CARTESIAN_POINT('Ctrl Pts',(39.6630611799201,38.0128044155958,48.5841467641083));
#36077=CARTESIAN_POINT('Ctrl Pts',(40.4280555682283,37.8865786731899,46.0141760639767));
#36078=CARTESIAN_POINT('Ctrl Pts',(43.0033285104073,37.7603529307841,45.2672255388693));
#36079=CARTESIAN_POINT('Ctrl Pts',(45.0247356104603,37.6341271883782,47.0290084850729));
#36080=CARTESIAN_POINT('Ctrl Pts',(44.6365907431038,37.5079014459724,49.6821781697375));
#36081=CARTESIAN_POINT('Ctrl Pts',(42.1952175033893,37.3816757035665,50.7910796613426));
#36082=CARTESIAN_POINT('Ctrl Pts',(39.9418380812742,37.2554499611607,49.3377225153987));
#36083=CARTESIAN_POINT('Ctrl Pts',(39.9450931422177,37.1292242187548,46.6563133302395));
#36084=CARTESIAN_POINT('Ctrl Pts',(42.2019944848676,37.002998476349,45.2084313795187));
#36085=CARTESIAN_POINT('Ctrl Pts',(44.6406682607653,36.8767727339431,46.3232569391591));
#36086=CARTESIAN_POINT('Ctrl Pts',(45.0223704336859,36.7505469915373,48.9773611693779));
#36087=CARTESIAN_POINT('Ctrl Pts',(42.9966919117353,36.6243212491314,50.7342312099288));
#36088=CARTESIAN_POINT('Ctrl Pts',(40.4232400582042,36.4980955067256,49.9810304589759));
#36089=CARTESIAN_POINT('Ctrl Pts',(39.6644874787135,36.3718697643197,47.4092100265205));
#36090=CARTESIAN_POINT('Ctrl Pts',(41.416981956363,36.2456440219139,45.3797448458667));
#36091=CARTESIAN_POINT('Ctrl Pts',(44.0719037305385,36.119418279508,45.7557184974497));
#36092=CARTESIAN_POINT('Ctrl Pts',(45.1919894217268,35.9931925371022,48.1919807694713));
#36093=CARTESIAN_POINT('Ctrl Pts',(43.7489812998462,35.8669667946963,50.4520014273119));
#36094=CARTESIAN_POINT('Ctrl Pts',(41.067585382989,35.7407410522905,50.4610430380741));
#36095=CARTESIAN_POINT('Ctrl Pts',(39.6093687642723,35.6145153098846,48.2108052491722));
#36096=CARTESIAN_POINT('Ctrl Pts',(40.7129991207698,35.4882895674788,45.7670446533085));
#36097=CARTESIAN_POINT('Ctrl Pts',(43.365324999706,35.3620638250729,45.3731750740055));
#36098=CARTESIAN_POINT('Ctrl Pts',(45.1314660976564,35.2358380826671,47.3907754893571));
#36099=CARTESIAN_POINT('Ctrl Pts',(44.3900748241373,35.1096123402612,49.9676543753674));
#36100=CARTESIAN_POINT('Ctrl Pts',(41.821760988144,34.9833865978554,50.7381930523941));
#36101=CARTESIAN_POINT('Ctrl Pts',(39.784280407157,34.8571608554495,48.9950238989286));
#36102=CARTESIAN_POINT('Ctrl Pts',(40.1480749367121,34.7309351130437,46.3384058697562));
#36103=CARTESIAN_POINT('Ctrl Pts',(42.5791750040333,34.6047093706378,45.2071595343498));
#36104=CARTESIAN_POINT('Ctrl Pts',(44.8457893708704,34.478483628232,46.6397882861432));
#36105=CARTESIAN_POINT('Ctrl Pts',(44.8671274581151,34.3522578858261,49.3211145415032));
#36106=CARTESIAN_POINT('Ctrl Pts',(42.623600556591,34.2260321434202,50.7896351656127));
#36107=CARTESIAN_POINT('Ctrl Pts',(40.174804514126,34.0998064010144,49.6972232134327));
#36108=CARTESIAN_POINT('Ctrl Pts',(39.7687758515636,33.9735806586085,47.0467314826819));
#36109=CARTESIAN_POINT('Ctrl Pts',(41.7782556499994,33.8473549162027,45.2713564357832));
#36110=CARTESIAN_POINT('Ctrl Pts',(44.3585075330677,33.7211291737969,46.000922708281));
#36111=CARTESIAN_POINT('Ctrl Pts',(45.1408157896746,33.594903431391,48.5656757993766));
#36112=CARTESIAN_POINT('Ctrl Pts',(43.4070092426123,33.4686776889851,50.6111292011137));
#36113=CARTESIAN_POINT('Ctrl Pts',(40.7487495907286,33.3424519465793,50.2595209084501));
#36114=CARTESIAN_POINT('Ctrl Pts',(39.6063688620587,33.2162262041734,47.8336352383348));
#36115=CARTESIAN_POINT('Ctrl Pts',(41.0285832239457,33.0900004617676,45.5604727126079));
#36116=CARTESIAN_POINT('Ctrl Pts',(43.7097931512442,32.9637747193617,45.5268428077786));
#36117=CARTESIAN_POINT('Ctrl Pts',(45.188567568384,32.8375489769558,47.763603269987));
#36118=CARTESIAN_POINT('Ctrl Pts',(44.1074354187682,32.7113232345501,50.2173998978709));
#36119=CARTESIAN_POINT('Ctrl Pts',(41.4587571919215,32.5850974921442,50.635546029088));
#36120=CARTESIAN_POINT('Ctrl Pts',(39.6743373833067,32.4588717497383,48.6342948602794));
#36121=CARTESIAN_POINT('Ctrl Pts',(40.3917614339282,32.3326460073325,46.0505935321538));
#36122=CARTESIAN_POINT('Ctrl Pts',(42.9535000609079,32.2064202649266,45.2567919948868));
#36123=CARTESIAN_POINT('Ctrl Pts',(45.0056887756311,32.0801945225208,46.9806829244104));
#36124=CARTESIAN_POINT('Ctrl Pts',(44.6686649560567,31.9539687801149,49.641554962929));
#36125=CARTESIAN_POINT('Ctrl Pts',(42.2430969350261,31.8277430377091,50.7930037613584));
#36126=CARTESIAN_POINT('Ctrl Pts',(40.7318882605603,31.7435925427718,49.8543657264344));
#36127=CARTESIAN_POINT('Ctrl Pts',(40.3425084896344,31.7015172953032,49.1690970811863));
#36128=CARTESIAN_POINT('Ctrl Pts',(43.7896421530199,47.1424960903491,46.2693725916266));
#36129=CARTESIAN_POINT('Ctrl Pts',(44.3662990039429,47.1004037206223,46.7323801067006));
#36130=CARTESIAN_POINT('Ctrl Pts',(45.0096869673307,47.0162361034272,48.2723993403344));
#36131=CARTESIAN_POINT('Ctrl Pts',(43.5804073902262,46.8899932387631,50.3461820616432));
#36132=CARTESIAN_POINT('Ctrl Pts',(41.066299738637,46.7637674963574,50.2600461014889));
#36133=CARTESIAN_POINT('Ctrl Pts',(39.7772640052281,46.6375417539514,48.1019761101771));
#36134=CARTESIAN_POINT('Ctrl Pts',(40.8955848764598,46.5113160115457,45.8488760108268));
#36135=CARTESIAN_POINT('Ctrl Pts',(43.3951654739739,46.3850902691396,45.5712551822226));
#36136=CARTESIAN_POINT('Ctrl Pts',(44.9810761520241,46.258864526734,47.5229059134362));
#36137=CARTESIAN_POINT('Ctrl Pts',(44.1975608031085,46.132638784328,49.9127169793489));
#36138=CARTESIAN_POINT('Ctrl Pts',(41.7638309934822,46.0064130419222,50.5465308345424));
#36139=CARTESIAN_POINT('Ctrl Pts',(39.9141267534222,45.8801872995164,48.8426315452909));
#36140=CARTESIAN_POINT('Ctrl Pts',(40.3464906354096,45.7539615571105,46.365159262816));
#36141=CARTESIAN_POINT('Ctrl Pts',(42.6640140014762,45.6277358147047,45.3885101198748));
#36142=CARTESIAN_POINT('Ctrl Pts',(44.7391665446088,45.5015100722988,46.8092473458512));
#36143=CARTESIAN_POINT('Ctrl Pts',(44.6669251259093,45.3752843298929,49.3231186906233));
#36144=CARTESIAN_POINT('Ctrl Pts',(42.5136074816954,45.249058587487,50.6223430901361));
#36145=CARTESIAN_POINT('Ctrl Pts',(40.2559964233466,45.1228328450813,49.5142126339507));
#36146=CARTESIAN_POINT('Ctrl Pts',(39.9666170480926,44.9966071026753,47.0160088346871));
#36147=CARTESIAN_POINT('Ctrl Pts',(41.911124690112,44.8703813602696,45.4211258607879));
#36148=CARTESIAN_POINT('Ctrl Pts',(44.3044281641036,44.7441556178636,46.1936931492063));
#36149=CARTESIAN_POINT('Ctrl Pts',(44.9494341792005,44.6179298754578,48.624480919965));
#36150=CARTESIAN_POINT('Ctrl Pts',(43.2540162164799,44.491704133052,50.4819845528282));
#36151=CARTESIAN_POINT('Ctrl Pts',(40.7745968334143,44.3654783906461,50.0609841309757));
#36152=CARTESIAN_POINT('Ctrl Pts',(39.7873252225867,44.2392526482402,47.7479651897821));
#36153=CARTESIAN_POINT('Ctrl Pts',(41.1985335299076,44.1130269058345,45.6663184974085));
#36154=CARTESIAN_POINT('Ctrl Pts',(43.7127085071794,43.9868011634285,45.727031145715));
#36155=CARTESIAN_POINT('Ctrl Pts',(45.0217947307526,43.8605754210227,47.8743678924197));
#36156=CARTESIAN_POINT('Ctrl Pts',(43.9240287644484,43.7343496786169,50.1370370519486));
#36157=CARTESIAN_POINT('Ctrl Pts',(41.4271784511338,43.6081239362109,50.4378698223493));
#36158=CARTESIAN_POINT('Ctrl Pts',(39.8233948785613,43.4818981938052,48.5006965994701));
#36159=CARTESIAN_POINT('Ctrl Pts',(40.5849786652346,43.3556724513993,46.1038753757059));
#36160=CARTESIAN_POINT('Ctrl Pts',(43.01278293165,43.2294467089935,45.4477288319546));
#36161=CARTESIAN_POINT('Ctrl Pts',(44.878042036313,43.1032209665876,47.1346106640329));
#36162=CARTESIAN_POINT('Ctrl Pts',(44.4684163715807,42.9769952241817,49.6159346367703));
#36163=CARTESIAN_POINT('Ctrl Pts',(42.1599492701339,42.8507694817759,50.6138031072814));
#36164=CARTESIAN_POINT('Ctrl Pts',(40.0718528247337,42.72454373937,49.2121558343877));
#36165=CARTESIAN_POINT('Ctrl Pts',(40.121035114847,42.5983179969642,46.6977288727842));
#36166=CARTESIAN_POINT('Ctrl Pts',(42.2623459609919,42.4720922545583,45.378808972607));
#36167=CARTESIAN_POINT('Ctrl Pts',(44.5300255580282,42.3458665121525,46.4661870522494));
#36168=CARTESIAN_POINT('Ctrl Pts',(44.842305436508,42.2196407697466,48.9616315257646));
#36169=CARTESIAN_POINT('Ctrl Pts',(42.9125073525067,42.0934150273407,50.5742818901914));
#36170=CARTESIAN_POINT('Ctrl Pts',(40.5122187952467,41.9671892849349,49.823697661215));
#36171=CARTESIAN_POINT('Ctrl Pts',(39.8449455168682,41.840963542529,47.3989279371251));
#36172=CARTESIAN_POINT('Ctrl Pts',(41.5232557449324,41.7147378001232,45.5259525979185));
#36173=CARTESIAN_POINT('Ctrl Pts',(44.0064321226742,41.5885120577173,45.9241948858863));
#36174=CARTESIAN_POINT('Ctrl Pts',(45.0148764678742,41.4622863153115,48.2280616019822));
#36175=CARTESIAN_POINT('Ctrl Pts',(43.6228197063765,41.3360605729056,50.3225638855021));
#36176=CARTESIAN_POINT('Ctrl Pts',(41.1081936401671,41.2098348304998,50.2849129885481));
#36177=CARTESIAN_POINT('Ctrl Pts',(39.7794678008006,41.0836090880939,48.1496730754001));
#36178=CARTESIAN_POINT('Ctrl Pts',(40.8564351257576,40.9573833456881,45.8770307313704));
#36179=CARTESIAN_POINT('Ctrl Pts',(43.3504212790996,40.8311576032823,45.5533103121206));
#36180=CARTESIAN_POINT('Ctrl Pts',(44.9719045206072,40.7049318608764,47.4756926727375));
#36181=CARTESIAN_POINT('Ctrl Pts',(44.2323356344563,40.5787061184706,49.8793980842926));
#36182=CARTESIAN_POINT('Ctrl Pts',(41.810651446725,40.4524803760646,50.5577840642425));
#36183=CARTESIAN_POINT('Ctrl Pts',(39.9299992625121,40.3262546336588,48.8880807358286));
#36184=CARTESIAN_POINT('Ctrl Pts',(40.3168497984963,40.200028891253,46.4031041754342));
#36185=CARTESIAN_POINT('Ctrl Pts',(42.6160676778573,40.0738031488471,45.3841051635958));
#36186=CARTESIAN_POINT('Ctrl Pts',(44.7169317511437,39.9475774064413,46.7665421380998));
#36187=CARTESIAN_POINT('Ctrl Pts',(44.6908130391648,39.8213516640354,49.2813144251639));
#36188=CARTESIAN_POINT('Ctrl Pts',(42.5616889640978,39.6951259216296,50.61981826));
#36189=CARTESIAN_POINT('Ctrl Pts',(40.284131667796,39.5689001792237,49.5532843388501));
#36190=CARTESIAN_POINT('Ctrl Pts',(39.9489775157664,39.4426744368179,47.0608089553651));
#36191=CARTESIAN_POINT('Ctrl Pts',(41.8639037244077,39.316448694412,45.4305269373203));
#36192=CARTESIAN_POINT('Ctrl Pts',(44.2709754392195,39.1902229520062,46.1590649271693));
#36193=CARTESIAN_POINT('Ctrl Pts',(44.9604598539699,39.0639972096003,48.5776126494022));
#36194=CARTESIAN_POINT('Ctrl Pts',(43.2993985398404,38.9377714671945,50.4659021276348));
#36195=CARTESIAN_POINT('Ctrl Pts',(40.8126740570015,38.8115457247886,50.0904514792801));
#36196=CARTESIAN_POINT('Ctrl Pts',(39.7831418085458,38.6853199823828,47.795930790271));
#36197=CARTESIAN_POINT('Ctrl Pts',(41.1559299227662,38.5590942399769,45.6887491093625));
#36198=CARTESIAN_POINT('Ctrl Pts',(43.6707955438592,38.432868497571,45.7033350870777));
#36199=CARTESIAN_POINT('Ctrl Pts',(45.0190492248093,38.3066427551652,47.8262985475982));
#36200=CARTESIAN_POINT('Ctrl Pts',(43.9629711371687,38.1804170127594,50.1087228980875));
#36201=CARTESIAN_POINT('Ctrl Pts',(41.4720589414524,38.0541912703535,50.4553037344496));
#36202=CARTESIAN_POINT('Ctrl Pts',(39.8330124324563,37.9279655279477,48.5478739495694));
#36203=CARTESIAN_POINT('Ctrl Pts',(40.5505042045122,37.8017397855418,46.1374865533334));
#36204=CARTESIAN_POINT('Ctrl Pts',(42.9658645980677,37.6755140431359,45.4369182039595));
#36205=CARTESIAN_POINT('Ctrl Pts',(44.8617516587178,37.5492883007301,47.0893025709156));
#36206=CARTESIAN_POINT('Ctrl Pts',(44.4977087938937,37.4230625583242,49.5777226792316));
#36207=CARTESIAN_POINT('Ctrl Pts',(42.2079335500693,37.2968368159184,50.6177665127646));
#36208=CARTESIAN_POINT('Ctrl Pts',(40.0944785765455,37.1706110735125,49.2546561291975));
#36209=CARTESIAN_POINT('Ctrl Pts',(40.0975315132471,37.0443853311067,46.7397500628646));
#36210=CARTESIAN_POINT('Ctrl Pts',(42.2142897123163,36.9181595887008,45.3817748901996));
#36211=CARTESIAN_POINT('Ctrl Pts',(44.5015331165518,36.791933846295,46.4273749345198));
#36212=CARTESIAN_POINT('Ctrl Pts',(44.8595333484911,36.6657081038891,48.9166715574299));
#36213=CARTESIAN_POINT('Ctrl Pts',(42.9596401015033,36.5394823614832,50.5644480874703));
#36214=CARTESIAN_POINT('Ctrl Pts',(40.5459877154068,36.4132566190774,49.8580176223918));
#36215=CARTESIAN_POINT('Ctrl Pts',(39.834350164686,36.2870308766715,47.4458953536611));
#36216=CARTESIAN_POINT('Ctrl Pts',(41.4780228340604,36.1608051342657,45.5424505819768));
#36217=CARTESIAN_POINT('Ctrl Pts',(43.9680862352258,36.0345793918598,45.89507800728));
#36218=CARTESIAN_POINT('Ctrl Pts',(45.0186197812332,35.908353649454,48.1800596508862));
#36219=CARTESIAN_POINT('Ctrl Pts',(43.6652157951609,35.7821279070482,50.2997434700879));
#36220=CARTESIAN_POINT('Ctrl Pts',(41.1503221732296,35.6559021646423,50.3082236386059));
#36221=CARTESIAN_POINT('Ctrl Pts',(39.782654067692,35.5296764222365,48.197715217391));
#36222=CARTESIAN_POINT('Ctrl Pts',(40.8177540792481,35.4034506798305,45.9057008612016));
#36223=CARTESIAN_POINT('Ctrl Pts',(43.3053827782721,35.2772249374248,45.5362887625874));
#36224=CARTESIAN_POINT('Ctrl Pts',(44.9618546758917,35.1509991950188,47.4286055160642));
#36225=CARTESIAN_POINT('Ctrl Pts',(44.2665003742732,35.0247734526131,49.8454721317606));
#36226=CARTESIAN_POINT('Ctrl Pts',(41.8576669585695,34.8985477102072,50.5681639178273));
#36227=CARTESIAN_POINT('Ctrl Pts',(39.9467045058711,34.7723219678014,48.9332375131001));
#36228=CARTESIAN_POINT('Ctrl Pts',(40.2879090763414,34.6460962253955,46.4415831865344));
#36229=CARTESIAN_POINT('Ctrl Pts',(42.5680490643027,34.5198704829896,45.3805820207381));
#36230=CARTESIAN_POINT('Ctrl Pts',(44.693917153644,34.3936447405838,46.7242511476396));
#36231=CARTESIAN_POINT('Ctrl Pts',(44.71393024428,34.2674189981779,49.2390794337307));
#36232=CARTESIAN_POINT('Ctrl Pts',(42.60971599535,34.1411932557721,50.616411713544));
#36233=CARTESIAN_POINT('Ctrl Pts',(40.3129788705228,34.0149675133662,49.591833495241));
#36234=CARTESIAN_POINT('Ctrl Pts',(39.932162711529,33.8887417709604,47.1059250522761));
#36235=CARTESIAN_POINT('Ctrl Pts',(41.8168631008729,33.7625160285545,45.4407925912651));
#36236=CARTESIAN_POINT('Ctrl Pts',(44.2368932660975,33.6362902861487,46.1250561697789));
#36237=CARTESIAN_POINT('Ctrl Pts',(44.9706237952432,33.5100645437428,48.5305499463878));
#36238=CARTESIAN_POINT('Ctrl Pts',(43.3444786223289,33.383838801337,50.4489901445125));
#36239=CARTESIAN_POINT('Ctrl Pts',(40.8512846102357,33.2576130589311,50.1192151019391));
#36240=CARTESIAN_POINT('Ctrl Pts',(39.7798404455423,33.1313873165252,47.8439657212142));
#36241=CARTESIAN_POINT('Ctrl Pts',(41.1137418680227,33.0051615741194,45.7119560833894));
#36242=CARTESIAN_POINT('Ctrl Pts',(43.6284610494873,32.8789358317135,45.6804144402365));
#36243=CARTESIAN_POINT('Ctrl Pts',(45.0154104091695,32.7527100893077,47.7782824144628));
#36244=CARTESIAN_POINT('Ctrl Pts',(44.0014115698186,32.6264843469018,50.0797096114633));
#36245=CARTESIAN_POINT('Ctrl Pts',(41.5172040205462,32.500258604496,50.4718908003069));
#36246=CARTESIAN_POINT('Ctrl Pts',(39.8435884357232,32.3740328620901,48.5949080807171));
#36247=CARTESIAN_POINT('Ctrl Pts',(40.5164637682265,32.2478071196843,46.1716426650325));
#36248=CARTESIAN_POINT('Ctrl Pts',(42.9191302650105,32.1215813772784,45.4271325348419));
#36249=CARTESIAN_POINT('Ctrl Pts',(44.8438875443106,31.9953556348726,47.0439778042436));
#36250=CARTESIAN_POINT('Ctrl Pts',(44.5277913464465,31.8691298924667,49.5396219858342));
#36251=CARTESIAN_POINT('Ctrl Pts',(42.2528398902663,31.7429041500609,50.6195711350613));
#36252=CARTESIAN_POINT('Ctrl Pts',(40.8354702907496,31.6587536551236,49.7392181843865));
#36253=CARTESIAN_POINT('Ctrl Pts',(40.470269204161,31.616678407655,49.0965015551825));
#36254=CARTESIAN_POINT('Ctrl Pts',(43.6976388151507,47.0576572027009,46.3839513684954));
#36255=CARTESIAN_POINT('Ctrl Pts',(44.2361172364869,47.0155648329742,46.8163047783));
#36256=CARTESIAN_POINT('Ctrl Pts',(44.8369087371464,46.9313972157789,48.2543647344542));
#36257=CARTESIAN_POINT('Ctrl Pts',(43.5022567528767,46.805154351115,50.1908495679857));
#36258=CARTESIAN_POINT('Ctrl Pts',(41.1545993598711,46.6789286087091,50.1104163679468));
#36259=CARTESIAN_POINT('Ctrl Pts',(39.9509061657975,46.5527028663033,48.0952246292301));
#36260=CARTESIAN_POINT('Ctrl Pts',(40.9951869305611,46.4264771238975,45.9912943929581));
#36261=CARTESIAN_POINT('Ctrl Pts',(43.3292790548416,46.3002513814916,45.7320538666771));
#36262=CARTESIAN_POINT('Ctrl Pts',(44.8101921436736,46.1740256390857,47.5544926412469));
#36263=CARTESIAN_POINT('Ctrl Pts',(44.078550600698,46.0477998966799,49.7860826899984));
#36264=CARTESIAN_POINT('Ctrl Pts',(41.8059495143702,45.921574154274,50.3779339506211));
#36265=CARTESIAN_POINT('Ctrl Pts',(40.0787077109787,45.7953484118682,48.7868438631224));
#36266=CARTESIAN_POINT('Ctrl Pts',(40.4824462952732,45.6691226694624,46.4733963398063));
#36267=CARTESIAN_POINT('Ctrl Pts',(42.6465345595011,45.5428969270565,45.5614077145981));
#36268=CARTESIAN_POINT('Ctrl Pts',(44.584298523753,45.4166711846506,46.8880829068769));
#36269=CARTESIAN_POINT('Ctrl Pts',(44.5168399562632,45.2904454422447,49.2355196381119));
#36270=CARTESIAN_POINT('Ctrl Pts',(42.5060859283947,45.1642196998389,50.4487269424059));
#36271=CARTESIAN_POINT('Ctrl Pts',(40.3979433879137,45.037993957433,49.413961921014));
#36272=CARTESIAN_POINT('Ctrl Pts',(40.1277228071566,44.9117682150272,47.081155441996));
#36273=CARTESIAN_POINT('Ctrl Pts',(41.9434914114395,44.7855424726214,45.5918640815856));
#36274=CARTESIAN_POINT('Ctrl Pts',(44.1783426481677,44.6593167302155,46.3132823967892));
#36275=CARTESIAN_POINT('Ctrl Pts',(44.7806450750023,44.5330909878097,48.5831362263346));
#36276=CARTESIAN_POINT('Ctrl Pts',(43.197474795122,44.4068652454038,50.3176610520595));
#36277=CARTESIAN_POINT('Ctrl Pts',(40.8822090819232,44.2806395029979,49.9245335930203));
#36278=CARTESIAN_POINT('Ctrl Pts',(39.9603012652077,44.1544137605921,47.7646515314772));
#36279=CARTESIAN_POINT('Ctrl Pts',(41.2780784151475,44.0281880181862,45.8208233728511));
#36280=CARTESIAN_POINT('Ctrl Pts',(43.6257986764382,43.9019622757804,45.8775164494406));
#36281=CARTESIAN_POINT('Ctrl Pts',(44.8482148879759,43.7757365333745,47.882685554068));
#36282=CARTESIAN_POINT('Ctrl Pts',(43.8231281599055,43.6495107909687,49.9955513165726));
#36283=CARTESIAN_POINT('Ctrl Pts',(41.4915855572742,43.5232850485628,50.2764670033147));
#36284=CARTESIAN_POINT('Ctrl Pts',(39.9939828756426,43.397059306157,48.4675472319794));
#36285=CARTESIAN_POINT('Ctrl Pts',(40.7051448682671,43.2708335637511,46.2294111433652));
#36286=CARTESIAN_POINT('Ctrl Pts',(42.9722127208382,43.1446078213453,45.6167057632439));
#36287=CARTESIAN_POINT('Ctrl Pts',(44.7139795557488,43.0183820789394,47.1919050597825));
#36288=CARTESIAN_POINT('Ctrl Pts',(44.3314737710161,42.8921563365336,49.5089492664443));
#36289=CARTESIAN_POINT('Ctrl Pts',(42.1758421878593,42.7659305941277,50.4407523618933));
#36290=CARTESIAN_POINT('Ctrl Pts',(40.2259912917555,42.6397048517219,49.1319032437917));
#36291=CARTESIAN_POINT('Ctrl Pts',(40.2719173947672,42.513479109316,46.7839476811689));
#36292=CARTESIAN_POINT('Ctrl Pts',(42.2714595525971,42.3872533669102,45.5523488462996));
#36293=CARTESIAN_POINT('Ctrl Pts',(44.3890040290975,42.2610276245043,46.5677354332865));
#36294=CARTESIAN_POINT('Ctrl Pts',(44.6806089510015,42.1348018820984,48.8979652718457));
#36295=CARTESIAN_POINT('Ctrl Pts',(42.8785760364404,42.0085761396926,50.4038477061108));
#36296=CARTESIAN_POINT('Ctrl Pts',(40.6372021743322,41.8823503972867,49.7029570290087));
#36297=CARTESIAN_POINT('Ctrl Pts',(40.0141067216971,41.7561246548809,47.4387228123483));
#36298=CARTESIAN_POINT('Ctrl Pts',(41.5813019100897,41.629898912475,45.6897506077468));
#36299=CARTESIAN_POINT('Ctrl Pts',(43.9000758805113,41.5036731700692,46.0616266692049));
#36300=CARTESIAN_POINT('Ctrl Pts',(44.841754659042,41.3774474276633,48.2129624424062));
#36301=CARTESIAN_POINT('Ctrl Pts',(43.5418610981805,41.2512216852575,50.1687950685326));
#36302=CARTESIAN_POINT('Ctrl Pts',(41.1937196129703,41.1249959428516,50.1336369055434));
#36303=CARTESIAN_POINT('Ctrl Pts',(39.9529640557869,40.9987702004458,48.139763745508));
#36304=CARTESIAN_POINT('Ctrl Pts',(40.9586291476786,40.87254445804,46.0175850881041));
#36305=CARTESIAN_POINT('Ctrl Pts',(43.2874972163334,40.746318715634,45.7152970635486));
#36306=CARTESIAN_POINT('Ctrl Pts',(44.8016277338369,40.6200929732283,47.5104052237872));
#36307=CARTESIAN_POINT('Ctrl Pts',(44.1110231123078,40.4938672308223,49.7549697222396));
#36308=CARTESIAN_POINT('Ctrl Pts',(41.8496701494549,40.3676414884165,50.3884421434123));
#36309=CARTESIAN_POINT('Ctrl Pts',(40.0935293568565,40.2414157460107,48.8292840220013));
#36310=CARTESIAN_POINT('Ctrl Pts',(40.4547678743152,40.1151900036048,46.508829052713));
#36311=CARTESIAN_POINT('Ctrl Pts',(42.6017625939728,39.988964261199,45.55729439504));
#36312=CARTESIAN_POINT('Ctrl Pts',(44.563535818056,39.8627385187931,46.8482050612988));
#36313=CARTESIAN_POINT('Ctrl Pts',(44.5391463344816,39.7365127763873,49.1964830865931));
#36314=CARTESIAN_POINT('Ctrl Pts',(42.5509841043168,39.6102870339814,50.4463692724266));
#36315=CARTESIAN_POINT('Ctrl Pts',(40.4242158964095,39.4840612915755,49.4504468252328));
#36316=CARTESIAN_POINT('Ctrl Pts',(40.1112511264596,39.3578355491697,47.1229895036563));
#36317=CARTESIAN_POINT('Ctrl Pts',(41.8993967804196,39.2316098067638,45.6006427457807));
#36318=CARTESIAN_POINT('Ctrl Pts',(44.1471047109853,39.105384064358,46.2809467880016));
#36319=CARTESIAN_POINT('Ctrl Pts',(44.7909407784774,38.9791583219522,48.5393709397469));
#36320=CARTESIAN_POINT('Ctrl Pts',(43.2398525138651,38.8529325795463,50.3026433878879));
#36321=CARTESIAN_POINT('Ctrl Pts',(40.917765345953,38.7267068371405,49.9520500114421));
#36322=CARTESIAN_POINT('Ctrl Pts',(39.9563948203524,38.6004810947346,47.8094414976215));
#36323=CARTESIAN_POINT('Ctrl Pts',(41.2382954435587,38.4742553523287,45.8417689325808));
#36324=CARTESIAN_POINT('Ctrl Pts',(43.5866606235631,38.3480296099229,45.8553892238186));
#36325=CARTESIAN_POINT('Ctrl Pts',(44.8456511523612,38.2218038675171,47.8377987121399));
#36326=CARTESIAN_POINT('Ctrl Pts',(43.8594922945758,38.0955781251112,49.9691117436304));
#36327=CARTESIAN_POINT('Ctrl Pts',(41.5334946675828,37.9693523827053,50.2927466771805));
#36328=CARTESIAN_POINT('Ctrl Pts',(40.0029636849925,37.8431266402995,48.5116011350304));
#36329=CARTESIAN_POINT('Ctrl Pts',(40.6729528407962,37.7169008978936,46.2607970426901));
#36330=CARTESIAN_POINT('Ctrl Pts',(42.9284006857281,37.5906751554878,45.6066108690497));
#36331=CARTESIAN_POINT('Ctrl Pts',(44.6987677069752,37.4644494130819,47.1495966567582));
#36332=CARTESIAN_POINT('Ctrl Pts',(44.3588268446837,37.3382236706761,49.4732671887257));
#36333=CARTESIAN_POINT('Ctrl Pts',(42.2206495967492,37.2119979282702,50.4444533641866));
#36334=CARTESIAN_POINT('Ctrl Pts',(40.2471190718168,37.0857721858644,49.1715897429963));
#36335=CARTESIAN_POINT('Ctrl Pts',(40.2499698842764,36.9595464434585,46.8231867954894));
#36336=CARTESIAN_POINT('Ctrl Pts',(42.2265849397648,36.8333207010527,45.5551184008806));
#36337=CARTESIAN_POINT('Ctrl Pts',(44.3623979723383,36.7070949586468,46.5314929298803));
#36338=CARTESIAN_POINT('Ctrl Pts',(44.6966962632961,36.5808692162409,48.855981945482));
#36339=CARTESIAN_POINT('Ctrl Pts',(42.9225882912717,36.4546434738351,50.3946649650118));
#36340=CARTESIAN_POINT('Ctrl Pts',(40.6687353726094,36.3284177314293,49.7350047858075));
#36341=CARTESIAN_POINT('Ctrl Pts',(40.0042128506585,36.2021919890234,47.482580680802));
#36342=CARTESIAN_POINT('Ctrl Pts',(41.5390637117578,36.0759662466176,45.7051563180868));
#36343=CARTESIAN_POINT('Ctrl Pts',(43.8642687399131,35.9497405042117,46.0344375171106));
#36344=CARTESIAN_POINT('Ctrl Pts',(44.8452501407396,35.8235147618058,48.1681385323011));
#36345=CARTESIAN_POINT('Ctrl Pts',(43.5814502904756,35.6972890194,50.1474855128642));
#36346=CARTESIAN_POINT('Ctrl Pts',(41.2330589634704,35.5710632769941,50.1554042391373));
#36347=CARTESIAN_POINT('Ctrl Pts',(39.9559393711116,35.4448375345883,48.1846251856098));
#36348=CARTESIAN_POINT('Ctrl Pts',(40.9225090377262,35.3186117921824,46.0443570690945));
#36349=CARTESIAN_POINT('Ctrl Pts',(43.2454405568381,35.1923860497766,45.6994024511693));
#36350=CARTESIAN_POINT('Ctrl Pts',(44.7922432541268,35.0661603073707,47.4664355427714));
#36351=CARTESIAN_POINT('Ctrl Pts',(44.1429259244093,34.9399345649648,49.7232898881538));
#36352=CARTESIAN_POINT('Ctrl Pts',(41.893572928995,34.813708822559,50.3981347832605));
#36353=CARTESIAN_POINT('Ctrl Pts',(40.1091286045852,34.6874830801532,48.8714511272717));
#36354=CARTESIAN_POINT('Ctrl Pts',(40.4277432159704,34.5612573377473,46.5447605033124));
#36355=CARTESIAN_POINT('Ctrl Pts',(42.5569231245721,34.4350315953415,45.5540045071265));
#36356=CARTESIAN_POINT('Ctrl Pts',(44.5420449364172,34.3088058529356,46.8087140091359));
#36357=CARTESIAN_POINT('Ctrl Pts',(44.5607330304451,34.1825801105298,49.1570443259581));
#36358=CARTESIAN_POINT('Ctrl Pts',(42.5958314341089,34.0563543681239,50.4431882614755));
#36359=CARTESIAN_POINT('Ctrl Pts',(40.4511532269197,33.930128625718,49.486443777049));
#36360=CARTESIAN_POINT('Ctrl Pts',(40.0955495714944,33.8039028833122,47.1651186218703));
#36361=CARTESIAN_POINT('Ctrl Pts',(41.8554705517465,33.6776771409063,45.610228746747));
#36362=CARTESIAN_POINT('Ctrl Pts',(44.1152789991272,33.5514513985005,46.2491896312768));
#36363=CARTESIAN_POINT('Ctrl Pts',(44.8004318008118,33.4252256560946,48.495424093399));
#36364=CARTESIAN_POINT('Ctrl Pts',(43.2819480020455,33.2989999136888,50.2868510879112));
#36365=CARTESIAN_POINT('Ctrl Pts',(40.9538196297428,33.1727741712829,49.9789092954279));
#36366=CARTESIAN_POINT('Ctrl Pts',(39.9533120290261,33.0465484288771,47.8542962040937));
#36367=CARTESIAN_POINT('Ctrl Pts',(41.1989005120996,32.9203226864712,45.863439454171));
#36368=CARTESIAN_POINT('Ctrl Pts',(43.5471289477304,32.7940969440654,45.8339860726943));
#36369=CARTESIAN_POINT('Ctrl Pts',(44.8422532499551,32.6678712016595,47.7929615589386));
#36370=CARTESIAN_POINT('Ctrl Pts',(43.8953877208691,32.5416454592536,49.9420193250558));
#36371=CARTESIAN_POINT('Ctrl Pts',(41.5756508491709,32.4154197168479,50.3082355715256));
#36372=CARTESIAN_POINT('Ctrl Pts',(40.0128394881397,32.2891939744419,48.555521301155));
#36373=CARTESIAN_POINT('Ctrl Pts',(40.6411661025247,32.1629682320361,46.2926917979112));
#36374=CARTESIAN_POINT('Ctrl Pts',(42.884760469113,32.0367424896302,45.5974730747969));
#36375=CARTESIAN_POINT('Ctrl Pts',(44.68208631299,31.9105167472244,47.1072726840769));
#36376=CARTESIAN_POINT('Ctrl Pts',(44.3869177368363,31.7842910048185,49.4376890087395));
#36377=CARTESIAN_POINT('Ctrl Pts',(42.2625828455065,31.6580652624127,50.4461385087641));
#36378=CARTESIAN_POINT('Ctrl Pts',(40.939052320939,31.5739147674755,49.6240706423386));
#36379=CARTESIAN_POINT('Ctrl Pts',(40.5980299186877,31.5318395200069,49.0239060291786));
#36380=CARTESIAN_POINT('Ctrl Pts',(43.6056354772814,46.9728183150527,46.4985301453641));
#36381=CARTESIAN_POINT('Ctrl Pts',(44.1059354690308,46.930725945326,46.9002294498996));
#36382=CARTESIAN_POINT('Ctrl Pts',(44.6641305069622,46.8465583281308,48.2363301285741));
#36383=CARTESIAN_POINT('Ctrl Pts',(43.4241061155271,46.7203154634668,50.0355170743283));
#36384=CARTESIAN_POINT('Ctrl Pts',(41.242898981105,46.594089721061,49.9607866344046));
#36385=CARTESIAN_POINT('Ctrl Pts',(40.124548326367,46.4678639786551,48.0884731482832));
#36386=CARTESIAN_POINT('Ctrl Pts',(41.0947889846625,46.3416382362493,46.1337127750893));
#36387=CARTESIAN_POINT('Ctrl Pts',(43.2633926357093,46.2154124938433,45.8928525511316));
#36388=CARTESIAN_POINT('Ctrl Pts',(44.6393081353231,46.0891867514376,47.5860793690575));
#36389=CARTESIAN_POINT('Ctrl Pts',(43.9595403982877,45.9629610090316,49.6594484006477));
#36390=CARTESIAN_POINT('Ctrl Pts',(41.8480680352578,45.8367352666259,50.2093370666999));
#36391=CARTESIAN_POINT('Ctrl Pts',(40.2432886685352,45.71050952422,48.7310561809538));
#36392=CARTESIAN_POINT('Ctrl Pts',(40.6184019551368,45.5842837818142,46.5816334167968));
#36393=CARTESIAN_POINT('Ctrl Pts',(42.6290551175259,45.4580580394083,45.7343053093214));
#36394=CARTESIAN_POINT('Ctrl Pts',(44.4294305028971,45.3318322970025,46.9669184679027));
#36395=CARTESIAN_POINT('Ctrl Pts',(44.3667547866172,45.2056065545965,49.1479205856004));
#36396=CARTESIAN_POINT('Ctrl Pts',(42.4985643750939,45.0793808121907,50.2751107946758));
#36397=CARTESIAN_POINT('Ctrl Pts',(40.5398903524809,44.9531550697849,49.3137112080772));
#36398=CARTESIAN_POINT('Ctrl Pts',(40.2888285662205,44.826929327379,47.1463020493048));
#36399=CARTESIAN_POINT('Ctrl Pts',(41.9758581327668,44.7007035849732,45.7626023023833));
#36400=CARTESIAN_POINT('Ctrl Pts',(44.0522571322319,44.5744778425673,46.4328716443721));
#36401=CARTESIAN_POINT('Ctrl Pts',(44.6118559708041,44.4482521001614,48.5417915327042));
#36402=CARTESIAN_POINT('Ctrl Pts',(43.1409333737641,44.3220263577557,50.1533375512908));
#36403=CARTESIAN_POINT('Ctrl Pts',(40.9898213304319,44.1958006153497,49.7880830550646));
#36404=CARTESIAN_POINT('Ctrl Pts',(40.1332773078288,44.0695748729439,47.7813378731723));
#36405=CARTESIAN_POINT('Ctrl Pts',(41.3576233003874,43.9433491305381,45.9753282482937));
#36406=CARTESIAN_POINT('Ctrl Pts',(43.538888845697,43.8171233881322,46.0280017531661));
#36407=CARTESIAN_POINT('Ctrl Pts',(44.6746350451991,43.6908976457263,47.8910032157163));
#36408=CARTESIAN_POINT('Ctrl Pts',(43.7222275553626,43.5646719033205,49.8540655811966));
#36409=CARTESIAN_POINT('Ctrl Pts',(41.5559926634146,43.4384461609146,50.1150641842801));
#36410=CARTESIAN_POINT('Ctrl Pts',(40.1645708727237,43.3122204185088,48.4343978644888));
#36411=CARTESIAN_POINT('Ctrl Pts',(40.8253110712996,43.1859946761029,46.3549469110244));
#36412=CARTESIAN_POINT('Ctrl Pts',(42.9316425100263,43.0597689336971,45.7856826945333));
#36413=CARTESIAN_POINT('Ctrl Pts',(44.5499170751846,42.9335431912913,47.2491994555321));
#36414=CARTESIAN_POINT('Ctrl Pts',(44.1945311704516,42.8073174488854,49.4019638961184));
#36415=CARTESIAN_POINT('Ctrl Pts',(42.1917351055846,42.6810917064796,50.2677016165051));
#36416=CARTESIAN_POINT('Ctrl Pts',(40.3801297587773,42.5548659640736,49.0516506531956));
#36417=CARTESIAN_POINT('Ctrl Pts',(40.4227996746874,42.4286402216679,46.8701664895536));
#36418=CARTESIAN_POINT('Ctrl Pts',(42.2805731442023,42.3024144792619,45.7258887199923));
#36419=CARTESIAN_POINT('Ctrl Pts',(44.2479825001668,42.1761887368562,46.6692838143236));
#36420=CARTESIAN_POINT('Ctrl Pts',(44.5189124654952,42.0499629944503,48.8342990179267));
#36421=CARTESIAN_POINT('Ctrl Pts',(42.8446447203741,41.9237372520444,50.2334135220303));
#36422=CARTESIAN_POINT('Ctrl Pts',(40.7621855534177,41.7975115096386,49.5822163968025));
#36423=CARTESIAN_POINT('Ctrl Pts',(40.183267926526,41.6712857672327,47.4785176875716));
#36424=CARTESIAN_POINT('Ctrl Pts',(41.6393480752472,41.5450600248269,45.8535486175751));
#36425=CARTESIAN_POINT('Ctrl Pts',(43.7937196383484,41.418834282421,46.1990584525238));
#36426=CARTESIAN_POINT('Ctrl Pts',(44.66863285021,41.2926085400152,48.19786328283));
#36427=CARTESIAN_POINT('Ctrl Pts',(43.4609024899845,41.1663827976093,50.0150262515631));
#36428=CARTESIAN_POINT('Ctrl Pts',(41.2792455857734,41.0401570552035,49.9823608225385));
#36429=CARTESIAN_POINT('Ctrl Pts',(40.1264603107733,40.9139313127976,48.1298544156162));
#36430=CARTESIAN_POINT('Ctrl Pts',(41.0608231695995,40.7877055703918,46.1581394448378));
#36431=CARTESIAN_POINT('Ctrl Pts',(43.2245731535674,40.6614798279859,45.8772838149767));
#36432=CARTESIAN_POINT('Ctrl Pts',(44.6313509470666,40.5352540855801,47.5451177748369));
#36433=CARTESIAN_POINT('Ctrl Pts',(43.9897105901593,40.4090283431742,49.6305413601867));
#36434=CARTESIAN_POINT('Ctrl Pts',(41.8886888521848,40.2828026007683,50.2191002225822));
#36435=CARTESIAN_POINT('Ctrl Pts',(40.257059451201,40.1565768583625,48.7704873081738));
#36436=CARTESIAN_POINT('Ctrl Pts',(40.592685950134,40.0303511159566,46.6145539299918));
#36437=CARTESIAN_POINT('Ctrl Pts',(42.5874575100881,39.9041253735508,45.7304836264844));
#36438=CARTESIAN_POINT('Ctrl Pts',(44.4101398849683,39.777899631145,46.9298679844975));
#36439=CARTESIAN_POINT('Ctrl Pts',(44.3874796297982,39.6516738887391,49.1116517480225));
#36440=CARTESIAN_POINT('Ctrl Pts',(42.5402792445361,39.5254481463332,50.272920284853));
#36441=CARTESIAN_POINT('Ctrl Pts',(40.5643001250229,39.3992224039274,49.3476093116157));
#36442=CARTESIAN_POINT('Ctrl Pts',(40.2735247371529,39.2729966615215,47.1851700519474));
#36443=CARTESIAN_POINT('Ctrl Pts',(41.9348898364317,39.1467709191157,45.770758554241));
#36444=CARTESIAN_POINT('Ctrl Pts',(44.0232339827512,39.0205451767098,46.4028286488339));
#36445=CARTESIAN_POINT('Ctrl Pts',(44.6214217029848,38.894319434304,48.5011292300917));
#36446=CARTESIAN_POINT('Ctrl Pts',(43.18030648789,38.7680936918981,50.1393846481409));
#36447=CARTESIAN_POINT('Ctrl Pts',(41.0228566349045,38.6418679494923,49.8136485436042));
#36448=CARTESIAN_POINT('Ctrl Pts',(40.1296478321591,38.5156422070864,47.822952204972));
#36449=CARTESIAN_POINT('Ctrl Pts',(41.3206609643514,38.3894164646805,45.9947887557993));
#36450=CARTESIAN_POINT('Ctrl Pts',(43.502525703267,38.2631907222747,46.0074433605592));
#36451=CARTESIAN_POINT('Ctrl Pts',(44.6722530799132,38.1369649798688,47.8492988766815));
#36452=CARTESIAN_POINT('Ctrl Pts',(43.7560134519829,38.010739237463,49.8295005891734));
#36453=CARTESIAN_POINT('Ctrl Pts',(41.5949303937134,37.8845134950571,50.1301896199112));
#36454=CARTESIAN_POINT('Ctrl Pts',(40.1729149375288,37.7582877526513,48.4753283204915));
#36455=CARTESIAN_POINT('Ctrl Pts',(40.7954014770801,37.6320620102454,46.3841075320469));
#36456=CARTESIAN_POINT('Ctrl Pts',(42.8909367733884,37.5058362678396,45.7763035341399));
#36457=CARTESIAN_POINT('Ctrl Pts',(44.5357837552328,37.3796105254338,47.2098907426008));
#36458=CARTESIAN_POINT('Ctrl Pts',(44.2199448954737,37.2533847830279,49.3688116982201));
#36459=CARTESIAN_POINT('Ctrl Pts',(42.2333656434293,37.127159040622,50.2711402156085));
#36460=CARTESIAN_POINT('Ctrl Pts',(40.3997595670881,37.0009332982162,49.0885233567951));
#36461=CARTESIAN_POINT('Ctrl Pts',(40.4024082553057,36.8747075558104,46.9066235281145));
#36462=CARTESIAN_POINT('Ctrl Pts',(42.2388801672136,36.7484818134045,45.7284619115615));
#36463=CARTESIAN_POINT('Ctrl Pts',(44.2232628281249,36.6222560709986,46.6356109252409));
#36464=CARTESIAN_POINT('Ctrl Pts',(44.5338591781011,36.4960303285928,48.795292333534));
#36465=CARTESIAN_POINT('Ctrl Pts',(42.8855364810398,36.3698045861869,50.2248818425534));
#36466=CARTESIAN_POINT('Ctrl Pts',(40.7914830298119,36.2435788437811,49.6119919492234));
#36467=CARTESIAN_POINT('Ctrl Pts',(40.1740755366309,36.1173531013752,47.5192660079426));
#36468=CARTESIAN_POINT('Ctrl Pts',(41.6001045894553,35.9911273589694,45.8678620541969));
#36469=CARTESIAN_POINT('Ctrl Pts',(43.7604512446002,35.8649016165635,46.1737970269411));
#36470=CARTESIAN_POINT('Ctrl Pts',(44.671880500246,35.7386758741577,48.1562174137159));
#36471=CARTESIAN_POINT('Ctrl Pts',(43.4976847857903,35.6124501317518,49.9952275556402));
#36472=CARTESIAN_POINT('Ctrl Pts',(41.315795753711,35.486224389346,50.0025848396691));
#36473=CARTESIAN_POINT('Ctrl Pts',(40.1292246745312,35.3599986469401,48.1715351538286));
#36474=CARTESIAN_POINT('Ctrl Pts',(41.0272639962045,35.2337729045342,46.1830132769877));
#36475=CARTESIAN_POINT('Ctrl Pts',(43.185498335404,35.1075471621284,45.862516139751));
#36476=CARTESIAN_POINT('Ctrl Pts',(44.6226318323623,34.9813214197226,47.5042655694787));
#36477=CARTESIAN_POINT('Ctrl Pts',(44.0193514745451,34.8550956773167,49.6011076445469));
#36478=CARTESIAN_POINT('Ctrl Pts',(41.9294788994206,34.7288699349108,50.2281056486939));
#36479=CARTESIAN_POINT('Ctrl Pts',(40.2715527032993,34.602644192505,48.8096647414431));
#36480=CARTESIAN_POINT('Ctrl Pts',(40.5675773555997,34.4764184500991,46.6479378200906));
#36481=CARTESIAN_POINT('Ctrl Pts',(42.5457971848414,34.3501927076933,45.7274269935147));
#36482=CARTESIAN_POINT('Ctrl Pts',(44.3901727191906,34.2239669652874,46.8931768706323));
#36483=CARTESIAN_POINT('Ctrl Pts',(44.4075358166101,34.0977412228816,49.0750092181854));
#36484=CARTESIAN_POINT('Ctrl Pts',(42.5819468728678,33.9715154804757,50.2699648094069));
#36485=CARTESIAN_POINT('Ctrl Pts',(40.5893275833166,33.8452897380698,49.3810540588572));
#36486=CARTESIAN_POINT('Ctrl Pts',(40.2589364314598,33.719063995664,47.2243121914646));
#36487=CARTESIAN_POINT('Ctrl Pts',(41.89407800262,33.5928382532582,45.7796649022288));
#36488=CARTESIAN_POINT('Ctrl Pts',(43.993664732157,33.4666125108523,46.3733230927746));
#36489=CARTESIAN_POINT('Ctrl Pts',(44.6302398063803,33.3403867684465,48.4602982404102));
#36490=CARTESIAN_POINT('Ctrl Pts',(43.2194173817619,33.2141610260406,50.12471203131));
#36491=CARTESIAN_POINT('Ctrl Pts',(41.0563546492499,33.0879352836347,49.8386034889169));
#36492=CARTESIAN_POINT('Ctrl Pts',(40.1267836125097,32.9617095412289,47.8646266869731));
#36493=CARTESIAN_POINT('Ctrl Pts',(41.2840591561766,32.835483798823,46.0149228249524));
#36494=CARTESIAN_POINT('Ctrl Pts',(43.4657968459734,32.7092580564172,45.9875577051523));
#36495=CARTESIAN_POINT('Ctrl Pts',(44.6690960907408,32.5830323140114,47.8076407034142));
#36496=CARTESIAN_POINT('Ctrl Pts',(43.7893638719195,32.4568065716055,49.8043290386482));
#36497=CARTESIAN_POINT('Ctrl Pts',(41.6340976777956,32.3305808291997,50.1445803427444));
#36498=CARTESIAN_POINT('Ctrl Pts',(40.1820905405563,32.2043550867938,48.5161345215927));
#36499=CARTESIAN_POINT('Ctrl Pts',(40.765868436823,32.078129344388,46.4137409307898));
#36500=CARTESIAN_POINT('Ctrl Pts',(42.8503906732154,31.951903601982,45.7678136147519));
#36501=CARTESIAN_POINT('Ctrl Pts',(44.5202850816693,31.8256778595762,47.1705675639103));
#36502=CARTESIAN_POINT('Ctrl Pts',(44.2460441272262,31.6994521171704,49.3357560316449));
#36503=CARTESIAN_POINT('Ctrl Pts',(42.2723258007466,31.5732263747646,50.2727058824669));
#36504=CARTESIAN_POINT('Ctrl Pts',(41.0426343511285,31.4890758798273,49.5089231002906));
#36505=CARTESIAN_POINT('Ctrl Pts',(40.7257906332145,31.4470006323587,48.9513105031748));
#36506=CARTESIAN_POINT('Ctrl Pts',(43.4903488624466,46.9748,50.0969334274272));
#36507=CARTESIAN_POINT('Ctrl Pts',(43.5035273931069,46.9748,50.0899215423449));
#36508=CARTESIAN_POINT('Ctrl Pts',(43.5167059237672,46.9748,50.0829096572625));
#36509=CARTESIAN_POINT('Ctrl Pts',(43.5298844544276,46.9748,50.0758977721803));
#36510=CARTESIAN_POINT('Origin',(42.4,46.9748,48.));
#36511=CARTESIAN_POINT('',(42.4,47.1748,45.43653));
#36512=CARTESIAN_POINT('Origin',(42.4,47.1748,48.));
#36513=CARTESIAN_POINT('Origin',(42.4,46.9748,45.43653));
#36514=CARTESIAN_POINT('Origin',(42.4,47.1748,48.));
#36515=CARTESIAN_POINT('',(38.4376,47.1748,48.));
#36516=CARTESIAN_POINT('Origin',(42.4,47.1748,48.));
#36517=CARTESIAN_POINT('Origin',(42.4,31.4998,48.));
#36518=CARTESIAN_POINT('',(40.43653,31.2998,48.));
#36519=CARTESIAN_POINT('',(40.23653,31.4998,48.));
#36520=CARTESIAN_POINT('Origin',(42.4,31.2998,48.));
#36521=CARTESIAN_POINT('Origin',(42.4,31.2998,48.));
#36522=CARTESIAN_POINT('Origin',(46.6323742019726,52.0008,47.4568035581149));
#36523=CARTESIAN_POINT('',(46.3131875668744,47.7748,47.3774433146613));
#36524=CARTESIAN_POINT('',(46.3131875668744,51.6008,47.3774433146613));
#36525=CARTESIAN_POINT('',(46.3131875668744,47.1748,47.3774433146613));
#36526=CARTESIAN_POINT('',(46.1544810775837,47.7748,47.3379836874626));
#36527=CARTESIAN_POINT('',(46.6323742019726,47.7748,47.4568035581149));
#36528=CARTESIAN_POINT('',(46.1544810775837,51.7508,47.3379836874626));
#36529=CARTESIAN_POINT('',(46.1544810775837,52.0008,47.3379836874626));
#36530=CARTESIAN_POINT('Ctrl Pts',(46.3131875668744,51.6008,47.3774433146613));
#36531=CARTESIAN_POINT('Ctrl Pts',(46.2323033520825,51.6775199678396,47.3573328517797));
#36532=CARTESIAN_POINT('Ctrl Pts',(46.1544810775837,51.7508,47.3379836874626));
#36533=CARTESIAN_POINT('Origin',(46.1544810775837,52.0008,47.3379836874626));
#36534=CARTESIAN_POINT('',(46.2901204070909,51.6008,47.2466229507511));
#36535=CARTESIAN_POINT('',(46.2901204070909,47.7748,47.2466229507511));
#36536=CARTESIAN_POINT('',(46.2901204070909,47.1748,47.2466229507511));
#36537=CARTESIAN_POINT('Ctrl Pts',(46.1544810775837,51.7508,47.3379836874626));
#36538=CARTESIAN_POINT('Ctrl Pts',(46.2209922907101,51.6775199678396,47.2931846350574));
#36539=CARTESIAN_POINT('Ctrl Pts',(46.2901204070909,51.6008,47.2466229507511));
#36540=CARTESIAN_POINT('',(46.1544810775837,47.7748,47.3379836874626));
#36541=CARTESIAN_POINT('Origin',(46.3760628220115,47.7748,47.2989128474875));
#36542=CARTESIAN_POINT('Origin',(42.4,47.7748,48.));
#36543=CARTESIAN_POINT('Origin',(42.4,51.8008,48.));
#36544=CARTESIAN_POINT('',(38.5876,51.7508,48.));
#36545=CARTESIAN_POINT('',(38.4381567112477,51.6008,48.0664192394455));
#36546=CARTESIAN_POINT('Ctrl Pts',(38.5876,51.7508,48.));
#36547=CARTESIAN_POINT('Ctrl Pts',(38.5143199678398,51.6775199678398,48.0325689031823));
#36548=CARTESIAN_POINT('Ctrl Pts',(38.4381567112477,51.6008,48.0664192394454));
#36549=CARTESIAN_POINT('',(38.4868124331256,51.6008,48.6225566853387));
#36550=CARTESIAN_POINT('Origin',(42.4,51.6008,48.));
#36551=CARTESIAN_POINT('',(38.6455189224163,51.7508,48.6620163125374));
#36552=CARTESIAN_POINT('Ctrl Pts',(38.4868124331256,51.6008,48.6225566853387));
#36553=CARTESIAN_POINT('Ctrl Pts',(38.5676966479175,51.6775199678396,48.6426671482203));
#36554=CARTESIAN_POINT('Ctrl Pts',(38.6455189224163,51.7508,48.6620163125374));
#36555=CARTESIAN_POINT('',(38.5098795929091,51.6008,48.7533770492488));
#36556=CARTESIAN_POINT('Ctrl Pts',(38.6455189224163,51.7508,48.6620163125374));
#36557=CARTESIAN_POINT('Ctrl Pts',(38.5790077092897,51.6775199678393,48.7068153649427));
#36558=CARTESIAN_POINT('Ctrl Pts',(38.5098795929091,51.6008,48.7533770492488));
#36559=CARTESIAN_POINT('',(38.6543683790546,51.6008,49.2926165402678));
#36560=CARTESIAN_POINT('Origin',(42.4,51.6008,48.));
#36561=CARTESIAN_POINT('',(38.8175158525158,51.7508,49.3039175944148));
#36562=CARTESIAN_POINT('Ctrl Pts',(38.6543683790546,51.6008,49.2926165402678));
#36563=CARTESIAN_POINT('Ctrl Pts',(38.7375159261089,51.6775199678392,49.2983760835296));
#36564=CARTESIAN_POINT('Ctrl Pts',(38.8175158525158,51.7508,49.3039175944148));
#36565=CARTESIAN_POINT('',(38.699801814644,51.6008,49.417443878638));
#36566=CARTESIAN_POINT('Ctrl Pts',(38.8175158525158,51.7508,49.3039175944148));
#36567=CARTESIAN_POINT('Ctrl Pts',(38.7597943679781,51.6775199678396,49.3595855995048));
#36568=CARTESIAN_POINT('Ctrl Pts',(38.699801814644,51.6008,49.417443878638));
#36569=CARTESIAN_POINT('',(38.9357334464049,51.6008,49.9234008957163));
#36570=CARTESIAN_POINT('Origin',(42.4,51.6008,48.));
#36571=CARTESIAN_POINT('',(39.0983647506122,51.7508,49.9062));
#36572=CARTESIAN_POINT('Ctrl Pts',(38.9357334464049,51.6008,49.9234008957163));
#36573=CARTESIAN_POINT('Ctrl Pts',(39.0186179295798,51.6775199678394,49.9146345185509));
#36574=CARTESIAN_POINT('Ctrl Pts',(39.0983647506122,51.7508,49.9062));
#36575=CARTESIAN_POINT('',(39.0021526858504,51.6008,50.038442393036));
#36576=CARTESIAN_POINT('Ctrl Pts',(39.0983647506122,51.7508,49.9062));
#36577=CARTESIAN_POINT('Ctrl Pts',(39.051186832762,51.677519967839,49.9710455136101));
#36578=CARTESIAN_POINT('Ctrl Pts',(39.0021526858504,51.6008,50.038442393036));
#36579=CARTESIAN_POINT('',(39.3223584999828,51.6008,50.4957436882364));
#36580=CARTESIAN_POINT('Origin',(42.4,51.6008,48.));
#36581=CARTESIAN_POINT('',(39.4795321650532,51.7508,50.450563483169));
#36582=CARTESIAN_POINT('Ctrl Pts',(39.3223584999828,51.6008,50.4957436882363));
#36583=CARTESIAN_POINT('Ctrl Pts',(39.4024615161986,51.6775199678397,50.4727177525777));
#36584=CARTESIAN_POINT('Ctrl Pts',(39.4795321650532,51.7508,50.450563483169));
#36585=CARTESIAN_POINT('',(39.4077454283035,51.6008,50.5975038668231));
#36586=CARTESIAN_POINT('Ctrl Pts',(39.4795321650532,51.7508,50.450563483169));
#36587=CARTESIAN_POINT('Ctrl Pts',(39.4443312910517,51.6775199678393,50.5226162071808));
#36588=CARTESIAN_POINT('Ctrl Pts',(39.4077454283035,51.6008,50.5975038668231));
#36589=CARTESIAN_POINT('',(39.8024961331769,51.6008,50.9922545716966));
#36590=CARTESIAN_POINT('Origin',(42.4,51.6008,48.));
#36591=CARTESIAN_POINT('',(39.949436516831,51.7508,50.9204678349468));
#36592=CARTESIAN_POINT('Ctrl Pts',(39.8024961331769,51.6008,50.9922545716966));
#36593=CARTESIAN_POINT('Ctrl Pts',(39.8773837928195,51.6775199678396,50.9556687089481));
#36594=CARTESIAN_POINT('Ctrl Pts',(39.949436516831,51.7508,50.9204678349468));
#36595=CARTESIAN_POINT('',(39.9042563117637,51.6008,51.0776415000173));
#36596=CARTESIAN_POINT('Ctrl Pts',(39.949436516831,51.7508,50.9204678349468));
#36597=CARTESIAN_POINT('Ctrl Pts',(39.9272822474223,51.6775199678397,50.9975384838015));
#36598=CARTESIAN_POINT('Ctrl Pts',(39.9042563117637,51.6008,51.0776415000173));
#36599=CARTESIAN_POINT('',(40.3615576069641,51.6008,51.3978473141496));
#36600=CARTESIAN_POINT('Origin',(42.4,51.6008,48.));
#36601=CARTESIAN_POINT('',(40.4938,51.7508,51.3016352493878));
#36602=CARTESIAN_POINT('Ctrl Pts',(40.3615576069641,51.6008,51.3978473141496));
#36603=CARTESIAN_POINT('Ctrl Pts',(40.4289544863899,51.677519967839,51.348813167238));
#36604=CARTESIAN_POINT('Ctrl Pts',(40.4938,51.7508,51.3016352493878));
#36605=CARTESIAN_POINT('',(40.4765991042837,51.6008,51.4642665535951));
#36606=CARTESIAN_POINT('Ctrl Pts',(40.4938,51.7508,51.3016352493878));
#36607=CARTESIAN_POINT('Ctrl Pts',(40.4853654814492,51.6775199678399,51.3813820704198));
#36608=CARTESIAN_POINT('Ctrl Pts',(40.4765991042837,51.6008,51.4642665535951));
#36609=CARTESIAN_POINT('',(40.982556121362,51.6008,51.700198185356));
#36610=CARTESIAN_POINT('Origin',(42.4,51.6008,48.));
#36611=CARTESIAN_POINT('',(41.0960824055852,51.7508,51.5824841474842));
#36612=CARTESIAN_POINT('Ctrl Pts',(40.982556121362,51.6008,51.700198185356));
#36613=CARTESIAN_POINT('Ctrl Pts',(41.040414400495,51.6775199678393,51.6402056320221));
#36614=CARTESIAN_POINT('Ctrl Pts',(41.0960824055852,51.7508,51.5824841474842));
#36615=CARTESIAN_POINT('',(41.1073834597322,51.6008,51.7456316209454));
#36616=CARTESIAN_POINT('Ctrl Pts',(41.0960824055852,51.7508,51.5824841474842));
#36617=CARTESIAN_POINT('Ctrl Pts',(41.1016239164704,51.6775199678393,51.662484073891));
#36618=CARTESIAN_POINT('Ctrl Pts',(41.1073834597322,51.6008,51.7456316209454));
#36619=CARTESIAN_POINT('',(41.6466229507512,51.6008,51.8901204070909));
#36620=CARTESIAN_POINT('Origin',(42.4,51.6008,48.));
#36621=CARTESIAN_POINT('',(41.7379836874626,51.7508,51.7544810775837));
#36622=CARTESIAN_POINT('Ctrl Pts',(41.6466229507512,51.6008,51.8901204070909));
#36623=CARTESIAN_POINT('Ctrl Pts',(41.6931846350573,51.6775199678395,51.8209922907102));
#36624=CARTESIAN_POINT('Ctrl Pts',(41.7379836874626,51.7508,51.7544810775837));
#36625=CARTESIAN_POINT('',(41.7774433146613,51.6008,51.9131875668744));
#36626=CARTESIAN_POINT('Ctrl Pts',(41.7379836874626,51.7508,51.7544810775837));
#36627=CARTESIAN_POINT('Ctrl Pts',(41.7573328517799,51.6775199678389,51.8323033520833));
#36628=CARTESIAN_POINT('Ctrl Pts',(41.7774433146613,51.6008,51.9131875668744));
#36629=CARTESIAN_POINT('',(42.3335807605545,51.6008,51.9618432887523));
#36630=CARTESIAN_POINT('Origin',(42.4,51.6008,48.));
#36631=CARTESIAN_POINT('',(42.4,51.7508,51.8124));
#36632=CARTESIAN_POINT('Ctrl Pts',(42.3335807605545,51.6008,51.9618432887523));
#36633=CARTESIAN_POINT('Ctrl Pts',(42.3674310968175,51.6775199678395,51.8856800321605));
#36634=CARTESIAN_POINT('Ctrl Pts',(42.4,51.7508,51.8124));
#36635=CARTESIAN_POINT('',(42.4664192394455,51.6008,51.9618432887523));
#36636=CARTESIAN_POINT('Ctrl Pts',(42.4,51.7508,51.8124));
#36637=CARTESIAN_POINT('Ctrl Pts',(42.4325689031826,51.6775199678391,51.8856800321609));
#36638=CARTESIAN_POINT('Ctrl Pts',(42.4664192394455,51.6008,51.9618432887523));
#36639=CARTESIAN_POINT('',(43.0225566853387,51.6008,51.9131875668744));
#36640=CARTESIAN_POINT('Origin',(42.4,51.6008,48.));
#36641=CARTESIAN_POINT('',(43.0620163125374,51.7508,51.7544810775837));
#36642=CARTESIAN_POINT('Ctrl Pts',(43.0225566853387,51.6008,51.9131875668744));
#36643=CARTESIAN_POINT('Ctrl Pts',(43.0426671482202,51.6775199678391,51.832303352083));
#36644=CARTESIAN_POINT('Ctrl Pts',(43.0620163125374,51.7508,51.7544810775837));
#36645=CARTESIAN_POINT('',(43.1533770492489,51.6008,51.8901204070909));
#36646=CARTESIAN_POINT('Ctrl Pts',(43.0620163125374,51.7508,51.7544810775837));
#36647=CARTESIAN_POINT('Ctrl Pts',(43.1068153649428,51.6775199678392,51.8209922907104));
#36648=CARTESIAN_POINT('Ctrl Pts',(43.1533770492489,51.6008,51.8901204070909));
#36649=CARTESIAN_POINT('',(43.6926165402678,51.6008,51.7456316209454));
#36650=CARTESIAN_POINT('Origin',(42.4,51.6008,48.));
#36651=CARTESIAN_POINT('',(43.7039175944148,51.7508,51.5824841474842));
#36652=CARTESIAN_POINT('Ctrl Pts',(43.6926165402678,51.6008,51.7456316209454));
#36653=CARTESIAN_POINT('Ctrl Pts',(43.6983760835296,51.6775199678391,51.6624840738913));
#36654=CARTESIAN_POINT('Ctrl Pts',(43.7039175944148,51.7508,51.5824841474842));
#36655=CARTESIAN_POINT('',(43.817443878638,51.6008,51.700198185356));
#36656=CARTESIAN_POINT('Ctrl Pts',(43.7039175944148,51.7508,51.5824841474842));
#36657=CARTESIAN_POINT('Ctrl Pts',(43.759585599505,51.6775199678393,51.6402056320221));
#36658=CARTESIAN_POINT('Ctrl Pts',(43.817443878638,51.6008,51.700198185356));
#36659=CARTESIAN_POINT('',(44.3234008957163,51.6008,51.4642665535951));
#36660=CARTESIAN_POINT('Origin',(42.4,51.6008,48.));
#36661=CARTESIAN_POINT('',(44.3062,51.7508,51.3016352493878));
#36662=CARTESIAN_POINT('Ctrl Pts',(44.3234008957163,51.6008,51.4642665535951));
#36663=CARTESIAN_POINT('Ctrl Pts',(44.3146345185509,51.6775199678393,51.3813820704204));
#36664=CARTESIAN_POINT('Ctrl Pts',(44.3062,51.7508,51.3016352493878));
#36665=CARTESIAN_POINT('',(44.438442393036,51.6008,51.3978473141496));
#36666=CARTESIAN_POINT('Ctrl Pts',(44.3062,51.7508,51.3016352493878));
#36667=CARTESIAN_POINT('Ctrl Pts',(44.3710455136094,51.6775199678397,51.3488131672376));
#36668=CARTESIAN_POINT('Ctrl Pts',(44.438442393036,51.6008,51.3978473141496));
#36669=CARTESIAN_POINT('',(44.8957436882364,51.6008,51.0776415000172));
#36670=CARTESIAN_POINT('Origin',(42.4,51.6008,48.));
#36671=CARTESIAN_POINT('',(44.850563483169,51.7508,50.9204678349468));
#36672=CARTESIAN_POINT('Ctrl Pts',(44.8957436882364,51.6008,51.0776415000173));
#36673=CARTESIAN_POINT('Ctrl Pts',(44.8727177525779,51.6775199678391,50.9975384838021));
#36674=CARTESIAN_POINT('Ctrl Pts',(44.850563483169,51.7508,50.9204678349468));
#36675=CARTESIAN_POINT('',(44.9975038668231,51.6008,50.9922545716965));
#36676=CARTESIAN_POINT('Ctrl Pts',(44.850563483169,51.7508,50.9204678349468));
#36677=CARTESIAN_POINT('Ctrl Pts',(44.9226162071806,51.6775199678395,50.9556687089482));
#36678=CARTESIAN_POINT('Ctrl Pts',(44.9975038668231,51.6008,50.9922545716965));
#36679=CARTESIAN_POINT('',(45.3922545716966,51.6008,50.5975038668231));
#36680=CARTESIAN_POINT('Origin',(42.4,51.6008,48.));
#36681=CARTESIAN_POINT('',(45.3204678349468,51.7508,50.4505634831689));
#36682=CARTESIAN_POINT('Ctrl Pts',(45.3922545716966,51.6008,50.5975038668231));
#36683=CARTESIAN_POINT('Ctrl Pts',(45.3556687089481,51.6775199678396,50.5226162071804));
#36684=CARTESIAN_POINT('Ctrl Pts',(45.3204678349468,51.7508,50.4505634831689));
#36685=CARTESIAN_POINT('',(45.4776415000172,51.6008,50.4957436882363));
#36686=CARTESIAN_POINT('Ctrl Pts',(45.3204678349468,51.7508,50.4505634831689));
#36687=CARTESIAN_POINT('Ctrl Pts',(45.3975384838014,51.6775199678397,50.4727177525777));
#36688=CARTESIAN_POINT('Ctrl Pts',(45.4776415000172,51.6008,50.4957436882363));
#36689=CARTESIAN_POINT('',(45.7978473141496,51.6008,50.038442393036));
#36690=CARTESIAN_POINT('Origin',(42.4,51.6008,48.));
#36691=CARTESIAN_POINT('',(45.7016352493878,51.7508,49.9062));
#36692=CARTESIAN_POINT('Ctrl Pts',(45.7978473141496,51.6008,50.038442393036));
#36693=CARTESIAN_POINT('Ctrl Pts',(45.7488131672377,51.6775199678395,49.9710455136096));
#36694=CARTESIAN_POINT('Ctrl Pts',(45.7016352493878,51.7508,49.9062));
#36695=CARTESIAN_POINT('',(45.8642665535951,51.6008,49.9234008957163));
#36696=CARTESIAN_POINT('Ctrl Pts',(45.7016352493878,51.7508,49.9062));
#36697=CARTESIAN_POINT('Ctrl Pts',(45.7813820704199,51.6775199678397,49.9146345185508));
#36698=CARTESIAN_POINT('Ctrl Pts',(45.8642665535951,51.6008,49.9234008957163));
#36699=CARTESIAN_POINT('',(46.100198185356,51.6008,49.417443878638));
#36700=CARTESIAN_POINT('Origin',(42.4,51.6008,48.));
#36701=CARTESIAN_POINT('',(45.9824841474842,51.7508,49.3039175944148));
#36702=CARTESIAN_POINT('Ctrl Pts',(46.100198185356,51.6008,49.417443878638));
#36703=CARTESIAN_POINT('Ctrl Pts',(46.0402056320216,51.67751996784,49.3595855995045));
#36704=CARTESIAN_POINT('Ctrl Pts',(45.9824841474842,51.7508,49.3039175944148));
#36705=CARTESIAN_POINT('',(46.1456316209454,51.6008,49.2926165402678));
#36706=CARTESIAN_POINT('Ctrl Pts',(45.9824841474842,51.7508,49.3039175944148));
#36707=CARTESIAN_POINT('Ctrl Pts',(46.0624840738902,51.67751996784,49.2983760835296));
#36708=CARTESIAN_POINT('Ctrl Pts',(46.1456316209454,51.6008,49.2926165402678));
#36709=CARTESIAN_POINT('',(46.2901204070909,51.6008,48.7533770492488));
#36710=CARTESIAN_POINT('Origin',(42.4,51.6008,48.));
#36711=CARTESIAN_POINT('',(46.1544810775837,51.7508,48.6620163125374));
#36712=CARTESIAN_POINT('Ctrl Pts',(46.2901204070909,51.6008,48.7533770492488));
#36713=CARTESIAN_POINT('Ctrl Pts',(46.2209922907101,51.6775199678395,48.7068153649426));
#36714=CARTESIAN_POINT('Ctrl Pts',(46.1544810775837,51.7508,48.6620163125374));
#36715=CARTESIAN_POINT('',(46.3131875668744,51.6008,48.6225566853387));
#36716=CARTESIAN_POINT('Ctrl Pts',(46.1544810775837,51.7508,48.6620163125374));
#36717=CARTESIAN_POINT('Ctrl Pts',(46.2323033520828,51.6775199678393,48.6426671482202));
#36718=CARTESIAN_POINT('Ctrl Pts',(46.3131875668744,51.6008,48.6225566853387));
#36719=CARTESIAN_POINT('',(46.3618432887523,51.6008,48.0664192394455));
#36720=CARTESIAN_POINT('Origin',(42.4,51.6008,48.));
#36721=CARTESIAN_POINT('',(46.2124,51.7508,48.));
#36722=CARTESIAN_POINT('Ctrl Pts',(46.3618432887523,51.6008,48.0664192394455));
#36723=CARTESIAN_POINT('Ctrl Pts',(46.28568003216,51.67751996784,48.0325689031822));
#36724=CARTESIAN_POINT('Ctrl Pts',(46.2124,51.7508,48.));
#36725=CARTESIAN_POINT('',(46.3618432887523,51.6008,47.9335807605545));
#36726=CARTESIAN_POINT('Ctrl Pts',(46.2124,51.7508,48.));
#36727=CARTESIAN_POINT('Ctrl Pts',(46.2856800321602,51.6775199678398,47.9674310968177));
#36728=CARTESIAN_POINT('Ctrl Pts',(46.3618432887523,51.6008,47.9335807605545));
#36729=CARTESIAN_POINT('Origin',(42.4,51.6008,48.));
#36730=CARTESIAN_POINT('',(46.1456316209454,51.6008,46.7073834597322));
#36731=CARTESIAN_POINT('Origin',(42.4,51.6008,48.));
#36732=CARTESIAN_POINT('',(45.9824841474842,51.7508,46.6960824055852));
#36733=CARTESIAN_POINT('Ctrl Pts',(46.1456316209454,51.6008,46.7073834597322));
#36734=CARTESIAN_POINT('Ctrl Pts',(46.0624840738912,51.6775199678392,46.7016239164704));
#36735=CARTESIAN_POINT('Ctrl Pts',(45.9824841474842,51.7508,46.6960824055852));
#36736=CARTESIAN_POINT('',(46.100198185356,51.6008,46.582556121362));
#36737=CARTESIAN_POINT('Ctrl Pts',(45.9824841474842,51.7508,46.6960824055852));
#36738=CARTESIAN_POINT('Ctrl Pts',(46.040205632022,51.6775199678395,46.6404144004951));
#36739=CARTESIAN_POINT('Ctrl Pts',(46.100198185356,51.6008,46.582556121362));
#36740=CARTESIAN_POINT('',(45.8642665535951,51.6008,46.0765991042837));
#36741=CARTESIAN_POINT('Origin',(42.4,51.6008,48.));
#36742=CARTESIAN_POINT('',(45.7016352493878,51.7508,46.0938));
#36743=CARTESIAN_POINT('Ctrl Pts',(45.8642665535951,51.6008,46.0765991042837));
#36744=CARTESIAN_POINT('Ctrl Pts',(45.7813820704199,51.6775199678398,46.0853654814492));
#36745=CARTESIAN_POINT('Ctrl Pts',(45.7016352493878,51.7508,46.0938));
#36746=CARTESIAN_POINT('',(45.7978473141496,51.6008,45.961557606964));
#36747=CARTESIAN_POINT('Ctrl Pts',(45.7016352493878,51.7508,46.0938));
#36748=CARTESIAN_POINT('Ctrl Pts',(45.7488131672375,51.6775199678399,46.0289544863907));
#36749=CARTESIAN_POINT('Ctrl Pts',(45.7978473141496,51.6008,45.961557606964));
#36750=CARTESIAN_POINT('',(45.4776415000172,51.6008,45.5042563117636));
#36751=CARTESIAN_POINT('Origin',(42.4,51.6008,48.));
#36752=CARTESIAN_POINT('',(45.3204678349468,51.7508,45.549436516831));
#36753=CARTESIAN_POINT('Ctrl Pts',(45.4776415000173,51.6008,45.5042563117637));
#36754=CARTESIAN_POINT('Ctrl Pts',(45.3975384838014,51.6775199678398,45.5272822474223));
#36755=CARTESIAN_POINT('Ctrl Pts',(45.3204678349468,51.7508,45.549436516831));
#36756=CARTESIAN_POINT('',(45.3922545716966,51.6008,45.4024961331769));
#36757=CARTESIAN_POINT('Ctrl Pts',(45.3204678349468,51.7508,45.549436516831));
#36758=CARTESIAN_POINT('Ctrl Pts',(45.3556687089482,51.6775199678395,45.4773837928194));
#36759=CARTESIAN_POINT('Ctrl Pts',(45.3922545716966,51.6008,45.4024961331769));
#36760=CARTESIAN_POINT('',(44.9975038668231,51.6008,45.0077454283035));
#36761=CARTESIAN_POINT('Origin',(42.4,51.6008,48.));
#36762=CARTESIAN_POINT('',(44.850563483169,51.7508,45.0795321650532));
#36763=CARTESIAN_POINT('Ctrl Pts',(44.9975038668231,51.6008,45.0077454283034));
#36764=CARTESIAN_POINT('Ctrl Pts',(44.9226162071805,51.6775199678396,45.0443312910519));
#36765=CARTESIAN_POINT('Ctrl Pts',(44.850563483169,51.7508,45.0795321650532));
#36766=CARTESIAN_POINT('',(44.8957436882364,51.6008,44.9223584999827));
#36767=CARTESIAN_POINT('Ctrl Pts',(44.850563483169,51.7508,45.0795321650532));
#36768=CARTESIAN_POINT('Ctrl Pts',(44.8727177525775,51.6775199678404,45.0024615161993));
#36769=CARTESIAN_POINT('Ctrl Pts',(44.8957436882364,51.6008,44.9223584999828));
#36770=CARTESIAN_POINT('',(44.4384423930359,51.6008,44.6021526858504));
#36771=CARTESIAN_POINT('Origin',(42.4,51.6008,48.));
#36772=CARTESIAN_POINT('',(44.3062,51.7508,44.6983647506122));
#36773=CARTESIAN_POINT('Ctrl Pts',(44.4384423930359,51.6008,44.6021526858504));
#36774=CARTESIAN_POINT('Ctrl Pts',(44.37104551361,51.6775199678391,44.651186832762));
#36775=CARTESIAN_POINT('Ctrl Pts',(44.3062,51.7508,44.6983647506122));
#36776=CARTESIAN_POINT('',(44.3234008957163,51.6008,44.5357334464049));
#36777=CARTESIAN_POINT('Ctrl Pts',(44.3062,51.7508,44.6983647506122));
#36778=CARTESIAN_POINT('Ctrl Pts',(44.3146345185509,51.6775199678395,44.6186179295799));
#36779=CARTESIAN_POINT('Ctrl Pts',(44.3234008957163,51.6008,44.5357334464049));
#36780=CARTESIAN_POINT('',(43.817443878638,51.6008,44.299801814644));
#36781=CARTESIAN_POINT('Origin',(42.4,51.6008,48.));
#36782=CARTESIAN_POINT('',(43.7039175944148,51.7508,44.4175158525158));
#36783=CARTESIAN_POINT('Ctrl Pts',(43.817443878638,51.6008,44.299801814644));
#36784=CARTESIAN_POINT('Ctrl Pts',(43.7595855995047,51.6775199678397,44.3597943679782));
#36785=CARTESIAN_POINT('Ctrl Pts',(43.7039175944148,51.7508,44.4175158525158));
#36786=CARTESIAN_POINT('',(43.6926165402678,51.6008,44.2543683790546));
#36787=CARTESIAN_POINT('Ctrl Pts',(43.7039175944148,51.7508,44.4175158525158));
#36788=CARTESIAN_POINT('Ctrl Pts',(43.6983760835296,51.6775199678396,44.3375159261093));
#36789=CARTESIAN_POINT('Ctrl Pts',(43.6926165402678,51.6008,44.2543683790546));
#36790=CARTESIAN_POINT('',(43.1533770492489,51.6008,44.1098795929091));
#36791=CARTESIAN_POINT('Origin',(42.4,51.6008,48.));
#36792=CARTESIAN_POINT('',(43.0620163125374,51.7508,44.2455189224163));
#36793=CARTESIAN_POINT('Ctrl Pts',(43.1533770492489,51.6008,44.1098795929091));
#36794=CARTESIAN_POINT('Ctrl Pts',(43.1068153649429,51.6775199678391,44.1790077092895));
#36795=CARTESIAN_POINT('Ctrl Pts',(43.0620163125374,51.7508,44.2455189224163));
#36796=CARTESIAN_POINT('',(43.0225566853387,51.6008,44.0868124331256));
#36797=CARTESIAN_POINT('Ctrl Pts',(43.0620163125374,51.7508,44.2455189224163));
#36798=CARTESIAN_POINT('Ctrl Pts',(43.0426671482202,51.6775199678393,44.1676966479172));
#36799=CARTESIAN_POINT('Ctrl Pts',(43.0225566853387,51.6008,44.0868124331256));
#36800=CARTESIAN_POINT('',(42.4664192394455,51.6008,44.0381567112477));
#36801=CARTESIAN_POINT('Origin',(42.4,51.6008,48.));
#36802=CARTESIAN_POINT('',(42.4,51.7508,44.1876));
#36803=CARTESIAN_POINT('Ctrl Pts',(42.4664192394455,51.6008,44.0381567112477));
#36804=CARTESIAN_POINT('Ctrl Pts',(42.4325689031828,51.6775199678388,44.1143199678388));
#36805=CARTESIAN_POINT('Ctrl Pts',(42.4,51.7508,44.1876));
#36806=CARTESIAN_POINT('',(42.3335807605545,51.6008,44.0381567112477));
#36807=CARTESIAN_POINT('Ctrl Pts',(42.4,51.7508,44.1876));
#36808=CARTESIAN_POINT('Ctrl Pts',(42.3674310968175,51.6775199678393,44.1143199678393));
#36809=CARTESIAN_POINT('Ctrl Pts',(42.3335807605545,51.6008,44.0381567112477));
#36810=CARTESIAN_POINT('',(41.7774433146613,51.6008,44.0868124331256));
#36811=CARTESIAN_POINT('Origin',(42.4,51.6008,48.));
#36812=CARTESIAN_POINT('',(41.7379836874626,51.7508,44.2455189224162));
#36813=CARTESIAN_POINT('Ctrl Pts',(41.7774433146613,51.6008,44.0868124331256));
#36814=CARTESIAN_POINT('Ctrl Pts',(41.7573328517799,51.6775199678389,44.1676966479167));
#36815=CARTESIAN_POINT('Ctrl Pts',(41.7379836874626,51.7508,44.2455189224162));
#36816=CARTESIAN_POINT('',(41.6466229507512,51.6008,44.1098795929091));
#36817=CARTESIAN_POINT('Ctrl Pts',(41.7379836874626,51.7508,44.2455189224162));
#36818=CARTESIAN_POINT('Ctrl Pts',(41.693184635057,51.6775199678389,44.1790077092893));
#36819=CARTESIAN_POINT('Ctrl Pts',(41.6466229507511,51.6008,44.1098795929091));
#36820=CARTESIAN_POINT('',(41.1073834597322,51.6008,44.2543683790546));
#36821=CARTESIAN_POINT('Origin',(42.4,51.6008,48.));
#36822=CARTESIAN_POINT('',(41.0960824055852,51.7508,44.4175158525158));
#36823=CARTESIAN_POINT('Ctrl Pts',(41.1073834597322,51.6008,44.2543683790546));
#36824=CARTESIAN_POINT('Ctrl Pts',(41.1016239164704,51.6775199678393,44.337515926109));
#36825=CARTESIAN_POINT('Ctrl Pts',(41.0960824055852,51.7508,44.4175158525158));
#36826=CARTESIAN_POINT('',(40.982556121362,51.6008,44.299801814644));
#36827=CARTESIAN_POINT('Ctrl Pts',(41.0960824055852,51.7508,44.4175158525158));
#36828=CARTESIAN_POINT('Ctrl Pts',(41.0404144004952,51.6775199678396,44.3597943679781));
#36829=CARTESIAN_POINT('Ctrl Pts',(40.982556121362,51.6008,44.299801814644));
#36830=CARTESIAN_POINT('',(40.4765991042837,51.6008,44.5357334464049));
#36831=CARTESIAN_POINT('Origin',(42.4,51.6008,48.));
#36832=CARTESIAN_POINT('',(40.4938,51.7508,44.6983647506122));
#36833=CARTESIAN_POINT('Ctrl Pts',(40.4765991042837,51.6008,44.5357334464049));
#36834=CARTESIAN_POINT('Ctrl Pts',(40.4853654814491,51.6775199678393,44.6186179295796));
#36835=CARTESIAN_POINT('Ctrl Pts',(40.4938,51.7508,44.6983647506122));
#36836=CARTESIAN_POINT('',(40.3615576069641,51.6008,44.6021526858504));
#36837=CARTESIAN_POINT('Ctrl Pts',(40.4938,51.7508,44.6983647506122));
#36838=CARTESIAN_POINT('Ctrl Pts',(40.4289544863898,51.6775199678389,44.6511868327619));
#36839=CARTESIAN_POINT('Ctrl Pts',(40.3615576069641,51.6008,44.6021526858504));
#36840=CARTESIAN_POINT('',(39.9042563117637,51.6008,44.9223584999827));
#36841=CARTESIAN_POINT('Origin',(42.4,51.6008,48.));
#36842=CARTESIAN_POINT('',(39.949436516831,51.7508,45.0795321650532));
#36843=CARTESIAN_POINT('Ctrl Pts',(39.9042563117637,51.6008,44.9223584999827));
#36844=CARTESIAN_POINT('Ctrl Pts',(39.9272822474223,51.6775199678396,45.0024615161984));
#36845=CARTESIAN_POINT('Ctrl Pts',(39.949436516831,51.7508,45.0795321650532));
#36846=CARTESIAN_POINT('',(39.8024961331769,51.6008,45.0077454283035));
#36847=CARTESIAN_POINT('Ctrl Pts',(39.949436516831,51.7508,45.0795321650532));
#36848=CARTESIAN_POINT('Ctrl Pts',(39.8773837928197,51.6775199678398,45.0443312910519));
#36849=CARTESIAN_POINT('Ctrl Pts',(39.8024961331769,51.6008,45.0077454283035));
#36850=CARTESIAN_POINT('',(39.4077454283035,51.6008,45.4024961331769));
#36851=CARTESIAN_POINT('Origin',(42.4,51.6008,48.));
#36852=CARTESIAN_POINT('',(39.4795321650532,51.7508,45.549436516831));
#36853=CARTESIAN_POINT('Ctrl Pts',(39.4077454283035,51.6008,45.4024961331769));
#36854=CARTESIAN_POINT('Ctrl Pts',(39.4443312910519,51.6775199678397,45.4773837928196));
#36855=CARTESIAN_POINT('Ctrl Pts',(39.4795321650532,51.7508,45.549436516831));
#36856=CARTESIAN_POINT('',(39.3223584999828,51.6008,45.5042563117637));
#36857=CARTESIAN_POINT('Ctrl Pts',(39.4795321650532,51.7508,45.549436516831));
#36858=CARTESIAN_POINT('Ctrl Pts',(39.4024615161982,51.6775199678394,45.5272822474222));
#36859=CARTESIAN_POINT('Ctrl Pts',(39.3223584999828,51.6008,45.5042563117637));
#36860=CARTESIAN_POINT('',(39.0021526858504,51.6008,45.961557606964));
#36861=CARTESIAN_POINT('Origin',(42.4,51.6008,48.));
#36862=CARTESIAN_POINT('',(39.0983647506122,51.7508,46.0938));
#36863=CARTESIAN_POINT('Ctrl Pts',(39.0021526858504,51.6008,45.961557606964));
#36864=CARTESIAN_POINT('Ctrl Pts',(39.0511868327623,51.6775199678396,46.0289544863904));
#36865=CARTESIAN_POINT('Ctrl Pts',(39.0983647506122,51.7508,46.0938));
#36866=CARTESIAN_POINT('',(38.9357334464049,51.6008,46.0765991042837));
#36867=CARTESIAN_POINT('Ctrl Pts',(39.0983647506122,51.7508,46.0938));
#36868=CARTESIAN_POINT('Ctrl Pts',(39.0186179295797,51.6775199678394,46.0853654814491));
#36869=CARTESIAN_POINT('Ctrl Pts',(38.9357334464049,51.6008,46.0765991042837));
#36870=CARTESIAN_POINT('',(38.699801814644,51.6008,46.582556121362));
#36871=CARTESIAN_POINT('Origin',(42.4,51.6008,48.));
#36872=CARTESIAN_POINT('',(38.8175158525158,51.7508,46.6960824055852));
#36873=CARTESIAN_POINT('Ctrl Pts',(38.699801814644,51.6008,46.582556121362));
#36874=CARTESIAN_POINT('Ctrl Pts',(38.7597943679782,51.6775199678396,46.6404144004952));
#36875=CARTESIAN_POINT('Ctrl Pts',(38.8175158525158,51.7508,46.6960824055852));
#36876=CARTESIAN_POINT('',(38.6543683790546,51.6008,46.7073834597322));
#36877=CARTESIAN_POINT('Ctrl Pts',(38.8175158525158,51.7508,46.6960824055852));
#36878=CARTESIAN_POINT('Ctrl Pts',(38.7375159261091,51.6775199678394,46.7016239164704));
#36879=CARTESIAN_POINT('Ctrl Pts',(38.6543683790546,51.6008,46.7073834597322));
#36880=CARTESIAN_POINT('',(38.5098795929091,51.6008,47.2466229507512));
#36881=CARTESIAN_POINT('Origin',(42.4,51.6008,48.));
#36882=CARTESIAN_POINT('',(38.6455189224163,51.7508,47.3379836874626));
#36883=CARTESIAN_POINT('Ctrl Pts',(38.5098795929091,51.6008,47.2466229507512));
#36884=CARTESIAN_POINT('Ctrl Pts',(38.5790077092902,51.6775199678398,47.2931846350576));
#36885=CARTESIAN_POINT('Ctrl Pts',(38.6455189224163,51.7508,47.3379836874626));
#36886=CARTESIAN_POINT('',(38.4868124331256,51.6008,47.3774433146613));
#36887=CARTESIAN_POINT('Ctrl Pts',(38.6455189224163,51.7508,47.3379836874626));
#36888=CARTESIAN_POINT('Ctrl Pts',(38.5676966479172,51.6775199678394,47.3573328517798));
#36889=CARTESIAN_POINT('Ctrl Pts',(38.4868124331256,51.6008,47.3774433146613));
#36890=CARTESIAN_POINT('',(38.4381567112477,51.6008,47.9335807605545));
#36891=CARTESIAN_POINT('Origin',(42.4,51.6008,48.));
#36892=CARTESIAN_POINT('Ctrl Pts',(38.4381567112477,51.6008,47.9335807605545));
#36893=CARTESIAN_POINT('Ctrl Pts',(38.5143199678391,51.6775199678391,47.9674310968174));
#36894=CARTESIAN_POINT('Ctrl Pts',(38.5876,51.7508,48.));
#36895=CARTESIAN_POINT('',(38.8376,52.0008,48.));
#36896=CARTESIAN_POINT('',(38.6376,51.8008,48.));
#36897=CARTESIAN_POINT('Origin',(42.4,52.0008,48.));
#36898=CARTESIAN_POINT('Origin',(46.473749855503,52.0008,46.7301118652459));
#36899=CARTESIAN_POINT('',(46.1456316209454,47.7748,46.7073834597322));
#36900=CARTESIAN_POINT('',(46.1456316209454,47.1748,46.7073834597322));
#36901=CARTESIAN_POINT('',(45.9824841474842,47.7748,46.6960824055852));
#36902=CARTESIAN_POINT('',(46.473749855503,47.7748,46.7301118652459));
#36903=CARTESIAN_POINT('',(45.9824841474842,52.0008,46.6960824055852));
#36904=CARTESIAN_POINT('Origin',(45.9824841474842,52.0008,46.6960824055852));
#36905=CARTESIAN_POINT('',(46.100198185356,47.7748,46.582556121362));
#36906=CARTESIAN_POINT('',(46.100198185356,47.1748,46.582556121362));
#36907=CARTESIAN_POINT('',(45.9824841474842,47.7748,46.6960824055852));
#36908=CARTESIAN_POINT('Origin',(46.193914987161,47.7748,46.6191278733369));
#36909=CARTESIAN_POINT('Origin',(42.4,47.7748,48.));
#36910=CARTESIAN_POINT('Origin',(46.1913466810908,52.0008,46.0420050807569));
#36911=CARTESIAN_POINT('',(45.8642665535951,47.7748,46.0765991042837));
#36912=CARTESIAN_POINT('',(45.8642665535951,47.1748,46.0765991042837));
#36913=CARTESIAN_POINT('',(45.7016352493878,47.7748,46.0938));
#36914=CARTESIAN_POINT('',(46.1913466810908,47.7748,46.0420050807569));
#36915=CARTESIAN_POINT('',(45.7016352493878,52.0008,46.0938));
#36916=CARTESIAN_POINT('Origin',(45.7016352493878,52.0008,46.0938));
#36917=CARTESIAN_POINT('',(45.7978473141496,47.7748,45.961557606964));
#36918=CARTESIAN_POINT('',(45.7978473141496,47.1748,45.961557606964));
#36919=CARTESIAN_POINT('',(45.7016352493878,47.7748,46.0938));
#36920=CARTESIAN_POINT('Origin',(45.8964909652393,47.7748,45.9813));
#36921=CARTESIAN_POINT('Origin',(42.4,47.7748,48.));
#36922=CARTESIAN_POINT('Origin',(45.7937453562877,52.0008,45.4133909810959));
#36923=CARTESIAN_POINT('',(45.4776415000172,47.7748,45.5042563117636));
#36924=CARTESIAN_POINT('',(45.4776415000172,47.1748,45.5042563117636));
#36925=CARTESIAN_POINT('',(45.3204678349468,47.7748,45.549436516831));
#36926=CARTESIAN_POINT('',(45.7937453562877,47.7748,45.4133909810959));
#36927=CARTESIAN_POINT('',(45.3204678349468,52.0008,45.549436516831));
#36928=CARTESIAN_POINT('Origin',(45.3204678349468,52.0008,45.549436516831));
#36929=CARTESIAN_POINT('',(45.3922545716966,47.7748,45.4024961331769));
#36930=CARTESIAN_POINT('',(45.3922545716966,47.1748,45.4024961331769));
#36931=CARTESIAN_POINT('',(45.3204678349468,47.7748,45.549436516831));
#36932=CARTESIAN_POINT('Origin',(45.4928278346486,47.7748,45.4048093046516));
#36933=CARTESIAN_POINT('Origin',(42.4,47.7748,48.));
#36934=CARTESIAN_POINT('Origin',(45.2930267961517,52.0008,44.863369687587));
#36935=CARTESIAN_POINT('',(44.9975038668231,47.7748,45.0077454283035));
#36936=CARTESIAN_POINT('',(44.9975038668231,47.1748,45.0077454283035));
#36937=CARTESIAN_POINT('',(44.850563483169,47.7748,45.0795321650532));
#36938=CARTESIAN_POINT('',(45.2930267961517,47.7748,44.863369687587));
#36939=CARTESIAN_POINT('',(44.850563483169,52.0008,45.0795321650532));
#36940=CARTESIAN_POINT('Origin',(44.850563483169,52.0008,45.0795321650532));
#36941=CARTESIAN_POINT('',(44.8957436882364,47.7748,44.9223584999827));
#36942=CARTESIAN_POINT('',(44.8957436882364,47.1748,44.9223584999827));
#36943=CARTESIAN_POINT('',(44.850563483169,47.7748,45.0795321650532));
#36944=CARTESIAN_POINT('Origin',(44.9951906953484,47.7748,44.9071721653514));
#36945=CARTESIAN_POINT('Origin',(42.4,47.7748,48.));
#36946=CARTESIAN_POINT('Origin',(44.7044050807569,52.0008,44.4086533189092));
#36947=CARTESIAN_POINT('',(44.4384423930359,47.7748,44.6021526858504));
#36948=CARTESIAN_POINT('',(44.4384423930359,47.1748,44.6021526858504));
#36949=CARTESIAN_POINT('',(44.3062,47.7748,44.6983647506122));
#36950=CARTESIAN_POINT('',(44.7044050807569,47.7748,44.4086533189092));
#36951=CARTESIAN_POINT('',(44.3062,52.0008,44.6983647506122));
#36952=CARTESIAN_POINT('Origin',(44.3062,52.0008,44.6983647506122));
#36953=CARTESIAN_POINT('',(44.3234008957163,47.7748,44.5357334464049));
#36954=CARTESIAN_POINT('',(44.3234008957163,47.1748,44.5357334464049));
#36955=CARTESIAN_POINT('',(44.3062,47.7748,44.6983647506122));
#36956=CARTESIAN_POINT('Origin',(44.4187,47.7748,44.5035090347607));
#36957=CARTESIAN_POINT('Origin',(42.4,47.7748,48.));
#36958=CARTESIAN_POINT('Origin',(44.0457651830685,52.0008,44.0630582018273));
#36959=CARTESIAN_POINT('',(43.817443878638,47.7748,44.299801814644));
#36960=CARTESIAN_POINT('',(43.817443878638,47.1748,44.299801814644));
#36961=CARTESIAN_POINT('',(43.7039175944148,47.7748,44.4175158525158));
#36962=CARTESIAN_POINT('',(44.0457651830685,47.7748,44.0630582018273));
#36963=CARTESIAN_POINT('',(43.7039175944148,52.0008,44.4175158525158));
#36964=CARTESIAN_POINT('Origin',(43.7039175944148,52.0008,44.4175158525158));
#36965=CARTESIAN_POINT('',(43.6926165402678,47.7748,44.2543683790546));
#36966=CARTESIAN_POINT('',(43.6926165402678,47.1748,44.2543683790546));
#36967=CARTESIAN_POINT('',(43.7039175944148,47.7748,44.4175158525158));
#36968=CARTESIAN_POINT('Origin',(43.7808721266631,47.7748,44.206085012839));
#36969=CARTESIAN_POINT('Origin',(42.4,47.7748,48.));
#36970=CARTESIAN_POINT('Origin',(43.33711954309,52.0008,43.8370850690942));
#36971=CARTESIAN_POINT('',(43.1533770492489,47.7748,44.1098795929091));
#36972=CARTESIAN_POINT('',(43.1533770492489,47.1748,44.1098795929091));
#36973=CARTESIAN_POINT('',(43.0620163125374,47.7748,44.2455189224163));
#36974=CARTESIAN_POINT('',(43.33711954309,47.7748,43.8370850690942));
#36975=CARTESIAN_POINT('',(43.0620163125374,52.0008,44.2455189224163));
#36976=CARTESIAN_POINT('Origin',(43.0620163125374,52.0008,44.2455189224163));
#36977=CARTESIAN_POINT('',(43.0225566853387,47.7748,44.0868124331256));
#36978=CARTESIAN_POINT('',(43.0225566853387,47.1748,44.0868124331256));
#36979=CARTESIAN_POINT('',(43.0620163125374,47.7748,44.2455189224163));
#36980=CARTESIAN_POINT('Origin',(43.1010871525125,47.7748,44.0239371779885));
#36981=CARTESIAN_POINT('Origin',(42.4,47.7748,48.));
#36982=CARTESIAN_POINT('Origin',(42.6,52.0008,43.7376));
#36983=CARTESIAN_POINT('',(42.4664192394455,47.7748,44.0381567112477));
#36984=CARTESIAN_POINT('',(42.4664192394455,47.1748,44.0381567112477));
#36985=CARTESIAN_POINT('',(42.4,47.7748,44.1876));
#36986=CARTESIAN_POINT('',(42.6,47.7748,43.7376));
#36987=CARTESIAN_POINT('',(42.4,52.0008,44.1876));
#36988=CARTESIAN_POINT('Origin',(42.4,52.0008,44.1876));
#36989=CARTESIAN_POINT('',(42.3335807605545,47.7748,44.0381567112477));
#36990=CARTESIAN_POINT('',(42.3335807605545,47.1748,44.0381567112477));
#36991=CARTESIAN_POINT('',(42.4,47.7748,44.1876));
#36992=CARTESIAN_POINT('Origin',(42.4,47.7748,43.9626));
#36993=CARTESIAN_POINT('Origin',(42.4,47.7748,48.));
#36994=CARTESIAN_POINT('Origin',(41.8568035581149,52.0008,43.7676257980274));
#36995=CARTESIAN_POINT('',(41.7774433146613,47.7748,44.0868124331256));
#36996=CARTESIAN_POINT('',(41.7774433146613,47.1748,44.0868124331256));
#36997=CARTESIAN_POINT('',(41.7379836874626,47.7748,44.2455189224162));
#36998=CARTESIAN_POINT('',(41.8568035581149,47.7748,43.7676257980274));
#36999=CARTESIAN_POINT('',(41.7379836874626,52.0008,44.2455189224162));
#37000=CARTESIAN_POINT('Origin',(41.7379836874626,52.0008,44.2455189224162));
#37001=CARTESIAN_POINT('',(41.6466229507512,47.7748,44.1098795929091));
#37002=CARTESIAN_POINT('',(41.6466229507512,47.1748,44.1098795929091));
#37003=CARTESIAN_POINT('',(41.7379836874626,47.7748,44.2455189224162));
#37004=CARTESIAN_POINT('Origin',(41.6989128474875,47.7748,44.0239371779885));
#37005=CARTESIAN_POINT('Origin',(42.4,47.7748,48.));
#37006=CARTESIAN_POINT('Origin',(41.1301118652459,52.0008,43.926250144497));
#37007=CARTESIAN_POINT('',(41.1073834597322,47.7748,44.2543683790546));
#37008=CARTESIAN_POINT('',(41.1073834597322,47.1748,44.2543683790546));
#37009=CARTESIAN_POINT('',(41.0960824055852,47.7748,44.4175158525158));
#37010=CARTESIAN_POINT('',(41.1301118652459,47.7748,43.926250144497));
#37011=CARTESIAN_POINT('',(41.0960824055852,52.0008,44.4175158525158));
#37012=CARTESIAN_POINT('Origin',(41.0960824055852,52.0008,44.4175158525158));
#37013=CARTESIAN_POINT('',(40.982556121362,47.7748,44.299801814644));
#37014=CARTESIAN_POINT('',(40.982556121362,47.1748,44.299801814644));
#37015=CARTESIAN_POINT('',(41.0960824055852,47.7748,44.4175158525158));
#37016=CARTESIAN_POINT('Origin',(41.0191278733369,47.7748,44.206085012839));
#37017=CARTESIAN_POINT('Origin',(42.4,47.7748,48.));
#37018=CARTESIAN_POINT('Origin',(40.4420050807569,52.0008,44.2086533189092));
#37019=CARTESIAN_POINT('',(40.4765991042837,47.7748,44.5357334464049));
#37020=CARTESIAN_POINT('',(40.4765991042837,47.1748,44.5357334464049));
#37021=CARTESIAN_POINT('',(40.4938,47.7748,44.6983647506122));
#37022=CARTESIAN_POINT('',(40.4420050807569,47.7748,44.2086533189092));
#37023=CARTESIAN_POINT('',(40.4938,52.0008,44.6983647506122));
#37024=CARTESIAN_POINT('Origin',(40.4938,52.0008,44.6983647506122));
#37025=CARTESIAN_POINT('',(40.3615576069641,47.7748,44.6021526858504));
#37026=CARTESIAN_POINT('',(40.3615576069641,47.1748,44.6021526858504));
#37027=CARTESIAN_POINT('',(40.4938,47.7748,44.6983647506122));
#37028=CARTESIAN_POINT('Origin',(40.3813,47.7748,44.5035090347607));
#37029=CARTESIAN_POINT('Origin',(42.4,47.7748,48.));
#37030=CARTESIAN_POINT('Origin',(39.8133909810959,52.0008,44.6062546437123));
#37031=CARTESIAN_POINT('',(39.9042563117637,47.7748,44.9223584999827));
#37032=CARTESIAN_POINT('',(39.9042563117637,47.1748,44.9223584999827));
#37033=CARTESIAN_POINT('',(39.949436516831,47.7748,45.0795321650532));
#37034=CARTESIAN_POINT('',(39.8133909810959,47.7748,44.6062546437123));
#37035=CARTESIAN_POINT('',(39.949436516831,52.0008,45.0795321650532));
#37036=CARTESIAN_POINT('Origin',(39.949436516831,52.0008,45.0795321650532));
#37037=CARTESIAN_POINT('',(39.8024961331769,47.7748,45.0077454283035));
#37038=CARTESIAN_POINT('',(39.8024961331769,47.1748,45.0077454283035));
#37039=CARTESIAN_POINT('',(39.949436516831,47.7748,45.0795321650532));
#37040=CARTESIAN_POINT('Origin',(39.8048093046516,47.7748,44.9071721653514));
#37041=CARTESIAN_POINT('Origin',(42.4,47.7748,48.));
#37042=CARTESIAN_POINT('Origin',(39.263369687587,52.0008,45.1069732038483));
#37043=CARTESIAN_POINT('',(39.4077454283035,47.7748,45.4024961331769));
#37044=CARTESIAN_POINT('',(39.4077454283035,47.1748,45.4024961331769));
#37045=CARTESIAN_POINT('',(39.4795321650532,47.7748,45.549436516831));
#37046=CARTESIAN_POINT('',(39.263369687587,47.7748,45.1069732038483));
#37047=CARTESIAN_POINT('',(39.4795321650532,52.0008,45.549436516831));
#37048=CARTESIAN_POINT('Origin',(39.4795321650532,52.0008,45.549436516831));
#37049=CARTESIAN_POINT('',(39.3223584999828,47.7748,45.5042563117637));
#37050=CARTESIAN_POINT('',(39.3223584999828,47.1748,45.5042563117637));
#37051=CARTESIAN_POINT('',(39.4795321650532,47.7748,45.549436516831));
#37052=CARTESIAN_POINT('Origin',(39.3071721653514,47.7748,45.4048093046516));
#37053=CARTESIAN_POINT('Origin',(42.4,47.7748,48.));
#37054=CARTESIAN_POINT('Origin',(38.8086533189092,52.0008,45.6955949192431));
#37055=CARTESIAN_POINT('',(39.0021526858504,47.7748,45.961557606964));
#37056=CARTESIAN_POINT('',(39.0021526858504,47.1748,45.961557606964));
#37057=CARTESIAN_POINT('',(39.0983647506122,47.7748,46.0938));
#37058=CARTESIAN_POINT('',(38.8086533189092,47.7748,45.6955949192431));
#37059=CARTESIAN_POINT('',(39.0983647506122,52.0008,46.0938));
#37060=CARTESIAN_POINT('Origin',(39.0983647506122,52.0008,46.0938));
#37061=CARTESIAN_POINT('',(38.9357334464049,47.7748,46.0765991042837));
#37062=CARTESIAN_POINT('',(38.9357334464049,47.1748,46.0765991042837));
#37063=CARTESIAN_POINT('',(39.0983647506122,47.7748,46.0938));
#37064=CARTESIAN_POINT('Origin',(38.9035090347607,47.7748,45.9813));
#37065=CARTESIAN_POINT('Origin',(42.4,47.7748,48.));
#37066=CARTESIAN_POINT('Origin',(38.4630582018273,52.0008,46.3542348169315));
#37067=CARTESIAN_POINT('',(38.699801814644,47.7748,46.582556121362));
#37068=CARTESIAN_POINT('',(38.699801814644,47.1748,46.582556121362));
#37069=CARTESIAN_POINT('',(38.8175158525158,47.7748,46.6960824055852));
#37070=CARTESIAN_POINT('',(38.4630582018273,47.7748,46.3542348169315));
#37071=CARTESIAN_POINT('',(38.8175158525158,52.0008,46.6960824055852));
#37072=CARTESIAN_POINT('Origin',(38.8175158525158,52.0008,46.6960824055852));
#37073=CARTESIAN_POINT('',(38.6543683790546,47.7748,46.7073834597322));
#37074=CARTESIAN_POINT('',(38.6543683790546,47.1748,46.7073834597322));
#37075=CARTESIAN_POINT('',(38.8175158525158,47.7748,46.6960824055852));
#37076=CARTESIAN_POINT('Origin',(38.606085012839,47.7748,46.619127873337));
#37077=CARTESIAN_POINT('Origin',(42.4,47.7748,48.));
#37078=CARTESIAN_POINT('Origin',(38.2370850690942,52.0008,47.06288045691));
#37079=CARTESIAN_POINT('',(38.5098795929091,47.7748,47.2466229507512));
#37080=CARTESIAN_POINT('',(38.5098795929091,47.1748,47.2466229507512));
#37081=CARTESIAN_POINT('',(38.6455189224163,47.7748,47.3379836874626));
#37082=CARTESIAN_POINT('',(38.2370850690942,47.7748,47.06288045691));
#37083=CARTESIAN_POINT('',(38.6455189224163,52.0008,47.3379836874626));
#37084=CARTESIAN_POINT('Origin',(38.6455189224163,52.0008,47.3379836874626));
#37085=CARTESIAN_POINT('',(38.4868124331256,47.7748,47.3774433146613));
#37086=CARTESIAN_POINT('',(38.4868124331256,47.1748,47.3774433146613));
#37087=CARTESIAN_POINT('',(38.6455189224163,47.7748,47.3379836874626));
#37088=CARTESIAN_POINT('Origin',(38.4239371779885,47.7748,47.2989128474875));
#37089=CARTESIAN_POINT('Origin',(42.4,47.7748,48.));
#37090=CARTESIAN_POINT('Origin',(38.1376,52.0008,47.8));
#37091=CARTESIAN_POINT('',(38.4381567112477,47.7748,47.9335807605545));
#37092=CARTESIAN_POINT('',(38.4381567112477,47.1748,47.9335807605545));
#37093=CARTESIAN_POINT('',(38.5876,47.7748,48.));
#37094=CARTESIAN_POINT('',(38.1376,47.7748,47.8));
#37095=CARTESIAN_POINT('',(38.5876,52.0008,48.));
#37096=CARTESIAN_POINT('Origin',(38.5876,52.0008,48.));
#37097=CARTESIAN_POINT('',(38.4381567112477,47.7748,48.0664192394455));
#37098=CARTESIAN_POINT('',(38.4381567112477,47.1748,48.0664192394455));
#37099=CARTESIAN_POINT('',(38.5876,47.7748,48.));
#37100=CARTESIAN_POINT('Origin',(38.3626,47.7748,48.));
#37101=CARTESIAN_POINT('',(38.4376,47.7748,48.));
#37102=CARTESIAN_POINT('Origin',(42.4,47.7748,48.));
#37103=CARTESIAN_POINT('Origin',(42.4,47.7748,48.));
#37104=CARTESIAN_POINT('Origin',(38.1676257980274,52.0008,48.5431964418851));
#37105=CARTESIAN_POINT('',(38.4868124331256,47.7748,48.6225566853387));
#37106=CARTESIAN_POINT('',(38.4868124331256,47.1748,48.6225566853387));
#37107=CARTESIAN_POINT('',(38.6455189224163,47.7748,48.6620163125374));
#37108=CARTESIAN_POINT('',(38.1676257980274,47.7748,48.5431964418851));
#37109=CARTESIAN_POINT('',(38.6455189224163,52.0008,48.6620163125374));
#37110=CARTESIAN_POINT('Origin',(38.6455189224163,52.0008,48.6620163125374));
#37111=CARTESIAN_POINT('',(38.5098795929091,47.7748,48.7533770492488));
#37112=CARTESIAN_POINT('',(38.5098795929091,47.1748,48.7533770492488));
#37113=CARTESIAN_POINT('',(38.6455189224163,47.7748,48.6620163125374));
#37114=CARTESIAN_POINT('Origin',(38.4239371779885,47.7748,48.7010871525125));
#37115=CARTESIAN_POINT('Origin',(42.4,47.7748,48.));
#37116=CARTESIAN_POINT('Origin',(38.326250144497,52.0008,49.2698881347541));
#37117=CARTESIAN_POINT('',(38.6543683790546,47.7748,49.2926165402678));
#37118=CARTESIAN_POINT('',(38.6543683790546,47.1748,49.2926165402678));
#37119=CARTESIAN_POINT('',(38.8175158525158,47.7748,49.3039175944148));
#37120=CARTESIAN_POINT('',(38.326250144497,47.7748,49.2698881347541));
#37121=CARTESIAN_POINT('',(38.8175158525158,52.0008,49.3039175944148));
#37122=CARTESIAN_POINT('Origin',(38.8175158525158,52.0008,49.3039175944148));
#37123=CARTESIAN_POINT('',(38.699801814644,47.7748,49.417443878638));
#37124=CARTESIAN_POINT('',(38.699801814644,47.1748,49.417443878638));
#37125=CARTESIAN_POINT('',(38.8175158525158,47.7748,49.3039175944148));
#37126=CARTESIAN_POINT('Origin',(38.606085012839,47.7748,49.380872126663));
#37127=CARTESIAN_POINT('Origin',(42.4,47.7748,48.));
#37128=CARTESIAN_POINT('Origin',(38.6086533189092,52.0008,49.9579949192431));
#37129=CARTESIAN_POINT('',(38.9357334464049,47.7748,49.9234008957163));
#37130=CARTESIAN_POINT('',(38.9357334464049,47.1748,49.9234008957163));
#37131=CARTESIAN_POINT('',(39.0983647506122,47.7748,49.9062));
#37132=CARTESIAN_POINT('',(38.6086533189092,47.7748,49.9579949192431));
#37133=CARTESIAN_POINT('',(39.0983647506122,52.0008,49.9062));
#37134=CARTESIAN_POINT('Origin',(39.0983647506122,52.0008,49.9062));
#37135=CARTESIAN_POINT('',(39.0021526858504,47.7748,50.038442393036));
#37136=CARTESIAN_POINT('',(39.0021526858504,47.1748,50.038442393036));
#37137=CARTESIAN_POINT('',(39.0983647506122,47.7748,49.9062));
#37138=CARTESIAN_POINT('Origin',(38.9035090347607,47.7748,50.0187));
#37139=CARTESIAN_POINT('Origin',(42.4,47.7748,48.));
#37140=CARTESIAN_POINT('Origin',(39.0062546437124,52.0008,50.5866090189041));
#37141=CARTESIAN_POINT('',(39.3223584999828,47.7748,50.4957436882364));
#37142=CARTESIAN_POINT('',(39.3223584999828,47.1748,50.4957436882364));
#37143=CARTESIAN_POINT('',(39.4795321650532,47.7748,50.450563483169));
#37144=CARTESIAN_POINT('',(39.0062546437124,47.7748,50.5866090189041));
#37145=CARTESIAN_POINT('',(39.4795321650532,52.0008,50.450563483169));
#37146=CARTESIAN_POINT('Origin',(39.4795321650532,52.0008,50.450563483169));
#37147=CARTESIAN_POINT('',(39.4077454283035,47.7748,50.5975038668231));
#37148=CARTESIAN_POINT('',(39.4077454283035,47.1748,50.5975038668231));
#37149=CARTESIAN_POINT('',(39.4795321650532,47.7748,50.450563483169));
#37150=CARTESIAN_POINT('Origin',(39.3071721653514,47.7748,50.5951906953484));
#37151=CARTESIAN_POINT('Origin',(42.4,47.7748,48.));
#37152=CARTESIAN_POINT('Origin',(39.5069732038483,52.0008,51.136630312413));
#37153=CARTESIAN_POINT('',(39.8024961331769,47.7748,50.9922545716966));
#37154=CARTESIAN_POINT('',(39.8024961331769,47.1748,50.9922545716966));
#37155=CARTESIAN_POINT('',(39.949436516831,47.7748,50.9204678349468));
#37156=CARTESIAN_POINT('',(39.5069732038483,47.7748,51.136630312413));
#37157=CARTESIAN_POINT('',(39.949436516831,52.0008,50.9204678349468));
#37158=CARTESIAN_POINT('Origin',(39.949436516831,52.0008,50.9204678349468));
#37159=CARTESIAN_POINT('',(39.9042563117637,47.7748,51.0776415000173));
#37160=CARTESIAN_POINT('',(39.9042563117637,47.1748,51.0776415000173));
#37161=CARTESIAN_POINT('',(39.949436516831,47.7748,50.9204678349468));
#37162=CARTESIAN_POINT('Origin',(39.8048093046516,47.7748,51.0928278346486));
#37163=CARTESIAN_POINT('Origin',(42.4,47.7748,48.));
#37164=CARTESIAN_POINT('Origin',(40.0955949192431,52.0008,51.5913466810908));
#37165=CARTESIAN_POINT('',(40.3615576069641,47.7748,51.3978473141496));
#37166=CARTESIAN_POINT('',(40.3615576069641,47.1748,51.3978473141496));
#37167=CARTESIAN_POINT('',(40.4938,47.7748,51.3016352493878));
#37168=CARTESIAN_POINT('',(40.0955949192431,47.7748,51.5913466810908));
#37169=CARTESIAN_POINT('',(40.4938,52.0008,51.3016352493878));
#37170=CARTESIAN_POINT('Origin',(40.4938,52.0008,51.3016352493878));
#37171=CARTESIAN_POINT('',(40.4765991042837,47.7748,51.4642665535951));
#37172=CARTESIAN_POINT('',(40.4765991042837,47.1748,51.4642665535951));
#37173=CARTESIAN_POINT('',(40.4938,47.7748,51.3016352493878));
#37174=CARTESIAN_POINT('Origin',(40.3813,47.7748,51.4964909652393));
#37175=CARTESIAN_POINT('Origin',(42.4,47.7748,48.));
#37176=CARTESIAN_POINT('Origin',(40.7542348169315,52.0008,51.9369417981727));
#37177=CARTESIAN_POINT('',(40.982556121362,47.7748,51.700198185356));
#37178=CARTESIAN_POINT('',(40.982556121362,47.1748,51.700198185356));
#37179=CARTESIAN_POINT('',(41.0960824055852,47.7748,51.5824841474842));
#37180=CARTESIAN_POINT('',(40.7542348169315,47.7748,51.9369417981727));
#37181=CARTESIAN_POINT('',(41.0960824055852,52.0008,51.5824841474842));
#37182=CARTESIAN_POINT('Origin',(41.0960824055852,52.0008,51.5824841474842));
#37183=CARTESIAN_POINT('',(41.1073834597322,47.7748,51.7456316209454));
#37184=CARTESIAN_POINT('',(41.1073834597322,47.1748,51.7456316209454));
#37185=CARTESIAN_POINT('',(41.0960824055852,47.7748,51.5824841474842));
#37186=CARTESIAN_POINT('Origin',(41.0191278733369,47.7748,51.793914987161));
#37187=CARTESIAN_POINT('Origin',(42.4,47.7748,48.));
#37188=CARTESIAN_POINT('Origin',(41.46288045691,52.0008,52.1629149309059));
#37189=CARTESIAN_POINT('',(41.6466229507512,47.7748,51.8901204070909));
#37190=CARTESIAN_POINT('',(41.6466229507512,47.1748,51.8901204070909));
#37191=CARTESIAN_POINT('',(41.7379836874626,47.7748,51.7544810775837));
#37192=CARTESIAN_POINT('',(41.46288045691,47.7748,52.1629149309059));
#37193=CARTESIAN_POINT('',(41.7379836874626,52.0008,51.7544810775837));
#37194=CARTESIAN_POINT('Origin',(41.7379836874626,52.0008,51.7544810775837));
#37195=CARTESIAN_POINT('',(41.7774433146613,47.7748,51.9131875668744));
#37196=CARTESIAN_POINT('',(41.7774433146613,47.1748,51.9131875668744));
#37197=CARTESIAN_POINT('',(41.7379836874626,47.7748,51.7544810775837));
#37198=CARTESIAN_POINT('Origin',(41.6989128474875,47.7748,51.9760628220115));
#37199=CARTESIAN_POINT('Origin',(42.4,47.7748,48.));
#37200=CARTESIAN_POINT('Origin',(42.2,52.0008,52.2624));
#37201=CARTESIAN_POINT('',(42.3335807605545,47.7748,51.9618432887523));
#37202=CARTESIAN_POINT('',(42.3335807605545,47.1748,51.9618432887523));
#37203=CARTESIAN_POINT('',(42.4,47.7748,51.8124));
#37204=CARTESIAN_POINT('',(42.2,47.7748,52.2624));
#37205=CARTESIAN_POINT('',(42.4,52.0008,51.8124));
#37206=CARTESIAN_POINT('Origin',(42.4,52.0008,51.8124));
#37207=CARTESIAN_POINT('',(42.4664192394455,47.7748,51.9618432887523));
#37208=CARTESIAN_POINT('',(42.4664192394455,47.1748,51.9618432887523));
#37209=CARTESIAN_POINT('',(42.4,47.7748,51.8124));
#37210=CARTESIAN_POINT('Origin',(42.4,47.7748,52.0374));
#37211=CARTESIAN_POINT('Origin',(42.4,47.7748,48.));
#37212=CARTESIAN_POINT('Origin',(42.9431964418851,52.0008,52.2323742019726));
#37213=CARTESIAN_POINT('',(43.0225566853387,47.7748,51.9131875668744));
#37214=CARTESIAN_POINT('',(43.0225566853387,47.1748,51.9131875668744));
#37215=CARTESIAN_POINT('',(43.0620163125374,47.7748,51.7544810775837));
#37216=CARTESIAN_POINT('',(42.9431964418851,47.7748,52.2323742019726));
#37217=CARTESIAN_POINT('',(43.0620163125374,52.0008,51.7544810775837));
#37218=CARTESIAN_POINT('Origin',(43.0620163125374,52.0008,51.7544810775837));
#37219=CARTESIAN_POINT('',(43.1533770492489,47.7748,51.8901204070909));
#37220=CARTESIAN_POINT('',(43.1533770492489,47.1748,51.8901204070909));
#37221=CARTESIAN_POINT('',(43.0620163125374,47.7748,51.7544810775837));
#37222=CARTESIAN_POINT('Origin',(43.1010871525125,47.7748,51.9760628220115));
#37223=CARTESIAN_POINT('Origin',(42.4,47.7748,48.));
#37224=CARTESIAN_POINT('Origin',(43.6698881347541,52.0008,52.073749855503));
#37225=CARTESIAN_POINT('',(43.6926165402678,47.7748,51.7456316209454));
#37226=CARTESIAN_POINT('',(43.6926165402678,47.1748,51.7456316209454));
#37227=CARTESIAN_POINT('',(43.7039175944148,47.7748,51.5824841474842));
#37228=CARTESIAN_POINT('',(43.6698881347541,47.7748,52.073749855503));
#37229=CARTESIAN_POINT('',(43.7039175944148,52.0008,51.5824841474842));
#37230=CARTESIAN_POINT('Origin',(43.7039175944148,52.0008,51.5824841474842));
#37231=CARTESIAN_POINT('',(43.817443878638,47.7748,51.700198185356));
#37232=CARTESIAN_POINT('',(43.817443878638,47.1748,51.700198185356));
#37233=CARTESIAN_POINT('',(43.7039175944148,47.7748,51.5824841474842));
#37234=CARTESIAN_POINT('Origin',(43.7808721266631,47.7748,51.793914987161));
#37235=CARTESIAN_POINT('Origin',(42.4,47.7748,48.));
#37236=CARTESIAN_POINT('Origin',(44.3579949192431,52.0008,51.7913466810908));
#37237=CARTESIAN_POINT('',(44.3234008957163,47.7748,51.4642665535951));
#37238=CARTESIAN_POINT('',(44.3234008957163,47.1748,51.4642665535951));
#37239=CARTESIAN_POINT('',(44.3062,47.7748,51.3016352493878));
#37240=CARTESIAN_POINT('',(44.3579949192431,47.7748,51.7913466810908));
#37241=CARTESIAN_POINT('',(44.3062,52.0008,51.3016352493878));
#37242=CARTESIAN_POINT('Origin',(44.3062,52.0008,51.3016352493878));
#37243=CARTESIAN_POINT('',(44.438442393036,47.7748,51.3978473141496));
#37244=CARTESIAN_POINT('',(44.438442393036,47.1748,51.3978473141496));
#37245=CARTESIAN_POINT('',(44.3062,47.7748,51.3016352493878));
#37246=CARTESIAN_POINT('Origin',(44.4187,47.7748,51.4964909652393));
#37247=CARTESIAN_POINT('Origin',(42.4,47.7748,48.));
#37248=CARTESIAN_POINT('Origin',(44.9866090189041,52.0008,51.3937453562876));
#37249=CARTESIAN_POINT('',(44.8957436882364,47.7748,51.0776415000172));
#37250=CARTESIAN_POINT('',(44.8957436882364,47.1748,51.0776415000172));
#37251=CARTESIAN_POINT('',(44.850563483169,47.7748,50.9204678349468));
#37252=CARTESIAN_POINT('',(44.9866090189041,47.7748,51.3937453562876));
#37253=CARTESIAN_POINT('',(44.850563483169,52.0008,50.9204678349468));
#37254=CARTESIAN_POINT('Origin',(44.850563483169,52.0008,50.9204678349468));
#37255=CARTESIAN_POINT('',(44.9975038668231,47.7748,50.9922545716965));
#37256=CARTESIAN_POINT('',(44.9975038668231,47.1748,50.9922545716965));
#37257=CARTESIAN_POINT('',(44.850563483169,47.7748,50.9204678349468));
#37258=CARTESIAN_POINT('Origin',(44.9951906953484,47.7748,51.0928278346486));
#37259=CARTESIAN_POINT('Origin',(42.4,47.7748,48.));
#37260=CARTESIAN_POINT('Origin',(45.536630312413,52.0008,50.8930267961517));
#37261=CARTESIAN_POINT('',(45.3922545716966,47.7748,50.5975038668231));
#37262=CARTESIAN_POINT('',(45.3922545716966,47.1748,50.5975038668231));
#37263=CARTESIAN_POINT('',(45.3204678349468,47.7748,50.4505634831689));
#37264=CARTESIAN_POINT('',(45.536630312413,47.7748,50.8930267961517));
#37265=CARTESIAN_POINT('',(45.3204678349468,52.0008,50.4505634831689));
#37266=CARTESIAN_POINT('Origin',(45.3204678349468,52.0008,50.4505634831689));
#37267=CARTESIAN_POINT('',(45.4776415000172,47.7748,50.4957436882363));
#37268=CARTESIAN_POINT('',(45.4776415000172,47.1748,50.4957436882363));
#37269=CARTESIAN_POINT('',(45.3204678349468,47.7748,50.4505634831689));
#37270=CARTESIAN_POINT('Origin',(45.4928278346486,47.7748,50.5951906953484));
#37271=CARTESIAN_POINT('Origin',(42.4,47.7748,48.));
#37272=CARTESIAN_POINT('Origin',(45.9913466810908,52.0008,50.3044050807569));
#37273=CARTESIAN_POINT('',(45.7978473141496,47.7748,50.038442393036));
#37274=CARTESIAN_POINT('',(45.7978473141496,47.1748,50.038442393036));
#37275=CARTESIAN_POINT('',(45.7016352493878,47.7748,49.9062));
#37276=CARTESIAN_POINT('',(45.9913466810908,47.7748,50.3044050807569));
#37277=CARTESIAN_POINT('',(45.7016352493878,52.0008,49.9062));
#37278=CARTESIAN_POINT('Origin',(45.7016352493878,52.0008,49.9062));
#37279=CARTESIAN_POINT('',(45.8642665535951,47.7748,49.9234008957163));
#37280=CARTESIAN_POINT('',(45.8642665535951,47.1748,49.9234008957163));
#37281=CARTESIAN_POINT('',(45.7016352493878,47.7748,49.9062));
#37282=CARTESIAN_POINT('Origin',(45.8964909652393,47.7748,50.0187));
#37283=CARTESIAN_POINT('Origin',(42.4,47.7748,48.));
#37284=CARTESIAN_POINT('Origin',(46.3369417981727,52.0008,49.6457651830685));
#37285=CARTESIAN_POINT('',(46.100198185356,47.7748,49.417443878638));
#37286=CARTESIAN_POINT('',(46.100198185356,47.1748,49.417443878638));
#37287=CARTESIAN_POINT('',(45.9824841474842,47.7748,49.3039175944148));
#37288=CARTESIAN_POINT('',(46.3369417981727,47.7748,49.6457651830685));
#37289=CARTESIAN_POINT('',(45.9824841474842,52.0008,49.3039175944148));
#37290=CARTESIAN_POINT('Origin',(45.9824841474842,52.0008,49.3039175944148));
#37291=CARTESIAN_POINT('',(46.1456316209454,47.7748,49.2926165402678));
#37292=CARTESIAN_POINT('',(46.1456316209454,47.1748,49.2926165402678));
#37293=CARTESIAN_POINT('',(45.9824841474842,47.7748,49.3039175944148));
#37294=CARTESIAN_POINT('Origin',(46.193914987161,47.7748,49.3808721266631));
#37295=CARTESIAN_POINT('Origin',(42.4,47.7748,48.));
#37296=CARTESIAN_POINT('Origin',(46.5629149309058,52.0008,48.93711954309));
#37297=CARTESIAN_POINT('',(46.2901204070909,47.7748,48.7533770492488));
#37298=CARTESIAN_POINT('',(46.2901204070909,47.1748,48.7533770492488));
#37299=CARTESIAN_POINT('',(46.1544810775837,47.7748,48.6620163125374));
#37300=CARTESIAN_POINT('',(46.5629149309058,47.7748,48.93711954309));
#37301=CARTESIAN_POINT('',(46.1544810775837,52.0008,48.6620163125374));
#37302=CARTESIAN_POINT('Origin',(46.1544810775837,52.0008,48.6620163125374));
#37303=CARTESIAN_POINT('',(46.3131875668744,47.7748,48.6225566853387));
#37304=CARTESIAN_POINT('',(46.3131875668744,47.1748,48.6225566853387));
#37305=CARTESIAN_POINT('',(46.1544810775837,47.7748,48.6620163125374));
#37306=CARTESIAN_POINT('Origin',(46.3760628220115,47.7748,48.7010871525125));
#37307=CARTESIAN_POINT('Origin',(42.4,47.7748,48.));
#37308=CARTESIAN_POINT('Origin',(46.6624,52.0008,48.2));
#37309=CARTESIAN_POINT('',(46.3618432887523,47.7748,48.0664192394455));
#37310=CARTESIAN_POINT('',(46.3618432887523,47.1748,48.0664192394455));
#37311=CARTESIAN_POINT('',(46.2124,47.7748,48.));
#37312=CARTESIAN_POINT('',(46.6624,47.7748,48.2));
#37313=CARTESIAN_POINT('',(46.2124,52.0008,48.));
#37314=CARTESIAN_POINT('Origin',(46.2124,52.0008,48.));
#37315=CARTESIAN_POINT('',(46.3618432887523,47.7748,47.9335807605545));
#37316=CARTESIAN_POINT('',(46.3618432887523,47.1748,47.9335807605545));
#37317=CARTESIAN_POINT('',(46.2124,47.7748,48.));
#37318=CARTESIAN_POINT('Origin',(46.4374,47.7748,48.));
#37319=CARTESIAN_POINT('Origin',(42.4,47.7748,48.));
#37320=CARTESIAN_POINT('Origin',(42.4,47.1748,48.));
#37321=CARTESIAN_POINT('',(38.4376,47.1748,48.));
#37322=CARTESIAN_POINT('Origin',(42.4,52.0008,48.));
#37323=CARTESIAN_POINT('',(40.1086411191537,52.0008,48.));
#37324=CARTESIAN_POINT('',(41.2543205595768,52.0008,46.015625));
#37325=CARTESIAN_POINT('',(40.3950609792595,52.0008,47.50390625));
#37326=CARTESIAN_POINT('',(43.5456794404232,52.0008,46.015625));
#37327=CARTESIAN_POINT('',(41.8271602797884,52.0008,46.015625));
#37328=CARTESIAN_POINT('',(44.6913588808463,52.0008,48.));
#37329=CARTESIAN_POINT('',(43.832099300529,52.0008,46.51171875));
#37330=CARTESIAN_POINT('',(43.5456794404232,52.0008,49.984375));
#37331=CARTESIAN_POINT('',(44.4049390207405,52.0008,48.49609375));
#37332=CARTESIAN_POINT('',(41.2543205595768,52.0008,49.984375));
#37333=CARTESIAN_POINT('',(42.9728397202116,52.0008,49.984375));
#37334=CARTESIAN_POINT('',(40.967900699471,52.0008,49.48828125));
#37335=CARTESIAN_POINT('Origin',(44.6913588808463,49.6008,48.));
#37336=CARTESIAN_POINT('',(40.1086411191537,49.6008,48.));
#37337=CARTESIAN_POINT('',(41.2543205595768,49.6008,46.015625));
#37338=CARTESIAN_POINT('',(40.1086411191537,49.6008,48.));
#37339=CARTESIAN_POINT('Origin',(42.4,49.6008,48.));
#37340=CARTESIAN_POINT('Origin',(44.6913588808463,49.6008,48.));
#37341=CARTESIAN_POINT('',(43.5456794404232,49.6008,46.015625));
#37342=CARTESIAN_POINT('',(41.2543205595768,49.6008,46.015625));
#37343=CARTESIAN_POINT('Origin',(42.4,49.6008,48.));
#37344=CARTESIAN_POINT('Origin',(44.6913588808463,49.6008,48.));
#37345=CARTESIAN_POINT('',(44.6913588808463,49.6008,48.));
#37346=CARTESIAN_POINT('',(43.5456794404232,49.6008,46.015625));
#37347=CARTESIAN_POINT('Origin',(42.4,49.6008,48.));
#37348=CARTESIAN_POINT('Origin',(44.6913588808463,49.6008,48.));
#37349=CARTESIAN_POINT('',(43.5456794404232,49.6008,49.984375));
#37350=CARTESIAN_POINT('',(44.6913588808463,49.6008,48.));
#37351=CARTESIAN_POINT('Origin',(42.4,49.6008,48.));
#37352=CARTESIAN_POINT('Origin',(44.6913588808463,49.6008,48.));
#37353=CARTESIAN_POINT('',(41.2543205595768,49.6008,49.984375));
#37354=CARTESIAN_POINT('',(43.5456794404232,49.6008,49.984375));
#37355=CARTESIAN_POINT('Origin',(42.4,49.6008,48.));
#37356=CARTESIAN_POINT('Origin',(44.6913588808463,49.6008,48.));
#37357=CARTESIAN_POINT('',(41.2543205595768,49.6008,49.984375));
#37358=CARTESIAN_POINT('Origin',(42.4,49.6008,48.));
#37359=CARTESIAN_POINT('Origin',(42.4,49.6008,48.));
#37360=CARTESIAN_POINT('',(42.4,48.2240126844404,48.));
#37361=CARTESIAN_POINT('',(40.1086411191537,49.6008,48.));
#37362=CARTESIAN_POINT('Origin',(40.1086411191537,52.0008,48.));
#37363=CARTESIAN_POINT('',(40.1086411191537,52.0008,48.));
#37364=CARTESIAN_POINT('',(41.2543205595768,52.0008,46.015625));
#37365=CARTESIAN_POINT('Origin',(41.2543205595768,52.0008,49.984375));
#37366=CARTESIAN_POINT('',(41.2543205595768,52.0008,49.984375));
#37367=CARTESIAN_POINT('Origin',(43.5456794404232,52.0008,49.984375));
#37368=CARTESIAN_POINT('',(43.5456794404232,52.0008,49.984375));
#37369=CARTESIAN_POINT('Origin',(44.6913588808463,52.0008,48.));
#37370=CARTESIAN_POINT('',(44.6913588808463,52.0008,48.));
#37371=CARTESIAN_POINT('Origin',(43.5456794404232,52.0008,46.015625));
#37372=CARTESIAN_POINT('',(43.5456794404232,52.0008,46.015625));
#37373=CARTESIAN_POINT('Origin',(41.2543205595768,52.0008,46.015625));
#37374=CARTESIAN_POINT('',(0.,0.,0.));
#37375=CARTESIAN_POINT('Origin',(20.,-1.3495818343519,38.1));
#37376=CARTESIAN_POINT('',(19.3941040087494,0.647822633508007,36.2684889831927));
#37377=CARTESIAN_POINT('',(19.3941040087494,0.476638002189708,36.2684889831927));
#37378=CARTESIAN_POINT('',(19.3941040087494,-1.3495818343519,36.2684889831927));
#37379=CARTESIAN_POINT('',(18.7916762743506,0.125,39.6038272277535));
#37380=CARTESIAN_POINT('Ctrl Pts',(18.7916762743506,0.125,39.6038272277535));
#37381=CARTESIAN_POINT('Ctrl Pts',(18.7943552369861,0.125226424639445,39.6059797716448));
#37382=CARTESIAN_POINT('Ctrl Pts',(18.7970399207417,0.125452849278891,39.6081251322344));
#37383=CARTESIAN_POINT('Ctrl Pts',(18.7997303009197,0.125679273918337,39.6102632904132));
#37384=CARTESIAN_POINT('Ctrl Pts',(18.8527715398381,0.130143268819914,39.652417391807));
#37385=CARTESIAN_POINT('Ctrl Pts',(18.9081395171264,0.134607263721491,39.6918559953245));
#37386=CARTESIAN_POINT('Ctrl Pts',(18.9655252616266,0.139071258623068,39.7283134134949));
#37387=CARTESIAN_POINT('Ctrl Pts',(19.0256935947433,0.143751709048666,39.766538622563));
#37388=CARTESIAN_POINT('Ctrl Pts',(19.0880799935966,0.148432159474263,39.801485767529));
#37389=CARTESIAN_POINT('Ctrl Pts',(19.1522887348155,0.153112609899861,39.8328958906349));
#37390=CARTESIAN_POINT('Ctrl Pts',(19.2133616772821,0.15756447851049,39.8627720197242));
#37391=CARTESIAN_POINT('Ctrl Pts',(19.2760826304735,0.16201634712112,39.8894482656142));
#37392=CARTESIAN_POINT('Ctrl Pts',(19.3400830864951,0.166468215731749,39.912747148438));
#37393=CARTESIAN_POINT('Ctrl Pts',(19.4040445432911,0.170917371558144,39.9360318338882));
#37394=CARTESIAN_POINT('Ctrl Pts',(19.4692834950642,0.175366527384539,39.9559430713765));
#37395=CARTESIAN_POINT('Ctrl Pts',(19.5354114062265,0.179815683210935,39.9723514615145));
#37396=CARTESIAN_POINT('Ctrl Pts',(19.6015216446514,0.184263649996855,39.9887554664971));
#37397=CARTESIAN_POINT('Ctrl Pts',(19.6685198937496,0.188711616782775,40.0016583645436));
#37398=CARTESIAN_POINT('Ctrl Pts',(19.7360041588761,0.193159583568696,40.0109810969157));
#37399=CARTESIAN_POINT('Ctrl Pts',(19.803493474664,0.197607883249622,40.0203045270204));
#37400=CARTESIAN_POINT('Ctrl Pts',(19.8714683913022,0.202056182930547,40.0260471949188));
#37401=CARTESIAN_POINT('Ctrl Pts',(19.9395202713372,0.206504482611473,40.0281817236249));
#37402=CARTESIAN_POINT('Ctrl Pts',(20.0076437637078,0.210957463325894,40.0303184985375));
#37403=CARTESIAN_POINT('Ctrl Pts',(20.0758438888056,0.215410444040316,40.0288395426711));
#37404=CARTESIAN_POINT('Ctrl Pts',(20.1437115234743,0.219863424754736,40.0237696210619));
#37405=CARTESIAN_POINT('Ctrl Pts',(20.2116206843039,0.224319130113897,40.0186965973205));
#37406=CARTESIAN_POINT('Ctrl Pts',(20.2791964621902,0.228774835473057,40.0100282974194));
#37407=CARTESIAN_POINT('Ctrl Pts',(20.3460371446334,0.233230540832217,39.9978411027886));
#37408=CARTESIAN_POINT('Ctrl Pts',(20.4129887122295,0.237693637970639,39.9856336902473));
#37409=CARTESIAN_POINT('Ctrl Pts',(20.4792022732528,0.242156735109061,39.9698958481344));
#37410=CARTESIAN_POINT('Ctrl Pts',(20.5442894922072,0.246619832247484,39.9507543071874));
#37411=CARTESIAN_POINT('Ctrl Pts',(20.5675366133854,0.248213911110794,39.9439175467746));
#37412=CARTESIAN_POINT('Ctrl Pts',(20.5906402239489,0.249807989974104,39.936647029397));
#37413=CARTESIAN_POINT('Ctrl Pts',(20.6135832762986,0.251402068837415,39.9289500047696));
#37414=CARTESIAN_POINT('Ctrl Pts',(20.6778578532506,0.255867854078437,39.9073869191707));
#37415=CARTESIAN_POINT('Ctrl Pts',(20.7411164687301,0.26033363931946,39.88239059202));
#37416=CARTESIAN_POINT('Ctrl Pts',(20.8029679697888,0.264799424560482,39.8540766791658));
#37417=CARTESIAN_POINT('Ctrl Pts',(20.8677895021583,0.269479651193649,39.8244031678173));
#37418=CARTESIAN_POINT('Ctrl Pts',(20.931064837103,0.274159877826817,39.7910855085163));
#37419=CARTESIAN_POINT('Ctrl Pts',(20.9923620316329,0.278840104459984,39.7543156153145));
#37420=CARTESIAN_POINT('Ctrl Pts',(21.0506972463998,0.283294174958602,39.7193225029326));
#37421=CARTESIAN_POINT('Ctrl Pts',(21.1072405867157,0.287748245457221,39.6812033504462));
#37422=CARTESIAN_POINT('Ctrl Pts',(21.1616427426004,0.29220231595584,39.6401716448058));
#37423=CARTESIAN_POINT('Ctrl Pts',(21.2160135371272,0.296653818804391,39.5991635928237));
#37424=CARTESIAN_POINT('Ctrl Pts',(21.2682452047201,0.301105321652942,39.5552466140312));
#37425=CARTESIAN_POINT('Ctrl Pts',(21.3180179847816,0.305556824501493,39.5086770917043));
#37426=CARTESIAN_POINT('Ctrl Pts',(21.3677790561345,0.310007280164227,39.4621185245412));
#37427=CARTESIAN_POINT('Ctrl Pts',(21.4150820300604,0.31445773582696,39.4129089884313));
#37428=CARTESIAN_POINT('Ctrl Pts',(21.4596421494538,0.318908191489694,39.3613434712393));
#37429=CARTESIAN_POINT('Ctrl Pts',(21.5042069909409,0.323359118772995,39.3097724895824));
#37430=CARTESIAN_POINT('Ctrl Pts',(21.5460280817612,0.327810046056297,39.2558454045799));
#37431=CARTESIAN_POINT('Ctrl Pts',(21.5848604853994,0.332260973339599,39.1998908121807));
#37432=CARTESIAN_POINT('Ctrl Pts',(21.6237354026205,0.336716773482887,39.1438749608848));
#37433=CARTESIAN_POINT('Ctrl Pts',(21.6596148236905,0.341172573626175,39.0858275775493));
#37434=CARTESIAN_POINT('Ctrl Pts',(21.6922973457646,0.345628373769463,39.0261059606859));
#37435=CARTESIAN_POINT('Ctrl Pts',(21.7250006909406,0.350087012848485,38.9663462932307));
#37436=CARTESIAN_POINT('Ctrl Pts',(21.7545028711533,0.354545651927507,38.9049107121163));
#37437=CARTESIAN_POINT('Ctrl Pts',(21.7806498663585,0.35900429100653,38.8421782874333));
#37438=CARTESIAN_POINT('Ctrl Pts',(21.8068410600254,0.36347046689762,38.7793398208647));
#37439=CARTESIAN_POINT('Ctrl Pts',(21.8296655876564,0.367936642788711,38.7152005987841));
#37440=CARTESIAN_POINT('Ctrl Pts',(21.8490189771101,0.372402818679801,38.6501557772003));
#37441=CARTESIAN_POINT('Ctrl Pts',(21.8558396949991,0.373976833705365,38.6272320211717));
#37442=CARTESIAN_POINT('Ctrl Pts',(21.8622297372655,0.375550848730929,38.60419587745));
#37443=CARTESIAN_POINT('Ctrl Pts',(21.8681860530549,0.377124863756493,38.5810648896679));
#37444=CARTESIAN_POINT('Ctrl Pts',(21.8850361759466,0.381577674445521,38.5156284688136));
#37445=CARTESIAN_POINT('Ctrl Pts',(21.8984781796439,0.386030485134548,38.4491732861511));
#37446=CARTESIAN_POINT('Ctrl Pts',(21.9083943940455,0.390483295823575,38.3820875638444));
#37447=CARTESIAN_POINT('Ctrl Pts',(21.9182954981267,0.394929321322826,38.3151040667139));
#37448=CARTESIAN_POINT('Ctrl Pts',(21.9246814026906,0.399375346822077,38.2474924218077));
#37449=CARTESIAN_POINT('Ctrl Pts',(21.9274848519018,0.403821372321328,38.179653641406));
#37450=CARTESIAN_POINT('Ctrl Pts',(21.9302849582794,0.408262096378659,38.111895751983));
#37451=CARTESIAN_POINT('Ctrl Pts',(21.9295110719468,0.41270282043599,38.0439117566393));
#37452=CARTESIAN_POINT('Ctrl Pts',(21.9251476493223,0.417143544493322,37.9761085749184));
#37453=CARTESIAN_POINT('Ctrl Pts',(21.9207869958352,0.421581450355942,37.9083484227949));
#37454=CARTESIAN_POINT('Ctrl Pts',(21.9128413560973,0.426019356218561,37.8407693490899));
#37455=CARTESIAN_POINT('Ctrl Pts',(21.9013472625657,0.430457262081182,37.7737774624066));
#37456=CARTESIAN_POINT('Ctrl Pts',(21.8898564746609,0.434893891630827,37.7068048421559));
#37457=CARTESIAN_POINT('Ctrl Pts',(21.8748193422825,0.439330521180472,37.6404195609068));
#37458=CARTESIAN_POINT('Ctrl Pts',(21.8563239229228,0.443767150730117,37.5750199526796));
#37459=CARTESIAN_POINT('Ctrl Pts',(21.8378274044089,0.448204043941816,37.5096164578545));
#37460=CARTESIAN_POINT('Ctrl Pts',(21.8158723280938,0.452640937153514,37.4451992274802));
#37461=CARTESIAN_POINT('Ctrl Pts',(21.7905967731438,0.457077830365213,37.3821519987442));
#37462=CARTESIAN_POINT('Ctrl Pts',(21.7652943156175,0.461519446078893,37.3190376643447));
#37463=CARTESIAN_POINT('Ctrl Pts',(21.7366645113313,0.465961061792574,37.2572967012708));
#37464=CARTESIAN_POINT('Ctrl Pts',(21.7048934160845,0.470402677506254,37.1972924079793));
#37465=CARTESIAN_POINT('Ctrl Pts',(21.6731030694789,0.474846984569945,37.1372517557216));
#37466=CARTESIAN_POINT('Ctrl Pts',(21.6381678984885,0.479291291633636,37.0789502914494));
#37467=CARTESIAN_POINT('Ctrl Pts',(21.600318260241,0.483735598697328,37.0227237945452));
#37468=CARTESIAN_POINT('Ctrl Pts',(21.5624036754847,0.488187531784446,36.9664008181276));
#37469=CARTESIAN_POINT('Ctrl Pts',(21.5215649411301,0.492639464871564,36.9121603087784));
#37470=CARTESIAN_POINT('Ctrl Pts',(21.4780731799131,0.497091397958683,36.8603055893804));
#37471=CARTESIAN_POINT('Ctrl Pts',(21.4593285198817,0.49901015153098,36.8379565499545));
#37472=CARTESIAN_POINT('Ctrl Pts',(21.4400915149616,0.500928905103276,36.81605022023));
#37473=CARTESIAN_POINT('Ctrl Pts',(21.4203858838668,0.502847658675573,36.7946086801989));
#37474=CARTESIAN_POINT('Ctrl Pts',(21.3745873671793,0.507307098065113,36.7447756794595));
#37475=CARTESIAN_POINT('Ctrl Pts',(21.3260729876969,0.511766537454653,36.6972576874258));
#37476=CARTESIAN_POINT('Ctrl Pts',(21.2751059152635,0.516225976844192,36.6523648727114));
#37477=CARTESIAN_POINT('Ctrl Pts',(21.2216063926417,0.520906996708795,36.6052414253227));
#37478=CARTESIAN_POINT('Ctrl Pts',(21.1654043808122,0.525588016573397,36.5610112966107));
#37479=CARTESIAN_POINT('Ctrl Pts',(21.1068509412939,0.530269036438,36.5199925472781));
#37480=CARTESIAN_POINT('Ctrl Pts',(21.0512203375097,0.534716391939854,36.4810213474542));
#37481=CARTESIAN_POINT('Ctrl Pts',(20.9934678971692,0.539163747441708,36.4449489261502));
#37482=CARTESIAN_POINT('Ctrl Pts',(20.9339294161898,0.543611102943563,36.4120075822222));
#37483=CARTESIAN_POINT('Ctrl Pts',(20.87442687296,0.548055773997544,36.3790861218678));
#37484=CARTESIAN_POINT('Ctrl Pts',(20.8131408580578,0.552500445051526,36.3492922278292));
#37485=CARTESIAN_POINT('Ctrl Pts',(20.750434433992,0.556945116105508,36.3228138203387));
#37486=CARTESIAN_POINT('Ctrl Pts',(20.6877442795779,0.56138863395626,36.2963422828696));
#37487=CARTESIAN_POINT('Ctrl Pts',(20.6236349015592,0.565832151807011,36.2731847156516));
#37488=CARTESIAN_POINT('Ctrl Pts',(20.5584904774809,0.570275669657763,36.2534813991018));
#37489=CARTESIAN_POINT('Ctrl Pts',(20.4933405370955,0.574719563777237,36.2337764141122));
#37490=CARTESIAN_POINT('Ctrl Pts',(20.4271558491791,0.579163457896711,36.2175264004943));
#37491=CARTESIAN_POINT('Ctrl Pts',(20.3603351656064,0.583607352016185,36.2048216112124));
#37492=CARTESIAN_POINT('Ctrl Pts',(20.2934426758394,0.588056021590008,36.1921031692333));
#37493=CARTESIAN_POINT('Ctrl Pts',(20.2259133117688,0.592504691163832,36.1829376452654));
#37494=CARTESIAN_POINT('Ctrl Pts',(20.1581543837085,0.596953360737655,36.177363854544));
#37495=CARTESIAN_POINT('Ctrl Pts',(20.0903531986524,0.601404804667809,36.1717865877988));
#37496=CARTESIAN_POINT('Ctrl Pts',(20.0223226572537,0.605856248597963,36.1698055259595));
#37497=CARTESIAN_POINT('Ctrl Pts',(19.9544707160184,0.610307692528117,36.1714073418163));
#37498=CARTESIAN_POINT('Ctrl Pts',(19.8865043551865,0.614766642985118,36.1730118588357));
#37499=CARTESIAN_POINT('Ctrl Pts',(19.8187176862162,0.619225593442118,36.1782112711688));
#37500=CARTESIAN_POINT('Ctrl Pts',(19.751513220206,0.623684543899118,36.1869404407684));
#37501=CARTESIAN_POINT('Ctrl Pts',(19.7269667149817,0.625313180464296,36.1901287795783));
#37502=CARTESIAN_POINT('Ctrl Pts',(19.7024977718556,0.626941817029474,36.1937875260745));
#37503=CARTESIAN_POINT('Ctrl Pts',(19.6781255600714,0.628570453594653,36.197911831218));
#37504=CARTESIAN_POINT('Ctrl Pts',(19.6114040371796,0.633029019474033,36.2092025553623));
#37505=CARTESIAN_POINT('Ctrl Pts',(19.5451461333542,0.637487585353413,36.2240304178763));
#37506=CARTESIAN_POINT('Ctrl Pts',(19.4797550914421,0.641946151232793,36.2423434676939));
#37507=CARTESIAN_POINT('Ctrl Pts',(19.4510261750782,0.643904978657864,36.2503891274845));
#37508=CARTESIAN_POINT('Ctrl Pts',(19.4224645378388,0.645863806082935,36.2591068223827));
#37509=CARTESIAN_POINT('Ctrl Pts',(19.3941040087494,0.647822633508007,36.2684889831927));
#37510=CARTESIAN_POINT('',(21.2084517554459,0.125,39.6037243469665));
#37511=CARTESIAN_POINT('Origin',(20.,0.125,38.1));
#37512=CARTESIAN_POINT('Ctrl Pts',(21.2084517554458,0.125,39.6037243469665));
#37513=CARTESIAN_POINT('Ctrl Pts',(21.2627376096932,0.129560603484813,39.5600981092233));
#37514=CARTESIAN_POINT('Ctrl Pts',(21.3146994432444,0.134121206969626,39.5134957854694));
#37515=CARTESIAN_POINT('Ctrl Pts',(21.3640099546876,0.138681810454439,39.4641918488296));
#37516=CARTESIAN_POINT('Ctrl Pts',(21.4144857146843,0.143350184807133,39.4137228190044));
#37517=CARTESIAN_POINT('Ctrl Pts',(21.4621828429471,0.148018559159826,39.3604231537668));
#37518=CARTESIAN_POINT('Ctrl Pts',(21.5067884173978,0.152686933512519,39.3046290807115));
#37519=CARTESIAN_POINT('Ctrl Pts',(21.5503322354305,0.157244185511301,39.2501630863971));
#37520=CARTESIAN_POINT('Ctrl Pts',(21.5909297798399,0.161801437510084,39.1933205213499));
#37521=CARTESIAN_POINT('Ctrl Pts',(21.6283303606513,0.166358689508866,39.1344480622444));
#37522=CARTESIAN_POINT('Ctrl Pts',(21.6657316400298,0.170916026627875,39.0755745035207));
#37523=CARTESIAN_POINT('Ctrl Pts',(21.6999355900822,0.175473363746883,39.0146713641847));
#37524=CARTESIAN_POINT('Ctrl Pts',(21.7307355640131,0.180030700865892,38.9521132344708));
#37525=CARTESIAN_POINT('Ctrl Pts',(21.7615445108611,0.184589365668115,38.8895368797768));
#37526=CARTESIAN_POINT('Ctrl Pts',(21.7889473072846,0.189148030470337,38.8253049897284));
#37527=CARTESIAN_POINT('Ctrl Pts',(21.8127844940208,0.19370669527256,38.759814318682));
#37528=CARTESIAN_POINT('Ctrl Pts',(21.8376291849045,0.19845803690977,38.6915556145019));
#37529=CARTESIAN_POINT('Ctrl Pts',(21.8585999537576,0.20320937854698,38.6219298656052));
#37530=CARTESIAN_POINT('Ctrl Pts',(21.8755737871372,0.20796072018419,38.5514039498098));
#37531=CARTESIAN_POINT('Ctrl Pts',(21.8918942303274,0.212529163831136,38.4835928563204));
#37532=CARTESIAN_POINT('Ctrl Pts',(21.9045198179867,0.217097607478081,38.4149501092095));
#37533=CARTESIAN_POINT('Ctrl Pts',(21.9133938566971,0.221666051125027,38.3458993819711));
#37534=CARTESIAN_POINT('Ctrl Pts',(21.9222760848515,0.226238710779403,38.2767849309787));
#37535=CARTESIAN_POINT('Ctrl Pts',(21.9273998345808,0.230811370433779,38.2072622086335));
#37536=CARTESIAN_POINT('Ctrl Pts',(21.9287604628908,0.235384030088155,38.1377575646606));
#37537=CARTESIAN_POINT('Ctrl Pts',(21.930123546716,0.239964941985415,38.0681274862038));
#37538=CARTESIAN_POINT('Ctrl Pts',(21.9277099705963,0.244545853882674,37.9985160104603));
#37539=CARTESIAN_POINT('Ctrl Pts',(21.9215670421166,0.249126765779933,37.9293463755113));
#37540=CARTESIAN_POINT('Ctrl Pts',(21.920853625729,0.249658775492982,37.9213132767601));
#37541=CARTESIAN_POINT('Ctrl Pts',(21.9200899660964,0.25019078520603,37.9132861268745));
#37542=CARTESIAN_POINT('Ctrl Pts',(21.9192761819109,0.250722794919078,37.9052655796997));
#37543=CARTESIAN_POINT('Ctrl Pts',(21.9125225038227,0.25513799787515,37.8387022393567));
#37544=CARTESIAN_POINT('Ctrl Pts',(21.9022856862431,0.259553200831222,37.7723320598081));
#37545=CARTESIAN_POINT('Ctrl Pts',(21.8885821956735,0.263968403787293,37.7065538828697));
#37546=CARTESIAN_POINT('Ctrl Pts',(21.8749016068258,0.268376227911696,37.6408856365733));
#37547=CARTESIAN_POINT('Ctrl Pts',(21.8577659358544,0.272784052036099,37.5758079191562));
#37548=CARTESIAN_POINT('Ctrl Pts',(21.837243454715,0.277191876160502,37.5117151667712));
#37549=CARTESIAN_POINT('Ctrl Pts',(21.8167489415847,0.281593693308219,37.4477097599015));
#37550=CARTESIAN_POINT('Ctrl Pts',(21.7928769325674,0.285995510455937,37.3846871307437));
#37551=CARTESIAN_POINT('Ctrl Pts',(21.765746443274,0.290397327603654,37.3230302097473));
#37552=CARTESIAN_POINT('Ctrl Pts',(21.738635932719,0.29479590327818,37.2614186925579));
#37553=CARTESIAN_POINT('Ctrl Pts',(21.7082719002178,0.299194478952705,37.2011713501745));
#37554=CARTESIAN_POINT('Ctrl Pts',(21.674822208485,0.303593054627231,37.1426530791477));
#37555=CARTESIAN_POINT('Ctrl Pts',(21.641385043491,0.307989983057618,37.0841567229147));
#37556=CARTESIAN_POINT('Ctrl Pts',(21.6048647612107,0.312386911488005,37.0273885910638));
#37557=CARTESIAN_POINT('Ctrl Pts',(21.5654751859442,0.316783839918392,36.97268904064));
#37558=CARTESIAN_POINT('Ctrl Pts',(21.5260861074007,0.321180712901217,36.9179901800062));
#37559=CARTESIAN_POINT('Ctrl Pts',(21.4838281044081,0.325577585884041,36.8653602566341));
#37560=CARTESIAN_POINT('Ctrl Pts',(21.4389571931852,0.329974458866865,36.8151090501212));
#37561=CARTESIAN_POINT('Ctrl Pts',(21.3940403604596,0.334375831669492,36.7648064158379));
#37562=CARTESIAN_POINT('Ctrl Pts',(21.3465056195152,0.33877720447212,36.7168877333888));
#37563=CARTESIAN_POINT('Ctrl Pts',(21.296647206045,0.343178577274747,36.6716272965519));
#37564=CARTESIAN_POINT('Ctrl Pts',(21.2467605011079,0.347582447575469,36.6263411773063));
#37565=CARTESIAN_POINT('Ctrl Pts',(21.194547891955,0.35198631787619,36.5837166223241));
#37566=CARTESIAN_POINT('Ctrl Pts',(21.1403358744458,0.356390188176912,36.5439869376024));
#37567=CARTESIAN_POINT('Ctrl Pts',(21.0860284939024,0.360801805218182,36.504187365364));
#37568=CARTESIAN_POINT('Ctrl Pts',(21.0297151087096,0.365213422259452,36.467293099977));
#37569=CARTESIAN_POINT('Ctrl Pts',(20.9717494139593,0.369625039300722,36.4334929843023));
#37570=CARTESIAN_POINT('Ctrl Pts',(20.9418769245158,0.371898556146533,36.4160741712779));
#37571=CARTESIAN_POINT('Ctrl Pts',(20.9115659819915,0.374172072992344,36.3994763468264));
#37572=CARTESIAN_POINT('Ctrl Pts',(20.880867022521,0.376445589838155,36.3837203475147));
#37573=CARTESIAN_POINT('Ctrl Pts',(20.8206082552473,0.380908259741876,36.3527930095181));
#37574=CARTESIAN_POINT('Ctrl Pts',(20.7586013631052,0.385370929645597,36.3249828044127));
#37575=CARTESIAN_POINT('Ctrl Pts',(20.6952010916089,0.389833599549318,36.3004895112488));
#37576=CARTESIAN_POINT('Ctrl Pts',(20.6318875145553,0.394290167134065,36.276029710566));
#37577=CARTESIAN_POINT('Ctrl Pts',(20.5671847915107,0.398746734718812,36.2548780018324));
#37578=CARTESIAN_POINT('Ctrl Pts',(20.5014711961506,0.403203302303558,36.2371878258044));
#37579=CARTESIAN_POINT('Ctrl Pts',(20.435824970736,0.407655300990293,36.2195157858438));
#37580=CARTESIAN_POINT('Ctrl Pts',(20.369170401583,0.412107299677028,36.2052983645708));
#37581=CARTESIAN_POINT('Ctrl Pts',(20.3019029312493,0.416559298363762,36.1946398825936));
#37582=CARTESIAN_POINT('Ctrl Pts',(20.2346814083733,0.421008256085516,36.1839886809578));
#37583=CARTESIAN_POINT('Ctrl Pts',(20.1668482998834,0.42545721380727,36.1768916692167));
#37584=CARTESIAN_POINT('Ctrl Pts',(20.0988095349356,0.429906171529024,36.1734021611385));
#37585=CARTESIAN_POINT('Ctrl Pts',(20.0307737249861,0.434354936027661,36.1699128046135));
#37586=CARTESIAN_POINT('Ctrl Pts',(19.9625327664683,0.438803700526298,36.1700306803602));
#37587=CARTESIAN_POINT('Ctrl Pts',(19.8944965629556,0.443252465024935,36.1737571332587));
#37588=CARTESIAN_POINT('Ctrl Pts',(19.8264630549438,0.447701053269634,36.1774834385203));
#37589=CARTESIAN_POINT('Ctrl Pts',(19.758634776505,0.452149641514334,36.1848180015745));
#37590=CARTESIAN_POINT('Ctrl Pts',(19.6914182418001,0.456598229759033,36.1957101440678));
#37591=CARTESIAN_POINT('Ctrl Pts',(19.6241487403264,0.461050323500489,36.206610869592));
#37592=CARTESIAN_POINT('Ctrl Pts',(19.5574924290986,0.465502417241944,36.2210746823356));
#37593=CARTESIAN_POINT('Ctrl Pts',(19.4918461247712,0.4699545109834,36.2389996786701));
#37594=CARTESIAN_POINT('Ctrl Pts',(19.4589966743643,0.472182341385503,36.247969357682));
#37595=CARTESIAN_POINT('Ctrl Pts',(19.4263999182602,0.474410171787605,36.257804929465));
#37596=CARTESIAN_POINT('Ctrl Pts',(19.3941040087494,0.476638002189708,36.2684889831927));
#37597=CARTESIAN_POINT('Origin',(20.,-1.3495818343519,38.1));
#37598=CARTESIAN_POINT('',(19.3941040087494,1.44151754323334,36.2684889831927));
#37599=CARTESIAN_POINT('',(19.3941039987112,1.2718084690693,36.2684889865135));
#37600=CARTESIAN_POINT('',(19.3941040087494,-1.3495818343519,36.2684889831927));
#37601=CARTESIAN_POINT('',(18.0708702148579,0.805831834310469,38.0990895178969));
#37602=CARTESIAN_POINT('Ctrl Pts',(18.0708702148576,0.805831834351889,38.0990895185324));
#37603=CARTESIAN_POINT('Ctrl Pts',(18.0708375364269,0.810344728670084,38.1683286368148));
#37604=CARTESIAN_POINT('Ctrl Pts',(18.0745368319364,0.814857622988279,38.2375583631981));
#37605=CARTESIAN_POINT('Ctrl Pts',(18.0819387408898,0.819370517306473,38.306357852287));
#37606=CARTESIAN_POINT('Ctrl Pts',(18.0893440199819,0.823885466375696,38.3751886662445));
#37607=CARTESIAN_POINT('Ctrl Pts',(18.1004552109146,0.828400415444919,38.4435883856162));
#37608=CARTESIAN_POINT('Ctrl Pts',(18.1151913368057,0.832915364514142,38.5111433570518));
#37609=CARTESIAN_POINT('Ctrl Pts',(18.1299502559231,0.837437297118666,38.5788028197055));
#37610=CARTESIAN_POINT('Ctrl Pts',(18.1483451999935,0.841959229723191,38.6456144655361));
#37611=CARTESIAN_POINT('Ctrl Pts',(18.1702446300288,0.846481162327715,38.7111774234718));
#37612=CARTESIAN_POINT('Ctrl Pts',(18.1921629410618,0.85100699359988,38.7767969077215));
#37613=CARTESIAN_POINT('Ctrl Pts',(18.2175915807431,0.855532824872045,38.8411651228237));
#37614=CARTESIAN_POINT('Ctrl Pts',(18.2463509663266,0.86005865614421,38.903901501178));
#37615=CARTESIAN_POINT('Ctrl Pts',(18.2751686126002,0.864593655833861,38.9667649707281));
#37616=CARTESIAN_POINT('Ctrl Pts',(18.3073302582298,0.869128655523511,39.027989586192));
#37617=CARTESIAN_POINT('Ctrl Pts',(18.3426107823526,0.873663655213162,39.0872201062205));
#37618=CARTESIAN_POINT('Ctrl Pts',(18.3590838144112,0.875781117953045,39.114875768361));
#37619=CARTESIAN_POINT('Ctrl Pts',(18.3762361871948,0.877898580692929,39.1420971267213));
#37620=CARTESIAN_POINT('Ctrl Pts',(18.3940419374892,0.880016043432812,39.1688504377866));
#37621=CARTESIAN_POINT('Ctrl Pts',(18.431533734575,0.884474574079813,39.2251822234877));
#37622=CARTESIAN_POINT('Ctrl Pts',(18.4720670317525,0.888933104726814,39.2796501817338));
#37623=CARTESIAN_POINT('Ctrl Pts',(18.515430207209,0.893391635373815,39.331907093588));
#37624=CARTESIAN_POINT('Ctrl Pts',(18.5609583929547,0.898072768831235,39.3867730568011));
#37625=CARTESIAN_POINT('Ctrl Pts',(18.6096062135336,0.902753902288654,39.4392009056546));
#37626=CARTESIAN_POINT('Ctrl Pts',(18.6610762557557,0.907435035746074,39.4888217178598));
#37627=CARTESIAN_POINT('Ctrl Pts',(18.7099658284056,0.911881478849085,39.5359547723224));
#37628=CARTESIAN_POINT('Ctrl Pts',(18.7614010415462,0.916327921952096,39.5805550863722));
#37629=CARTESIAN_POINT('Ctrl Pts',(18.8150864061707,0.920774365055107,39.6223410695565));
#37630=CARTESIAN_POINT('Ctrl Pts',(18.8687393732253,0.925218124857889,39.6641018361046));
#37631=CARTESIAN_POINT('Ctrl Pts',(18.9246394097628,0.929661884660671,39.7030513386402));
#37632=CARTESIAN_POINT('Ctrl Pts',(18.9824571914328,0.934105644463453,39.7389475859933));
#37633=CARTESIAN_POINT('Ctrl Pts',(19.0402600025174,0.938548253656791,39.7748345388383));
#37634=CARTESIAN_POINT('Ctrl Pts',(19.0999791541169,0.942990862850129,39.807669546138));
#37635=CARTESIAN_POINT('Ctrl Pts',(19.1612570588225,0.947433472043467,39.837254395742));
#37636=CARTESIAN_POINT('Ctrl Pts',(19.2225402092415,0.951876461547703,39.866841777966));
#37637=CARTESIAN_POINT('Ctrl Pts',(19.2853819324421,0.956319451051938,39.893178238275));
#37638=CARTESIAN_POINT('Ctrl Pts',(19.3494024709221,0.960762440556174,39.9161127200859));
#37639=CARTESIAN_POINT('Ctrl Pts',(19.4134919925981,0.965210217455566,39.9390719141827));
#37640=CARTESIAN_POINT('Ctrl Pts',(19.4787623989205,0.969657994354959,39.9586216491901));
#37641=CARTESIAN_POINT('Ctrl Pts',(19.5448174874032,0.974105771254351,39.9746603524708));
#37642=CARTESIAN_POINT('Ctrl Pts',(19.6109138654164,0.97855632835772,39.9907090811795));
#37643=CARTESIAN_POINT('Ctrl Pts',(19.677795417065,0.983006885461089,40.0032423202488));
#37644=CARTESIAN_POINT('Ctrl Pts',(19.7450572066299,0.987457442564458,40.0122099071516));
#37645=CARTESIAN_POINT('Ctrl Pts',(19.8124327009231,0.991915523246807,40.0211926535831));
#37646=CARTESIAN_POINT('Ctrl Pts',(19.8801892247977,0.996373603929156,40.0265976818341));
#37647=CARTESIAN_POINT('Ctrl Pts',(19.9479191791693,1.0008316846115,40.0284268575711));
#37648=CARTESIAN_POINT('Ctrl Pts',(19.9727700303623,1.00246740252497,40.0290980018893));
#37649=CARTESIAN_POINT('Ctrl Pts',(19.9976173359428,1.00410312043843,40.0292882585755));
#37650=CARTESIAN_POINT('Ctrl Pts',(20.0224411443908,1.00573883835189,40.028999469139));
#37651=CARTESIAN_POINT('Ctrl Pts',(20.090102396661,1.01019724861627,40.0282123274336));
#37652=CARTESIAN_POINT('Ctrl Pts',(20.1578557735094,1.01465565888065,40.0238594090442));
#37653=CARTESIAN_POINT('Ctrl Pts',(20.2252948295895,1.01911406914503,40.0159292253787));
#37654=CARTESIAN_POINT('Ctrl Pts',(20.2961030813753,1.02379521765028,40.0076028567382));
#37655=CARTESIAN_POINT('Ctrl Pts',(20.3665642414268,1.02847636615553,39.9953323339279));
#37656=CARTESIAN_POINT('Ctrl Pts',(20.4362069181355,1.03315751466077,39.9791663261858));
#37657=CARTESIAN_POINT('Ctrl Pts',(20.5023560627118,1.03760383958525,39.9638112646935));
#37658=CARTESIAN_POINT('Ctrl Pts',(20.5677663119074,1.04205016450972,39.9449422565196));
#37659=CARTESIAN_POINT('Ctrl Pts',(20.6320406205111,1.04649648943419,39.9226538922472));
#37660=CARTESIAN_POINT('Ctrl Pts',(20.6962761567255,1.05094013218837,39.9003789730536));
#37661=CARTESIAN_POINT('Ctrl Pts',(20.759376646732,1.05538377494255,39.8746889507375));
#37662=CARTESIAN_POINT('Ctrl Pts',(20.820959846084,1.05982741769673,39.8457283545895));
#37663=CARTESIAN_POINT('Ctrl Pts',(20.8825271177261,1.06426991115932,39.8167752487307));
#37664=CARTESIAN_POINT('Ctrl Pts',(20.9425774317927,1.06871240462191,39.7845534582554));
#37665=CARTESIAN_POINT('Ctrl Pts',(21.000749884414,1.0731548980845,39.7492550517568));
#37666=CARTESIAN_POINT('Ctrl Pts',(21.0589273367702,1.0775977733651,39.7139536114739));
#37667=CARTESIAN_POINT('Ctrl Pts',(21.115226187162,1.0820406486457,39.6755752883961));
#37668=CARTESIAN_POINT('Ctrl Pts',(21.1693130217081,1.0864835239263,39.6343564169266));
#37669=CARTESIAN_POINT('Ctrl Pts',(21.2234581738335,1.09093118960986,39.5930931023902));
#37670=CARTESIAN_POINT('Ctrl Pts',(21.2753861584475,1.09537885529341,39.5489834279105));
#37671=CARTESIAN_POINT('Ctrl Pts',(21.324796121244,1.09982652097696,39.5023044583959));
#37672=CARTESIAN_POINT('Ctrl Pts',(21.3742369877044,1.10427696847126,39.4555962933283));
#37673=CARTESIAN_POINT('Ctrl Pts',(21.4211563585478,1.10872741596556,39.4063159926053));
#37674=CARTESIAN_POINT('Ctrl Pts',(21.4652917531,1.11317786345986,39.3547759302749));
#37675=CARTESIAN_POINT('Ctrl Pts',(21.5095017936349,1.11763583797482,39.3031486984823));
#37676=CARTESIAN_POINT('Ctrl Pts',(21.550918163011,1.12209381248979,39.2492544697726));
#37677=CARTESIAN_POINT('Ctrl Pts',(21.5893205765428,1.12655178700475,39.1934361718353));
#37678=CARTESIAN_POINT('Ctrl Pts',(21.6034189034892,1.12818840242682,39.1729441104896));
#37679=CARTESIAN_POINT('Ctrl Pts',(21.6171114584664,1.1298250178489,39.1521929770421));
#37680=CARTESIAN_POINT('Ctrl Pts',(21.6303889112557,1.13146163327097,39.1312005406101));
#37681=CARTESIAN_POINT('Ctrl Pts',(21.6665573162937,1.13591985055228,39.0740161577577));
#37682=CARTESIAN_POINT('Ctrl Pts',(21.6997850246439,1.14037806783358,39.0148135949029));
#37683=CARTESIAN_POINT('Ctrl Pts',(21.7298411424651,1.14483628511489,38.9539275020369));
#37684=CARTESIAN_POINT('Ctrl Pts',(21.7614003660684,1.14951745774302,38.8899964970243));
#37685=CARTESIAN_POINT('Ctrl Pts',(21.789462086792,1.15419863037115,38.8242095647201));
#37686=CARTESIAN_POINT('Ctrl Pts',(21.813810486032,1.15887980299928,38.7569886434791));
#37687=CARTESIAN_POINT('Ctrl Pts',(21.8369363081649,1.16332592549403,38.6931430061166));
#37688=CARTESIAN_POINT('Ctrl Pts',(21.856712530907,1.16777204798877,38.6280044457409));
#37689=CARTESIAN_POINT('Ctrl Pts',(21.8730023608158,1.17221817048352,38.5619574799466));
#37690=CARTESIAN_POINT('Ctrl Pts',(21.8892823530286,1.17666160789183,38.4959504010002));
#37691=CARTESIAN_POINT('Ctrl Pts',(21.90208001124,1.18110504530014,38.4290364827223));
#37692=CARTESIAN_POINT('Ctrl Pts',(21.9113084892897,1.18554848270846,38.3616150142273));
#37693=CARTESIAN_POINT('Ctrl Pts',(21.9205345749982,1.18999076822389,38.2942110237121));
#37694=CARTESIAN_POINT('Ctrl Pts',(21.9261932507027,1.19443305373932,38.2263002326203));
#37695=CARTESIAN_POINT('Ctrl Pts',(21.9282491652835,1.19887533925475,38.1582899089341));
#37696=CARTESIAN_POINT('Ctrl Pts',(21.9303052555122,1.20331800429885,38.0902737747551));
#37697=CARTESIAN_POINT('Ctrl Pts',(21.9287579614393,1.20776066934295,38.0221585841003));
#37698=CARTESIAN_POINT('Ctrl Pts',(21.9236240288139,1.21220333438705,37.9543526427636));
#37699=CARTESIAN_POINT('Ctrl Pts',(21.9184845628255,1.21665078774448,37.886473620047));
#37700=CARTESIAN_POINT('Ctrl Pts',(21.9097507825299,1.2210982411019,37.8189050042981));
#37701=CARTESIAN_POINT('Ctrl Pts',(21.8974913247376,1.22554569445933,37.7520499612795));
#37702=CARTESIAN_POINT('Ctrl Pts',(21.8852242028801,1.22999592816582,37.685153123476));
#37703=CARTESIAN_POINT('Ctrl Pts',(21.8694271321472,1.2344461618723,37.6189712256426));
#37704=CARTESIAN_POINT('Ctrl Pts',(21.8502192575874,1.23889639557879,37.5538944646382));
#37705=CARTESIAN_POINT('Ctrl Pts',(21.8309788962331,1.24335415608515,37.4887076375589));
#37706=CARTESIAN_POINT('Ctrl Pts',(21.8083163849743,1.24781191659151,37.4246301410885));
#37707=CARTESIAN_POINT('Ctrl Pts',(21.7823994685512,1.25226967709787,37.3620334076611));
#37708=CARTESIAN_POINT('Ctrl Pts',(21.7728748658489,1.25390792746193,37.3390287798486));
#37709=CARTESIAN_POINT('Ctrl Pts',(21.7629111736797,1.25554617782599,37.3162239086065));
#37710=CARTESIAN_POINT('Ctrl Pts',(21.7525182496752,1.25718442819005,37.2936363466429));
#37711=CARTESIAN_POINT('Ctrl Pts',(21.7242347992446,1.26164278590963,37.2321662359342));
#37712=CARTESIAN_POINT('Ctrl Pts',(21.692657444663,1.26610114362921,37.1720645920368));
#37713=CARTESIAN_POINT('Ctrl Pts',(21.6579412609868,1.27055950134879,37.1137072787364));
#37714=CARTESIAN_POINT('Ctrl Pts',(21.6214902066828,1.27524065642214,37.0524336774676));
#37715=CARTESIAN_POINT('Ctrl Pts',(21.5815785269907,1.27992181149548,36.9930838459159));
#37716=CARTESIAN_POINT('Ctrl Pts',(21.5384427033784,1.28460296656883,36.9360684705183));
#37717=CARTESIAN_POINT('Ctrl Pts',(21.4974713161616,1.28904923421996,36.8819139690597));
#37718=CARTESIAN_POINT('Ctrl Pts',(21.4535918880559,1.29349550187109,36.8298657455208));
#37719=CARTESIAN_POINT('Ctrl Pts',(21.407052543974,1.29794176952222,36.7802478659247));
#37720=CARTESIAN_POINT('Ctrl Pts',(21.3605412908559,1.3023853534238,36.7306599354842));
#37721=CARTESIAN_POINT('Ctrl Pts',(21.311373643304,1.30682893732537,36.683499797911));
#37722=CARTESIAN_POINT('Ctrl Pts',(21.2598373041568,1.31127252122695,36.6390576589219));
#37723=CARTESIAN_POINT('Ctrl Pts',(21.2083143116984,1.31571495434575,36.594627029392));
#37724=CARTESIAN_POINT('Ctrl Pts',(21.1544242188662,1.32015738746455,36.5529133228303));
#37725=CARTESIAN_POINT('Ctrl Pts',(21.0984894509131,1.32459982058335,36.5141678893614));
#37726=CARTESIAN_POINT('Ctrl Pts',(21.0425498931683,1.32904263411545,36.4754191380533));
#37727=CARTESIAN_POINT('Ctrl Pts',(20.9845657196497,1.33348544764756,36.4396394429375));
#37728=CARTESIAN_POINT('Ctrl Pts',(20.9248885832387,1.33792826117966,36.4070370159113));
#37729=CARTESIAN_POINT('Ctrl Pts',(20.8651471238273,1.34237586339826,36.3743994483596));
#37730=CARTESIAN_POINT('Ctrl Pts',(20.8037094941599,1.34682346561685,36.3449462187376));
#37731=CARTESIAN_POINT('Ctrl Pts',(20.7409512806138,1.35127106783545,36.3188392108918));
#37732=CARTESIAN_POINT('Ctrl Pts',(20.6781538291989,1.35572145079656,36.2927158803482));
#37733=CARTESIAN_POINT('Ctrl Pts',(20.6140346155322,1.36017183375768,36.269943099653));
#37734=CARTESIAN_POINT('Ctrl Pts',(20.5489858398327,1.36462221671879,36.2506333233879));
#37735=CARTESIAN_POINT('Ctrl Pts',(20.4838270606544,1.36908012568793,36.2312908925104));
#37736=CARTESIAN_POINT('Ctrl Pts',(20.4177360617848,1.37353803465707,36.2154232658737));
#37737=CARTESIAN_POINT('Ctrl Pts',(20.3511157569468,1.37799594362621,36.2030919152148));
#37738=CARTESIAN_POINT('Ctrl Pts',(20.3266505544972,1.37963303678718,36.1985634311275));
#37739=CARTESIAN_POINT('Ctrl Pts',(20.3021140174735,1.38127012994815,36.1945113448649));
#37740=CARTESIAN_POINT('Ctrl Pts',(20.277526192677,1.38290722310913,36.1909369394181));
#37741=CARTESIAN_POINT('Ctrl Pts',(20.2105625873692,1.3873657574118,36.1812022403332));
#37742=CARTESIAN_POINT('Ctrl Pts',(20.1429538919583,1.39182429171447,36.1749758707396));
#37743=CARTESIAN_POINT('Ctrl Pts',(20.0750998695106,1.39628282601714,36.1723323506114));
#37744=CARTESIAN_POINT('Ctrl Pts',(20.0073627852413,1.40073367657666,36.1696933862695));
#37745=CARTESIAN_POINT('Ctrl Pts',(19.9393817025843,1.40518452713618,36.170625024732));
#37746=CARTESIAN_POINT('Ctrl Pts',(19.871563278678,1.4096353776957,36.1751502485867));
#37747=CARTESIAN_POINT('Ctrl Pts',(19.8038123646269,1.41408179765569,36.1796709678069));
#37748=CARTESIAN_POINT('Ctrl Pts',(19.7362242776704,1.41852821761569,36.1877781444111));
#37749=CARTESIAN_POINT('Ctrl Pts',(19.6692060914125,1.42297463757568,36.1994427272662));
#37750=CARTESIAN_POINT('Ctrl Pts',(19.6022324842504,1.42741809987012,36.2110995510848));
#37751=CARTESIAN_POINT('Ctrl Pts',(19.5358285100785,1.43186156216455,36.2263090000941));
#37752=CARTESIAN_POINT('Ctrl Pts',(19.4703946875471,1.43630502445899,36.2449903585368));
#37753=CARTESIAN_POINT('Ctrl Pts',(19.444808406263,1.4380425307171,36.2522952426684));
#37754=CARTESIAN_POINT('Ctrl Pts',(19.419370360307,1.43978003697522,36.2601304306196));
#37755=CARTESIAN_POINT('Ctrl Pts',(19.3941040087494,1.44151754323334,36.2684889831927));
#37756=CARTESIAN_POINT('Ctrl Pts',(19.3941040087494,0.647822633508007,36.2684889831927));
#37757=CARTESIAN_POINT('Ctrl Pts',(19.3296825780713,0.652272143768435,36.2898007231934));
#37758=CARTESIAN_POINT('Ctrl Pts',(19.2662997849573,0.656721654028864,36.3145443384515));
#37759=CARTESIAN_POINT('Ctrl Pts',(19.2043437516652,0.661171164289292,36.3425946138168));
#37760=CARTESIAN_POINT('Ctrl Pts',(19.1424379591573,0.66561706639612,36.3706221429255));
#37761=CARTESIAN_POINT('Ctrl Pts',(19.0819570792625,0.670062968502948,36.4019508116598));
#37762=CARTESIAN_POINT('Ctrl Pts',(19.0232707684852,0.674508870609776,36.436406730837));
#37763=CARTESIAN_POINT('Ctrl Pts',(18.9646118433448,0.678952698061392,36.4708465713532));
#37764=CARTESIAN_POINT('Ctrl Pts',(18.9077462502621,0.683396525513008,36.5084105175293));
#37765=CARTESIAN_POINT('Ctrl Pts',(18.8530188338067,0.687840352964625,36.5488788695599));
#37766=CARTESIAN_POINT('Ctrl Pts',(18.7982981155217,0.692283636529552,36.5893422686083));
#37767=CARTESIAN_POINT('Ctrl Pts',(18.7457154498577,0.69672692009448,36.6327090737228));
#37768=CARTESIAN_POINT('Ctrl Pts',(18.6955849742837,0.701170203659408,36.6787174814325));
#37769=CARTESIAN_POINT('Ctrl Pts',(18.6454071775631,0.705617681504766,36.7247693192231));
#37770=CARTESIAN_POINT('Ctrl Pts',(18.5976865603997,0.710065159350124,36.7734674081238));
#37771=CARTESIAN_POINT('Ctrl Pts',(18.5527018104802,0.714512637195483,36.8245116592016));
#37772=CARTESIAN_POINT('Ctrl Pts',(18.5076973583265,0.718962062928732,36.8755782664288));
#37773=CARTESIAN_POINT('Ctrl Pts',(18.4654314683306,0.723411488661982,36.9289926967059));
#37774=CARTESIAN_POINT('Ctrl Pts',(18.4261419147534,0.727860914395232,36.9844224435729));
#37775=CARTESIAN_POINT('Ctrl Pts',(18.38677833786,0.732318723050085,37.0399566226185));
#37776=CARTESIAN_POINT('Ctrl Pts',(18.3504025685493,0.736776531704938,37.0975132884453));
#37777=CARTESIAN_POINT('Ctrl Pts',(18.31720819634,0.741234340359791,37.1567321152321));
#37778=CARTESIAN_POINT('Ctrl Pts',(18.284794493295,0.745587309744439,37.2145582266594));
#37779=CARTESIAN_POINT('Ctrl Pts',(18.2554142752578,0.749940279129086,37.2739687353062));
#37780=CARTESIAN_POINT('Ctrl Pts',(18.2292031604449,0.754293248513733,37.3346104848368));
#37781=CARTESIAN_POINT('Ctrl Pts',(18.1996096019636,0.759207951874184,37.4030778191702));
#37782=CARTESIAN_POINT('Ctrl Pts',(18.1739551436919,0.764122655234634,37.4733458910155));
#37783=CARTESIAN_POINT('Ctrl Pts',(18.1524389775309,0.769037358595085,37.5449677260259));
#37784=CARTESIAN_POINT('Ctrl Pts',(18.1309889157911,0.773936962442971,37.6163695162608));
#37785=CARTESIAN_POINT('Ctrl Pts',(18.1136519233921,0.778836566290857,37.6891164859107));
#37786=CARTESIAN_POINT('Ctrl Pts',(18.1005789573201,0.783736170138742,37.7627430363586));
#37787=CARTESIAN_POINT('Ctrl Pts',(18.0875715999345,0.788611184572784,37.8360000806637));
#37788=CARTESIAN_POINT('Ctrl Pts',(18.0787857077949,0.793486199006826,37.9101276018189));
#37789=CARTESIAN_POINT('Ctrl Pts',(18.0743217702651,0.798361213440869,37.9846487432881));
#37790=CARTESIAN_POINT('Ctrl Pts',(18.0720415455723,0.800851420397402,38.0227149003028));
#37791=CARTESIAN_POINT('Ctrl Pts',(18.0708882467697,0.803341627353937,38.0608834971368));
#37792=CARTESIAN_POINT('Ctrl Pts',(18.0708702148579,0.80583183431047,38.0990895178969));
#37793=CARTESIAN_POINT('',(18.0708701424417,0.634793165648104,38.0992586653166));
#37794=CARTESIAN_POINT('Ctrl Pts',(19.3941040087494,0.476638002189708,36.2684889831927));
#37795=CARTESIAN_POINT('Ctrl Pts',(19.3294175465539,0.481100191651656,36.2898884002712));
#37796=CARTESIAN_POINT('Ctrl Pts',(19.2659395802241,0.485562381113605,36.3146945708179));
#37797=CARTESIAN_POINT('Ctrl Pts',(19.2040403110517,0.490024570575553,36.3427320265624));
#37798=CARTESIAN_POINT('Ctrl Pts',(19.1478875166129,0.494072508636116,36.3681665997014));
#37799=CARTESIAN_POINT('Ctrl Pts',(19.0930338622291,0.49812044669668,36.396259611507));
#37800=CARTESIAN_POINT('Ctrl Pts',(19.039736132611,0.502168384757243,36.4268485239264));
#37801=CARTESIAN_POINT('Ctrl Pts',(18.9809367333944,0.506634172094393,36.4605949834068));
#37802=CARTESIAN_POINT('Ctrl Pts',(18.9238067121829,0.511099959431543,36.4975088597523));
#37803=CARTESIAN_POINT('Ctrl Pts',(18.8687069543993,0.515565746768693,36.5374000505966));
#37804=CARTESIAN_POINT('Ctrl Pts',(18.8109614058647,0.520245973139844,36.5792067443038));
#37805=CARTESIAN_POINT('Ctrl Pts',(18.7554465291093,0.524926199510996,36.6242837043234));
#37806=CARTESIAN_POINT('Ctrl Pts',(18.7025482558196,0.529606425882147,36.6723580531438));
#37807=CARTESIAN_POINT('Ctrl Pts',(18.6522060845453,0.534060498632098,36.7181093972183));
#37808=CARTESIAN_POINT('Ctrl Pts',(18.604233914001,0.538514571382049,36.7665747903607));
#37809=CARTESIAN_POINT('Ctrl Pts',(18.5589324175991,0.542968644132,36.8174764018338));
#37810=CARTESIAN_POINT('Ctrl Pts',(18.513657035742,0.547420149282835,36.8683486705144));
#37811=CARTESIAN_POINT('Ctrl Pts',(18.4710495995293,0.551871654433669,36.9216540050198));
#37812=CARTESIAN_POINT('Ctrl Pts',(18.4313733960811,0.556323159584503,36.9770783044318));
#37813=CARTESIAN_POINT('Ctrl Pts',(18.3917065257618,0.56077361759705,37.0324895662522));
#37814=CARTESIAN_POINT('Ctrl Pts',(18.3549698047799,0.565224075609597,37.0900184039082));
#37815=CARTESIAN_POINT('Ctrl Pts',(18.3213846271721,0.569674533622144,37.1493197240892));
#37816=CARTESIAN_POINT('Ctrl Pts',(18.2877958901681,0.574125463299408,37.2086273290932));
#37817=CARTESIAN_POINT('Ctrl Pts',(18.257359599313,0.578576392976672,37.2697073608492));
#37818=CARTESIAN_POINT('Ctrl Pts',(18.2302515115956,0.583027322653936,37.3321895776363));
#37819=CARTESIAN_POINT('Ctrl Pts',(18.2031137457402,0.587483125242418,37.3947402004233));
#37820=CARTESIAN_POINT('Ctrl Pts',(18.179311649001,0.5919389278309,37.4586956198149));
#37821=CARTESIAN_POINT('Ctrl Pts',(18.158972662104,0.596394730419382,37.5236659839818));
#37822=CARTESIAN_POINT('Ctrl Pts',(18.1386207164334,0.600853371976063,37.5886777433394));
#37823=CARTESIAN_POINT('Ctrl Pts',(18.1217363932387,0.605312013532744,37.65470525861));
#37824=CARTESIAN_POINT('Ctrl Pts',(18.108396401476,0.609770655089425,37.7213466189892));
#37825=CARTESIAN_POINT('Ctrl Pts',(18.0950338599389,0.614236833484401,37.7881006291858));
#37826=CARTESIAN_POINT('Ctrl Pts',(18.085227675063,0.618703011879377,37.855470069508));
#37827=CARTESIAN_POINT('Ctrl Pts',(18.0790028157059,0.623169190274353,37.9230469699773));
#37828=CARTESIAN_POINT('Ctrl Pts',(18.076809014704,0.624743186741677,37.9468628127862));
#37829=CARTESIAN_POINT('Ctrl Pts',(18.0750595549418,0.626317183209,37.9707044216641));
#37830=CARTESIAN_POINT('Ctrl Pts',(18.0737539884187,0.627891179676323,37.9945539959639));
#37831=CARTESIAN_POINT('Ctrl Pts',(18.0718456821816,0.630191841666916,38.0294141816267));
#37832=CARTESIAN_POINT('Ctrl Pts',(18.070883565912,0.632492503657509,38.0643275905245));
#37833=CARTESIAN_POINT('Ctrl Pts',(18.0708701424417,0.634793165648104,38.0992586653166));
#37834=CARTESIAN_POINT('Ctrl Pts',(18.0708701850429,0.63643967452627,38.0991550480818));
#37835=CARTESIAN_POINT('Ctrl Pts',(18.0707960163012,0.647136816316794,38.2684914658409));
#37836=CARTESIAN_POINT('Ctrl Pts',(18.0930174737715,0.656903307811155,38.4371308561225));
#37837=CARTESIAN_POINT('Ctrl Pts',(18.1582675041732,0.67210444457396,38.6799011851684));
#37838=CARTESIAN_POINT('Ctrl Pts',(18.1845703861749,0.67714691526514,38.7576297569914));
#37839=CARTESIAN_POINT('Ctrl Pts',(18.2231528068951,0.683593516580006,38.8514900500262));
#37840=CARTESIAN_POINT('Ctrl Pts',(18.2308439642046,0.684841634406725,38.8694219384789));
#37841=CARTESIAN_POINT('Ctrl Pts',(18.2423267411974,0.686655017802892,38.8951111412327));
#37842=CARTESIAN_POINT('Ctrl Pts',(18.2459006862306,0.687212864084422,38.9029648840773));
#37843=CARTESIAN_POINT('Ctrl Pts',(18.2522231826203,0.688188580642212,38.9166149041945));
#37844=CARTESIAN_POINT('Ctrl Pts',(18.2549482000501,0.688605636372264,38.9224219835042));
#37845=CARTESIAN_POINT('Ctrl Pts',(18.2602703673209,0.68941357159051,38.9336181070046));
#37846=CARTESIAN_POINT('Ctrl Pts',(18.2628637245384,0.689804315978265,38.9390088809201));
#37847=CARTESIAN_POINT('Ctrl Pts',(18.2690840747754,0.690734667746149,38.9517865564289));
#37848=CARTESIAN_POINT('Ctrl Pts',(18.2727333199285,0.691275045090943,38.9591624353175));
#37849=CARTESIAN_POINT('Ctrl Pts',(18.285862423631,0.69320032785927,38.9852773252386));
#37850=CARTESIAN_POINT('Ctrl Pts',(18.2956006605865,0.69459423823625,39.003884066555));
#37851=CARTESIAN_POINT('Ctrl Pts',(18.3837937590825,0.706932227740955,39.1658989919137));
#37852=CARTESIAN_POINT('Ctrl Pts',(18.4798637686953,0.718545336308115,39.2989275004827));
#37853=CARTESIAN_POINT('Ctrl Pts',(18.6427729657352,0.735564467313776,39.472990751488));
#37854=CARTESIAN_POINT('Ctrl Pts',(18.6971823194854,0.740901450122557,39.5247232932139));
#37855=CARTESIAN_POINT('Ctrl Pts',(18.7717204429489,0.747657053450741,39.5877440006131));
#37856=CARTESIAN_POINT('Ctrl Pts',(18.7892270350464,0.749206704337762,39.6020259008141));
#37857=CARTESIAN_POINT('Ctrl Pts',(18.8149221637498,0.751423653507232,39.6222467566481));
#37858=CARTESIAN_POINT('Ctrl Pts',(18.8229122385359,0.752105184335773,39.6284335373905));
#37859=CARTESIAN_POINT('Ctrl Pts',(18.8354929635558,0.753165606238019,39.6380177256604));
#37860=CARTESIAN_POINT('Ctrl Pts',(18.840050581204,0.753547194083509,39.6414579171035));
#37861=CARTESIAN_POINT('Ctrl Pts',(18.8486349841852,0.754261010727628,39.6478779829543));
#37862=CARTESIAN_POINT('Ctrl Pts',(18.8526582191138,0.754593545653357,39.6508624984162));
#37863=CARTESIAN_POINT('Ctrl Pts',(18.8595633739831,0.755160790042152,39.6559433016052));
#37864=CARTESIAN_POINT('Ctrl Pts',(18.8624395340883,0.755396029692384,39.6580473173213));
#37865=CARTESIAN_POINT('Ctrl Pts',(18.8680420399243,0.755852238753741,39.6621219700122));
#37866=CARTESIAN_POINT('Ctrl Pts',(18.8707677018916,0.756073269352352,39.664093440276));
#37867=CARTESIAN_POINT('Ctrl Pts',(18.8780292384997,0.756659727816691,39.6693168309437));
#37868=CARTESIAN_POINT('Ctrl Pts',(18.8825741349209,0.757024307240007,39.6725562449382));
#37869=CARTESIAN_POINT('Ctrl Pts',(18.8989158878309,0.758326598704165,39.684097350207));
#37870=CARTESIAN_POINT('Ctrl Pts',(18.9107920682362,0.759257047103402,39.6922866413547));
#37871=CARTESIAN_POINT('Ctrl Pts',(19.0262125319464,0.768158508695826,39.769979778012));
#37872=CARTESIAN_POINT('Ctrl Pts',(19.1361903867827,0.77556621292686,39.8294324552203));
#37873=CARTESIAN_POINT('Ctrl Pts',(19.2552495734574,0.783281716279286,39.8795811647537));
#37874=CARTESIAN_POINT('Ctrl Pts',(19.2593524697077,0.7835472246046,39.8812926642275));
#37875=CARTESIAN_POINT('Ctrl Pts',(19.3930603468818,0.792188489346536,39.9365263085072));
#37876=CARTESIAN_POINT('Ctrl Pts',(19.5280898157622,0.800611551962914,39.9757659507804));
#37877=CARTESIAN_POINT('Ctrl Pts',(19.6814632105573,0.810550973013383,40.0027133225902));
#37878=CARTESIAN_POINT('Ctrl Pts',(19.6967884152628,0.811547629545846,40.0052155748134));
#37879=CARTESIAN_POINT('Ctrl Pts',(19.7199673222899,0.813061003573724,40.0087134121138));
#37880=CARTESIAN_POINT('Ctrl Pts',(19.7277999335788,0.813573425175118,40.0098461485));
#37881=CARTESIAN_POINT('Ctrl Pts',(19.7418935235069,0.814497379522793,40.0117958753232));
#37882=CARTESIAN_POINT('Ctrl Pts',(19.7481519960678,0.814908358030055,40.012630388614));
#37883=CARTESIAN_POINT('Ctrl Pts',(19.761600592569,0.815793009911337,40.0143564902148));
#37884=CARTESIAN_POINT('Ctrl Pts',(19.7687918492438,0.816266981316793,40.015238323999));
#37885=CARTESIAN_POINT('Ctrl Pts',(19.788289058924,0.817554632051001,40.0175177764687));
#37886=CARTESIAN_POINT('Ctrl Pts',(19.8006036118689,0.818370725618757,40.0188374120764));
#37887=CARTESIAN_POINT('Ctrl Pts',(19.8578997288973,0.822181417956825,40.0244197991112));
#37888=CARTESIAN_POINT('Ctrl Pts',(19.9030062547931,0.825220898845349,40.027219678699));
#37889=CARTESIAN_POINT('Ctrl Pts',(19.9803390362335,0.830503549754191,40.0292982725189));
#37890=CARTESIAN_POINT('Ctrl Pts',(20.0125266743961,0.832723378863548,40.0293577368835));
#37891=CARTESIAN_POINT('Ctrl Pts',(20.2134201905368,0.846703066048316,40.0247016366783));
#37892=CARTESIAN_POINT('Ctrl Pts',(20.3808766483001,0.858992780802981,39.9986703579415));
#37893=CARTESIAN_POINT('Ctrl Pts',(20.5792177119029,0.873336611371616,39.9405134148323));
#37894=CARTESIAN_POINT('Ctrl Pts',(20.6153149072154,0.875933970052457,39.9287621010812));
#37895=CARTESIAN_POINT('Ctrl Pts',(20.65816279416,0.878982612702795,39.9134005276838));
#37896=CARTESIAN_POINT('Ctrl Pts',(20.6652660212754,0.879486853049573,39.9108066884641));
#37897=CARTESIAN_POINT('Ctrl Pts',(20.67627343415,0.880266241686463,39.9067136700572));
#37898=CARTESIAN_POINT('Ctrl Pts',(20.6801882100622,0.880543035806873,39.9052434857994));
#37899=CARTESIAN_POINT('Ctrl Pts',(20.6874327623011,0.881054488765561,39.9024959009012));
#37900=CARTESIAN_POINT('Ctrl Pts',(20.6907637579902,0.881289343208352,39.9012220036757));
#37901=CARTESIAN_POINT('Ctrl Pts',(20.6983003141535,0.881820026355001,39.8983157616005));
#37902=CARTESIAN_POINT('Ctrl Pts',(20.7025036839451,0.882115524078313,39.8966779016372));
#37903=CARTESIAN_POINT('Ctrl Pts',(20.7152398133634,0.883009528429194,39.8916636884429));
#37904=CARTESIAN_POINT('Ctrl Pts',(20.723754414842,0.883605364522005,39.8882411241691));
#37905=CARTESIAN_POINT('Ctrl Pts',(20.7960084593035,0.888648508523762,39.8585969768404));
#37906=CARTESIAN_POINT('Ctrl Pts',(20.8583326581129,0.892912407315166,39.8290344517594));
#37907=CARTESIAN_POINT('Ctrl Pts',(21.0162270894044,0.903820048941298,39.7434920364688));
#37908=CARTESIAN_POINT('Ctrl Pts',(21.108794701564,0.910331683279342,39.6825167892982));
#37909=CARTESIAN_POINT('Ctrl Pts',(21.247491056949,0.920987725348736,39.5729820484525));
#37910=CARTESIAN_POINT('Ctrl Pts',(21.2972119206925,0.925019397247569,39.5293880463665));
#37911=CARTESIAN_POINT('Ctrl Pts',(21.3723055270313,0.931559816666425,39.4563972152351));
#37912=CARTESIAN_POINT('Ctrl Pts',(21.3991985193583,0.934003861492606,39.4286380414267));
#37913=CARTESIAN_POINT('Ctrl Pts',(21.4328130327208,0.937205259956507,39.3917877904446));
#37914=CARTESIAN_POINT('Ctrl Pts',(21.4403147516351,0.937929609547148,39.3834182053455));
#37915=CARTESIAN_POINT('Ctrl Pts',(21.4523581108634,0.939108953592014,39.3697429822542));
#37916=CARTESIAN_POINT('Ctrl Pts',(21.4569449012006,0.939562072951377,39.3644773133267));
#37917=CARTESIAN_POINT('Ctrl Pts',(21.4656882296254,0.940433514392385,39.3543291771277));
#37918=CARTESIAN_POINT('Ctrl Pts',(21.4698492204189,0.940851646005231,39.3494506547402));
#37919=CARTESIAN_POINT('Ctrl Pts',(21.479293127305,0.941808531647759,39.3382657547474));
#37920=CARTESIAN_POINT('Ctrl Pts',(21.4845601507583,0.942347919664299,39.3319461802863));
#37921=CARTESIAN_POINT('Ctrl Pts',(21.4983961657164,0.943780213787,39.3151276235494));
#37922=CARTESIAN_POINT('Ctrl Pts',(21.5068950982176,0.944675896160014,39.3045718567451));
#37923=CARTESIAN_POINT('Ctrl Pts',(21.5731329467551,0.951784841024621,39.2205056108505));
#37924=CARTESIAN_POINT('Ctrl Pts',(21.6255621293883,0.958204267880045,39.1429875795964));
#37925=CARTESIAN_POINT('Ctrl Pts',(21.7516517355951,0.975973155484309,38.9238137003631));
#37926=CARTESIAN_POINT('Ctrl Pts',(21.8137055665971,0.987578793068131,38.7763303791634));
#37927=CARTESIAN_POINT('Ctrl Pts',(21.864757995785,1.00055132173768,38.5950335299302));
#37928=CARTESIAN_POINT('Ctrl Pts',(21.8719769585452,1.00252093295614,38.5669936489798));
#37929=CARTESIAN_POINT('Ctrl Pts',(21.8801437592704,1.00492290312263,38.5320304732669));
#37930=CARTESIAN_POINT('Ctrl Pts',(21.8816884571423,1.00538607316343,38.5252522066387));
#37931=CARTESIAN_POINT('Ctrl Pts',(21.884072273019,1.00611501726964,38.514524458376));
#37932=CARTESIAN_POINT('Ctrl Pts',(21.8849356735058,1.00638213170949,38.5105805207751));
#37933=CARTESIAN_POINT('Ctrl Pts',(21.8865400994027,1.00688438491899,38.5031399081467));
#37934=CARTESIAN_POINT('Ctrl Pts',(21.8872837797117,1.0071196651795,38.4996439256088));
#37935=CARTESIAN_POINT('Ctrl Pts',(21.8889655145265,1.00765749491545,38.4916288333961));
#37936=CARTESIAN_POINT('Ctrl Pts',(21.8898970702666,1.00795967389074,38.4871084126011));
#37937=CARTESIAN_POINT('Ctrl Pts',(21.892336662193,1.00876269305062,38.4750514446379));
#37938=CARTESIAN_POINT('Ctrl Pts',(21.8938159160968,1.0092619547087,38.4675090609884));
#37939=CARTESIAN_POINT('Ctrl Pts',(21.9043118566782,1.01289890629662,38.4122458399231));
#37940=CARTESIAN_POINT('Ctrl Pts',(21.9115695930745,1.01594549089061,38.3642039177265));
#37941=CARTESIAN_POINT('Ctrl Pts',(21.9183505489168,1.01967728866055,38.3040045745128));
#37942=CARTESIAN_POINT('Ctrl Pts',(21.9195830202224,1.02041344054866,38.2920617938659));
#37943=CARTESIAN_POINT('Ctrl Pts',(21.9221052624138,1.02206349234712,38.2651641665881));
#37944=CARTESIAN_POINT('Ctrl Pts',(21.9233321530883,1.022975732715,38.2502041447357));
#37945=CARTESIAN_POINT('Ctrl Pts',(21.9360555465332,1.03396548389485,38.0691459421283));
#37946=CARTESIAN_POINT('Ctrl Pts',(21.9261779276229,1.04364714775701,37.902256663981));
#37947=CARTESIAN_POINT('Ctrl Pts',(21.8869798655989,1.05667509858616,37.6966621105194));
#37948=CARTESIAN_POINT('Ctrl Pts',(21.8775675320878,1.05937589815297,37.6548997920163));
#37949=CARTESIAN_POINT('Ctrl Pts',(21.8638423032375,1.0628668092626,37.6022353652431));
#37950=CARTESIAN_POINT('Ctrl Pts',(21.8608082343969,1.06361582274127,37.5910103457486));
#37951=CARTESIAN_POINT('Ctrl Pts',(21.8557684021907,1.06482505419686,37.5730122579171));
#37952=CARTESIAN_POINT('Ctrl Pts',(21.8538265605983,1.06528320764849,37.5662214654952));
#37953=CARTESIAN_POINT('Ctrl Pts',(21.8500597299149,1.06615752388676,37.5533170402039));
#37954=CARTESIAN_POINT('Ctrl Pts',(21.8482416139508,1.06657345907108,37.5472014855224));
#37955=CARTESIAN_POINT('Ctrl Pts',(21.8440241549386,1.06752474309475,37.533268725194));
#37956=CARTESIAN_POINT('Ctrl Pts',(21.8416053913345,1.06806071696698,37.525457572517));
#37957=CARTESIAN_POINT('Ctrl Pts',(21.8351802944888,1.06946009850651,37.5051658578971));
#37958=CARTESIAN_POINT('Ctrl Pts',(21.8310963443489,1.07032602107947,37.492710502936));
#37959=CARTESIAN_POINT('Ctrl Pts',(21.801802083034,1.07637953703526,37.4063508155474));
#37960=CARTESIAN_POINT('Ctrl Pts',(21.7722551273496,1.08170917872181,37.3340046641784));
#37961=CARTESIAN_POINT('Ctrl Pts',(21.6665824691851,1.09871027612872,37.1143555258832));
#37962=CARTESIAN_POINT('Ctrl Pts',(21.5758306126613,1.11077888950312,36.9749475707211));
#37963=CARTESIAN_POINT('Ctrl Pts',(21.4439390251137,1.12489334092605,36.8201545880476));
#37964=CARTESIAN_POINT('Ctrl Pts',(21.4186473943562,1.12747398346793,36.7921757680144));
#37965=CARTESIAN_POINT('Ctrl Pts',(21.3873440277018,1.13050364960865,36.7595240797643));
#37966=CARTESIAN_POINT('Ctrl Pts',(21.3821063372239,1.1310052850008,36.7541243663983));
#37967=CARTESIAN_POINT('Ctrl Pts',(21.3739230311748,1.13178067156206,36.7457860695225));
#37968=CARTESIAN_POINT('Ctrl Pts',(21.3709993403181,1.13205606075559,36.7428262179251));
#37969=CARTESIAN_POINT('Ctrl Pts',(21.3655588450559,1.1325654468632,36.737353955167));
#37970=CARTESIAN_POINT('Ctrl Pts',(21.3630446924697,1.1327996348585,36.7348390682933));
#37971=CARTESIAN_POINT('Ctrl Pts',(21.3573303355864,1.13332920121472,36.7291545660522));
#37972=CARTESIAN_POINT('Ctrl Pts',(21.3541259813858,1.13362424720658,36.7259892026511));
#37973=CARTESIAN_POINT('Ctrl Pts',(21.3443734919628,1.13451655867876,36.716422635718));
#37974=CARTESIAN_POINT('Ctrl Pts',(21.3377907227284,1.13511116180941,36.7100566921425));
#37975=CARTESIAN_POINT('Ctrl Pts',(21.2517062529015,1.14279172802983,36.6279858393434));
#37976=CARTESIAN_POINT('Ctrl Pts',(21.1659154650618,1.1494057570229,36.5591421675447));
#37977=CARTESIAN_POINT('Ctrl Pts',(21.0049569339048,1.1610022196217,36.4511636110249));
#37978=CARTESIAN_POINT('Ctrl Pts',(20.9322112546202,1.16598993992046,36.4089702550115));
#37979=CARTESIAN_POINT('Ctrl Pts',(20.7873145392698,1.17579597998761,36.3371274997301));
#37980=CARTESIAN_POINT('Ctrl Pts',(20.7156642217301,1.18058974441858,36.3068446062097));
#37981=CARTESIAN_POINT('Ctrl Pts',(20.6244491535183,1.18673977146044,36.2746321574692));
#37982=CARTESIAN_POINT('Ctrl Pts',(20.6064177683034,1.18795749820621,36.268562871661));
#37983=CARTESIAN_POINT('Ctrl Pts',(20.5801307918007,1.18973690232629,36.2601455489157));
#37984=CARTESIAN_POINT('Ctrl Pts',(20.5719442699373,1.19029163574229,36.2575842258181));
#37985=CARTESIAN_POINT('Ctrl Pts',(20.5575792945976,1.19126615697577,36.2531948128539));
#37986=CARTESIAN_POINT('Ctrl Pts',(20.5514082131198,1.19168516518386,36.2513429063608));
#37987=CARTESIAN_POINT('Ctrl Pts',(20.5394180026662,1.19250003474943,36.2478100901195));
#37988=CARTESIAN_POINT('Ctrl Pts',(20.5335999996139,1.19289577469736,36.2461256021853));
#37989=CARTESIAN_POINT('Ctrl Pts',(20.5196853622553,1.1938431070439,36.242167821334));
#37990=CARTESIAN_POINT('Ctrl Pts',(20.5115816613939,1.19439551454689,36.2399200340369));
#37991=CARTESIAN_POINT('Ctrl Pts',(20.4823193943168,1.19639290432491,36.2320090166902));
#37992=CARTESIAN_POINT('Ctrl Pts',(20.4610801117618,1.19784768074824,36.2266534288626));
#37993=CARTESIAN_POINT('Ctrl Pts',(20.2939809623087,1.20933667846055,36.1875323367276));
#37994=CARTESIAN_POINT('Ctrl Pts',(20.1447568125222,1.21991551290703,36.1704959383719));
#37995=CARTESIAN_POINT('Ctrl Pts',(19.9115029081894,1.23655862434039,36.1710886469682));
#37996=CARTESIAN_POINT('Ctrl Pts',(19.8280048581693,1.24252374294072,36.1767345175105));
#37997=CARTESIAN_POINT('Ctrl Pts',(19.7092569851297,1.25082747417029,36.1925616790356));
#37998=CARTESIAN_POINT('Ctrl Pts',(19.6735205398377,1.25330204619476,36.1983522867459));
#37999=CARTESIAN_POINT('Ctrl Pts',(19.6306543875835,1.25622455230929,36.2065423744961));
#38000=CARTESIAN_POINT('Ctrl Pts',(19.6233512429974,1.25672084510487,36.2079815859043));
#38001=CARTESIAN_POINT('Ctrl Pts',(19.6119922777559,1.25749004304902,36.2102884444262));
#38002=CARTESIAN_POINT('Ctrl Pts',(19.6079307133826,1.25776453970295,36.2111269415111));
#38003=CARTESIAN_POINT('Ctrl Pts',(19.6003871733627,1.25827331546823,36.212709661152));
#38004=CARTESIAN_POINT('Ctrl Pts',(19.5969045848095,1.25850777947081,36.2134504191743));
#38005=CARTESIAN_POINT('Ctrl Pts',(19.588993945551,1.25903942215689,36.2151559434509));
#38006=CARTESIAN_POINT('Ctrl Pts',(19.5845672387149,1.25933625923392,36.2161266719367));
#38007=CARTESIAN_POINT('Ctrl Pts',(19.5710707273061,1.26023936668985,36.2191361951521));
#38008=CARTESIAN_POINT('Ctrl Pts',(19.5620120387085,1.26084287958441,36.2212249928441));
#38009=CARTESIAN_POINT('Ctrl Pts',(19.4993892157924,1.26499889368438,36.2361424283669));
#38010=CARTESIAN_POINT('Ctrl Pts',(19.4463857933544,1.26843511091169,36.2511932508716));
#38011=CARTESIAN_POINT('Ctrl Pts',(19.3941039987112,1.2718084690693,36.2684889865135));
#38012=CARTESIAN_POINT('Origin',(20.,-1.3495818343519,38.1));
#38013=CARTESIAN_POINT('',(19.3941044697279,2.2350068401775,36.268488830693));
#38014=CARTESIAN_POINT('',(19.3941040086996,2.0626282966298,36.2684889832092));
#38015=CARTESIAN_POINT('',(19.3941040087494,-1.3495818343519,36.2684889831927));
#38016=CARTESIAN_POINT('',(18.0708707501997,1.59958183435189,38.1017013127004));
#38017=CARTESIAN_POINT('Ctrl Pts',(19.3941044697278,2.2350068401775,36.268488830693));
#38018=CARTESIAN_POINT('Ctrl Pts',(19.4507932707691,2.2314404515271,36.2497351961299));
#38019=CARTESIAN_POINT('Ctrl Pts',(19.5083755801345,2.22787598191983,36.2336059050976));
#38020=CARTESIAN_POINT('Ctrl Pts',(19.6569378025591,2.21866594071238,36.1993601201359));
#38021=CARTESIAN_POINT('Ctrl Pts',(19.7485745867547,2.21296672935016,36.1850834272658));
#38022=CARTESIAN_POINT('Ctrl Pts',(19.8543542171333,2.20618824044174,36.1763283007706));
#38023=CARTESIAN_POINT('Ctrl Pts',(19.8678448657718,2.20532023007072,36.1753544466455));
#38024=CARTESIAN_POINT('Ctrl Pts',(19.8895458458601,2.20391782389648,36.1740171453559));
#38025=CARTESIAN_POINT('Ctrl Pts',(19.8977503612361,2.20338620896967,36.1735641499162));
#38026=CARTESIAN_POINT('Ctrl Pts',(19.9123580233041,2.20243709349871,36.1728511977098));
#38027=CARTESIAN_POINT('Ctrl Pts',(19.9187600810145,2.20202023727746,36.1725707026816));
#38028=CARTESIAN_POINT('Ctrl Pts',(19.932141008767,2.20114705455525,36.1720512259766));
#38029=CARTESIAN_POINT('Ctrl Pts',(19.9391200049021,2.20069054826806,36.1718182290058));
#38030=CARTESIAN_POINT('Ctrl Pts',(19.9573427794452,2.19949565762935,36.1713088851594));
#38031=CARTESIAN_POINT('Ctrl Pts',(19.9685878496746,2.1987554089788,36.171092971994));
#38032=CARTESIAN_POINT('Ctrl Pts',(20.0185830385412,2.19545096404046,36.170570322036));
#38033=CARTESIAN_POINT('Ctrl Pts',(20.0573329530689,2.19285393954807,36.171332901201));
#38034=CARTESIAN_POINT('Ctrl Pts',(20.1623034239754,2.18571604444189,36.1765647789792));
#38035=CARTESIAN_POINT('Ctrl Pts',(20.2283544184992,2.18111181523569,36.1832845404902));
#38036=CARTESIAN_POINT('Ctrl Pts',(20.4101714268752,2.16815884595209,36.2113134340679));
#38037=CARTESIAN_POINT('Ctrl Pts',(20.5245315418614,2.15967931616343,36.2398272994171));
#38038=CARTESIAN_POINT('Ctrl Pts',(20.6490561115131,2.15037989891157,36.2832797552791));
#38039=CARTESIAN_POINT('Ctrl Pts',(20.6624801357608,2.14937679889695,36.2881318016347));
#38040=CARTESIAN_POINT('Ctrl Pts',(20.7212649547765,2.1449846921599,36.3101199545975));
#38041=CARTESIAN_POINT('Ctrl Pts',(20.7660285439669,2.14164128144961,36.3288153998273));
#38042=CARTESIAN_POINT('Ctrl Pts',(20.81702038343,2.13787068345194,36.3524075590737));
#38043=CARTESIAN_POINT('Ctrl Pts',(20.8239776408362,2.1373570747388,36.355677065808));
#38044=CARTESIAN_POINT('Ctrl Pts',(20.8350826227637,2.13653884151751,36.360977029408));
#38045=CARTESIAN_POINT('Ctrl Pts',(20.8392428352544,2.13623266628363,36.3629809029084));
#38046=CARTESIAN_POINT('Ctrl Pts',(20.8466122196426,2.13569099391951,36.3665632126058));
#38047=CARTESIAN_POINT('Ctrl Pts',(20.8498242436171,2.13545513439346,36.3681356571261));
#38048=CARTESIAN_POINT('Ctrl Pts',(20.8566546760643,2.13495408795059,36.3715030700618));
#38049=CARTESIAN_POINT('Ctrl Pts',(20.8602718203646,2.13468905424524,36.3733004700711));
#38050=CARTESIAN_POINT('Ctrl Pts',(20.8701047460266,2.13396933174123,36.3782251301066));
#38051=CARTESIAN_POINT('Ctrl Pts',(20.8763093707476,2.13351600313624,36.3813747173965));
#38052=CARTESIAN_POINT('Ctrl Pts',(20.9083037157767,2.13118194764366,36.3978339793025));
#38053=CARTESIAN_POINT('Ctrl Pts',(20.9338093302124,2.12933321831063,36.4116916285343));
#38054=CARTESIAN_POINT('Ctrl Pts',(21.097610775992,2.11747521889453,36.5055362700835));
#38055=CARTESIAN_POINT('Ctrl Pts',(21.2258408462013,2.10821859579922,36.6018709974587));
#38056=CARTESIAN_POINT('Ctrl Pts',(21.4074414563538,2.09296175578713,36.7774046579686));
#38057=CARTESIAN_POINT('Ctrl Pts',(21.4694020364037,2.08725421997025,36.8466029641151));
#38058=CARTESIAN_POINT('Ctrl Pts',(21.5344156480109,2.08046649715671,36.9306864352825));
#38059=CARTESIAN_POINT('Ctrl Pts',(21.5425781792487,2.07959826908749,36.9414758787773));
#38060=CARTESIAN_POINT('Ctrl Pts',(21.5555153509736,2.07819557842961,36.9589557036772));
#38061=CARTESIAN_POINT('Ctrl Pts',(21.5603619919794,2.07766389854119,36.9655924260498));
#38062=CARTESIAN_POINT('Ctrl Pts',(21.5689122600384,2.07671470826916,36.9774591568571));
#38063=CARTESIAN_POINT('Ctrl Pts',(21.5726325324638,2.07629784256363,36.9826770652986));
#38064=CARTESIAN_POINT('Ctrl Pts',(21.5803518669238,2.0754246820855,36.9936188324199));
#38065=CARTESIAN_POINT('Ctrl Pts',(21.5843459827438,2.07496820773579,36.9993460507146));
#38066=CARTESIAN_POINT('Ctrl Pts',(21.59469109849,2.07377349443919,37.0143530473067));
#38067=CARTESIAN_POINT('Ctrl Pts',(21.6009921333417,2.07303339222261,37.0236667869904));
#38068=CARTESIAN_POINT('Ctrl Pts',(21.6286316927265,2.06973055181848,37.0653013372799));
#38069=CARTESIAN_POINT('Ctrl Pts',(21.6490741740066,2.06713502475511,37.0982033557684));
#38070=CARTESIAN_POINT('Ctrl Pts',(21.7017897352187,2.06000246433147,37.1890390361639));
#38071=CARTESIAN_POINT('Ctrl Pts',(21.7320865344145,2.05540219003107,37.2480534855265));
#38072=CARTESIAN_POINT('Ctrl Pts',(21.7856966813067,2.04620233643336,37.3672146369147));
#38073=CARTESIAN_POINT('Ctrl Pts',(21.8091535209082,2.04161238838394,37.4272073576387));
#38074=CARTESIAN_POINT('Ctrl Pts',(21.8633663487556,2.02941308867271,37.5893442381055));
#38075=CARTESIAN_POINT('Ctrl Pts',(21.8887337073943,2.0218109901199,37.6930686912955));
#38076=CARTESIAN_POINT('Ctrl Pts',(21.9077191548918,2.013577731312,37.8129988745062));
#38077=CARTESIAN_POINT('Ctrl Pts',(21.9098669394027,2.0125808918645,37.8276577033432));
#38078=CARTESIAN_POINT('Ctrl Pts',(21.9125991992918,2.01121664867235,37.8479311901059));
#38079=CARTESIAN_POINT('Ctrl Pts',(21.9133281606586,2.01084171467088,37.8535253894243));
#38080=CARTESIAN_POINT('Ctrl Pts',(21.9144539713393,2.01024464933028,37.8624711852676));
#38081=CARTESIAN_POINT('Ctrl Pts',(21.9148665768341,2.01002165268001,37.8658207106375));
#38082=CARTESIAN_POINT('Ctrl Pts',(21.9157070536717,2.00955855915947,37.8727944562693));
#38083=CARTESIAN_POINT('Ctrl Pts',(21.9161334325785,2.00931855246834,37.8764188214585));
#38084=CARTESIAN_POINT('Ctrl Pts',(21.9171374437943,2.00874081014297,37.885167119784));
#38085=CARTESIAN_POINT('Ctrl Pts',(21.917704827661,2.00840364385596,37.8902922502798));
#38086=CARTESIAN_POINT('Ctrl Pts',(21.9196075787314,2.00723425761653,37.9081334344469));
#38087=CARTESIAN_POINT('Ctrl Pts',(21.9208371082332,2.0064077002014,37.9208607801551));
#38088=CARTESIAN_POINT('Ctrl Pts',(21.9273685714265,2.00154867294746,37.9962998842796));
#38089=CARTESIAN_POINT('Ctrl Pts',(21.9297262076623,1.9976590302256,38.0592350121007));
#38090=CARTESIAN_POINT('Ctrl Pts',(21.9280292278797,1.98869101391914,38.2068288926908));
#38091=CARTESIAN_POINT('Ctrl Pts',(21.9214849962555,1.98367277918552,38.2913257055998));
#38092=CARTESIAN_POINT('Ctrl Pts',(21.9040617944663,1.97636140845724,38.4122469062855));
#38093=CARTESIAN_POINT('Ctrl Pts',(21.8976310379399,1.97410943440645,38.4492073559744));
#38094=CARTESIAN_POINT('Ctrl Pts',(21.8726351533664,1.96654513500071,38.5716186951708));
#38095=CARTESIAN_POINT('Ctrl Pts',(21.8493422911781,1.96115271786269,38.6559826809058));
#38096=CARTESIAN_POINT('Ctrl Pts',(21.8159700956865,1.95471227839766,38.7511338384985));
#38097=CARTESIAN_POINT('Ctrl Pts',(21.8113965090545,1.95385093304808,38.7637509596665));
#38098=CARTESIAN_POINT('Ctrl Pts',(21.8038218761256,1.9524572270829,38.7839855310286));
#38099=CARTESIAN_POINT('Ctrl Pts',(21.8009032783104,1.95192759154989,38.7916335346268));
#38100=CARTESIAN_POINT('Ctrl Pts',(21.7956149040682,1.95098073664984,38.8052309422904));
#38101=CARTESIAN_POINT('Ctrl Pts',(21.7932639991833,1.95056415068805,38.8111875935802));
#38102=CARTESIAN_POINT('Ctrl Pts',(21.7882820050351,1.94969022556804,38.8236290500042));
#38103=CARTESIAN_POINT('Ctrl Pts',(21.7856452042971,1.94923270010994,38.8301114529622));
#38104=CARTESIAN_POINT('Ctrl Pts',(21.778652424007,1.94803221223502,38.8470382659769));
#38105=CARTESIAN_POINT('Ctrl Pts',(21.774239763459,1.94728735315036,38.8574588231719));
#38106=CARTESIAN_POINT('Ctrl Pts',(21.7540358815899,1.94393217260906,38.9040252209428));
#38107=CARTESIAN_POINT('Ctrl Pts',(21.7372309517583,1.94128776839284,38.9397182052802));
#38108=CARTESIAN_POINT('Ctrl Pts',(21.644890692471,1.92745172903296,39.1211908134855));
#38109=CARTESIAN_POINT('Ctrl Pts',(21.5520706900964,1.9156531798475,39.2573913118662));
#38110=CARTESIAN_POINT('Ctrl Pts',(21.3896674349672,1.8982745223557,39.4404719560063));
#38111=CARTESIAN_POINT('Ctrl Pts',(21.3324400903879,1.89261746114329,39.4973715463614));
#38112=CARTESIAN_POINT('Ctrl Pts',(21.2647991758318,1.8865714887543,39.5566786271996));
#38113=CARTESIAN_POINT('Ctrl Pts',(21.2577402972361,1.88594783549258,39.5627778134152));
#38114=CARTESIAN_POINT('Ctrl Pts',(21.2471822112282,1.88502615799459,39.5717675362585));
#38115=CARTESIAN_POINT('Ctrl Pts',(21.2437167279855,1.88472539649303,39.5746972063317));
#38116=CARTESIAN_POINT('Ctrl Pts',(21.2375142213121,1.88419027803698,39.5799033014332));
#38117=CARTESIAN_POINT('Ctrl Pts',(21.2347812112329,1.88395558612682,39.5821843983272));
#38118=CARTESIAN_POINT('Ctrl Pts',(21.2288563438598,1.88344917494439,39.5871018056004));
#38119=CARTESIAN_POINT('Ctrl Pts',(21.2256623176153,1.88317764993617,39.5897354053787));
#38120=CARTESIAN_POINT('Ctrl Pts',(21.2167227241839,1.88242172028747,39.5970582382639));
#38121=CARTESIAN_POINT('Ctrl Pts',(21.2109584816305,1.88193891551266,39.601724713925));
#38122=CARTESIAN_POINT('Ctrl Pts',(21.1772248881182,1.87913925505379,39.6287134030862));
#38123=CARTESIAN_POINT('Ctrl Pts',(21.1486636073784,1.87687154210921,39.6502888177987));
#38124=CARTESIAN_POINT('Ctrl Pts',(21.0527748065696,1.86952836687475,39.7186179579998));
#38125=CARTESIAN_POINT('Ctrl Pts',(20.9830645237154,1.86460965496047,39.761880042975));
#38126=CARTESIAN_POINT('Ctrl Pts',(20.7767106452603,1.85061531469911,39.8724005276207));
#38127=CARTESIAN_POINT('Ctrl Pts',(20.6346065649354,1.84159165283577,39.9281004588631));
#38128=CARTESIAN_POINT('Ctrl Pts',(20.4663691426416,1.83057383749607,39.9720354583529));
#38129=CARTESIAN_POINT('Ctrl Pts',(20.4452046962944,1.8291831386634,39.9771813050127));
#38130=CARTESIAN_POINT('Ctrl Pts',(20.4157749063247,1.8272410304509,39.9838110709465));
#38131=CARTESIAN_POINT('Ctrl Pts',(20.4075796596619,1.82669933387507,39.9856011617371));
#38132=CARTESIAN_POINT('Ctrl Pts',(20.3934542282003,1.82576403053848,39.9885901961467));
#38133=CARTESIAN_POINT('Ctrl Pts',(20.3875295508042,1.82537124185823,39.989814806943));
#38134=CARTESIAN_POINT('Ctrl Pts',(20.3752834750821,1.82455830403695,39.9922860206138));
#38135=CARTESIAN_POINT('Ctrl Pts',(20.368961403357,1.82413804138893,39.9935288621059));
#38136=CARTESIAN_POINT('Ctrl Pts',(20.3541954083266,1.82315505378918,39.9963549180992));
#38137=CARTESIAN_POINT('Ctrl Pts',(20.3457469527733,1.82259155677552,39.9979134340911));
#38138=CARTESIAN_POINT('Ctrl Pts',(20.3184745667366,1.82076891427311,40.002756324953));
#38139=CARTESIAN_POINT('Ctrl Pts',(20.2996126491822,1.81950278697212,40.0058173831284));
#38140=CARTESIAN_POINT('Ctrl Pts',(20.2553120899749,1.81651509168533,40.0123329326847));
#38141=CARTESIAN_POINT('Ctrl Pts',(20.2298442977432,1.81478674540491,40.015560753924));
#38142=CARTESIAN_POINT('Ctrl Pts',(20.1382329002551,1.80852957207585,40.0253185101236));
#38143=CARTESIAN_POINT('Ctrl Pts',(20.0718320083648,1.80391760089509,40.0289370902873));
#38144=CARTESIAN_POINT('Ctrl Pts',(19.8583148939675,1.78888284249018,40.0295328244532));
#38145=CARTESIAN_POINT('Ctrl Pts',(19.7116896374633,1.77820835032208,40.0131250442843));
#38146=CARTESIAN_POINT('Ctrl Pts',(19.5346473595094,1.7656275994403,39.9724811158433));
#38147=CARTESIAN_POINT('Ctrl Pts',(19.5011517467772,1.76326395740075,39.963837276327));
#38148=CARTESIAN_POINT('Ctrl Pts',(19.4612129796655,1.76047983247138,39.9523767337198));
#38149=CARTESIAN_POINT('Ctrl Pts',(19.454532011864,1.76001526768932,39.9504204101872));
#38150=CARTESIAN_POINT('Ctrl Pts',(19.4435992758105,1.75925712987044,39.9471547255062));
#38151=CARTESIAN_POINT('Ctrl Pts',(19.4393412581086,1.75896237286127,39.945866767122));
#38152=CARTESIAN_POINT('Ctrl Pts',(19.4316896738131,1.75843368004899,39.9435234089884));
#38153=CARTESIAN_POINT('Ctrl Pts',(19.4282945531312,1.75819944275547,39.9424733563879));
#38154=CARTESIAN_POINT('Ctrl Pts',(19.4208859263506,1.75768907522686,39.9401595449769));
#38155=CARTESIAN_POINT('Ctrl Pts',(19.4168736566528,1.75741316589101,39.9388920386466));
#38156=CARTESIAN_POINT('Ctrl Pts',(19.4055024901755,1.75663251525043,39.9352588418082));
#38157=CARTESIAN_POINT('Ctrl Pts',(19.3981535163404,1.75612954736795,39.932862002616));
#38158=CARTESIAN_POINT('Ctrl Pts',(19.3517824133652,1.75296453728294,39.9174292716258));
#38159=CARTESIAN_POINT('Ctrl Pts',(19.3131680109094,1.75036775200969,39.9031909485795));
#38160=CARTESIAN_POINT('Ctrl Pts',(19.176510405672,1.74121850229434,39.8477731408484));
#38161=CARTESIAN_POINT('Ctrl Pts',(19.0814488912306,1.73492344634107,39.7997392821798));
#38162=CARTESIAN_POINT('Ctrl Pts',(18.8864954628419,1.72124977208803,39.6800745261758));
#38163=CARTESIAN_POINT('Ctrl Pts',(18.7885128372743,1.71387227086999,39.6062607038128));
#38164=CARTESIAN_POINT('Ctrl Pts',(18.6824368869388,1.70476036202682,39.5092642079091));
#38165=CARTESIAN_POINT('Ctrl Pts',(18.666925296935,1.70339704031627,39.4946002807627));
#38166=CARTESIAN_POINT('Ctrl Pts',(18.6457115427248,1.70148720166272,39.4738684530208));
#38167=CARTESIAN_POINT('Ctrl Pts',(18.6398001441199,1.70094997472317,39.4680161184109));
#38168=CARTESIAN_POINT('Ctrl Pts',(18.6296679879405,1.70002031813664,39.4578546000221));
#38169=CARTESIAN_POINT('Ctrl Pts',(18.6254292166203,1.69962868366398,39.4535634814019));
#38170=CARTESIAN_POINT('Ctrl Pts',(18.6166968051763,1.69881617665422,39.4446399071986));
#38171=CARTESIAN_POINT('Ctrl Pts',(18.6122061539806,1.69839518194164,39.4400046448047));
#38172=CARTESIAN_POINT('Ctrl Pts',(18.6033516113706,1.69755872814182,39.4307727107335));
#38173=CARTESIAN_POINT('Ctrl Pts',(18.5989869453034,1.69714331013189,39.4261768916887));
#38174=CARTESIAN_POINT('Ctrl Pts',(18.5847326670758,1.69577630940671,39.4110188019155));
#38175=CARTESIAN_POINT('Ctrl Pts',(18.574939426932,1.69482066243933,39.4003669737457));
#38176=CARTESIAN_POINT('Ctrl Pts',(18.5130762733828,1.68867606895716,39.3315420129649));
#38177=CARTESIAN_POINT('Ctrl Pts',(18.4644652030882,1.68334621637136,39.2703708585176));
#38178=CARTESIAN_POINT('Ctrl Pts',(18.3815354524825,1.67325979233464,39.1519232211013));
#38179=CARTESIAN_POINT('Ctrl Pts',(18.3462208478869,1.66854230017805,39.0954815180123));
#38180=CARTESIAN_POINT('Ctrl Pts',(18.2860631393927,1.65971710801372,38.9872677129937));
#38181=CARTESIAN_POINT('Ctrl Pts',(18.260475091997,1.65562055226872,38.9359885036831));
#38182=CARTESIAN_POINT('Ctrl Pts',(18.2345792689278,1.65110013482322,38.8777364774162));
#38183=CARTESIAN_POINT('Ctrl Pts',(18.2319817614508,1.65064200493078,38.8718133810185));
#38184=CARTESIAN_POINT('Ctrl Pts',(18.2017566778354,1.64525583950333,38.8019378179573));
#38185=CARTESIAN_POINT('Ctrl Pts',(18.17757967331,1.64039450091763,38.7365392125818));
#38186=CARTESIAN_POINT('Ctrl Pts',(18.1542737854331,1.63509422561632,38.6611790690177));
#38187=CARTESIAN_POINT('Ctrl Pts',(18.1516183030349,1.63447923158132,38.6523697287277));
#38188=CARTESIAN_POINT('Ctrl Pts',(18.147754475172,1.63356783121536,38.6392118646773));
#38189=CARTESIAN_POINT('Ctrl Pts',(18.1464982455233,1.63326877405658,38.6348777116633));
#38190=CARTESIAN_POINT('Ctrl Pts',(18.1442787528356,1.6327354971082,38.6271184574297));
#38191=CARTESIAN_POINT('Ctrl Pts',(18.1433097497119,1.63250095182484,38.62369507399));
#38192=CARTESIAN_POINT('Ctrl Pts',(18.1412288149985,1.63199349800191,38.6162649783913));
#38193=CARTESIAN_POINT('Ctrl Pts',(18.1401203671355,1.63172079098415,38.6122573554059));
#38194=CARTESIAN_POINT('Ctrl Pts',(18.1370488062906,1.63095821055714,38.6010106425219));
#38195=CARTESIAN_POINT('Ctrl Pts',(18.1351149148659,1.63046998295604,38.5937635444221));
#38196=CARTESIAN_POINT('Ctrl Pts',(18.1308728542652,1.6293800978456,38.5774862677129));
#38197=CARTESIAN_POINT('Ctrl Pts',(18.1285877430864,1.62877966754483,38.5684502059073));
#38198=CARTESIAN_POINT('Ctrl Pts',(18.0896410123783,1.61829974201645,38.4096078135587));
#38199=CARTESIAN_POINT('Ctrl Pts',(18.0710045347108,1.60929535803221,38.255936396569));
#38200=CARTESIAN_POINT('Ctrl Pts',(18.0708707257347,1.60004847844167,38.1016733417687));
#38201=CARTESIAN_POINT('Ctrl Pts',(19.3941040087494,1.44151754323334,36.2684889831927));
#38202=CARTESIAN_POINT('Ctrl Pts',(19.3295043521928,1.44595990632178,36.2898596834422));
#38203=CARTESIAN_POINT('Ctrl Pts',(19.2660284166685,1.45040226941022,36.3146550158227));
#38204=CARTESIAN_POINT('Ctrl Pts',(19.2040563963221,1.45484463249867,36.3427247407807));
#38205=CARTESIAN_POINT('Ctrl Pts',(19.1415298209384,1.45932674795946,36.3710456469537));
#38206=CARTESIAN_POINT('Ctrl Pts',(19.0805346871417,1.46380886342026,36.4026996559877));
#38207=CARTESIAN_POINT('Ctrl Pts',(19.0214381046462,1.46829097888105,36.4374840831254));
#38208=CARTESIAN_POINT('Ctrl Pts',(18.962786240726,1.47273936514943,36.4720067475649));
#38209=CARTESIAN_POINT('Ctrl Pts',(18.9060048339152,1.47718775141779,36.5096125497364));
#38210=CARTESIAN_POINT('Ctrl Pts',(18.8514234687525,1.48163613768617,36.5500598370365));
#38211=CARTESIAN_POINT('Ctrl Pts',(18.796221321606,1.48613511774317,36.5909671521716));
#38212=CARTESIAN_POINT('Ctrl Pts',(18.7432699822867,1.49063409780018,36.6347806741961));
#38213=CARTESIAN_POINT('Ctrl Pts',(18.6928740704282,1.49513307785719,36.6812102477318));
#38214=CARTESIAN_POINT('Ctrl Pts',(18.6424781585697,1.49963205791419,36.7276398212676));
#38215=CARTESIAN_POINT('Ctrl Pts',(18.5946379872075,1.5041310379712,36.7766850326004));
#38216=CARTESIAN_POINT('Ctrl Pts',(18.5496164787244,1.50863001802821,36.8280211487167));
#38217=CARTESIAN_POINT('Ctrl Pts',(18.5054073944355,1.51304781288349,36.8784308919907));
#38218=CARTESIAN_POINT('Ctrl Pts',(18.4637338189911,1.51746560773877,36.9312575117532));
#38219=CARTESIAN_POINT('Ctrl Pts',(18.4248740293338,1.52188340259406,36.9862133357627));
#38220=CARTESIAN_POINT('Ctrl Pts',(18.3860685084149,1.52629502788034,37.04109241249));
#38221=CARTESIAN_POINT('Ctrl Pts',(18.3500692719598,1.53070665316662,37.0980943932937));
#38222=CARTESIAN_POINT('Ctrl Pts',(18.3171157241828,1.5351182784529,37.1568971047086));
#38223=CARTESIAN_POINT('Ctrl Pts',(18.2841963309236,1.53952533133515,37.2156388703864));
#38224=CARTESIAN_POINT('Ctrl Pts',(18.2543166109693,1.5439323842174,37.2761772294216));
#38225=CARTESIAN_POINT('Ctrl Pts',(18.2276727115185,1.54833943709965,37.3381610804088));
#38226=CARTESIAN_POINT('Ctrl Pts',(18.2010410830137,1.55274446029748,37.4001163845053));
#38227=CARTESIAN_POINT('Ctrl Pts',(18.1776425273966,1.5571494834953,37.4635154036111));
#38228=CARTESIAN_POINT('Ctrl Pts',(18.157626462877,1.56155450669312,37.5279839979432));
#38229=CARTESIAN_POINT('Ctrl Pts',(18.1376167710586,1.56595812742263,37.5924320668078));
#38230=CARTESIAN_POINT('Ctrl Pts',(18.1209875777404,1.57036174815214,37.6579485535264));
#38231=CARTESIAN_POINT('Ctrl Pts',(18.1078387655014,1.57476536888165,37.7241430863206));
#38232=CARTESIAN_POINT('Ctrl Pts',(18.0946818547531,1.57917170185332,37.7903783891114));
#38233=CARTESIAN_POINT('Ctrl Pts',(18.0850097061681,1.58357803482498,37.8572920782553));
#38234=CARTESIAN_POINT('Ctrl Pts',(18.0788710086126,1.58798436779665,37.9244837461924));
#38235=CARTESIAN_POINT('Ctrl Pts',(18.0734853254718,1.59185018998173,37.9834332269135));
#38236=CARTESIAN_POINT('Ctrl Pts',(18.0708186250899,1.59571601216681,38.0425963204681));
#38237=CARTESIAN_POINT('Ctrl Pts',(18.0708707501997,1.59958183435189,38.1017013127004));
#38238=CARTESIAN_POINT('Ctrl Pts',(19.3941039987112,1.2718084690693,36.2684889865135));
#38239=CARTESIAN_POINT('Ctrl Pts',(19.3729704333272,1.27317206199249,36.2754803410098));
#38240=CARTESIAN_POINT('Ctrl Pts',(19.3519547771375,1.27452534683923,36.2828385068952));
#38241=CARTESIAN_POINT('Ctrl Pts',(19.2353762315221,1.28204040096756,36.325936541027));
#38242=CARTESIAN_POINT('Ctrl Pts',(19.1426419244413,1.28805758975417,36.3688476111492));
#38243=CARTESIAN_POINT('Ctrl Pts',(18.9960606939578,1.29819804784758,36.4513555214064));
#38244=CARTESIAN_POINT('Ctrl Pts',(18.9400997606449,1.30223503154551,36.4867631523017));
#38245=CARTESIAN_POINT('Ctrl Pts',(18.8544898325454,1.3087833623047,36.5473102870164));
#38246=CARTESIAN_POINT('Ctrl Pts',(18.8235886346127,1.31122973923878,36.5705900276741));
#38247=CARTESIAN_POINT('Ctrl Pts',(18.7846392504342,1.31443359811905,36.6018120440878));
#38248=CARTESIAN_POINT('Ctrl Pts',(18.7759306338103,1.31515798437925,36.6089188214961));
#38249=CARTESIAN_POINT('Ctrl Pts',(18.7619145414513,1.31633723986449,36.6205623717716));
#38250=CARTESIAN_POINT('Ctrl Pts',(18.7565686311313,1.3167902320251,36.6250526357596));
#38251=CARTESIAN_POINT('Ctrl Pts',(18.7463623132792,1.31766132621961,36.6337202925881));
#38252=CARTESIAN_POINT('Ctrl Pts',(18.7414981096668,1.31807923731729,36.63789308862));
#38253=CARTESIAN_POINT('Ctrl Pts',(18.7304423972041,1.31903547385862,36.6474733651038));
#38254=CARTESIAN_POINT('Ctrl Pts',(18.7242645119804,1.31957443202707,36.6528963088349));
#38255=CARTESIAN_POINT('Ctrl Pts',(18.7080055045157,1.32100527287077,36.6673534892347));
#38256=CARTESIAN_POINT('Ctrl Pts',(18.6979846364914,1.32189992539169,36.6764545042204));
#38257=CARTESIAN_POINT('Ctrl Pts',(18.6198218405995,1.3289811239902,36.7489581842059));
#38258=CARTESIAN_POINT('Ctrl Pts',(18.5562640631192,1.33537206128373,36.8171018831818));
#38259=CARTESIAN_POINT('Ctrl Pts',(18.3977500555834,1.35312131761996,37.013812597373));
#38260=CARTESIAN_POINT('Ctrl Pts',(18.3134311631152,1.36473915158736,37.1500045888991));
#38261=CARTESIAN_POINT('Ctrl Pts',(18.2347590313027,1.37772452529724,37.3213435401196));
#38262=CARTESIAN_POINT('Ctrl Pts',(18.2232659692866,1.37969526278953,37.3479375242969));
#38263=CARTESIAN_POINT('Ctrl Pts',(18.2097614844733,1.38209842981782,37.3812253725997));
#38264=CARTESIAN_POINT('Ctrl Pts',(18.2071822776167,1.38256169758878,37.3876829881169));
#38265=CARTESIAN_POINT('Ctrl Pts',(18.2031605988728,1.38329077114152,37.3979123789754));
#38266=CARTESIAN_POINT('Ctrl Pts',(18.2016949873493,1.38355791769078,37.4016749014544));
#38267=CARTESIAN_POINT('Ctrl Pts',(18.1989536603523,1.38406031978542,37.4087783078228));
#38268=CARTESIAN_POINT('Ctrl Pts',(18.1976754361683,1.38429571638796,37.4121180972454));
#38269=CARTESIAN_POINT('Ctrl Pts',(18.1947676312976,1.38483386531823,37.4197794604327));
#38270=CARTESIAN_POINT('Ctrl Pts',(18.1931442783298,1.38513624670678,37.424103343979));
#38271=CARTESIAN_POINT('Ctrl Pts',(18.1888590532329,1.38593979819903,37.4356430328213));
#38272=CARTESIAN_POINT('Ctrl Pts',(18.1862247447007,1.38643938902646,37.4428690869163));
#38273=CARTESIAN_POINT('Ctrl Pts',(18.1672595705472,1.39007920439081,37.4958745935455));
#38274=CARTESIAN_POINT('Ctrl Pts',(18.1526192543012,1.39312825434638,37.5422453251091));
#38275=CARTESIAN_POINT('Ctrl Pts',(18.1330725053582,1.39767509173209,37.6134209624401));
#38276=CARTESIAN_POINT('Ctrl Pts',(18.1268763229125,1.39921214922491,37.6378472140587));
#38277=CARTESIAN_POINT('Ctrl Pts',(18.0878297021189,1.40964436688018,37.8054898616816));
#38278=CARTESIAN_POINT('Ctrl Pts',(18.0709568775046,1.41821775313881,37.9519275109852));
#38279=CARTESIAN_POINT('Ctrl Pts',(18.0708347172606,1.43096131211979,38.1593364460134));
#38280=CARTESIAN_POINT('Ctrl Pts',(18.0736425407378,1.43474043564055,38.2197719057908));
#38281=CARTESIAN_POINT('Ctrl Pts',(18.0804245816936,1.43939132766768,38.2921521264353));
#38282=CARTESIAN_POINT('Ctrl Pts',(18.0816817258341,1.44017748412289,38.3043213502303));
#38283=CARTESIAN_POINT('Ctrl Pts',(18.083942616572,1.44147814806944,38.3243419198796));
#38284=CARTESIAN_POINT('Ctrl Pts',(18.0848791009267,1.4419905551029,38.3322006297621));
#38285=CARTESIAN_POINT('Ctrl Pts',(18.0866550158689,1.44291731449753,38.3463614160093));
#38286=CARTESIAN_POINT('Ctrl Pts',(18.0874772971379,1.44333112461121,38.3526655596277));
#38287=CARTESIAN_POINT('Ctrl Pts',(18.0893016298007,1.44421780805564,38.3661326864701));
#38288=CARTESIAN_POINT('Ctrl Pts',(18.0903128304379,1.4446909623743,38.373294311514));
#38289=CARTESIAN_POINT('Ctrl Pts',(18.0931640726627,1.44597748389273,38.3926987786005));
#38290=CARTESIAN_POINT('Ctrl Pts',(18.0950817091464,1.44679327318482,38.4049296998816));
#38291=CARTESIAN_POINT('Ctrl Pts',(18.1056612585528,1.45105329528453,38.468408217996));
#38292=CARTESIAN_POINT('Ctrl Pts',(18.1162731819594,1.45455833356645,38.5193045268177));
#38293=CARTESIAN_POINT('Ctrl Pts',(18.1766648431342,1.47157002523195,38.7598744639977));
#38294=CARTESIAN_POINT('Ctrl Pts',(18.2531010698094,1.48591420585538,38.9416098130526));
#38295=CARTESIAN_POINT('Ctrl Pts',(18.3747793559549,1.50206009194551,39.1399746432878));
#38296=CARTESIAN_POINT('Ctrl Pts',(18.3948588477879,1.50457186717874,39.1707061733587));
#38297=CARTESIAN_POINT('Ctrl Pts',(18.4198515539288,1.50750738948235,39.2066723738999));
#38298=CARTESIAN_POINT('Ctrl Pts',(18.4239307876661,1.50798078825759,39.2124741329671));
#38299=CARTESIAN_POINT('Ctrl Pts',(18.4306436305957,1.5087503660928,39.2219105517576));
#38300=CARTESIAN_POINT('Ctrl Pts',(18.433258047894,1.50904778918022,39.2255586865455));
#38301=CARTESIAN_POINT('Ctrl Pts',(18.4379666563443,1.50957930106087,39.2320808430067));
#38302=CARTESIAN_POINT('Ctrl Pts',(18.4400560748509,1.50981370627135,39.2349582163485));
#38303=CARTESIAN_POINT('Ctrl Pts',(18.4446165487979,1.51032218540873,39.2412021360998));
#38304=CARTESIAN_POINT('Ctrl Pts',(18.4470905770178,1.5105960506815,39.2445664334331));
#38305=CARTESIAN_POINT('Ctrl Pts',(18.4540876844341,1.51136513100577,39.2540169708251));
#38306=CARTESIAN_POINT('Ctrl Pts',(18.4586358136344,1.51185865496014,39.260084697769));
#38307=CARTESIAN_POINT('Ctrl Pts',(18.4866157817758,1.51485723981956,39.2969581401084));
#38308=CARTESIAN_POINT('Ctrl Pts',(18.5109364179864,1.51730464163332,39.327082198269));
#38309=CARTESIAN_POINT('Ctrl Pts',(18.6518033981245,1.53075474392431,39.4912011253199));
#38310=CARTESIAN_POINT('Ctrl Pts',(18.7855144180612,1.5409613047013,39.6093414955046));
#38311=CARTESIAN_POINT('Ctrl Pts',(18.9885418136757,1.55587979756541,39.7440364465344));
#38312=CARTESIAN_POINT('Ctrl Pts',(19.0454031862377,1.55999537934415,39.7776909691126));
#38313=CARTESIAN_POINT('Ctrl Pts',(19.1149890050844,1.56502029795779,39.8141924164311));
#38314=CARTESIAN_POINT('Ctrl Pts',(19.1261607057953,1.56582660525961,39.8199142355381));
#38315=CARTESIAN_POINT('Ctrl Pts',(19.1445540069957,1.56715382882963,39.8291092818812));
#38316=CARTESIAN_POINT('Ctrl Pts',(19.1517429361519,1.5676724934482,39.8326473115085));
#38317=CARTESIAN_POINT('Ctrl Pts',(19.1646840285857,1.56860612843992,39.8389164237411));
#38318=CARTESIAN_POINT('Ctrl Pts',(19.1704280988774,1.5690205219728,39.8416640204426));
#38319=CARTESIAN_POINT('Ctrl Pts',(19.1826694018392,1.56990367028045,39.8474451825756));
#38320=CARTESIAN_POINT('Ctrl Pts',(19.1891701412489,1.57037268138688,39.850471053923));
#38321=CARTESIAN_POINT('Ctrl Pts',(19.2066807131758,1.57163614860674,39.8585031543281));
#38322=CARTESIAN_POINT('Ctrl Pts',(19.2177208606355,1.57243288004147,39.8634421372659));
#38323=CARTESIAN_POINT('Ctrl Pts',(19.272992460545,1.57642294459216,39.8875475803889));
#38324=CARTESIAN_POINT('Ctrl Pts',(19.3178815220938,1.57966822717996,39.9051537327229));
#38325=CARTESIAN_POINT('Ctrl Pts',(19.4509857541633,1.58931318161689,39.951685371188));
#38326=CARTESIAN_POINT('Ctrl Pts',(19.5406777150738,1.59584658676708,39.9759463591679));
#38327=CARTESIAN_POINT('Ctrl Pts',(19.7636805904726,1.61201926405306,40.0193117595022));
#38328=CARTESIAN_POINT('Ctrl Pts',(19.8979328690707,1.62170794521142,40.0311116951321));
#38329=CARTESIAN_POINT('Ctrl Pts',(20.0464083560802,1.63176653625457,40.0286231078209));
#38330=CARTESIAN_POINT('Ctrl Pts',(20.0604847424205,1.63271333120259,40.0282329869045));
#38331=CARTESIAN_POINT('Ctrl Pts',(20.0800763341537,1.634020442352,40.0274752543962));
#38332=CARTESIAN_POINT('Ctrl Pts',(20.0855957220287,1.63438750752973,40.0272380366286));
#38333=CARTESIAN_POINT('Ctrl Pts',(20.0944628801919,1.63497524213699,40.0268187669263));
#38334=CARTESIAN_POINT('Ctrl Pts',(20.0978112758904,1.63519672885188,40.0266516942747));
#38335=CARTESIAN_POINT('Ctrl Pts',(20.104822799378,1.63565954981811,40.0262835191699));
#38336=CARTESIAN_POINT('Ctrl Pts',(20.1084858088695,1.63590078209794,40.02608069537));
#38337=CARTESIAN_POINT('Ctrl Pts',(20.1173962873301,1.6364862822048,40.025561815158));
#38338=CARTESIAN_POINT('Ctrl Pts',(20.1226431370371,1.63682994215671,40.0252347531679));
#38339=CARTESIAN_POINT('Ctrl Pts',(20.141278392357,1.63804679783516,40.0239966343775));
#38340=CARTESIAN_POINT('Ctrl Pts',(20.1546589311806,1.63891369879547,40.0229673092837));
#38341=CARTESIAN_POINT('Ctrl Pts',(20.2369541191611,1.64420938180913,40.0157720160734));
#38342=CARTESIAN_POINT('Ctrl Pts',(20.305514124898,1.64846607075289,40.006041171184));
#38343=CARTESIAN_POINT('Ctrl Pts',(20.5095452254164,1.66105352068333,39.9657868197054));
#38344=CARTESIAN_POINT('Ctrl Pts',(20.6423830643676,1.66916889523237,39.9243195392538));
#38345=CARTESIAN_POINT('Ctrl Pts',(20.8296603340419,1.68167847969386,39.8428404238884));
#38346=CARTESIAN_POINT('Ctrl Pts',(20.8883211370104,1.68575988078262,39.813684092192));
#38347=CARTESIAN_POINT('Ctrl Pts',(20.9562984762563,1.69074694824613,39.7754678769476));
#38348=CARTESIAN_POINT('Ctrl Pts',(20.9671544287993,1.69155143618401,39.769224874407));
#38349=CARTESIAN_POINT('Ctrl Pts',(20.9848474163789,1.69287625110042,39.7588195132976));
#38350=CARTESIAN_POINT('Ctrl Pts',(20.9917208030249,1.69339434012079,39.754719449609));
#38351=CARTESIAN_POINT('Ctrl Pts',(21.0040153548731,1.69432732218336,39.7472814733811));
#38352=CARTESIAN_POINT('Ctrl Pts',(21.0094459160056,1.69474164146732,39.7439592532683));
#38353=CARTESIAN_POINT('Ctrl Pts',(21.0209621487264,1.69562504248094,39.7368354634614));
#38354=CARTESIAN_POINT('Ctrl Pts',(21.027043239418,1.69609438263717,39.7330267069481));
#38355=CARTESIAN_POINT('Ctrl Pts',(21.0433368396896,1.6973597401718,39.7226945629928));
#38356=CARTESIAN_POINT('Ctrl Pts',(21.0535092297617,1.6981580450261,39.7161088135706));
#38357=CARTESIAN_POINT('Ctrl Pts',(21.1040881519733,1.70216985736208,39.6826828418386));
#38358=CARTESIAN_POINT('Ctrl Pts',(21.1435310710896,1.70543600372661,39.6544232382592));
#38359=CARTESIAN_POINT('Ctrl Pts',(21.3120581448833,1.72002452814741,39.5237910331012));
#38360=CARTESIAN_POINT('Ctrl Pts',(21.4287772880356,1.73191637436645,39.4066204687615));
#38361=CARTESIAN_POINT('Ctrl Pts',(21.5716378434624,1.74849486570901,39.2208697251584));
#38362=CARTESIAN_POINT('Ctrl Pts',(21.6110865878945,1.75335554094964,39.1633892644592));
#38363=CARTESIAN_POINT('Ctrl Pts',(21.6521305759144,1.75865517169651,39.0960380317368));
#38364=CARTESIAN_POINT('Ctrl Pts',(21.6568620949549,1.75927014380579,39.0881473610174));
#38365=CARTESIAN_POINT('Ctrl Pts',(21.6638298888144,1.76018151390984,39.0763365296709));
#38366=CARTESIAN_POINT('Ctrl Pts',(21.6661090680606,1.76048056260083,39.0724420252314));
#38367=CARTESIAN_POINT('Ctrl Pts',(21.6701608243531,1.76101382713724,39.0654626019151));
#38368=CARTESIAN_POINT('Ctrl Pts',(21.671938545601,1.7612483684443,39.0623807538233));
#38369=CARTESIAN_POINT('Ctrl Pts',(21.6757754234894,1.76175581752478,39.0556864423114));
#38370=CARTESIAN_POINT('Ctrl Pts',(21.6778314252505,1.76202852375884,39.0520722426568));
#38371=CARTESIAN_POINT('Ctrl Pts',(21.6835633381278,1.76279110362143,39.0419200075224));
#38372=CARTESIAN_POINT('Ctrl Pts',(21.6872128780378,1.76327933142902,39.0353670524104));
#38373=CARTESIAN_POINT('Ctrl Pts',(21.7087480064532,1.76617747663021,38.9961633528117));
#38374=CARTESIAN_POINT('Ctrl Pts',(21.7257250011852,1.76853412264443,38.9630192153938));
#38375=CARTESIAN_POINT('Ctrl Pts',(21.8107461283317,1.7808494956279,38.7844759460339));
#38376=CARTESIAN_POINT('Ctrl Pts',(21.8614067773933,1.79013980882812,38.6314921095146));
#38377=CARTESIAN_POINT('Ctrl Pts',(21.9086809738058,1.80493249588095,38.3922650207015));
#38378=CARTESIAN_POINT('Ctrl Pts',(21.9195182800998,1.8100807565815,38.3095920990348));
#38379=CARTESIAN_POINT('Ctrl Pts',(21.9258490491677,1.81624924577941,38.2132434340396));
#38380=CARTESIAN_POINT('Ctrl Pts',(21.9265824110817,1.81710103211466,38.1999941734814));
#38381=CARTESIAN_POINT('Ctrl Pts',(21.927549034963,1.81848793774505,38.17851750765));
#38382=CARTESIAN_POINT('Ctrl Pts',(21.9278664389684,1.81902044523461,38.1702941764443));
#38383=CARTESIAN_POINT('Ctrl Pts',(21.9283368531232,1.81996943415594,38.1556811210317));
#38384=CARTESIAN_POINT('Ctrl Pts',(21.9285107436,1.82038526100485,38.1492921549011));
#38385=CARTESIAN_POINT('Ctrl Pts',(21.9288095661928,1.82126155981125,38.1358587891713));
#38386=CARTESIAN_POINT('Ctrl Pts',(21.9289276623608,1.82172223791559,38.1288143465335));
#38387=CARTESIAN_POINT('Ctrl Pts',(21.9291372827702,1.82294004599769,38.110239762459));
#38388=CARTESIAN_POINT('Ctrl Pts',(21.9291640243603,1.82369917420297,38.0987093145578));
#38389=CARTESIAN_POINT('Ctrl Pts',(21.9288104507416,1.82721689264437,38.0455073419514));
#38390=CARTESIAN_POINT('Ctrl Pts',(21.9271833009245,1.8300137567064,38.0038580460169));
#38391=CARTESIAN_POINT('Ctrl Pts',(21.9122464158868,1.84425778675632,37.7951362214163));
#38392=CARTESIAN_POINT('Ctrl Pts',(21.8785525233989,1.8563314950612,37.6302657114153));
#38393=CARTESIAN_POINT('Ctrl Pts',(21.821276834621,1.86879920534607,37.4639470701502));
#38394=CARTESIAN_POINT('Ctrl Pts',(21.8184995227837,1.86939171258202,37.456049593733));
#38395=CARTESIAN_POINT('Ctrl Pts',(21.8080171955679,1.87158364067586,37.4268510796458));
#38396=CARTESIAN_POINT('Ctrl Pts',(21.7999883944055,1.8731765007669,37.4056675955477));
#38397=CARTESIAN_POINT('Ctrl Pts',(21.7748703005412,1.87790584083554,37.3427613097129));
#38398=CARTESIAN_POINT('Ctrl Pts',(21.7566883111422,1.8810079388215,37.3014876693979));
#38399=CARTESIAN_POINT('Ctrl Pts',(21.733798110862,1.88453847053896,37.254102001857));
#38400=CARTESIAN_POINT('Ctrl Pts',(21.7304814299476,1.88504170944507,37.2473375007421));
#38401=CARTESIAN_POINT('Ctrl Pts',(21.725088156308,1.88584661694057,37.2364988029708));
#38402=CARTESIAN_POINT('Ctrl Pts',(21.7230365978252,1.88614975920024,37.2324123399177));
#38403=CARTESIAN_POINT('Ctrl Pts',(21.7193570866823,1.88668802719513,37.2251477178879));
#38404=CARTESIAN_POINT('Ctrl Pts',(21.7177348193876,1.8869234989278,37.2219667443105));
#38405=CARTESIAN_POINT('Ctrl Pts',(21.7142461608097,1.88742593676269,37.2151727890593));
#38406=CARTESIAN_POINT('Ctrl Pts',(21.7123771785754,1.8876927382315,37.2115612051906));
#38407=CARTESIAN_POINT('Ctrl Pts',(21.7072219181284,1.88842227965474,37.2016759847729));
#38408=CARTESIAN_POINT('Ctrl Pts',(21.7039124500888,1.88888359611933,37.1954144151575));
#38409=CARTESIAN_POINT('Ctrl Pts',(21.6860758786098,1.89133359845821,37.1621125385456));
#38410=CARTESIAN_POINT('Ctrl Pts',(21.6709384949103,1.89328638063969,37.1354018646076));
#38411=CARTESIAN_POINT('Ctrl Pts',(21.5722060715657,1.90533758476987,36.9704885557513));
#38412=CARTESIAN_POINT('Ctrl Pts',(21.47216148179,1.91468603520564,36.8428680513414));
#38413=CARTESIAN_POINT('Ctrl Pts',(21.293926270049,1.92986041538412,36.6663791007295));
#38414=CARTESIAN_POINT('Ctrl Pts',(21.2262067302,1.93536240026429,36.6080455726267));
#38415=CARTESIAN_POINT('Ctrl Pts',(21.1439300959397,1.94192232284586,36.5465692280945));
#38416=CARTESIAN_POINT('Ctrl Pts',(21.1330789265493,1.94278499662619,36.5386366985708));
#38417=CARTESIAN_POINT('Ctrl Pts',(21.1154822977052,1.94418043901437,36.5260530781324));
#38418=CARTESIAN_POINT('Ctrl Pts',(21.10878843039,1.94471047149803,36.521330344062));
#38419=CARTESIAN_POINT('Ctrl Pts',(21.0968080372016,1.9456577817736,36.5129915857391));
#38420=CARTESIAN_POINT('Ctrl Pts',(21.091533170505,1.94607442399018,36.5093589614733));
#38421=CARTESIAN_POINT('Ctrl Pts',(21.0804594993875,1.94694820570668,36.5018139158502));
#38422=CARTESIAN_POINT('Ctrl Pts',(21.0746573184269,1.9474055302054,36.4979066396822));
#38423=CARTESIAN_POINT('Ctrl Pts',(21.0594248996098,1.94860490476069,36.4877688793451));
#38424=CARTESIAN_POINT('Ctrl Pts',(21.0499610422031,1.94934884498679,36.4815896364051));
#38425=CARTESIAN_POINT('Ctrl Pts',(21.0073452738725,1.95269381332018,36.4542956134918));
#38426=CARTESIAN_POINT('Ctrl Pts',(20.9736090501128,1.95532866914261,36.4341151107134));
#38427=CARTESIAN_POINT('Ctrl Pts',(20.7960748347889,1.96913864233127,36.3351520622656));
#38428=CARTESIAN_POINT('Ctrl Pts',(20.643292403629,1.98091936690152,36.2739166757123));
#38429=CARTESIAN_POINT('Ctrl Pts',(20.4062570484523,1.99831113208683,36.2123937851366));
#38430=CARTESIAN_POINT('Ctrl Pts',(20.3266503599643,2.00399593007626,36.1970011097992));
#38431=CARTESIAN_POINT('Ctrl Pts',(20.2370472690983,2.01006770961643,36.1854665745116));
#38432=CARTESIAN_POINT('Ctrl Pts',(20.2277827835748,2.0106916055411,36.1843422390202));
#38433=CARTESIAN_POINT('Ctrl Pts',(20.214000918111,2.01161357294287,36.1827710719501));
#38434=CARTESIAN_POINT('Ctrl Pts',(20.2094897006305,2.01191438407465,36.1822729021368));
#38435=CARTESIAN_POINT('Ctrl Pts',(20.2014369117707,2.01244955790994,36.1814123943049));
#38436=CARTESIAN_POINT('Ctrl Pts',(20.1978960652365,2.01268425583637,36.1810439353046));
#38437=CARTESIAN_POINT('Ctrl Pts',(20.1902359565547,2.01319064215454,36.1802682554683));
#38438=CARTESIAN_POINT('Ctrl Pts',(20.1861164068655,2.01346213648274,36.1798644907141));
#38439=CARTESIAN_POINT('Ctrl Pts',(20.1746146559484,2.01421789236132,36.178774545891));
#38440=CARTESIAN_POINT('Ctrl Pts',(20.167229653574,2.01470055524974,36.178117649049));
#38441=CARTESIAN_POINT('Ctrl Pts',(20.1242160166671,2.0174976912525,36.1745413939392));
#38442=CARTESIAN_POINT('Ctrl Pts',(20.0885128961982,2.01976312541157,36.1725700209739));
#38443=CARTESIAN_POINT('Ctrl Pts',(19.9709981319986,2.02709505233458,36.1693541033206));
#38444=CARTESIAN_POINT('Ctrl Pts',(19.8891566211293,2.03200534347251,36.1723198731452));
#38445=CARTESIAN_POINT('Ctrl Pts',(19.6670110749501,2.04535258710982,36.1945694437807));
#38446=CARTESIAN_POINT('Ctrl Pts',(19.5283038416974,2.05373968933419,36.2240933229587));
#38447=CARTESIAN_POINT('Ctrl Pts',(19.3941040086996,2.0626282966298,36.2684889832092));
#38448=CARTESIAN_POINT('Origin',(20.,-1.3495818343519,38.1));
#38449=CARTESIAN_POINT('',(19.3941040093468,3.02765621357216,36.2684889829951));
#38450=CARTESIAN_POINT('',(19.3941039244954,2.85753017062829,36.2684890110654));
#38451=CARTESIAN_POINT('',(19.3941040087494,-1.3495818343519,36.2684889831927));
#38452=CARTESIAN_POINT('Ctrl Pts',(19.3941040093468,3.02765621357216,36.2684889829951));
#38453=CARTESIAN_POINT('Ctrl Pts',(19.4103477405592,3.0264616496969,36.2631152716041));
#38454=CARTESIAN_POINT('Ctrl Pts',(19.4266683458038,3.02527319948087,36.2579558773622));
#38455=CARTESIAN_POINT('Ctrl Pts',(19.4719784478927,3.02200993305801,36.2442931254959));
#38456=CARTESIAN_POINT('Ctrl Pts',(19.5010979961917,3.01995323104104,36.2362532883861));
#38457=CARTESIAN_POINT('Ctrl Pts',(19.5372307457135,3.01746056567672,36.2271847857557));
#38458=CARTESIAN_POINT('Ctrl Pts',(19.5440747136245,3.01699103180448,36.2255069094698));
#38459=CARTESIAN_POINT('Ctrl Pts',(19.5548749377827,3.01625434343587,36.2229217629558));
#38460=CARTESIAN_POINT('Ctrl Pts',(19.5588250418642,3.01598580184797,36.2219894339839));
#38461=CARTESIAN_POINT('Ctrl Pts',(19.5662574535603,3.01548224395285,36.2202599324133));
#38462=CARTESIAN_POINT('Ctrl Pts',(19.5697389925866,3.01524707815708,36.2194599754244));
#38463=CARTESIAN_POINT('Ctrl Pts',(19.5776944067483,3.01471132296863,36.2176553007359));
#38464=CARTESIAN_POINT('Ctrl Pts',(19.5821696524334,3.01441109248322,36.2166568600859));
#38465=CARTESIAN_POINT('Ctrl Pts',(19.5940492064252,3.01361708429234,36.2140509241906));
#38466=CARTESIAN_POINT('Ctrl Pts',(19.6014595878548,3.01312482665771,36.2124710577546));
#38467=CARTESIAN_POINT('Ctrl Pts',(19.653836902804,3.00966568901347,36.2016266166513));
#38468=CARTESIAN_POINT('Ctrl Pts',(19.6991167777806,3.00678006171815,36.1939253799233));
#38469=CARTESIAN_POINT('Ctrl Pts',(19.7740206317822,3.00211433489331,36.1839219851429));
#38470=CARTESIAN_POINT('Ctrl Pts',(19.8034966126408,3.00030546784903,36.1806750717983));
#38471=CARTESIAN_POINT('Ctrl Pts',(19.9989030140084,2.98842734893121,36.1636992453304));
#38472=CARTESIAN_POINT('Ctrl Pts',(20.1659289182774,2.97874559193828,36.1708213566674));
#38473=CARTESIAN_POINT('Ctrl Pts',(20.3723125048065,2.965708013295,36.2066503281714));
#38474=CARTESIAN_POINT('Ctrl Pts',(20.4143959192395,2.96299624351154,36.2154137948));
#38475=CARTESIAN_POINT('Ctrl Pts',(20.4674693629423,2.95949257503285,36.2283294400888));
#38476=CARTESIAN_POINT('Ctrl Pts',(20.4787640548026,2.95874209845827,36.2311866705605));
#38477=CARTESIAN_POINT('Ctrl Pts',(20.4968720901933,2.95753080157063,36.2359424104362));
#38478=CARTESIAN_POINT('Ctrl Pts',(20.5037021979015,2.95707205373753,36.2377764192104));
#38479=CARTESIAN_POINT('Ctrl Pts',(20.516679695697,2.95619679486494,36.2413377332806));
#38480=CARTESIAN_POINT('Ctrl Pts',(20.5228289085563,2.95578051274444,36.2430580891123));
#38481=CARTESIAN_POINT('Ctrl Pts',(20.5368356559794,2.954828700196,36.2470518237536));
#38482=CARTESIAN_POINT('Ctrl Pts',(20.5446874573377,2.95429254584453,36.2493447009952));
#38483=CARTESIAN_POINT('Ctrl Pts',(20.5650793606633,2.95289322286747,36.2554405437587));
#38484=CARTESIAN_POINT('Ctrl Pts',(20.5775955461457,2.95202754494522,36.2593214180105));
#38485=CARTESIAN_POINT('Ctrl Pts',(20.6650349588565,2.94593100705766,36.2874132595377));
#38486=CARTESIAN_POINT('Ctrl Pts',(20.7384441290456,2.94055573692867,36.316060667094));
#38487=CARTESIAN_POINT('Ctrl Pts',(20.959625679844,2.92355341205621,36.4183701467329));
#38488=CARTESIAN_POINT('Ctrl Pts',(21.0998415565625,2.91153862120623,36.5065439597648));
#38489=CARTESIAN_POINT('Ctrl Pts',(21.2561679375433,2.89747849979775,36.6354176235858));
#38490=CARTESIAN_POINT('Ctrl Pts',(21.2845075876979,2.8949023595772,36.6602082985367));
#38491=CARTESIAN_POINT('Ctrl Pts',(21.317621354433,2.89187685816499,36.6909318208766));
#38492=CARTESIAN_POINT('Ctrl Pts',(21.3231070735429,2.89137512380437,36.6960816107763));
#38493=CARTESIAN_POINT('Ctrl Pts',(21.3315811805419,2.89059944840638,36.7041305761382));
#38494=CARTESIAN_POINT('Ctrl Pts',(21.3345904750762,2.89032387101778,36.7070074826135));
#38495=CARTESIAN_POINT('Ctrl Pts',(21.3401538891474,2.8898142117348,36.7123607221437));
#38496=CARTESIAN_POINT('Ctrl Pts',(21.342710450588,2.88957993808304,36.7148343570985));
#38497=CARTESIAN_POINT('Ctrl Pts',(21.3484895604084,2.88905018827784,36.7204570457118));
#38498=CARTESIAN_POINT('Ctrl Pts',(21.3517079221277,2.888755044586,36.7236103198832));
#38499=CARTESIAN_POINT('Ctrl Pts',(21.3614399995793,2.8878620502191,36.7332126348524));
#38500=CARTESIAN_POINT('Ctrl Pts',(21.3679189430422,2.88726686849352,36.7396969649001));
#38501=CARTESIAN_POINT('Ctrl Pts',(21.4511441669796,2.87960847912856,36.8241873115798));
#38502=CARTESIAN_POINT('Ctrl Pts',(21.5211766932684,2.87301418110241,36.908552847676));
#38503=CARTESIAN_POINT('Ctrl Pts',(21.631305782772,2.86147457275045,37.0668789037245));
#38504=CARTESIAN_POINT('Ctrl Pts',(21.6744379299934,2.85652318184319,37.1383582028391));
#38505=CARTESIAN_POINT('Ctrl Pts',(21.7489218396207,2.84671179155065,37.282090680764));
#38506=CARTESIAN_POINT('Ctrl Pts',(21.780744836716,2.8418729276214,37.3539109035469));
#38507=CARTESIAN_POINT('Ctrl Pts',(21.8147692315096,2.83566884880557,37.4453850083448));
#38508=CARTESIAN_POINT('Ctrl Pts',(21.8211680497288,2.83444510166513,37.4634035470905));
#38509=CARTESIAN_POINT('Ctrl Pts',(21.8300528389004,2.83265861714853,37.4896533707494));
#38510=CARTESIAN_POINT('Ctrl Pts',(21.832753415039,2.83210290710937,37.4978112283146));
#38511=CARTESIAN_POINT('Ctrl Pts',(21.8373834170219,2.83112738288449,37.5121171426652));
#38512=CARTESIAN_POINT('Ctrl Pts',(21.8393367259354,2.83070835478478,37.5182573747399));
#38513=CARTESIAN_POINT('Ctrl Pts',(21.8430641465167,2.82989397374695,37.5301809910386));
#38514=CARTESIAN_POINT('Ctrl Pts',(21.8448418907531,2.82949874463527,37.5359631679815));
#38515=CARTESIAN_POINT('Ctrl Pts',(21.8490191418076,2.82855348514106,37.5497808646332));
#38516=CARTESIAN_POINT('Ctrl Pts',(21.8513934890125,2.82800264663377,37.557823802819));
#38517=CARTESIAN_POINT('Ctrl Pts',(21.8597413942069,2.82601600279909,37.5867961187604));
#38518=CARTESIAN_POINT('Ctrl Pts',(21.8654129075072,2.82457053394606,37.6078101017201));
#38519=CARTESIAN_POINT('Ctrl Pts',(21.9079435708128,2.8129124481545,37.7767037264029));
#38520=CARTESIAN_POINT('Ctrl Pts',(21.9275085337689,2.80213283157299,37.9283544080817));
#38521=CARTESIAN_POINT('Ctrl Pts',(21.9298517307292,2.78542764369942,38.1624490844719));
#38522=CARTESIAN_POINT('Ctrl Pts',(21.9254716135726,2.77959722016018,38.2441815852222));
#38523=CARTESIAN_POINT('Ctrl Pts',(21.9117422408348,2.77145494660324,38.3608855220005));
#38524=CARTESIAN_POINT('Ctrl Pts',(21.9065811577922,2.76901222884761,38.3962572195072));
#38525=CARTESIAN_POINT('Ctrl Pts',(21.8991661056456,2.7661224196174,38.4387707436596));
#38526=CARTESIAN_POINT('Ctrl Pts',(21.8978502273035,2.76562815207771,38.4460665148581));
#38527=CARTESIAN_POINT('Ctrl Pts',(21.8957341509273,2.76486150372461,38.4574237232509));
#38528=CARTESIAN_POINT('Ctrl Pts',(21.8949629006628,2.76458754589498,38.4614903800184));
#38529=CARTESIAN_POINT('Ctrl Pts',(21.8935039703952,2.76407934637782,38.4690500568951));
#38530=CARTESIAN_POINT('Ctrl Pts',(21.8928197166378,2.76384492253005,38.4725436229835));
#38531=CARTESIAN_POINT('Ctrl Pts',(21.8912410664991,2.76331287028463,38.4804870370712));
#38532=CARTESIAN_POINT('Ctrl Pts',(21.890340635975,2.76301558648448,38.484935628402));
#38533=CARTESIAN_POINT('Ctrl Pts',(21.8875406903118,2.7621096323015,38.4985220262328));
#38534=CARTESIAN_POINT('Ctrl Pts',(21.8855905217025,2.76150374571872,38.507649427731));
#38535=CARTESIAN_POINT('Ctrl Pts',(21.8660557509568,2.75566646922722,38.5959375671419));
#38536=CARTESIAN_POINT('Ctrl Pts',(21.8435601883917,2.75069028718033,38.6739402958565));
#38537=CARTESIAN_POINT('Ctrl Pts',(21.7609757076507,2.73590353698134,38.9045883064166));
#38538=CARTESIAN_POINT('Ctrl Pts',(21.686304973013,2.72634491017049,39.0511953319656));
#38539=CARTESIAN_POINT('Ctrl Pts',(21.5718828412208,2.71366463210328,39.2190482510695));
#38540=CARTESIAN_POINT('Ctrl Pts',(21.548779634438,2.7111819205209,39.2508110009356));
#38541=CARTESIAN_POINT('Ctrl Pts',(21.5178024014421,2.7079369139024,39.29077541743));
#38542=CARTESIAN_POINT('Ctrl Pts',(21.5108020730258,2.70720879825165,39.2996446606775));
#38543=CARTESIAN_POINT('Ctrl Pts',(21.4993429186813,2.70602497061475,39.3139037401377));
#38544=CARTESIAN_POINT('Ctrl Pts',(21.4949319131556,2.705571163259,39.3193318051359));
#38545=CARTESIAN_POINT('Ctrl Pts',(21.4864252892428,2.70469951975784,39.3296842843577));
#38546=CARTESIAN_POINT('Ctrl Pts',(21.4823344666383,2.70428188010314,39.3346125331692));
#38547=CARTESIAN_POINT('Ctrl Pts',(21.4729545304108,2.70332768198222,39.3457987980023));
#38548=CARTESIAN_POINT('Ctrl Pts',(21.4676499645987,2.70279050011322,39.3520436380918));
#38549=CARTESIAN_POINT('Ctrl Pts',(21.4535354974341,2.70136743375187,39.3684470518819));
#38550=CARTESIAN_POINT('Ctrl Pts',(21.4446590159347,2.70047882719762,39.3785474875494));
#38551=CARTESIAN_POINT('Ctrl Pts',(21.3759054453228,2.69364286459706,39.4551511625999));
#38552=CARTESIAN_POINT('Ctrl Pts',(21.3115807262736,2.68750718281808,39.5174985928199));
#38553=CARTESIAN_POINT('Ctrl Pts',(21.1192444162555,2.66986429621142,39.6795883737103));
#38554=CARTESIAN_POINT('Ctrl Pts',(20.9826616067041,2.65805951154523,39.7679869209663));
#38555=CARTESIAN_POINT('Ctrl Pts',(20.8095689876326,2.64481552014014,39.8512975871015));
#38556=CARTESIAN_POINT('Ctrl Pts',(20.7821950730113,2.64276987420016,39.8636939358309));
#38557=CARTESIAN_POINT('Ctrl Pts',(20.7480665920808,2.64028869356715,39.8781980820234));
#38558=CARTESIAN_POINT('Ctrl Pts',(20.7415771047436,2.63981994626655,39.8809142165149));
#38559=CARTESIAN_POINT('Ctrl Pts',(20.7313227642944,2.63908421201398,39.8851403369242));
#38560=CARTESIAN_POINT('Ctrl Pts',(20.727567838374,2.63881584384386,39.8866740187865));
#38561=CARTESIAN_POINT('Ctrl Pts',(20.7204962670545,2.63831242771437,39.8895363787909));
#38562=CARTESIAN_POINT('Ctrl Pts',(20.7171808063892,2.63807723132922,39.890867670446));
#38563=CARTESIAN_POINT('Ctrl Pts',(20.7095979773278,2.63754117357786,39.89388804833));
#38564=CARTESIAN_POINT('Ctrl Pts',(20.7053282696522,2.63724067261447,39.8955711215295));
#38565=CARTESIAN_POINT('Ctrl Pts',(20.6939805882409,2.63644547408643,39.8999975339677));
#38566=CARTESIAN_POINT('Ctrl Pts',(20.686892272989,2.63595230386472,39.9027143947518));
#38567=CARTESIAN_POINT('Ctrl Pts',(20.6365228130546,2.63247170303313,39.9216801384828));
#38568=CARTESIAN_POINT('Ctrl Pts',(20.5926819389425,2.62956667003102,39.9364119175139));
#38569=CARTESIAN_POINT('Ctrl Pts',(20.4275985956237,2.61893859112482,39.9853552925194));
#38570=CARTESIAN_POINT('Ctrl Pts',(20.3036236393871,2.61155247367216,40.0092465645142));
#38571=CARTESIAN_POINT('Ctrl Pts',(20.071384872498,2.59753259676736,40.0307909766193));
#38572=CARTESIAN_POINT('Ctrl Pts',(19.9639473736855,2.59097562209409,40.0317725047487));
#38573=CARTESIAN_POINT('Ctrl Pts',(19.8423139832667,2.58318347090327,40.0227309663199));
#38574=CARTESIAN_POINT('Ctrl Pts',(19.8276473386552,2.58223802884719,40.0214717769315));
#38575=CARTESIAN_POINT('Ctrl Pts',(19.8052970532705,2.58078774996471,40.0192949666091));
#38576=CARTESIAN_POINT('Ctrl Pts',(19.7976019209633,2.58028669662734,40.0184987414758));
#38577=CARTESIAN_POINT('Ctrl Pts',(19.7836031582776,2.57937196134497,40.0169651122066));
#38578=CARTESIAN_POINT('Ctrl Pts',(19.7772979519516,2.57895875772002,40.0162428423127));
#38579=CARTESIAN_POINT('Ctrl Pts',(19.7636810505516,2.57806375335962,40.0146148937941));
#38580=CARTESIAN_POINT('Ctrl Pts',(19.756370771401,2.57758162083575,40.0136984176844));
#38581=CARTESIAN_POINT('Ctrl Pts',(19.7365203670184,2.57626786499577,40.0110942263146));
#38582=CARTESIAN_POINT('Ctrl Pts',(19.7239914849026,2.57543370355801,40.0093249973601));
#38583=CARTESIAN_POINT('Ctrl Pts',(19.6620619283136,2.57128518945258,39.9999575140884));
#38584=CARTESIAN_POINT('Ctrl Pts',(19.6129561118462,2.56791510531554,39.9905652459399));
#38585=CARTESIAN_POINT('Ctrl Pts',(19.5384408765842,2.56267277912306,39.9732882726191));
#38586=CARTESIAN_POINT('Ctrl Pts',(19.5127350954418,2.56084064285159,39.9667668809669));
#38587=CARTESIAN_POINT('Ctrl Pts',(19.365874586633,2.55024045298943,39.926269308208));
#38588=CARTESIAN_POINT('Ctrl Pts',(19.2481465339524,2.54119143588346,39.8810350696547));
#38589=CARTESIAN_POINT('Ctrl Pts',(19.0864568095457,2.52835464991372,39.8000035886388));
#38590=CARTESIAN_POINT('Ctrl Pts',(19.0383135496695,2.52448005371354,39.7732403928952));
#38591=CARTESIAN_POINT('Ctrl Pts',(18.9674775824633,2.51876185415784,39.7297932810787));
#38592=CARTESIAN_POINT('Ctrl Pts',(18.9438979976954,2.51685551083962,39.7146137142168));
#38593=CARTESIAN_POINT('Ctrl Pts',(18.914952761141,2.5145196159674,39.6950744182306));
#38594=CARTESIAN_POINT('Ctrl Pts',(18.9092697907039,2.51406120767834,39.6911937419147));
#38595=CARTESIAN_POINT('Ctrl Pts',(18.900298265023,2.51333802126474,39.6849967911428));
#38596=CARTESIAN_POINT('Ctrl Pts',(18.8969960469015,2.51307193817817,39.6827005446481));
#38597=CARTESIAN_POINT('Ctrl Pts',(18.8907680847924,2.51257034434057,39.6783408796276));
#38598=CARTESIAN_POINT('Ctrl Pts',(18.8878409387374,2.51233469928018,39.6762796695677));
#38599=CARTESIAN_POINT('Ctrl Pts',(18.8811274371085,2.51179445268715,39.6715242089815));
#38600=CARTESIAN_POINT('Ctrl Pts',(18.8773450663637,2.51149023211789,39.6688244173586));
#38601=CARTESIAN_POINT('Ctrl Pts',(18.8672503682369,2.51067860581816,39.6615637911655));
#38602=CARTESIAN_POINT('Ctrl Pts',(18.8609557599148,2.5101728294972,39.6569782998532));
#38603=CARTESIAN_POINT('Ctrl Pts',(18.8135966291405,2.50636846243603,39.6220372298172));
#38604=CARTESIAN_POINT('Ctrl Pts',(18.7737201048851,2.50317058316769,39.5900969579077));
#38605=CARTESIAN_POINT('Ctrl Pts',(18.6370708370491,2.49204419624869,39.4714376298351));
#38606=CARTESIAN_POINT('Ctrl Pts',(18.5478355178802,2.48444154210104,39.3765733955574));
#38607=CARTESIAN_POINT('Ctrl Pts',(18.4145035042108,2.47122505034933,39.2025940612386));
#38608=CARTESIAN_POINT('Ctrl Pts',(18.3651889648186,2.46575407074745,39.1280577722659));
#38609=CARTESIAN_POINT('Ctrl Pts',(18.311136379595,2.45878922739923,39.0325774938197));
#38610=CARTESIAN_POINT('Ctrl Pts',(18.3013416839863,2.45748110233096,39.0146152113554));
#38611=CARTESIAN_POINT('Ctrl Pts',(18.28773129818,2.45559396135025,38.9886824067608));
#38612=CARTESIAN_POINT('Ctrl Pts',(18.2836815872703,2.455023147258,38.9808357560809));
#38613=CARTESIAN_POINT('Ctrl Pts',(18.2767523736861,2.45402998562907,38.9671806051903));
#38614=CARTESIAN_POINT('Ctrl Pts',(18.2738479936511,2.45360851143797,38.9613848343723));
#38615=CARTESIAN_POINT('Ctrl Pts',(18.2683170668068,2.45279574552673,38.9502074076196));
#38616=CARTESIAN_POINT('Ctrl Pts',(18.2656862531136,2.45240460759234,38.9448279369723));
#38617=CARTESIAN_POINT('Ctrl Pts',(18.2595344007411,2.45147910845092,38.9320988337403));
#38618=CARTESIAN_POINT('Ctrl Pts',(18.2560348256246,2.4509440155397,38.9247390123206));
#38619=CARTESIAN_POINT('Ctrl Pts',(18.2439642600965,2.44906775947515,38.8989335019963));
#38620=CARTESIAN_POINT('Ctrl Pts',(18.2356386931552,2.44771827324523,38.88037515708));
#38621=CARTESIAN_POINT('Ctrl Pts',(18.1608324141978,2.43505490225917,38.7063067607359));
#38622=CARTESIAN_POINT('Ctrl Pts',(18.114792244157,2.42302274532309,38.5428465110104));
#38623=CARTESIAN_POINT('Ctrl Pts',(18.0805797129769,2.40594633895446,38.305759905488));
#38624=CARTESIAN_POINT('Ctrl Pts',(18.0743427887243,2.40094444206335,38.2354882626051));
#38625=CARTESIAN_POINT('Ctrl Pts',(18.0712319781269,2.39456633323423,38.143255844243));
#38626=CARTESIAN_POINT('Ctrl Pts',(18.0708664568246,2.39307365318261,38.1214711559831));
#38627=CARTESIAN_POINT('Ctrl Pts',(18.0708723612183,2.39063161387751,38.0854280318276));
#38628=CARTESIAN_POINT('Ctrl Pts',(18.0710327202739,2.3896728751938,38.0711720263516));
#38629=CARTESIAN_POINT('Ctrl Pts',(18.0714751079546,2.38835210647864,38.051367410205));
#38630=CARTESIAN_POINT('Ctrl Pts',(18.0716230764981,2.3879831441303,38.0458166924315));
#38631=CARTESIAN_POINT('Ctrl Pts',(18.0718989790891,2.38739317178397,38.0369105057474));
#38632=CARTESIAN_POINT('Ctrl Pts',(18.0720117098403,2.38717133291001,38.0335546498165));
#38633=CARTESIAN_POINT('Ctrl Pts',(18.0722657605068,2.38670848260905,38.0265378970563));
#38634=CARTESIAN_POINT('Ctrl Pts',(18.0724087477532,2.38646757023914,38.0228770900491));
#38635=CARTESIAN_POINT('Ctrl Pts',(18.0727812291302,2.38588405129458,38.0139899240755));
#38636=CARTESIAN_POINT('Ctrl Pts',(18.0730215576221,2.38554204277053,38.0087639975883));
#38637=CARTESIAN_POINT('Ctrl Pts',(18.073945986909,2.38433738415484,37.9902993932441));
#38638=CARTESIAN_POINT('Ctrl Pts',(18.074745300028,2.38348086312548,37.9770664887699));
#38639=CARTESIAN_POINT('Ctrl Pts',(18.0804482971912,2.37829968707831,37.8964658548161));
#38640=CARTESIAN_POINT('Ctrl Pts',(18.0887514985972,2.3741391856421,37.8293783406481));
#38641=CARTESIAN_POINT('Ctrl Pts',(18.1219088814571,2.36264470240885,37.6425712657982));
#38642=CARTESIAN_POINT('Ctrl Pts',(18.1546368139108,2.35547522620142,37.5245842842083));
#38643=CARTESIAN_POINT('Ctrl Pts',(18.227807506339,2.34305210998545,37.3333905924606));
#38644=CARTESIAN_POINT('Ctrl Pts',(18.2622250155511,2.33794882236075,37.2582804772984));
#38645=CARTESIAN_POINT('Ctrl Pts',(18.3076218454999,2.33183000691493,37.1739469731754));
#38646=CARTESIAN_POINT('Ctrl Pts',(18.3140203935903,2.33097967525284,37.1623482634531));
#38647=CARTESIAN_POINT('Ctrl Pts',(18.3245835198597,2.3295946714876,37.1436581223657));
#38648=CARTESIAN_POINT('Ctrl Pts',(18.3286749561505,2.32906259924003,37.1365256810891));
#38649=CARTESIAN_POINT('Ctrl Pts',(18.3360270389649,2.3281140936265,37.1238968386692));
#38650=CARTESIAN_POINT('Ctrl Pts',(18.3392696543895,2.32769831235906,37.1183900397063));
#38651=CARTESIAN_POINT('Ctrl Pts',(18.3461464961397,2.32682180992262,37.1068429952113));
#38652=CARTESIAN_POINT('Ctrl Pts',(18.3497865811584,2.32636088109772,37.1008063658869));
#38653=CARTESIAN_POINT('Ctrl Pts',(18.3594764756729,2.3251417203357,37.0849342588209));
#38654=CARTESIAN_POINT('Ctrl Pts',(18.3655815752862,2.32438148224348,37.0751330350015));
#38655=CARTESIAN_POINT('Ctrl Pts',(18.3942189907791,2.3208508566806,37.0300647857358));
#38656=CARTESIAN_POINT('Ctrl Pts',(18.4178056613398,2.3180418522169,36.9954844377372));
#38657=CARTESIAN_POINT('Ctrl Pts',(18.5412971267982,2.3037937555316,36.8265145133867));
#38658=CARTESIAN_POINT('Ctrl Pts',(18.6572678458037,2.2917302167849,36.7047826648682));
#38659=CARTESIAN_POINT('Ctrl Pts',(18.7964907657336,2.27904327237431,36.5922722474851));
#38660=CARTESIAN_POINT('Ctrl Pts',(18.8055900426846,2.27822171005806,36.5850536931518));
#38661=CARTESIAN_POINT('Ctrl Pts',(18.827182235825,2.2762908871701,36.5682398461245));
#38662=CARTESIAN_POINT('Ctrl Pts',(18.8397287397793,2.27518344950221,36.5587144003546));
#38663=CARTESIAN_POINT('Ctrl Pts',(18.8912966929374,2.27069419711152,36.5205500096734));
#38664=CARTESIAN_POINT('Ctrl Pts',(18.9312764141424,2.26735695047316,36.4932280516757));
#38665=CARTESIAN_POINT('Ctrl Pts',(18.9787475590504,2.26359244768881,36.4633433334009));
#38666=CARTESIAN_POINT('Ctrl Pts',(18.9852743656991,2.26307907681671,36.459288726077));
#38667=CARTESIAN_POINT('Ctrl Pts',(18.9957613189835,2.26226114897953,36.4528604973739));
#38668=CARTESIAN_POINT('Ctrl Pts',(18.9997059817277,2.26195504307505,36.4504619593149));
#38669=CARTESIAN_POINT('Ctrl Pts',(19.0067214963704,2.26141344904227,36.4462306207904));
#38670=CARTESIAN_POINT('Ctrl Pts',(19.0097888779322,2.26117759889086,36.4443921720605));
#38671=CARTESIAN_POINT('Ctrl Pts',(19.0163321473246,2.26067652301233,36.4404951246609));
#38672=CARTESIAN_POINT('Ctrl Pts',(19.0198093890805,2.26041145074962,36.4384389139521));
#38673=CARTESIAN_POINT('Ctrl Pts',(19.0292958248408,2.25969151271216,36.4328694070494));
#38674=CARTESIAN_POINT('Ctrl Pts',(19.0353176884968,2.25923800851437,36.4293776455734));
#38675=CARTESIAN_POINT('Ctrl Pts',(19.0665740660081,2.25690146777443,36.4114790769709));
#38676=CARTESIAN_POINT('Ctrl Pts',(19.0921143856017,2.25505051011215,36.3976102637962));
#38677=CARTESIAN_POINT('Ctrl Pts',(19.2069417831661,2.24694070403176,36.338576797337));
#38678=CARTESIAN_POINT('Ctrl Pts',(19.2992730025973,2.24097284866353,36.299860718032));
#38679=CARTESIAN_POINT('Ctrl Pts',(19.3941044697278,2.2350068401775,36.268488830693));
#38680=CARTESIAN_POINT('',(18.0708706743286,2.22141497567151,38.1016129892876));
#38681=CARTESIAN_POINT('Ctrl Pts',(19.3941040086996,2.0626282966298,36.2684889832092));
#38682=CARTESIAN_POINT('Ctrl Pts',(19.3837674814086,2.06331292737663,36.2719084878653));
#38683=CARTESIAN_POINT('Ctrl Pts',(19.3734576817228,2.06400028375384,36.2754162315735));
#38684=CARTESIAN_POINT('Ctrl Pts',(19.3426326342688,2.0660695318738,36.2861961695889));
#38685=CARTESIAN_POINT('Ctrl Pts',(19.3222132677515,2.06745915353942,36.2937272427941));
#38686=CARTESIAN_POINT('Ctrl Pts',(19.2941088216315,2.06939999429191,36.3046363815698));
#38687=CARTESIAN_POINT('Ctrl Pts',(19.2863113020811,2.06994151740616,36.3077217523744));
#38688=CARTESIAN_POINT('Ctrl Pts',(19.2729239932806,2.07087660059436,36.3131201410377));
#38689=CARTESIAN_POINT('Ctrl Pts',(19.2673244661449,2.07126934347668,36.3154088113464));
#38690=CARTESIAN_POINT('Ctrl Pts',(19.2557828735064,2.07208226101268,36.3201896325796));
#38691=CARTESIAN_POINT('Ctrl Pts',(19.2498423516104,2.07250254950246,36.3226852906081));
#38692=CARTESIAN_POINT('Ctrl Pts',(19.2361661600603,2.07347452345652,36.3285115426101));
#38693=CARTESIAN_POINT('Ctrl Pts',(19.2284396214318,2.07402691172667,36.3318631082023));
#38694=CARTESIAN_POINT('Ctrl Pts',(19.2039324085865,2.07578953688088,36.3426849059176));
#38695=CARTESIAN_POINT('Ctrl Pts',(19.1872367786683,2.07700616077794,36.3503440748035));
#38696=CARTESIAN_POINT('Ctrl Pts',(19.148409691538,2.07987368153634,36.3688317609161));
#38697=CARTESIAN_POINT('Ctrl Pts',(19.126371685827,2.08153081106813,36.3798479716506));
#38698=CARTESIAN_POINT('Ctrl Pts',(19.0491866014652,2.0874415986763,36.420296599831));
#38699=CARTESIAN_POINT('Ctrl Pts',(18.9952697390479,2.09176865068765,36.4519813695081));
#38700=CARTESIAN_POINT('Ctrl Pts',(18.8277802712925,2.10583271508917,36.5616856104231));
#38701=CARTESIAN_POINT('Ctrl Pts',(18.7209901401899,2.11580306557456,36.649261791309));
#38702=CARTESIAN_POINT('Ctrl Pts',(18.5904697249032,2.12883024623558,36.7820037402358));
#38703=CARTESIAN_POINT('Ctrl Pts',(18.5578123162378,2.1321707479992,36.8178200882498));
#38704=CARTESIAN_POINT('Ctrl Pts',(18.5215749130172,2.13593846750677,36.8607014553424));
#38705=CARTESIAN_POINT('Ctrl Pts',(18.5166494151853,2.13645196227061,36.8666011723855));
#38706=CARTESIAN_POINT('Ctrl Pts',(18.5088214395908,2.13727004826609,36.8760921703944));
#38707=CARTESIAN_POINT('Ctrl Pts',(18.5058964312515,2.1375761893785,36.8796646357067));
#38708=CARTESIAN_POINT('Ctrl Pts',(18.5007286692489,2.1381178220528,36.8860227256939));
#38709=CARTESIAN_POINT('Ctrl Pts',(18.4984808031248,2.13835367583354,36.8888041248516));
#38710=CARTESIAN_POINT('Ctrl Pts',(18.4937104067454,2.13885473301535,36.8947404702165));
#38711=CARTESIAN_POINT('Ctrl Pts',(18.4911900506403,2.13911978308861,36.8978970882922));
#38712=CARTESIAN_POINT('Ctrl Pts',(18.484354455053,2.13983960134159,36.9065136905843));
#38713=CARTESIAN_POINT('Ctrl Pts',(18.4800587642489,2.14029300869801,36.9119892121048));
#38714=CARTESIAN_POINT('Ctrl Pts',(18.4579931863945,2.14262820041621,36.9404307952289));
#38715=CARTESIAN_POINT('Ctrl Pts',(18.4407127616884,2.14447794987287,36.9637741056941));
#38716=CARTESIAN_POINT('Ctrl Pts',(18.3383613315816,2.1556261271066,37.1087713845485));
#38717=CARTESIAN_POINT('Ctrl Pts',(18.2670313528305,2.1642745534715,37.239530788041));
#38718=CARTESIAN_POINT('Ctrl Pts',(18.1955004796772,2.17576009324727,37.4165347113017));
#38719=CARTESIAN_POINT('Ctrl Pts',(18.1809038118789,2.17833025404646,37.4563913204045));
#38720=CARTESIAN_POINT('Ctrl Pts',(18.1477329086564,2.18483426385661,37.5571385189386));
#38721=CARTESIAN_POINT('Ctrl Pts',(18.1308367911885,2.18880476548764,37.618523557311));
#38722=CARTESIAN_POINT('Ctrl Pts',(18.1143038206637,2.19366898491016,37.6927569314287));
#38723=CARTESIAN_POINT('Ctrl Pts',(18.1117195549744,2.19446741301666,37.7049127349891));
#38724=CARTESIAN_POINT('Ctrl Pts',(18.1076701947323,2.19578425777799,37.7249079415508));
#38725=CARTESIAN_POINT('Ctrl Pts',(18.10613591901,2.19630048248717,37.7327330891463));
#38726=CARTESIAN_POINT('Ctrl Pts',(18.1034645937295,2.19723142816394,37.746819446872));
#38727=CARTESIAN_POINT('Ctrl Pts',(18.1023099198421,2.19764558579903,37.7530772299217));
#38728=CARTESIAN_POINT('Ctrl Pts',(18.1001323311239,2.19845008584416,37.7652149686975));
#38729=CARTESIAN_POINT('Ctrl Pts',(18.0991056989401,2.19884030576123,37.7710941908712));
#38730=CARTESIAN_POINT('Ctrl Pts',(18.0969243607689,2.19969396873407,37.7839375065397));
#38731=CARTESIAN_POINT('Ctrl Pts',(18.0957805688173,2.2001577500138,37.7909033418525));
#38732=CARTESIAN_POINT('Ctrl Pts',(18.09307340656,2.20129639992165,37.8079758369018));
#38733=CARTESIAN_POINT('Ctrl Pts',(18.0915521365483,2.201972578416,37.8180888610348));
#38734=CARTESIAN_POINT('Ctrl Pts',(18.0772218344598,2.20872315228076,37.9187902017144));
#38735=CARTESIAN_POINT('Ctrl Pts',(18.0707942025025,2.21499668833455,38.0101529632487));
#38736=CARTESIAN_POINT('Ctrl Pts',(18.0708706743286,2.22141497567151,38.1016129892876));
#38737=CARTESIAN_POINT('Ctrl Pts',(18.0708706726244,2.22141483255489,38.101610949888));
#38738=CARTESIAN_POINT('Ctrl Pts',(18.0709609419981,2.22900073837971,38.2097094683175));
#38739=CARTESIAN_POINT('Ctrl Pts',(18.0801371753914,2.23676879516904,38.3176093215099));
#38740=CARTESIAN_POINT('Ctrl Pts',(18.1104940944532,2.24959110593643,38.495695526882));
#38741=CARTESIAN_POINT('Ctrl Pts',(18.1267142218013,2.25468398518988,38.5664870627855));
#38742=CARTESIAN_POINT('Ctrl Pts',(18.1507073391127,2.26052604307724,38.6494070975814));
#38743=CARTESIAN_POINT('Ctrl Pts',(18.1546691527667,2.26144961169759,38.6625705246755));
#38744=CARTESIAN_POINT('Ctrl Pts',(18.1603552841934,2.26271915466431,38.6807564415166));
#38745=CARTESIAN_POINT('Ctrl Pts',(18.1619600210698,2.26307162883516,38.6858154677575));
#38746=CARTESIAN_POINT('Ctrl Pts',(18.1647122872409,2.26366635901946,38.694369496987));
#38747=CARTESIAN_POINT('Ctrl Pts',(18.1658489638607,2.2639092373872,38.6978679327191));
#38748=CARTESIAN_POINT('Ctrl Pts',(18.1680374130316,2.26437163514157,38.7045385057978));
#38749=CARTESIAN_POINT('Ctrl Pts',(18.169087427831,2.26459125823236,38.7077111802016));
#38750=CARTESIAN_POINT('Ctrl Pts',(18.1718775310252,2.26516903548758,38.7160687509546));
#38751=CARTESIAN_POINT('Ctrl Pts',(18.1736314485895,2.26552638672897,38.7212490512517));
#38752=CARTESIAN_POINT('Ctrl Pts',(18.1798720596672,2.26677780406596,38.7394262139612));
#38753=CARTESIAN_POINT('Ctrl Pts',(18.1844757741283,2.26766532294951,38.7523828734396));
#38754=CARTESIAN_POINT('Ctrl Pts',(18.237220697295,2.27746063615847,38.8959437566029));
#38755=CARTESIAN_POINT('Ctrl Pts',(18.2992310100625,2.28566008279396,39.0210397683309));
#38756=CARTESIAN_POINT('Ctrl Pts',(18.4127755032649,2.29827107498648,39.1988189258553));
#38757=CARTESIAN_POINT('Ctrl Pts',(18.4547114529037,2.30257688317349,39.2570510130127));
#38758=CARTESIAN_POINT('Ctrl Pts',(18.5259468670265,2.30953179534874,39.3451670791728));
#38759=CARTESIAN_POINT('Ctrl Pts',(18.5531428812381,2.3121152190768,39.3766666835909));
#38760=CARTESIAN_POINT('Ctrl Pts',(18.6000092488074,2.31647486485586,39.4275269886585));
#38761=CARTESIAN_POINT('Ctrl Pts',(18.6191151506446,2.31822856140567,39.4473896690387));
#38762=CARTESIAN_POINT('Ctrl Pts',(18.6454931391802,2.32062252827853,39.4736620027975));
#38763=CARTESIAN_POINT('Ctrl Pts',(18.6523982104883,2.32124676921118,39.4804367226639));
#38764=CARTESIAN_POINT('Ctrl Pts',(18.6636305877078,2.32225846966197,39.4912924659715));
#38765=CARTESIAN_POINT('Ctrl Pts',(18.6679263862433,2.32264452216654,39.4954059689565));
#38766=CARTESIAN_POINT('Ctrl Pts',(18.6768882345388,2.3234481453241,39.503908418453));
#38767=CARTESIAN_POINT('Ctrl Pts',(18.6815572536949,2.3238658476275,39.5082941150078));
#38768=CARTESIAN_POINT('Ctrl Pts',(18.6922527724101,2.32482053559937,39.518240807613));
#38769=CARTESIAN_POINT('Ctrl Pts',(18.6982930275449,2.32535814693835,39.5237867656403));
#38770=CARTESIAN_POINT('Ctrl Pts',(18.714347158798,2.32678309904504,39.538339573154));
#38771=CARTESIAN_POINT('Ctrl Pts',(18.7244201721483,2.32767317345917,39.5472802226952));
#38772=CARTESIAN_POINT('Ctrl Pts',(18.8015692546965,2.33446137931533,39.6143254645469));
#38773=CARTESIAN_POINT('Ctrl Pts',(18.8724794809763,2.34054455229296,39.6678364830251));
#38774=CARTESIAN_POINT('Ctrl Pts',(19.0812216282755,2.3580150087443,39.8038562215967));
#38775=CARTESIAN_POINT('Ctrl Pts',(19.2260215775423,2.36969488126651,39.8743262352871));
#38776=CARTESIAN_POINT('Ctrl Pts',(19.4082628650795,2.38299358288505,39.9364152078867));
#38777=CARTESIAN_POINT('Ctrl Pts',(19.4389139965967,2.38518310687873,39.9460109552883));
#38778=CARTESIAN_POINT('Ctrl Pts',(19.4766972120311,2.38781324187271,39.9568113310942));
#38779=CARTESIAN_POINT('Ctrl Pts',(19.4836130027279,2.3882918624023,39.9587465131705));
#38780=CARTESIAN_POINT('Ctrl Pts',(19.4944827097626,2.38903956703852,39.9617227345097));
#38781=CARTESIAN_POINT('Ctrl Pts',(19.4984293159343,2.3893101068305,39.9627898755835));
#38782=CARTESIAN_POINT('Ctrl Pts',(19.50582564974,2.3898153299646,39.9647645943081));
#38783=CARTESIAN_POINT('Ctrl Pts',(19.5092744643569,2.39005017496455,39.96567514042));
#38784=CARTESIAN_POINT('Ctrl Pts',(19.5171906144162,2.39058756040116,39.9677416701674));
#38785=CARTESIAN_POINT('Ctrl Pts',(19.5216595813365,2.39088972861176,39.9688911937968));
#38786=CARTESIAN_POINT('Ctrl Pts',(19.5334116883059,2.39168128253318,39.9718691969183));
#38787=CARTESIAN_POINT('Ctrl Pts',(19.5407015408204,2.39216920128345,39.9736712285856));
#38788=CARTESIAN_POINT('Ctrl Pts',(19.5913510317723,2.39553905554356,39.9858782780073));
#38789=CARTESIAN_POINT('Ctrl Pts',(19.6350533939722,2.39834437620869,39.9948207177396));
#38790=CARTESIAN_POINT('Ctrl Pts',(19.8266182305024,2.41035294625213,40.027143922744));
#38791=CARTESIAN_POINT('Ctrl Pts',(19.9766114017382,2.41905134242259,40.0347880714908));
#38792=CARTESIAN_POINT('Ctrl Pts',(20.2043027713724,2.43288062786482,40.0198859857278));
#38793=CARTESIAN_POINT('Ctrl Pts',(20.2822220750879,2.4377189529152,40.0099870102348));
#38794=CARTESIAN_POINT('Ctrl Pts',(20.378101033434,2.44392238238293,39.9918106970656));
#38795=CARTESIAN_POINT('Ctrl Pts',(20.3968312347448,2.44514605375802,39.9879706127031));
#38796=CARTESIAN_POINT('Ctrl Pts',(20.4238920935745,2.44693244664039,39.9820020961753));
#38797=CARTESIAN_POINT('Ctrl Pts',(20.4322708662512,2.44748814181692,39.9800952878166));
#38798=CARTESIAN_POINT('Ctrl Pts',(20.4469095845359,2.44846364779153,39.9766608371438));
#38799=CARTESIAN_POINT('Ctrl Pts',(20.4531751818969,2.44888267258375,39.9751576806381));
#38800=CARTESIAN_POINT('Ctrl Pts',(20.4653083681166,2.44969705297167,39.9721824895531));
#38801=CARTESIAN_POINT('Ctrl Pts',(20.4711768017813,2.45009228476865,39.9707141876015));
#38802=CARTESIAN_POINT('Ctrl Pts',(20.485164032666,2.45103755996511,39.9671445440556));
#38803=CARTESIAN_POINT('Ctrl Pts',(20.4932761691972,2.45158841155734,39.965017829444));
#38804=CARTESIAN_POINT('Ctrl Pts',(20.5223925511194,2.45357515712556,39.9571812937121));
#38805=CARTESIAN_POINT('Ctrl Pts',(20.5433130162198,2.45502071594099,39.9511691538027));
#38806=CARTESIAN_POINT('Ctrl Pts',(20.7098551754629,2.46667804172203,39.9002418840376));
#38807=CARTESIAN_POINT('Ctrl Pts',(20.8497629334488,2.47745669931358,39.8385771134705));
#38808=CARTESIAN_POINT('Ctrl Pts',(21.0513417662641,2.49416159725634,39.7195399100313));
#38809=CARTESIAN_POINT('Ctrl Pts',(21.1190419285904,2.49999266928135,39.6735233920551));
#38810=CARTESIAN_POINT('Ctrl Pts',(21.2118419231335,2.50813571857942,39.6014189822083));
#38811=CARTESIAN_POINT('Ctrl Pts',(21.2394505980905,2.51057858889319,39.578709715305));
#38812=CARTESIAN_POINT('Ctrl Pts',(21.2720066774823,2.51346855251977,39.5503780637209));
#38813=CARTESIAN_POINT('Ctrl Pts',(21.2775710039241,2.51396282775438,39.5454791072874));
#38814=CARTESIAN_POINT('Ctrl Pts',(21.2861978723628,2.5147294848541,39.5377950904769));
#38815=CARTESIAN_POINT('Ctrl Pts',(21.2892798513917,2.5150034437997,39.5350321092801));
#38816=CARTESIAN_POINT('Ctrl Pts',(21.294996006555,2.5155116434555,39.5298743208044));
#38817=CARTESIAN_POINT('Ctrl Pts',(21.2976324218261,2.51574606633729,39.5274821639645));
#38818=CARTESIAN_POINT('Ctrl Pts',(21.3036150682087,2.51627811384295,39.5220235266704));
#38819=CARTESIAN_POINT('Ctrl Pts',(21.3069571037145,2.51657539388721,39.5189525314664));
#38820=CARTESIAN_POINT('Ctrl Pts',(21.317138055274,2.51748132798786,39.5095307735622));
#38821=CARTESIAN_POINT('Ctrl Pts',(21.3239418751051,2.51808719841528,39.5031420377499));
#38822=CARTESIAN_POINT('Ctrl Pts',(21.3893905170916,2.52392281948971,39.4407863375027));
#38823=CARTESIAN_POINT('Ctrl Pts',(21.4445070103362,2.52889752383458,39.3812170001058));
#38824=CARTESIAN_POINT('Ctrl Pts',(21.5992226525299,2.54368379363837,39.1912788415149));
#38825=CARTESIAN_POINT('Ctrl Pts',(21.6861082669779,2.55324315995879,39.0515465072539));
#38826=CARTESIAN_POINT('Ctrl Pts',(21.7706251192927,2.56592484791844,38.8667933744221));
#38827=CARTESIAN_POINT('Ctrl Pts',(21.7858693434932,2.5684081405143,38.8305858888898));
#38828=CARTESIAN_POINT('Ctrl Pts',(21.8040618525085,2.5716538036117,38.783396720437));
#38829=CARTESIAN_POINT('Ctrl Pts',(21.808033834689,2.57238197726352,38.7728178720649));
#38830=CARTESIAN_POINT('Ctrl Pts',(21.8143135761112,2.5735658752575,38.7556353622928));
#38831=CARTESIAN_POINT('Ctrl Pts',(21.8166787971334,2.5740196945362,38.7490528689272));
#38832=CARTESIAN_POINT('Ctrl Pts',(21.8211411402213,2.57489134468714,38.7364185148809));
#38833=CARTESIAN_POINT('Ctrl Pts',(21.823244026951,2.57530897898102,38.730368777164));
#38834=CARTESIAN_POINT('Ctrl Pts',(21.8279682464349,2.5762631422604,38.7165563854847));
#38835=CARTESIAN_POINT('Ctrl Pts',(21.8305703159642,2.57680029449718,38.7087873202346));
#38836=CARTESIAN_POINT('Ctrl Pts',(21.8373114587073,2.57822323363825,38.6882260874263));
#38837=CARTESIAN_POINT('Ctrl Pts',(21.8413663656927,2.57911174183464,38.6754070020759));
#38838=CARTESIAN_POINT('Ctrl Pts',(21.8713651384373,2.58594379149808,38.5770039244058));
#38839=CARTESIAN_POINT('Ctrl Pts',(21.8914597506812,2.59207540821949,38.4897640808411));
#38840=CARTESIAN_POINT('Ctrl Pts',(21.9307315793931,2.60970288143303,38.241536479277));
#38841=CARTESIAN_POINT('Ctrl Pts',(21.9357985521885,2.62149577502337,38.0790797125331));
#38842=CARTESIAN_POINT('Ctrl Pts',(21.9176626776828,2.63474443700944,37.8878055753898));
#38843=CARTESIAN_POINT('Ctrl Pts',(21.9141014895529,2.6368032742196,37.8577762222596));
#38844=CARTESIAN_POINT('Ctrl Pts',(21.9088411887868,2.63929815585782,37.8208628350344));
#38845=CARTESIAN_POINT('Ctrl Pts',(21.9078085128571,2.63976784016104,37.813890016022));
#38846=CARTESIAN_POINT('Ctrl Pts',(21.9061209607066,2.64050471050852,37.8029109290229));
#38847=CARTESIAN_POINT('Ctrl Pts',(21.905491631387,2.6407732847713,37.7989008860716));
#38848=CARTESIAN_POINT('Ctrl Pts',(21.9042846707602,2.64127686862687,37.7913655718566));
#38849=CARTESIAN_POINT('Ctrl Pts',(21.9037099114485,2.64151202791202,37.7878399595895));
#38850=CARTESIAN_POINT('Ctrl Pts',(21.9023751573773,2.64204772341363,37.7797932948486));
#38851=CARTESIAN_POINT('Ctrl Pts',(21.9016088382092,2.64234790101261,37.775273344266));
#38852=CARTESIAN_POINT('Ctrl Pts',(21.8995337617006,2.64314167792473,37.763293288296));
#38853=CARTESIAN_POINT('Ctrl Pts',(21.8981971552068,2.64363375857316,37.7558379944219));
#38854=CARTESIAN_POINT('Ctrl Pts',(21.8884599243563,2.6470887678886,37.7033088455004));
#38855=CARTESIAN_POINT('Ctrl Pts',(21.8784978716309,2.64997066305941,37.6585350753943));
#38856=CARTESIAN_POINT('Ctrl Pts',(21.8594741673796,2.65463465864422,37.585432999102));
#38857=CARTESIAN_POINT('Ctrl Pts',(21.8513376119807,2.65644537548504,37.556886244054));
#38858=CARTESIAN_POINT('Ctrl Pts',(21.7932504613387,2.668320503885,37.3695979596894));
#38859=CARTESIAN_POINT('Ctrl Pts',(21.7236015157723,2.67799748101472,37.2177114922496));
#38860=CARTESIAN_POINT('Ctrl Pts',(21.6124725188639,2.69103523714952,37.0401270388563));
#38861=CARTESIAN_POINT('Ctrl Pts',(21.5884051671132,2.69375326852014,37.0043874308613));
#38862=CARTESIAN_POINT('Ctrl Pts',(21.5563303471501,2.69726398894659,36.9600375646843));
#38863=CARTESIAN_POINT('Ctrl Pts',(21.5494121598154,2.69801504751461,36.9506521619984));
#38864=CARTESIAN_POINT('Ctrl Pts',(21.5381606147526,2.69922705878787,36.9356742195972));
#38865=CARTESIAN_POINT('Ctrl Pts',(21.5338807579841,2.699685934565,36.9300417025522));
#38866=CARTESIAN_POINT('Ctrl Pts',(21.5256792593149,2.70056128992854,36.9193704554545));
#38867=CARTESIAN_POINT('Ctrl Pts',(21.5217633842612,2.70097753976601,36.9143273957617));
#38868=CARTESIAN_POINT('Ctrl Pts',(21.5127761986139,2.70192907157628,36.9028711110164));
#38869=CARTESIAN_POINT('Ctrl Pts',(21.5076890348471,2.70246497613587,36.8964705343582));
#38870=CARTESIAN_POINT('Ctrl Pts',(21.4943507319243,2.70386322411135,36.8799058085624));
#38871=CARTESIAN_POINT('Ctrl Pts',(21.4860366536778,2.70472807050399,36.8697931086134));
#38872=CARTESIAN_POINT('Ctrl Pts',(21.4279109684917,2.71072963489348,36.800541900227));
#38873=CARTESIAN_POINT('Ctrl Pts',(21.3746924570972,2.71600539709617,36.7443676857191));
#38874=CARTESIAN_POINT('Ctrl Pts',(21.1968432062746,2.73298840488644,36.5779086061822));
#38875=CARTESIAN_POINT('Ctrl Pts',(21.0612650157502,2.74510147445316,36.4804614467146));
#38876=CARTESIAN_POINT('Ctrl Pts',(20.8816380553973,2.75926228354161,36.383700874751));
#38877=CARTESIAN_POINT('Ctrl Pts',(20.847873332075,2.76184672217634,36.3667719057651));
#38878=CARTESIAN_POINT('Ctrl Pts',(20.8068027356714,2.76488063783682,36.3476676649037));
#38879=CARTESIAN_POINT('Ctrl Pts',(20.7999560031608,2.76538281956287,36.3445314971458));
#38880=CARTESIAN_POINT('Ctrl Pts',(20.7892945620614,2.76615903509646,36.3397233186012));
#38881=CARTESIAN_POINT('Ctrl Pts',(20.7854926011904,2.76643470884167,36.3380234748825));
#38882=CARTESIAN_POINT('Ctrl Pts',(20.7784329779411,2.76694445519502,36.3348945329433));
#38883=CARTESIAN_POINT('Ctrl Pts',(20.7751768950254,2.76717872013273,36.3334621451137));
#38884=CARTESIAN_POINT('Ctrl Pts',(20.7677893963602,2.76770833463933,36.3302366591734));
#38885=CARTESIAN_POINT('Ctrl Pts',(20.7636556599757,2.76800335245849,36.3284490202931));
#38886=CARTESIAN_POINT('Ctrl Pts',(20.7510988108066,2.76889559023584,36.3230709153021));
#38887=CARTESIAN_POINT('Ctrl Pts',(20.7426562116054,2.76949014786703,36.3195258622957));
#38888=CARTESIAN_POINT('Ctrl Pts',(20.6326846360213,2.77716962817051,36.2742670509938));
#38889=CARTESIAN_POINT('Ctrl Pts',(20.527783909128,2.78378269262661,36.241225594123));
#38890=CARTESIAN_POINT('Ctrl Pts',(20.3386623072263,2.7953768385389,36.1989728909579));
#38891=CARTESIAN_POINT('Ctrl Pts',(20.2555894045633,2.80036323486063,36.1860329601209));
#38892=CARTESIAN_POINT('Ctrl Pts',(20.0945206081371,2.81016808452353,36.1716197982785));
#38893=CARTESIAN_POINT('Ctrl Pts',(20.0167612999912,2.81496205283437,36.1693779979842));
#38894=CARTESIAN_POINT('Ctrl Pts',(19.920071811922,2.82111215505278,36.1724326505139));
#38895=CARTESIAN_POINT('Ctrl Pts',(19.9010695584797,2.82232969974099,36.1733144707299));
#38896=CARTESIAN_POINT('Ctrl Pts',(19.8735245838303,2.82410876170631,36.1750012820883));
#38897=CARTESIAN_POINT('Ctrl Pts',(19.8649688967471,2.82466333443581,36.1755825057665));
#38898=CARTESIAN_POINT('Ctrl Pts',(19.849994708311,2.82563753989242,36.1767001140822));
#38899=CARTESIAN_POINT('Ctrl Pts',(19.8435744420332,2.82605639304065,36.177211638831));
#38900=CARTESIAN_POINT('Ctrl Pts',(19.8311241652542,2.82687093507917,36.1782663647949));
#38901=CARTESIAN_POINT('Ctrl Pts',(19.8250939064596,2.82726650249305,36.1788058220782));
#38902=CARTESIAN_POINT('Ctrl Pts',(19.8106979941921,2.82821337809269,36.1801619968691));
#38903=CARTESIAN_POINT('Ctrl Pts',(19.8023349998851,2.82876550072339,36.1810050152163));
#38904=CARTESIAN_POINT('Ctrl Pts',(19.7722151856953,2.83076157986249,36.1842401730162));
#38905=CARTESIAN_POINT('Ctrl Pts',(19.7504946331037,2.83221532017182,36.1869478204954));
#38906=CARTESIAN_POINT('Ctrl Pts',(19.6150531465257,2.84137334453092,36.2061775242916));
#38907=CARTESIAN_POINT('Ctrl Pts',(19.5030370899688,2.84937933430976,36.2324520023598));
#38908=CARTESIAN_POINT('Ctrl Pts',(19.3941039244954,2.85753017062829,36.2684890110654));
#38909=CARTESIAN_POINT('Origin',(20.,-1.3495818343519,38.1));
#38910=CARTESIAN_POINT('',(19.3941042587802,3.8243647438501,36.2684889004781));
#38911=CARTESIAN_POINT('',(19.3941040086362,3.65343403802913,36.2684889832302));
#38912=CARTESIAN_POINT('',(19.3941040087494,-1.3495818343519,36.2684889831927));
#38913=CARTESIAN_POINT('',(18.0708705425584,3.18824125908482,38.0985531651523));
#38914=CARTESIAN_POINT('Ctrl Pts',(19.3941042587802,3.8243647438501,36.2684889004781));
#38915=CARTESIAN_POINT('Ctrl Pts',(19.5025433210666,3.81660121883645,36.2326153717628));
#38916=CARTESIAN_POINT('Ctrl Pts',(19.6139981162338,3.80853747388574,36.2064285893548));
#38917=CARTESIAN_POINT('Ctrl Pts',(19.8481095679091,3.79167443629537,36.1729819420564));
#38918=CARTESIAN_POINT('Ctrl Pts',(19.9704351967536,3.78290655232174,36.1672298042598));
#38919=CARTESIAN_POINT('Ctrl Pts',(20.107006183639,3.77363918350316,36.1737852183773));
#38920=CARTESIAN_POINT('Ctrl Pts',(20.1215127262511,3.77266167470754,36.174645903566));
#38921=CARTESIAN_POINT('Ctrl Pts',(20.1415918807353,3.77131943144695,36.1760650676144));
#38922=CARTESIAN_POINT('Ctrl Pts',(20.1471734234849,3.77094747330308,36.1764839823665));
#38923=CARTESIAN_POINT('Ctrl Pts',(20.1561088410343,3.77035394411287,36.1771937387333));
#38924=CARTESIAN_POINT('Ctrl Pts',(20.159463861605,3.77013152597861,36.1774690728387));
#38925=CARTESIAN_POINT('Ctrl Pts',(20.1664613743643,3.76966856762079,36.1780617762628));
#38926=CARTESIAN_POINT('Ctrl Pts',(20.1701037009248,3.76942812196083,36.1783807202722));
#38927=CARTESIAN_POINT('Ctrl Pts',(20.1789170405876,3.7688475589309,36.1791777237417));
#38928=CARTESIAN_POINT('Ctrl Pts',(20.1840871227174,3.76850802490127,36.1796663161911));
#38929=CARTESIAN_POINT('Ctrl Pts',(20.2022067486207,3.76732149272778,36.1814525392052));
#38930=CARTESIAN_POINT('Ctrl Pts',(20.2151454297398,3.76648038144531,36.1828603611538));
#38931=CARTESIAN_POINT('Ctrl Pts',(20.2927612751864,3.76146644101594,36.1921012164594));
#38932=CARTESIAN_POINT('Ctrl Pts',(20.3570289023945,3.75744650594636,36.2030763991522));
#38933=CARTESIAN_POINT('Ctrl Pts',(20.5019014198875,3.74844009564498,36.2354428835545));
#38934=CARTESIAN_POINT('Ctrl Pts',(20.5819198626719,3.74350314700833,36.2588458980446));
#38935=CARTESIAN_POINT('Ctrl Pts',(20.6899625171287,3.7366202859837,36.2981955957557));
#38936=CARTESIAN_POINT('Ctrl Pts',(20.719475208269,3.73471737891405,36.3097757838709));
#38937=CARTESIAN_POINT('Ctrl Pts',(20.8334108091746,3.72724693098387,36.3577544224452));
#38938=CARTESIAN_POINT('Ctrl Pts',(20.9154638346477,3.72158924801021,36.3994366071388));
#38939=CARTESIAN_POINT('Ctrl Pts',(21.0058030523098,3.71485681565364,36.4537663432116));
#38940=CARTESIAN_POINT('Ctrl Pts',(21.017305550735,3.71398990064518,36.4608494778251));
#38941=CARTESIAN_POINT('Ctrl Pts',(21.0356793735786,3.71258892387703,36.4724318054191));
#38942=CARTESIAN_POINT('Ctrl Pts',(21.0425981413652,3.71205763378613,36.4768551805027));
#38943=CARTESIAN_POINT('Ctrl Pts',(21.0548647146645,3.71110888958743,36.4848083560577));
#38944=CARTESIAN_POINT('Ctrl Pts',(21.0602236050805,3.71069207800875,36.4883209008967));
#38945=CARTESIAN_POINT('Ctrl Pts',(21.0713879324936,3.70981877517561,36.4957184627461));
#38946=CARTESIAN_POINT('Ctrl Pts',(21.0771899560768,3.70936210307275,36.4996084388377));
#38947=CARTESIAN_POINT('Ctrl Pts',(21.0922876465777,3.70816630228019,36.5098500054185));
#38948=CARTESIAN_POINT('Ctrl Pts',(21.1015489553772,3.70742530404474,36.5162515357664));
#38949=CARTESIAN_POINT('Ctrl Pts',(21.1425281534099,3.70411266899588,36.5451101931637));
#38950=CARTESIAN_POINT('Ctrl Pts',(21.1736172330131,3.70150800319788,36.5684403002368));
#38951=CARTESIAN_POINT('Ctrl Pts',(21.2560428001338,3.69434287162441,36.6342786234473));
#38952=CARTESIAN_POINT('Ctrl Pts',(21.3059120722831,3.68971844521503,36.6785307763896));
#38953=CARTESIAN_POINT('Ctrl Pts',(21.4451927637774,3.67595455738178,36.8156492241863));
#38954=CARTESIAN_POINT('Ctrl Pts',(21.5277087359096,3.66664359036591,36.9149922428716));
#38955=CARTESIAN_POINT('Ctrl Pts',(21.6282058439836,3.6540405146561,37.0641001398016));
#38956=CARTESIAN_POINT('Ctrl Pts',(21.655020567939,3.65051920900012,37.1075027733854));
#38957=CARTESIAN_POINT('Ctrl Pts',(21.6839118589527,3.6465731684424,37.1587008922485));
#38958=CARTESIAN_POINT('Ctrl Pts',(21.6876967045008,3.64605294754337,37.1655038803737));
#38959=CARTESIAN_POINT('Ctrl Pts',(21.6936745738103,3.64522623131345,37.1764034528446));
#38960=CARTESIAN_POINT('Ctrl Pts',(21.695894110163,3.64491813520693,37.1804852844453));
#38961=CARTESIAN_POINT('Ctrl Pts',(21.6997976837887,3.64437429253333,37.1877263529914));
#38962=CARTESIAN_POINT('Ctrl Pts',(21.7014877002396,3.64413817319311,37.1908823070664));
#38963=CARTESIAN_POINT('Ctrl Pts',(21.7050580135407,3.64363793982618,37.1975943772408));
#38964=CARTESIAN_POINT('Ctrl Pts',(21.7069359739587,3.6433739720348,37.2011516707111));
#38965=CARTESIAN_POINT('Ctrl Pts',(21.7119973347179,3.64266015736078,37.2108121320031));
#38966=CARTESIAN_POINT('Ctrl Pts',(21.71515925621,3.64221163318699,37.2169265783588));
#38967=CARTESIAN_POINT('Ctrl Pts',(21.7310457212049,3.63994414737874,37.2480546655005));
#38968=CARTESIAN_POINT('Ctrl Pts',(21.7432568432671,3.63815504853951,37.2733284082068));
#38969=CARTESIAN_POINT('Ctrl Pts',(21.7778079793526,3.63292337642989,37.3490134603445));
#38970=CARTESIAN_POINT('Ctrl Pts',(21.798544501222,3.62955207640777,37.4001281502922));
#38971=CARTESIAN_POINT('Ctrl Pts',(21.8593526728616,3.61861456140839,37.570658033933));
#38972=CARTESIAN_POINT('Ctrl Pts',(21.8899291538575,3.61122580694507,37.6931048355494));
#38973=CARTESIAN_POINT('Ctrl Pts',(21.9121862126765,3.60195472760078,37.8435414122052));
#38974=CARTESIAN_POINT('Ctrl Pts',(21.9154884493044,3.60034923090744,37.8694982773877));
#38975=CARTESIAN_POINT('Ctrl Pts',(21.9235738439877,3.59562963942916,37.9453463586235));
#38976=CARTESIAN_POINT('Ctrl Pts',(21.9269417735406,3.59248140563564,37.9953634372041));
#38977=CARTESIAN_POINT('Ctrl Pts',(21.9287167358271,3.58846138683155,38.0581109541955));
#38978=CARTESIAN_POINT('Ctrl Pts',(21.9289501583924,3.58764662366278,38.0707730724771));
#38979=CARTESIAN_POINT('Ctrl Pts',(21.9291221702567,3.58635158223311,38.0908061356981));
#38980=CARTESIAN_POINT('Ctrl Pts',(21.9291432155285,3.58587386548661,38.0981761559781));
#38981=CARTESIAN_POINT('Ctrl Pts',(21.9291037829279,3.58498233913905,38.111892321641));
#38982=CARTESIAN_POINT('Ctrl Pts',(21.9290542219237,3.58456887436756,38.118238418028));
#38983=CARTESIAN_POINT('Ctrl Pts',(21.9288748005464,3.58364941829366,38.1323165894047));
#38984=CARTESIAN_POINT('Ctrl Pts',(21.9287297598687,3.58314296219173,38.140048328313));
#38985=CARTESIAN_POINT('Ctrl Pts',(21.9281740246796,3.58166917862733,38.1624799190289));
#38986=CARTESIAN_POINT('Ctrl Pts',(21.9276417361844,3.58069809842653,38.1771759444177));
#38987=CARTESIAN_POINT('Ctrl Pts',(21.9218660123355,3.5726452998271,38.2983275216931));
#38988=CARTESIAN_POINT('Ctrl Pts',(21.9079772807468,3.56529257211311,38.4041685881899));
#38989=CARTESIAN_POINT('Ctrl Pts',(21.8576451070652,3.54849997592396,38.6365860869335));
#38990=CARTESIAN_POINT('Ctrl Pts',(21.8168470541981,3.53900638468864,38.7616920046678));
#38991=CARTESIAN_POINT('Ctrl Pts',(21.7466282471285,3.5269331584024,38.9201218589893));
#38992=CARTESIAN_POINT('Ctrl Pts',(21.7283392513016,3.52404578659653,38.9579942591744));
#38993=CARTESIAN_POINT('Ctrl Pts',(21.705398770605,3.52073038495009,39.0017827441544));
#38994=CARTESIAN_POINT('Ctrl Pts',(21.7019343905949,3.52023724293405,39.0083041444553));
#38995=CARTESIAN_POINT('Ctrl Pts',(21.6962621799369,3.51944209482291,39.0188351984868));
#38996=CARTESIAN_POINT('Ctrl Pts',(21.6940774159525,3.51913870681818,39.0228570934297));
#38997=CARTESIAN_POINT('Ctrl Pts',(21.6901662994261,3.51860072651248,39.0299963087989));
#38998=CARTESIAN_POINT('Ctrl Pts',(21.6884456063757,3.51836578469834,39.03311665356));
#38999=CARTESIAN_POINT('Ctrl Pts',(21.6847202587229,3.51786087290266,39.0398282404255));
#39000=CARTESIAN_POINT('Ctrl Pts',(21.6827127670511,3.5175910864004,39.0434178374598));
#39001=CARTESIAN_POINT('Ctrl Pts',(21.6771137977364,3.51684489818896,39.0533546302021));
#39002=CARTESIAN_POINT('Ctrl Pts',(21.6734977383796,3.51637003016424,39.059688004126));
#39003=CARTESIAN_POINT('Ctrl Pts',(21.6529227880819,3.51370654926248,39.0952542194193));
#39004=CARTESIAN_POINT('Ctrl Pts',(21.6352327336523,3.51156166116654,39.1240600318223));
#39005=CARTESIAN_POINT('Ctrl Pts',(21.5762624347535,3.50480633402643,39.2146566429716));
#39006=CARTESIAN_POINT('Ctrl Pts',(21.53216428244,3.50032534346411,39.274536988412));
#39007=CARTESIAN_POINT('Ctrl Pts',(21.3804969029989,3.48609968014812,39.4573559849003));
#39008=CARTESIAN_POINT('Ctrl Pts',(21.2607669663413,3.47647053990753,39.5692336949343));
#39009=CARTESIAN_POINT('Ctrl Pts',(21.1114061524359,3.46479194693231,39.6769455292146));
#39010=CARTESIAN_POINT('Ctrl Pts',(21.0942281774938,3.4634544115764,39.6889133012857));
#39011=CARTESIAN_POINT('Ctrl Pts',(21.0700142047057,3.46157509300193,39.7052041065539));
#39012=CARTESIAN_POINT('Ctrl Pts',(21.0631396684544,3.46104221091463,39.7097654064699));
#39013=CARTESIAN_POINT('Ctrl Pts',(21.051203676807,3.46011803690985,39.717575208539));
#39014=CARTESIAN_POINT('Ctrl Pts',(21.0461558594991,3.45972751810159,39.7208444224199));
#39015=CARTESIAN_POINT('Ctrl Pts',(21.0356502455313,3.45891538211942,39.7275788523453));
#39016=CARTESIAN_POINT('Ctrl Pts',(21.0301901588556,3.45849363418281,39.7310403387302));
#39017=CARTESIAN_POINT('Ctrl Pts',(21.0173205799296,3.45750031016147,39.7391087573173));
#39018=CARTESIAN_POINT('Ctrl Pts',(21.0098970775913,3.45692791301771,39.7436929668037));
#39019=CARTESIAN_POINT('Ctrl Pts',(20.985477352857,3.45504671563211,39.7585449162368));
#39020=CARTESIAN_POINT('Ctrl Pts',(20.9683541306402,3.45373029139789,39.7686003356105));
#39021=CARTESIAN_POINT('Ctrl Pts',(20.8777111089287,3.4467732558458,39.8199642812923));
#39022=CARTESIAN_POINT('Ctrl Pts',(20.8017060280256,3.44097314349407,39.8566780890556));
#39023=CARTESIAN_POINT('Ctrl Pts',(20.5989410530765,3.42561412041804,39.9387175233243));
#39024=CARTESIAN_POINT('Ctrl Pts',(20.4694102680866,3.41589133475475,39.97597007301));
#39025=CARTESIAN_POINT('Ctrl Pts',(20.2855653899182,3.40279403552321,40.0085938696197));
#39026=CARTESIAN_POINT('Ctrl Pts',(20.2337112340199,3.3991794484512,40.0156352250331));
#39027=CARTESIAN_POINT('Ctrl Pts',(20.1730817546099,3.39509119298739,40.02136904098));
#39028=CARTESIAN_POINT('Ctrl Pts',(20.1645278671098,3.39451759588833,40.0221204106642));
#39029=CARTESIAN_POINT('Ctrl Pts',(20.1515386303621,3.39365170658775,40.0231740322234));
#39030=CARTESIAN_POINT('Ctrl Pts',(20.1471069217298,3.39335718477633,40.0235180969446));
#39031=CARTESIAN_POINT('Ctrl Pts',(20.1391301544877,3.39282874161915,40.0241096603328));
#39032=CARTESIAN_POINT('Ctrl Pts',(20.1355855859339,3.39259452008685,40.0243626826556));
#39033=CARTESIAN_POINT('Ctrl Pts',(20.1278396708874,3.39208398713389,40.0248941018442));
#39034=CARTESIAN_POINT('Ctrl Pts',(20.1236381158603,3.39180789770246,40.0251685385727));
#39035=CARTESIAN_POINT('Ctrl Pts',(20.1117076468648,3.3910262159495,40.025908593446));
#39036=CARTESIAN_POINT('Ctrl Pts',(20.1039766723116,3.39052240451841,40.0263414456479));
#39037=CARTESIAN_POINT('Ctrl Pts',(20.0544894142823,3.38731362729925,40.0288134136018));
#39038=CARTESIAN_POINT('Ctrl Pts',(20.0126752242087,3.3846761089191,40.0295414551389));
#39039=CARTESIAN_POINT('Ctrl Pts',(19.8682150890163,3.37571760218043,40.0273596187466));
#39040=CARTESIAN_POINT('Ctrl Pts',(19.76584254203,3.36963052880947,40.0176172765035));
#39041=CARTESIAN_POINT('Ctrl Pts',(19.5314299373878,3.35540641149355,39.976247761211));
#39042=CARTESIAN_POINT('Ctrl Pts',(19.401000942513,3.34725290050035,39.9387649279003));
#39043=CARTESIAN_POINT('Ctrl Pts',(19.2628950097487,3.33773860501639,39.8828084621858));
#39044=CARTESIAN_POINT('Ctrl Pts',(19.2502687592799,3.33686063858492,39.8775356060379));
#39045=CARTESIAN_POINT('Ctrl Pts',(19.2301091772033,3.33544524494969,39.8688637480313));
#39046=CARTESIAN_POINT('Ctrl Pts',(19.222539587481,3.33491068294472,39.8655498128344));
#39047=CARTESIAN_POINT('Ctrl Pts',(19.2091317837365,3.33395819025838,39.8595769870236));
#39048=CARTESIAN_POINT('Ctrl Pts',(19.2032850664722,3.3335409201871,39.856937398372));
#39049=CARTESIAN_POINT('Ctrl Pts',(19.1973148407526,3.33311284200173,39.8542061209186));
#39050=CARTESIAN_POINT('Ctrl Pts',(19.1971780071591,3.33310302966088,39.8541435024978));
#39051=CARTESIAN_POINT('Ctrl Pts',(19.196920628429,3.33308457100355,39.8540256832314));
#39052=CARTESIAN_POINT('Ctrl Pts',(19.1968000813616,3.33307592478898,39.8539704858341));
#39053=CARTESIAN_POINT('Ctrl Pts',(19.1965733244084,3.33305965912167,39.8538666276248));
#39054=CARTESIAN_POINT('Ctrl Pts',(19.1964671125088,3.33305203971096,39.853817969251));
#39055=CARTESIAN_POINT('Ctrl Pts',(19.1962673082783,3.33303770497076,39.8537264118891));
#39056=CARTESIAN_POINT('Ctrl Pts',(19.1961737139265,3.33303098964095,39.8536835145818));
#39057=CARTESIAN_POINT('Ctrl Pts',(19.195997634089,3.33301835508762,39.8536027944615));
#39058=CARTESIAN_POINT('Ctrl Pts',(19.1959151464363,3.33301243582085,39.8535649726778));
#39059=CARTESIAN_POINT('Ctrl Pts',(19.1957599543809,3.33300129859176,39.85349380162));
#39060=CARTESIAN_POINT('Ctrl Pts',(19.1956872477326,3.33299608055567,39.8534604528873));
#39061=CARTESIAN_POINT('Ctrl Pts',(19.1955504354527,3.33298626119168,39.8533976901928));
#39062=CARTESIAN_POINT('Ctrl Pts',(19.1954863363428,3.33298166039979,39.8533682804427));
#39063=CARTESIAN_POINT('Ctrl Pts',(19.1953657212189,3.33297300265714,39.8533129321879));
#39064=CARTESIAN_POINT('Ctrl Pts',(19.1953092047704,3.3329689457278,39.8532869944307));
#39065=CARTESIAN_POINT('Ctrl Pts',(19.1951834533378,3.3329599184834,39.8532292744882));
#39066=CARTESIAN_POINT('Ctrl Pts',(19.1951142190453,3.33295494812582,39.8531974909631));
#39067=CARTESIAN_POINT('Ctrl Pts',(19.1949777051892,3.33294514719756,39.8531348114845));
#39068=CARTESIAN_POINT('Ctrl Pts',(19.1949104215934,3.33294031635255,39.8531039139543));
#39069=CARTESIAN_POINT('Ctrl Pts',(19.1947777435711,3.33293078978758,39.8530429771771));
#39070=CARTESIAN_POINT('Ctrl Pts',(19.1947123483465,3.33292609402465,39.8530129378223));
#39071=CARTESIAN_POINT('Ctrl Pts',(19.1945833879339,3.33291683342051,39.8529536910029));
#39072=CARTESIAN_POINT('Ctrl Pts',(19.194519821919,3.33291226853342,39.8529244834023));
#39073=CARTESIAN_POINT('Ctrl Pts',(19.1943944626362,3.332903265607,39.8528668744925));
#39074=CARTESIAN_POINT('Ctrl Pts',(19.1943326685502,3.33289882752165,39.8528384730369));
#39075=CARTESIAN_POINT('Ctrl Pts',(19.1942107983545,3.33289007430297,39.8527824519268));
#39076=CARTESIAN_POINT('Ctrl Pts',(19.1941507210981,3.33288575909927,39.8527548319614));
#39077=CARTESIAN_POINT('Ctrl Pts',(19.1940322345453,3.33287724808706,39.8527003514805));
#39078=CARTESIAN_POINT('Ctrl Pts',(19.193973824156,3.33287305221163,39.8526734906676));
#39079=CARTESIAN_POINT('Ctrl Pts',(19.1938586030765,3.3328647749856,39.8526204977049));
#39080=CARTESIAN_POINT('Ctrl Pts',(19.1938018015442,3.33286069430381,39.8525943699601));
#39081=CARTESIAN_POINT('Ctrl Pts',(19.1936897607892,3.33285264481112,39.852542826507));
#39082=CARTESIAN_POINT('Ctrl Pts',(19.193634521446,3.33284867600164,39.8525174109245));
#39083=CARTESIAN_POINT('Ctrl Pts',(19.1935255569654,3.33284084682734,39.8524672702022));
#39084=CARTESIAN_POINT('Ctrl Pts',(19.1934718317688,3.33283698646777,39.8524425452058));
#39085=CARTESIAN_POINT('Ctrl Pts',(19.19336584887,3.33282937086509,39.852393764666));
#39086=CARTESIAN_POINT('Ctrl Pts',(19.1933135912527,3.33282561563704,39.8523697093228));
#39087=CARTESIAN_POINT('Ctrl Pts',(19.1932104990866,3.33281820713157,39.8523222481176));
#39088=CARTESIAN_POINT('Ctrl Pts',(19.1931596643523,3.33281455384927,39.8522988423222));
#39089=CARTESIAN_POINT('Ctrl Pts',(19.1930593744085,3.33280734613107,39.8522526606156));
#39090=CARTESIAN_POINT('Ctrl Pts',(19.1930099191916,3.33280379170262,39.8522298848443));
#39091=CARTESIAN_POINT('Ctrl Pts',(19.1862562440235,3.33231837458077,39.849119246355));
#39092=CARTESIAN_POINT('Ctrl Pts',(19.1795698800316,3.33183519942183,39.8459929707942));
#39093=CARTESIAN_POINT('Ctrl Pts',(19.1609340160753,3.33048115245289,39.8371489038218));
#39094=CARTESIAN_POINT('Ctrl Pts',(19.1490254109,3.32960737779564,39.8313463758972));
#39095=CARTESIAN_POINT('Ctrl Pts',(19.122513678488,3.32764261494977,39.8180887987205));
#39096=CARTESIAN_POINT('Ctrl Pts',(19.1079440755324,3.32654944694703,39.8105693684809));
#39097=CARTESIAN_POINT('Ctrl Pts',(19.0626998276581,3.32311185895985,39.7864834023164));
#39098=CARTESIAN_POINT('Ctrl Pts',(19.0323786655581,3.32074552658446,39.7692712705601));
#39099=CARTESIAN_POINT('Ctrl Pts',(18.9152349315449,3.31135278730419,39.6985090626837));
#39100=CARTESIAN_POINT('Ctrl Pts',(18.8322578005596,3.3041327295335,39.6389347527952));
#39101=CARTESIAN_POINT('Ctrl Pts',(18.6634585832339,3.28836582766895,39.4962017405979));
#39102=CARTESIAN_POINT('Ctrl Pts',(18.5798357193322,3.27983032609332,39.4110533821716));
#39103=CARTESIAN_POINT('Ctrl Pts',(18.4953586505283,3.27076582689681,39.307398300588));
#39104=CARTESIAN_POINT('Ctrl Pts',(18.4862523798787,3.26978237502493,39.2959617138258));
#39105=CARTESIAN_POINT('Ctrl Pts',(18.4738317434508,3.26843335481722,39.2799934288007));
#39106=CARTESIAN_POINT('Ctrl Pts',(18.4704061092114,3.26806046925801,39.2755494759969));
#39107=CARTESIAN_POINT('Ctrl Pts',(18.4649547370027,3.26746583835805,39.2684134315649));
#39108=CARTESIAN_POINT('Ctrl Pts',(18.4629166103936,3.26724324026399,39.2657309124936));
#39109=CARTESIAN_POINT('Ctrl Pts',(18.4586825288022,3.26678024264511,39.260127735203));
#39110=CARTESIAN_POINT('Ctrl Pts',(18.4564878356473,3.2665399363093,39.2572061647643));
#39111=CARTESIAN_POINT('Ctrl Pts',(18.4512011675586,3.26596026427782,39.2501267673303));
#39112=CARTESIAN_POINT('Ctrl Pts',(18.4481175873644,3.26562147749728,39.2459626447587));
#39113=CARTESIAN_POINT('Ctrl Pts',(18.4373909288732,3.26444037765165,39.2313544712812));
#39114=CARTESIAN_POINT('Ctrl Pts',(18.4298359957502,3.26360387987085,39.2208456943403));
#39115=CARTESIAN_POINT('Ctrl Pts',(18.3852992776554,3.25863936253422,39.157561766277));
#39116=CARTESIAN_POINT('Ctrl Pts',(18.3508711473351,3.25466098733777,39.1030309771968));
#39117=CARTESIAN_POINT('Ctrl Pts',(18.2569194275424,3.24304235477764,38.9362601942));
#39118=CARTESIAN_POINT('Ctrl Pts',(18.2056753856786,3.23560300123534,38.8197651313276));
#39119=CARTESIAN_POINT('Ctrl Pts',(18.1535277955956,3.22540677745552,38.6601433722484));
#39120=CARTESIAN_POINT('Ctrl Pts',(18.1420520435353,3.22289657108618,38.6208160000969));
#39121=CARTESIAN_POINT('Ctrl Pts',(18.1207279500748,3.2175848628011,38.5380216842226));
#39122=CARTESIAN_POINT('Ctrl Pts',(18.1111166947998,3.21477867284623,38.4945197203968));
#39123=CARTESIAN_POINT('Ctrl Pts',(18.1007824823921,3.21113595460981,38.4386249178573));
#39124=CARTESIAN_POINT('Ctrl Pts',(18.0986609354056,3.21034374109631,38.426502318923));
#39125=CARTESIAN_POINT('Ctrl Pts',(18.0954795121904,3.20908115485691,38.407239896711));
#39126=CARTESIAN_POINT('Ctrl Pts',(18.0943434429813,3.20861318319632,38.4001128570536));
#39127=CARTESIAN_POINT('Ctrl Pts',(18.0923780460689,3.20777176754015,38.387321780416));
#39128=CARTESIAN_POINT('Ctrl Pts',(18.0915338824086,3.2073987946462,38.3816600813881));
#39129=CARTESIAN_POINT('Ctrl Pts',(18.0898485791259,3.2066296217493,38.3700014383462));
#39130=CARTESIAN_POINT('Ctrl Pts',(18.0890104537975,3.2062333315492,38.3640041292778));
#39131=CARTESIAN_POINT('Ctrl Pts',(18.0872001154099,3.20534549390767,38.3505895431773));
#39132=CARTESIAN_POINT('Ctrl Pts',(18.0862427852809,3.20485348607942,38.343170388998));
#39133=CARTESIAN_POINT('Ctrl Pts',(18.0839541868887,3.20361832718392,38.3245829479623));
#39134=CARTESIAN_POINT('Ctrl Pts',(18.0826774073341,3.20287348971464,38.3134083527984));
#39135=CARTESIAN_POINT('Ctrl Pts',(18.0743662104803,3.19760127102859,38.2345597038922));
#39136=CARTESIAN_POINT('Ctrl Pts',(18.0708195264918,3.19296679823777,38.1665751630418));
#39137=CARTESIAN_POINT('Ctrl Pts',(18.0708705425584,3.18824125908482,38.0985531651523));
#39138=CARTESIAN_POINT('Ctrl Pts',(18.0708705408095,3.18824142121201,38.0985554989003));
#39139=CARTESIAN_POINT('Ctrl Pts',(18.0709626172183,3.17969875041658,37.9755875671282));
#39140=CARTESIAN_POINT('Ctrl Pts',(18.0828122062449,3.17086948894766,37.8529133384598));
#39141=CARTESIAN_POINT('Ctrl Pts',(18.1210858155559,3.1565976689777,37.6558418696555));
#39142=CARTESIAN_POINT('Ctrl Pts',(18.1405257136007,3.15112172667708,37.5804300173344));
#39143=CARTESIAN_POINT('Ctrl Pts',(18.168849811871,3.14488776678673,37.4928474918395));
#39144=CARTESIAN_POINT('Ctrl Pts',(18.1733798313619,3.14393089377516,37.4793519769664));
#39145=CARTESIAN_POINT('Ctrl Pts',(18.179827744326,3.14262359023829,37.460825161733));
#39146=CARTESIAN_POINT('Ctrl Pts',(18.1816177931501,3.14226615086213,37.4557503079314));
#39147=CARTESIAN_POINT('Ctrl Pts',(18.184672176106,3.14166547475043,37.4472051709506));
#39148=CARTESIAN_POINT('Ctrl Pts',(18.185925273283,3.14142158738759,37.4437309365291));
#39149=CARTESIAN_POINT('Ctrl Pts',(18.1883264429393,3.14095908577815,37.4371330796245));
#39150=CARTESIAN_POINT('Ctrl Pts',(18.1894726289196,3.14074035911772,37.4340088060122));
#39151=CARTESIAN_POINT('Ctrl Pts',(18.1924976491082,3.14016838021045,37.4258287316373));
#39152=CARTESIAN_POINT('Ctrl Pts',(18.1943896283659,3.13981590032939,37.4207777719108));
#39153=CARTESIAN_POINT('Ctrl Pts',(18.2010203899488,3.13859838487663,37.4032993365387));
#39154=CARTESIAN_POINT('Ctrl Pts',(18.2058666191329,3.13773943792469,37.3909126378704));
#39155=CARTESIAN_POINT('Ctrl Pts',(18.2642861115132,3.12772734579599,37.2460299206992));
#39156=CARTESIAN_POINT('Ctrl Pts',(18.3323038746261,3.11932527790169,37.1198111357329));
#39157=CARTESIAN_POINT('Ctrl Pts',(18.4553914536909,3.1063880510586,36.9419383734885));
#39158=CARTESIAN_POINT('Ctrl Pts',(18.5005321590342,3.10197762000265,36.884056965834));
#39159=CARTESIAN_POINT('Ctrl Pts',(18.5743967845471,3.09507801435943,36.7997305790491));
#39160=CARTESIAN_POINT('Ctrl Pts',(18.6008092646648,3.09266561422367,36.771350275337));
#39161=CARTESIAN_POINT('Ctrl Pts',(18.6404864019471,3.0891032463412,36.7312129838761));
#39162=CARTESIAN_POINT('Ctrl Pts',(18.6530872805532,3.08798046085748,36.7188116663069));
#39163=CARTESIAN_POINT('Ctrl Pts',(18.6759971329724,3.08595285232503,36.6968763178888));
#39164=CARTESIAN_POINT('Ctrl Pts',(18.6862432204556,3.08505080543691,36.687278241609));
#39165=CARTESIAN_POINT('Ctrl Pts',(18.7021770857202,3.08365477265673,36.6726753650743));
#39166=CARTESIAN_POINT('Ctrl Pts',(18.7077912551356,3.08316415732544,36.667590670481));
#39167=CARTESIAN_POINT('Ctrl Pts',(18.7134723617415,3.08266891377676,36.6625059320505));
#39168=CARTESIAN_POINT('Ctrl Pts',(18.7135095662566,3.08266567057094,36.6624726356415));
#39169=CARTESIAN_POINT('Ctrl Pts',(18.7135862850425,3.08265898292055,36.662403981057));
#39170=CARTESIAN_POINT('Ctrl Pts',(18.7136257994007,3.08265553847507,36.6623686231359));
#39171=CARTESIAN_POINT('Ctrl Pts',(18.7137073067292,3.08264843364679,36.6622956954529));
#39172=CARTESIAN_POINT('Ctrl Pts',(18.7137492998584,3.08264477325779,36.662258125928));
#39173=CARTESIAN_POINT('Ctrl Pts',(18.7138359488241,3.08263722051897,36.662180611498));
#39174=CARTESIAN_POINT('Ctrl Pts',(18.7138806049412,3.0826333281534,36.6621406667746));
#39175=CARTESIAN_POINT('Ctrl Pts',(18.7139727813229,3.08262529393003,36.662058223089));
#39176=CARTESIAN_POINT('Ctrl Pts',(18.7140203018249,3.08262115206151,36.6620157244094));
#39177=CARTESIAN_POINT('Ctrl Pts',(18.7141184275495,3.08261259963772,36.6619279770677));
#39178=CARTESIAN_POINT('Ctrl Pts',(18.7141690329902,3.08260818907488,36.661882728778));
#39179=CARTESIAN_POINT('Ctrl Pts',(18.7142735703587,3.08259907822612,36.6617892677862));
#39180=CARTESIAN_POINT('Ctrl Pts',(18.7143275026305,3.08259437792334,36.6617410554282));
#39181=CARTESIAN_POINT('Ctrl Pts',(18.7144389594826,3.08258466446811,36.6616414306731));
#39182=CARTESIAN_POINT('Ctrl Pts',(18.7144964844927,3.08257965129328,36.6615900186419));
#39183=CARTESIAN_POINT('Ctrl Pts',(18.7146154197221,3.08256928661462,36.6614837350708));
#39184=CARTESIAN_POINT('Ctrl Pts',(18.7146768304129,3.08256393508711,36.6614288639749));
#39185=CARTESIAN_POINT('Ctrl Pts',(18.7148038603794,3.08255286557648,36.6613153759958));
#39186=CARTESIAN_POINT('Ctrl Pts',(18.7148694801646,3.0825471475691,36.6612567596582));
#39187=CARTESIAN_POINT('Ctrl Pts',(18.7150052862623,3.08253531396997,36.6611354645343));
#39188=CARTESIAN_POINT('Ctrl Pts',(18.7150754730873,3.08252919835688,36.6610727864506));
#39189=CARTESIAN_POINT('Ctrl Pts',(18.7152208101716,3.08251653503415,36.6609430169612));
#39190=CARTESIAN_POINT('Ctrl Pts',(18.7152959610692,3.082509987296,36.6608759263345));
#39191=CARTESIAN_POINT('Ctrl Pts',(18.7154516675819,3.08249642135833,36.6607369419596));
#39192=CARTESIAN_POINT('Ctrl Pts',(18.7155322240176,3.08248940311891,36.6606650490519));
#39193=CARTESIAN_POINT('Ctrl Pts',(18.7156992338346,3.08247485339189,36.660516025671));
#39194=CARTESIAN_POINT('Ctrl Pts',(18.7157856881107,3.08246732186327,36.6604388962389));
#39195=CARTESIAN_POINT('Ctrl Pts',(18.7159650437198,3.08245169774806,36.6602789147041));
#39196=CARTESIAN_POINT('Ctrl Pts',(18.7160579461528,3.08244360510896,36.6601960637789));
#39197=CARTESIAN_POINT('Ctrl Pts',(18.7162508149785,3.08242680516823,36.66002409576));
#39198=CARTESIAN_POINT('Ctrl Pts',(18.7163507826064,3.08241809780997,36.6599349801068));
#39199=CARTESIAN_POINT('Ctrl Pts',(18.7165584754023,3.08240000817572,36.6597498721897));
#39200=CARTESIAN_POINT('Ctrl Pts',(18.7166662020305,3.08239062583273,36.6596538816284));
#39201=CARTESIAN_POINT('Ctrl Pts',(18.7168587458894,3.08237385719388,36.6594823528331));
#39202=CARTESIAN_POINT('Ctrl Pts',(18.7169435590601,3.0823664710863,36.6594068099702));
#39203=CARTESIAN_POINT('Ctrl Pts',(18.7171507824376,3.0823484253228,36.6592222694792));
#39204=CARTESIAN_POINT('Ctrl Pts',(18.717273203459,3.08233776501619,36.6591132767623));
#39205=CARTESIAN_POINT('Ctrl Pts',(18.7175738838384,3.08231158342707,36.6588456465641));
#39206=CARTESIAN_POINT('Ctrl Pts',(18.717752156434,3.08229606161821,36.6586870286051));
#39207=CARTESIAN_POINT('Ctrl Pts',(18.7227175746267,3.08186376638179,36.6542707004457));
#39208=CARTESIAN_POINT('Ctrl Pts',(18.7275258218925,3.08144600778244,36.6500368742098));
#39209=CARTESIAN_POINT('Ctrl Pts',(18.7385405675419,3.08049088779077,36.6404349986686));
#39210=CARTESIAN_POINT('Ctrl Pts',(18.7447603728366,3.07995289873603,36.6350824706683));
#39211=CARTESIAN_POINT('Ctrl Pts',(18.7612933087796,3.07852629012478,36.6210374555612));
#39212=CARTESIAN_POINT('Ctrl Pts',(18.7716636290791,3.07763492672971,36.6124132902688));
#39213=CARTESIAN_POINT('Ctrl Pts',(18.8514254742044,3.07080422851566,36.5474844678337));
#39214=CARTESIAN_POINT('Ctrl Pts',(18.924553176691,3.06467716519431,36.4959620137343));
#39215=CARTESIAN_POINT('Ctrl Pts',(19.1248584470688,3.04825373440208,36.3747058490964));
#39216=CARTESIAN_POINT('Ctrl Pts',(19.2567338464206,3.03775841435496,36.3139334439782));
#39217=CARTESIAN_POINT('Ctrl Pts',(19.3941040093468,3.02765621357216,36.2684889829951));
#39218=CARTESIAN_POINT('Ctrl Pts',(19.3941039244954,2.85753017062829,36.2684890110654));
#39219=CARTESIAN_POINT('Ctrl Pts',(19.3606565940364,2.86003284017505,36.2795539767597));
#39220=CARTESIAN_POINT('Ctrl Pts',(19.3274997762525,2.86254735914615,36.291539331038));
#39221=CARTESIAN_POINT('Ctrl Pts',(19.217090903976,2.87101193801834,36.3349098074678));
#39222=CARTESIAN_POINT('Ctrl Pts',(19.1415620849291,2.87695947541409,36.3703826759163));
#39223=CARTESIAN_POINT('Ctrl Pts',(19.0369204836252,2.88524193442019,36.4280771993552));
#39224=CARTESIAN_POINT('Ctrl Pts',(19.0057737880163,2.88771226505888,36.4464091623806));
#39225=CARTESIAN_POINT('Ctrl Pts',(18.9688575436691,2.89063021769136,36.4695573921715));
#39226=CARTESIAN_POINT('Ctrl Pts',(18.9625797377048,2.8911260707425,36.4735446312671));
#39227=CARTESIAN_POINT('Ctrl Pts',(18.9528396766222,2.89189463614446,36.4798101998695));
#39228=CARTESIAN_POINT('Ctrl Pts',(18.9493615242401,2.89216893803576,36.4820634977358));
#39229=CARTESIAN_POINT('Ctrl Pts',(18.942909585528,2.892677444386,36.4862729221553));
#39230=CARTESIAN_POINT('Ctrl Pts',(18.939933979045,2.89291183305399,36.4882260525492));
#39231=CARTESIAN_POINT('Ctrl Pts',(18.933182269606,2.8934433820139,36.4926845294928));
#39232=CARTESIAN_POINT('Ctrl Pts',(18.9294095840057,2.89374020034283,36.4951949483408));
#39233=CARTESIAN_POINT('Ctrl Pts',(18.9179241961722,2.89464332956517,36.5028960774762));
#39234=CARTESIAN_POINT('Ctrl Pts',(18.9102399994164,2.89524688189357,36.5081293601266));
#39235=CARTESIAN_POINT('Ctrl Pts',(18.8388727186767,2.90084906322997,36.5574926490255));
#39236=CARTESIAN_POINT('Ctrl Pts',(18.7778561464931,2.90561493726354,36.6053719517119));
#39237=CARTESIAN_POINT('Ctrl Pts',(18.6412756796865,2.91665279091833,36.7265189500819));
#39238=CARTESIAN_POINT('Ctrl Pts',(18.5684994543961,2.92284534630685,36.802545196496));
#39239=CARTESIAN_POINT('Ctrl Pts',(18.4619008066149,2.93305337383519,36.9338538260545));
#39240=CARTESIAN_POINT('Ctrl Pts',(18.4240317057074,2.93696623387303,36.9855633991839));
#39241=CARTESIAN_POINT('Ctrl Pts',(18.3680051820332,2.94333261595461,37.0706477270633));
#39242=CARTESIAN_POINT('Ctrl Pts',(18.348138474401,2.94572578419467,37.1028408433733));
#39243=CARTESIAN_POINT('Ctrl Pts',(18.3236564332125,2.94886929523905,37.1452543884238));
#39244=CARTESIAN_POINT('Ctrl Pts',(18.3181650374371,2.94958809106539,37.1549613304519));
#39245=CARTESIAN_POINT('Ctrl Pts',(18.309382863252,2.95076047560509,37.1708042597458));
#39246=CARTESIAN_POINT('Ctrl Pts',(18.3060405412513,2.95121222798076,37.1769115011092));
#39247=CARTESIAN_POINT('Ctrl Pts',(18.2996823790901,2.95208246985336,37.188680247262));
#39248=CARTESIAN_POINT('Ctrl Pts',(18.2966615697999,2.9525007767508,37.1943389738711));
#39249=CARTESIAN_POINT('Ctrl Pts',(18.2898152521597,2.95346007202808,37.2073192484962));
#39250=CARTESIAN_POINT('Ctrl Pts',(18.28600845766,2.95400170734519,37.2146504729416));
#39251=CARTESIAN_POINT('Ctrl Pts',(18.276025428328,2.95544435569914,37.2341817636596));
#39252=CARTESIAN_POINT('Ctrl Pts',(18.2699317166256,2.95634821223243,37.2464232543445));
#39253=CARTESIAN_POINT('Ctrl Pts',(18.2206881797153,2.96384976562581,37.3480412096713));
#39254=CARTESIAN_POINT('Ctrl Pts',(18.1843712913556,2.97068114028936,37.4405461961855));
#39255=CARTESIAN_POINT('Ctrl Pts',(18.1283939640001,2.98415466143783,37.6234425681543));
#39256=CARTESIAN_POINT('Ctrl Pts',(18.1077895144003,2.99075596854252,37.7132773812141));
#39257=CARTESIAN_POINT('Ctrl Pts',(18.0894152127722,2.99927813992268,37.8317068334954));
#39258=CARTESIAN_POINT('Ctrl Pts',(18.0857471412592,3.00124835183975,37.8592687770811));
#39259=CARTESIAN_POINT('Ctrl Pts',(18.0766766357657,3.00702870372052,37.9408791946194));
#39260=CARTESIAN_POINT('Ctrl Pts',(18.0729588246628,3.01080012689968,37.9950921738115));
#39261=CARTESIAN_POINT('Ctrl Pts',(18.0712230541167,3.01526575877315,38.0612387957881));
#39262=CARTESIAN_POINT('Ctrl Pts',(18.07102136121,3.01606024452581,38.0730859472011));
#39263=CARTESIAN_POINT('Ctrl Pts',(18.0708897744506,3.01718189750547,38.0899351242414));
#39264=CARTESIAN_POINT('Ctrl Pts',(18.0708701650209,3.01751376283918,38.0949358885933));
#39265=CARTESIAN_POINT('Ctrl Pts',(18.0708698822856,3.01808411229999,38.1035581921408));
#39266=CARTESIAN_POINT('Ctrl Pts',(18.0708799610129,3.01832310323502,38.107179684489));
#39267=CARTESIAN_POINT('Ctrl Pts',(18.0709220493142,3.01881797255005,38.1146966758045));
#39268=CARTESIAN_POINT('Ctrl Pts',(18.0709556599471,3.01907376149468,38.118592118772));
#39269=CARTESIAN_POINT('Ctrl Pts',(18.0710746585202,3.0197423732211,38.1287999393209));
#39270=CARTESIAN_POINT('Ctrl Pts',(18.0711792328244,3.02015414569974,38.1351121109923));
#39271=CARTESIAN_POINT('Ctrl Pts',(18.0717819535514,3.02197780612953,38.1631747124895));
#39272=CARTESIAN_POINT('Ctrl Pts',(18.0726170531775,3.0233720777768,38.1849173283251));
#39273=CARTESIAN_POINT('Ctrl Pts',(18.0759119799343,3.02714858187199,38.2444305307918));
#39274=CARTESIAN_POINT('Ctrl Pts',(18.079115810438,3.02949823566847,38.2821515514698));
#39275=CARTESIAN_POINT('Ctrl Pts',(18.0939605533097,3.03748445652043,38.4116178669593));
#39276=CARTESIAN_POINT('Ctrl Pts',(18.1110848353842,3.04296581959771,38.5026082776116));
#39277=CARTESIAN_POINT('Ctrl Pts',(18.1678688506281,3.05627763384533,38.7178843701909));
#39278=CARTESIAN_POINT('Ctrl Pts',(18.2137147134431,3.06413886766502,38.8400430351));
#39279=CARTESIAN_POINT('Ctrl Pts',(18.2776273340055,3.07332731941447,38.9690023519358));
#39280=CARTESIAN_POINT('Ctrl Pts',(18.2838825347054,3.07421198771667,38.9812908247222));
#39281=CARTESIAN_POINT('Ctrl Pts',(18.2941104295105,3.07563611745089,39.0008618787903));
#39282=CARTESIAN_POINT('Ctrl Pts',(18.2979993733752,3.07617265626179,39.0081878741759));
#39283=CARTESIAN_POINT('Ctrl Pts',(18.3049818771035,3.07712742112649,39.0211391486641));
#39284=CARTESIAN_POINT('Ctrl Pts',(18.3080565194163,3.07754497562069,39.0267745275963));
#39285=CARTESIAN_POINT('Ctrl Pts',(18.3145166126529,3.07841644298993,39.0384756586106));
#39286=CARTESIAN_POINT('Ctrl Pts',(18.3179068081447,3.07887051990703,39.0445386718518));
#39287=CARTESIAN_POINT('Ctrl Pts',(18.326790392616,3.08005206612961,39.0602265257058));
#39288=CARTESIAN_POINT('Ctrl Pts',(18.3323340424217,3.08078132343595,39.0698224663245));
#39289=CARTESIAN_POINT('Ctrl Pts',(18.356818837048,3.08396810926838,39.1113743937927));
#39290=CARTESIAN_POINT('Ctrl Pts',(18.3765969939247,3.08645565417387,39.1428254195511));
#39291=CARTESIAN_POINT('Ctrl Pts',(18.4320071721571,3.09320842091878,39.2255383624308));
#39292=CARTESIAN_POINT('Ctrl Pts',(18.4692375184685,3.09752884194965,39.2756713045008));
#39293=CARTESIAN_POINT('Ctrl Pts',(18.5959967078172,3.11156251566992,39.4301107518972));
#39294=CARTESIAN_POINT('Ctrl Pts',(18.6942546102255,3.12150813881917,39.5266906211271));
#39295=CARTESIAN_POINT('Ctrl Pts',(18.8118494723276,3.13201024246337,39.6198687195273));
#39296=CARTESIAN_POINT('Ctrl Pts',(18.8218421960231,3.13289243296248,39.6276278351887));
#39297=CARTESIAN_POINT('Ctrl Pts',(18.8615795268422,3.13635838779042,39.6578610831623));
#39298=CARTESIAN_POINT('Ctrl Pts',(18.8918988828837,3.13891087913397,39.6795710458001));
#39299=CARTESIAN_POINT('Ctrl Pts',(18.9287491881109,3.14188839636503,39.7043737568169));
#39300=CARTESIAN_POINT('Ctrl Pts',(18.9346898163073,3.14236463810694,39.7083244914924));
#39301=CARTESIAN_POINT('Ctrl Pts',(18.9444141773534,3.14313791895853,39.7147140270134));
#39302=CARTESIAN_POINT('Ctrl Pts',(18.9481847049677,3.14343622135924,39.7171726574992));
#39303=CARTESIAN_POINT('Ctrl Pts',(18.9549502058018,3.14396868716129,39.7215505348805));
#39304=CARTESIAN_POINT('Ctrl Pts',(18.9579419022527,3.14420317184882,39.7234747091133));
#39305=CARTESIAN_POINT('Ctrl Pts',(18.9644493866687,3.14471110848823,39.7276347388192));
#39306=CARTESIAN_POINT('Ctrl Pts',(18.9679670926901,3.14498435562395,39.7298674776873));
#39307=CARTESIAN_POINT('Ctrl Pts',(18.9778701396599,3.1457499689596,39.736108169004));
#39308=CARTESIAN_POINT('Ctrl Pts',(18.984271867837,3.1462406682692,39.740090167696));
#39309=CARTESIAN_POINT('Ctrl Pts',(19.0230029439931,3.14918511777159,39.7638678879222));
#39310=CARTESIAN_POINT('Ctrl Pts',(19.0558892159563,3.15158359635412,39.7827462338069));
#39311=CARTESIAN_POINT('Ctrl Pts',(19.2373648379795,3.16439516233087,39.8799255526703));
#39312=CARTESIAN_POINT('Ctrl Pts',(19.3951456018111,3.17408508161758,39.9395405972609));
#39313=CARTESIAN_POINT('Ctrl Pts',(19.5950314304877,3.18658919610805,39.9865148925349));
#39314=CARTESIAN_POINT('Ctrl Pts',(19.6316350870102,3.18888475112402,39.9940023886546));
#39315=CARTESIAN_POINT('Ctrl Pts',(19.7102353174229,3.19384976857441,40.0077158410235));
#39316=CARTESIAN_POINT('Ctrl Pts',(19.7522655753833,3.19652629059773,40.0136275852931));
#39317=CARTESIAN_POINT('Ctrl Pts',(19.8064844367045,3.20002178832332,40.0194375922835));
#39318=CARTESIAN_POINT('Ctrl Pts',(19.8185262460074,3.20080079419798,40.0206134982633));
#39319=CARTESIAN_POINT('Ctrl Pts',(19.8377216143814,3.20204715013185,40.0223058312568));
#39320=CARTESIAN_POINT('Ctrl Pts',(19.8448685024871,3.20251220527648,40.0228957848792));
#39321=CARTESIAN_POINT('Ctrl Pts',(19.8577316769104,3.20335110410796,40.0238854216106));
#39322=CARTESIAN_POINT('Ctrl Pts',(19.8634467968227,3.20372449420392,40.0242995122275));
#39323=CARTESIAN_POINT('Ctrl Pts',(19.8768527272242,3.20460195704782,40.0252108200386));
#39324=CARTESIAN_POINT('Ctrl Pts',(19.8845447963421,3.20510666537722,40.0256874215289));
#39325=CARTESIAN_POINT('Ctrl Pts',(19.906796583996,3.2065703811387,40.0269323429763));
#39326=CARTESIAN_POINT('Ctrl Pts',(19.9213621617662,3.20753306285815,40.0275816978332));
#39327=CARTESIAN_POINT('Ctrl Pts',(20.0370742272766,3.21521864588983,40.0314266298124));
#39328=CARTESIAN_POINT('Ctrl Pts',(20.1383057442437,3.22218461519501,40.0268235137575));
#39329=CARTESIAN_POINT('Ctrl Pts',(20.3575865011105,3.23775651747657,39.9994813268921));
#39330=CARTESIAN_POINT('Ctrl Pts',(20.4748322496389,3.24639959752661,39.9736142241968));
#39331=CARTESIAN_POINT('Ctrl Pts',(20.6003917854264,3.25567756394384,39.9333623264736));
#39332=CARTESIAN_POINT('Ctrl Pts',(20.6118303366539,3.25652278487469,39.9295768267147));
#39333=CARTESIAN_POINT('Ctrl Pts',(20.6673239656198,3.26062114142124,39.9106329973402));
#39334=CARTESIAN_POINT('Ctrl Pts',(20.710859670402,3.2638298946142,39.8939878679183));
#39335=CARTESIAN_POINT('Ctrl Pts',(20.7607557653881,3.26746699746689,39.8728088125102));
#39336=CARTESIAN_POINT('Ctrl Pts',(20.7677403915589,3.2679751838393,39.8697952186996));
#39337=CARTESIAN_POINT('Ctrl Pts',(20.7789144816431,3.26878645291078,39.8648954338632));
#39338=CARTESIAN_POINT('Ctrl Pts',(20.7831152646312,3.26909104581512,39.8630354918629));
#39339=CARTESIAN_POINT('Ctrl Pts',(20.7905715975828,3.26963093854884,39.8597022118905));
#39340=CARTESIAN_POINT('Ctrl Pts',(20.7938297421493,3.26986659222329,39.8582348155809));
#39341=CARTESIAN_POINT('Ctrl Pts',(20.8007748522966,3.27036834685185,39.8550836506415));
#39342=CARTESIAN_POINT('Ctrl Pts',(20.8044605884069,3.27063428870413,39.8533973158611));
#39343=CARTESIAN_POINT('Ctrl Pts',(20.8145170219371,3.27135905557493,39.8487578116812));
#39344=CARTESIAN_POINT('Ctrl Pts',(20.820877031485,3.2718164880243,39.8457814198315));
#39345=CARTESIAN_POINT('Ctrl Pts',(20.8542038708978,3.27420928072242,39.829962551754));
#39346=CARTESIAN_POINT('Ctrl Pts',(20.8808877082171,3.27611069433907,39.8165289883437));
#39347=CARTESIAN_POINT('Ctrl Pts',(21.0503796740883,3.28816318876497,39.7262068387402));
#39348=CARTESIAN_POINT('Ctrl Pts',(21.1833339428641,3.29754861330043,39.6321812574369));
#39349=CARTESIAN_POINT('Ctrl Pts',(21.368990712367,3.31277746034923,39.462139432262));
#39350=CARTESIAN_POINT('Ctrl Pts',(21.4307202180323,3.31829438936203,39.3971491521977));
#39351=CARTESIAN_POINT('Ctrl Pts',(21.4962705972888,3.32487084475763,39.3177428700691));
#39352=CARTESIAN_POINT('Ctrl Pts',(21.5047227649264,3.32573391964674,39.3072832244121));
#39353=CARTESIAN_POINT('Ctrl Pts',(21.5181479012924,3.32712988330401,39.2903094762243));
#39354=CARTESIAN_POINT('Ctrl Pts',(21.5231900190743,3.32766003256288,39.2838504389381));
#39355=CARTESIAN_POINT('Ctrl Pts',(21.5320997429895,3.32860747302606,39.2722857832726));
#39356=CARTESIAN_POINT('Ctrl Pts',(21.5359833825756,3.32902412799145,39.2671926263201));
#39357=CARTESIAN_POINT('Ctrl Pts',(21.5440547353663,3.32989785572525,39.2564974922133));
#39358=CARTESIAN_POINT('Ctrl Pts',(21.5482374831827,3.3303551130889,39.2508919014435));
#39359=CARTESIAN_POINT('Ctrl Pts',(21.5590969714671,3.3315541306618,39.2361720111342));
#39360=CARTESIAN_POINT('Ctrl Pts',(21.5657242102423,3.3322977790176,39.2270216917204));
#39361=CARTESIAN_POINT('Ctrl Pts',(21.5950201538103,3.33563956212094,39.1858152331914));
#39362=CARTESIAN_POINT('Ctrl Pts',(21.6167860662026,3.33827144585541,39.1531317331278));
#39363=CARTESIAN_POINT('Ctrl Pts',(21.7241729661074,3.35207317478636,38.9806972879289));
#39364=CARTESIAN_POINT('Ctrl Pts',(21.792716199008,3.36384821357922,38.8311298154114));
#39365=CARTESIAN_POINT('Ctrl Pts',(21.8656912555979,3.38124435133031,38.5973109541305));
#39366=CARTESIAN_POINT('Ctrl Pts',(21.8849528545098,3.38693818482651,38.5184232493386));
#39367=CARTESIAN_POINT('Ctrl Pts',(21.9008291882576,3.393018358466,38.4293600797896));
#39368=CARTESIAN_POINT('Ctrl Pts',(21.9024004326275,3.393642326996,38.4201597532931));
#39369=CARTESIAN_POINT('Ctrl Pts',(21.9046364626845,3.39456437833259,38.4064687620989));
#39370=CARTESIAN_POINT('Ctrl Pts',(21.9053522425979,3.39486520157069,38.401986737793));
#39371=CARTESIAN_POINT('Ctrl Pts',(21.9066012054349,3.39540038691316,38.3939848185075));
#39372=CARTESIAN_POINT('Ctrl Pts',(21.9071404684264,3.39563508431498,38.3904659437615));
#39373=CARTESIAN_POINT('Ctrl Pts',(21.9082856586623,3.39614145866971,38.3828524944419));
#39374=CARTESIAN_POINT('Ctrl Pts',(21.9088881488409,3.39641294161807,38.3787574656925));
#39375=CARTESIAN_POINT('Ctrl Pts',(21.9105329131224,3.39716863498561,38.3673228381058));
#39376=CARTESIAN_POINT('Ctrl Pts',(21.9115460815999,3.39765124716439,38.3599790263823));
#39377=CARTESIAN_POINT('Ctrl Pts',(21.9171965677959,3.40044749505698,38.3172023349757));
#39378=CARTESIAN_POINT('Ctrl Pts',(21.9208913192791,3.40271212805838,38.2816492978243));
#39379=CARTESIAN_POINT('Ctrl Pts',(21.929784166013,3.4100401041277,38.1644924340166));
#39380=CARTESIAN_POINT('Ctrl Pts',(21.9307841933275,3.41494743721398,38.0826553543596));
#39381=CARTESIAN_POINT('Ctrl Pts',(21.918766757882,3.42894686422972,37.8488000130439));
#39382=CARTESIAN_POINT('Ctrl Pts',(21.8929412888471,3.43798567802056,37.6980866919558));
#39383=CARTESIAN_POINT('Ctrl Pts',(21.8434727859557,3.44902021139449,37.5311200991605));
#39384=CARTESIAN_POINT('Ctrl Pts',(21.8369375769129,3.45040992751758,37.5103589806116));
#39385=CARTESIAN_POINT('Ctrl Pts',(21.8273997796909,3.45235087965272,37.4817581967076));
#39386=CARTESIAN_POINT('Ctrl Pts',(21.8246950267113,3.45289241822277,37.4738203628228));
#39387=CARTESIAN_POINT('Ctrl Pts',(21.8199502567549,3.45382752121336,37.4601873604978));
#39388=CARTESIAN_POINT('Ctrl Pts',(21.8179350321529,3.45422026836438,37.4544836421762));
#39389=CARTESIAN_POINT('Ctrl Pts',(21.8137179363228,3.45503318827303,37.4427243177723));
#39390=CARTESIAN_POINT('Ctrl Pts',(21.8115124883044,3.45545347483833,37.4366700835791));
#39391=CARTESIAN_POINT('Ctrl Pts',(21.8062950554161,3.45643663635152,37.4225676606151));
#39392=CARTESIAN_POINT('Ctrl Pts',(21.8032595617032,3.45700028419012,37.4145283734796));
#39393=CARTESIAN_POINT('Ctrl Pts',(21.7932968783317,3.45882391198117,37.3886671180075));
#39394=CARTESIAN_POINT('Ctrl Pts',(21.7861585833522,3.4600908843147,37.3709282384805));
#39395=CARTESIAN_POINT('Ctrl Pts',(21.7483754508612,3.46660414451008,37.2809229456293));
#39396=CARTESIAN_POINT('Ctrl Pts',(21.7136079033426,3.47198792406805,37.2104781801012));
#39397=CARTESIAN_POINT('Ctrl Pts',(21.6332505120093,3.48331934721461,37.0699559286707));
#39398=CARTESIAN_POINT('Ctrl Pts',(21.5872008859281,3.48926990723426,37.0003228609735));
#39399=CARTESIAN_POINT('Ctrl Pts',(21.4706451992611,3.50302697117811,36.8467160860199));
#39400=CARTESIAN_POINT('Ctrl Pts',(21.397190430497,3.51081236917967,36.7653155435785));
#39401=CARTESIAN_POINT('Ctrl Pts',(21.3105229159966,3.51878263051532,36.6843177365225));
#39402=CARTESIAN_POINT('Ctrl Pts',(21.3037810629325,3.519395333194,36.6781063567993));
#39403=CARTESIAN_POINT('Ctrl Pts',(21.2936596427981,3.52030401011307,36.6689138436782));
#39404=CARTESIAN_POINT('Ctrl Pts',(21.290313611638,3.52060261254146,36.6658962231185));
#39405=CARTESIAN_POINT('Ctrl Pts',(21.2843069233402,3.52113540054059,36.6605171281088));
#39406=CARTESIAN_POINT('Ctrl Pts',(21.2816502880951,3.52136990906736,36.6581512730098));
#39407=CARTESIAN_POINT('Ctrl Pts',(21.2758704535842,3.52187765304127,36.6530326632327));
#39408=CARTESIAN_POINT('Ctrl Pts',(21.2727448907782,3.52215068498439,36.650282671757));
#39409=CARTESIAN_POINT('Ctrl Pts',(21.2639458820651,3.52291508614333,36.6425913518342));
#39410=CARTESIAN_POINT('Ctrl Pts',(21.2582523196022,3.52340479692815,36.6376729964587));
#39411=CARTESIAN_POINT('Ctrl Pts',(21.2239073391883,3.52633056760956,36.6083533628937));
#39412=CARTESIAN_POINT('Ctrl Pts',(21.1945734436347,3.52871216800814,36.5847595545678));
#39413=CARTESIAN_POINT('Ctrl Pts',(21.0331277234954,3.54131866137796,36.4625107149812));
#39414=CARTESIAN_POINT('Ctrl Pts',(20.8894641921953,3.55084323614717,36.3802360006423));
#39415=CARTESIAN_POINT('Ctrl Pts',(20.6642805108857,3.56565781676785,36.2871352227005));
#39416=CARTESIAN_POINT('Ctrl Pts',(20.5897198160718,3.57053650479522,36.2615290164322));
#39417=CARTESIAN_POINT('Ctrl Pts',(20.5011492577656,3.57640794543208,36.2370548903965));
#39418=CARTESIAN_POINT('Ctrl Pts',(20.4884545017127,3.57725115478762,36.2336861876901));
#39419=CARTESIAN_POINT('Ctrl Pts',(20.4677906724299,3.57862682006475,36.2284280670368));
#39420=CARTESIAN_POINT('Ctrl Pts',(20.4598420855925,3.57915673395525,36.2264592701559));
#39421=CARTESIAN_POINT('Ctrl Pts',(20.4456725551757,3.58010281668604,36.2230452011473));
#39422=CARTESIAN_POINT('Ctrl Pts',(20.4394564787172,3.58051834554433,36.2215800935219));
#39423=CARTESIAN_POINT('Ctrl Pts',(20.426346663231,3.58139578418474,36.2185587906178));
#39424=CARTESIAN_POINT('Ctrl Pts',(20.4194514319023,3.58185790900996,36.2170095603926));
#39425=CARTESIAN_POINT('Ctrl Pts',(20.401188663845,3.58308363503248,36.2130115449745));
#39426=CARTESIAN_POINT('Ctrl Pts',(20.3898073719483,3.58384928145929,36.210627623742));
#39427=CARTESIAN_POINT('Ctrl Pts',(20.3365028435584,3.58744402788592,36.1999646106391));
#39428=CARTESIAN_POINT('Ctrl Pts',(20.2943363829374,3.590313478552,36.1929776484724));
#39429=CARTESIAN_POINT('Ctrl Pts',(20.0866916685304,3.60458156266655,36.1656215506618));
#39430=CARTESIAN_POINT('Ctrl Pts',(19.919300113629,3.6165942432145,36.1653669394137));
#39431=CARTESIAN_POINT('Ctrl Pts',(19.7245752579247,3.63050769669728,36.1904021273118));
#39432=CARTESIAN_POINT('Ctrl Pts',(19.6952383133604,3.63259952211904,36.1948639784605));
#39433=CARTESIAN_POINT('Ctrl Pts',(19.6207342097879,3.63788445187441,36.2079604331612));
#39434=CARTESIAN_POINT('Ctrl Pts',(19.5757480278968,3.64104970535346,36.2175369025958));
#39435=CARTESIAN_POINT('Ctrl Pts',(19.5237909081485,3.64464354099556,36.2305549199736));
#39436=CARTESIAN_POINT('Ctrl Pts',(19.5164493996503,3.6451498843845,36.2324404084693));
#39437=CARTESIAN_POINT('Ctrl Pts',(19.5046839739135,3.64595878512668,36.2355361030975));
#39438=CARTESIAN_POINT('Ctrl Pts',(19.500253017933,3.64626283901879,36.2367188769425));
#39439=CARTESIAN_POINT('Ctrl Pts',(19.4923780768534,3.64680212770163,36.2388510801924));
#39440=CARTESIAN_POINT('Ctrl Pts',(19.4889324658017,3.64703771342144,36.2397942869541));
#39441=CARTESIAN_POINT('Ctrl Pts',(19.4815783484048,3.64753971901391,36.2418293900072));
#39442=CARTESIAN_POINT('Ctrl Pts',(19.477670667882,3.64780597774356,36.2429240472601));
#39443=CARTESIAN_POINT('Ctrl Pts',(19.4669894898028,3.64853250512679,36.2459525432283));
#39444=CARTESIAN_POINT('Ctrl Pts',(19.4602230009392,3.64899136983806,36.2479111870733));
#39445=CARTESIAN_POINT('Ctrl Pts',(19.4335812699271,3.65079313461476,36.2557813737182));
#39446=CARTESIAN_POINT('Ctrl Pts',(19.4137909377445,3.65212070577368,36.2619762015326));
#39447=CARTESIAN_POINT('Ctrl Pts',(19.3941040086362,3.65343403802913,36.2684889832302));
#39448=CARTESIAN_POINT('Origin',(20.,-1.3495818343519,38.1));
#39449=CARTESIAN_POINT('',(19.3941040488142,4.61690666843697,36.2684889699386));
#39450=CARTESIAN_POINT('',(19.3941039894965,4.44426476764078,36.2684889895619));
#39451=CARTESIAN_POINT('',(19.3941040087494,-1.3495818343519,36.2684889831927));
#39452=CARTESIAN_POINT('Ctrl Pts',(19.3941040488142,4.61690666843697,36.2684889699386));
#39453=CARTESIAN_POINT('Ctrl Pts',(19.4217433849466,4.61516042926103,36.259345393088));
#39454=CARTESIAN_POINT('Ctrl Pts',(19.4495925545255,4.61340744069853,36.2508265292804));
#39455=CARTESIAN_POINT('Ctrl Pts',(19.5534307922853,4.6068707433316,36.2216180341652));
#39456=CARTESIAN_POINT('Ctrl Pts',(19.6304573128013,4.60201702819168,36.2049593908931));
#39457=CARTESIAN_POINT('Ctrl Pts',(19.7272129739756,4.5957950934203,36.1901579568729));
#39458=CARTESIAN_POINT('Ctrl Pts',(19.7461871599995,4.59456930132189,36.1875438850572));
#39459=CARTESIAN_POINT('Ctrl Pts',(19.77373178223,4.59278037058269,36.1841661879457));
#39460=CARTESIAN_POINT('Ctrl Pts',(19.7822737569181,4.59222428668319,36.183176643265));
#39461=CARTESIAN_POINT('Ctrl Pts',(19.7972283433773,4.59124832893086,36.1815454807755));
#39462=CARTESIAN_POINT('Ctrl Pts',(19.8036381325037,4.5908292433062,36.1808788202984));
#39463=CARTESIAN_POINT('Ctrl Pts',(19.8160693562865,4.59001491468124,36.1796488213164));
#39464=CARTESIAN_POINT('Ctrl Pts',(19.822090343592,4.58961979627771,36.1790816561008));
#39465=CARTESIAN_POINT('Ctrl Pts',(19.8364603098112,4.58867506534529,36.1777961742714));
#39466=CARTESIAN_POINT('Ctrl Pts',(19.8448114414141,4.58812464675447,36.1771039327467));
#39467=CARTESIAN_POINT('Ctrl Pts',(19.8748290181767,4.58614106413554,36.1748125358137));
#39468=CARTESIAN_POINT('Ctrl Pts',(19.8965169300648,4.58469827538078,36.1735250492253));
#39469=CARTESIAN_POINT('Ctrl Pts',(20.0711483949763,4.57299900619799,36.1661154940672));
#39470=CARTESIAN_POINT('Ctrl Pts',(20.2242756992017,4.56216998168005,36.1778517810998));
#39471=CARTESIAN_POINT('Ctrl Pts',(20.4541170603095,4.54545143079664,36.2233198843081));
#39472=CARTESIAN_POINT('Ctrl Pts',(20.5327895805914,4.53965580306748,36.2441208314317));
#39473=CARTESIAN_POINT('Ctrl Pts',(20.6437100857044,4.53155527609672,36.2810858953062));
#39474=CARTESIAN_POINT('Ctrl Pts',(20.6771853761131,4.52912085015314,36.2932815499375));
#39475=CARTESIAN_POINT('Ctrl Pts',(20.7171920528624,4.52623949880148,36.3091250832975));
#39476=CARTESIAN_POINT('Ctrl Pts',(20.7240622727002,4.52574571201067,36.3118917153617));
#39477=CARTESIAN_POINT('Ctrl Pts',(20.7347455796272,4.52497964515902,36.3162655440651));
#39478=CARTESIAN_POINT('Ctrl Pts',(20.738569626017,4.52470579187046,36.3178455217364));
#39479=CARTESIAN_POINT('Ctrl Pts',(20.7456745932028,4.52419768553872,36.3208078707606));
#39480=CARTESIAN_POINT('Ctrl Pts',(20.748956739662,4.52396325095684,36.3221870081106));
#39481=CARTESIAN_POINT('Ctrl Pts',(20.7564166140534,4.523431045377,36.3253459258456));
#39482=CARTESIAN_POINT('Ctrl Pts',(20.7605918812098,4.52313361977978,36.3271313731109));
#39483=CARTESIAN_POINT('Ctrl Pts',(20.7733394338673,4.5222268032921,36.3326358635828));
#39484=CARTESIAN_POINT('Ctrl Pts',(20.7818911922611,4.52162020392953,36.3364025281686));
#39485=CARTESIAN_POINT('Ctrl Pts',(20.8772129033101,4.51487464809053,36.379217104958));
#39486=CARTESIAN_POINT('Ctrl Pts',(20.9610203061125,4.50908852955465,36.4245772284742));
#39487=CARTESIAN_POINT('Ctrl Pts',(21.1876794987629,4.49292381154619,36.5698835996926));
#39488=CARTESIAN_POINT('Ctrl Pts',(21.3208086480482,4.4827138251842,36.6832084689386));
#39489=CARTESIAN_POINT('Ctrl Pts',(21.4506174311852,4.4703644713334,36.8281225635701));
#39490=CARTESIAN_POINT('Ctrl Pts',(21.4640560335353,4.46905321659646,36.8436150970497));
#39491=CARTESIAN_POINT('Ctrl Pts',(21.4829291148577,4.46716235299635,36.866086745611));
#39492=CARTESIAN_POINT('Ctrl Pts',(21.4885668701474,4.46659099124767,36.8728939133538));
#39493=CARTESIAN_POINT('Ctrl Pts',(21.4982591741286,4.46559718583685,36.884761731152));
#39494=CARTESIAN_POINT('Ctrl Pts',(21.5023353868492,4.46517561871386,36.8898045667551));
#39495=CARTESIAN_POINT('Ctrl Pts',(21.5101257319498,4.46436289364722,36.8995423094714));
#39496=CARTESIAN_POINT('Ctrl Pts',(21.513843592365,4.46397189053471,36.904234149364));
#39497=CARTESIAN_POINT('Ctrl Pts',(21.5225661776168,4.46304705141315,36.9153476978905));
#39498=CARTESIAN_POINT('Ctrl Pts',(21.5275521750585,4.4625124862287,36.9217838945412));
#39499=CARTESIAN_POINT('Ctrl Pts',(21.5448231133803,4.46063986048519,36.9443720712433));
#39500=CARTESIAN_POINT('Ctrl Pts',(21.5568934593972,4.45929351914829,36.9606857043561));
#39501=CARTESIAN_POINT('Ctrl Pts',(21.6673829967903,4.446605864438,37.1150526713218));
#39502=CARTESIAN_POINT('Ctrl Pts',(21.7474382586424,4.43454217570489,37.2653008480401));
#39503=CARTESIAN_POINT('Ctrl Pts',(21.8314283322691,4.417455576334,37.4897997992774));
#39504=CARTESIAN_POINT('Ctrl Pts',(21.8524272067254,4.41247314441218,37.5568712449273));
#39505=CARTESIAN_POINT('Ctrl Pts',(21.8777682402318,4.40536145964218,37.6566080470622));
#39506=CARTESIAN_POINT('Ctrl Pts',(21.8850086484524,4.4031328345844,37.6884751580249));
#39507=CARTESIAN_POINT('Ctrl Pts',(21.8928566472806,4.40046240012044,37.7275911044223));
#39508=CARTESIAN_POINT('Ctrl Pts',(21.8942370361446,4.3999812255997,37.7346772281675));
#39509=CARTESIAN_POINT('Ctrl Pts',(21.896338357497,4.39923042633378,37.7457964244269));
#39510=CARTESIAN_POINT('Ctrl Pts',(21.8970862593421,4.3989593263756,37.7498242377682));
#39511=CARTESIAN_POINT('Ctrl Pts',(21.8984611350802,4.39845362546502,37.7573623052131));
#39512=CARTESIAN_POINT('Ctrl Pts',(21.8990912005849,4.39821885947163,37.7608718775434));
#39513=CARTESIAN_POINT('Ctrl Pts',(21.9005120707179,4.39768239405247,37.7689145140589));
#39514=CARTESIAN_POINT('Ctrl Pts',(21.9012963892106,4.39738106212558,37.7734486695756));
#39515=CARTESIAN_POINT('Ctrl Pts',(21.903310698097,4.39659314028827,37.7853467273748));
#39516=CARTESIAN_POINT('Ctrl Pts',(21.9045141915785,4.39610799566289,37.7927151257903));
#39517=CARTESIAN_POINT('Ctrl Pts',(21.9124680268063,4.39279847236769,37.8432551140782));
#39518=CARTESIAN_POINT('Ctrl Pts',(21.9177932487008,4.39004763771808,37.8866420248929));
#39519=CARTESIAN_POINT('Ctrl Pts',(21.9228476258785,4.38649579342051,37.9438347610123));
#39520=CARTESIAN_POINT('Ctrl Pts',(21.923909070375,4.38565231098272,37.9575062183754));
#39521=CARTESIAN_POINT('Ctrl Pts',(21.9335429046849,4.37681852324583,38.1014637308141));
#39522=CARTESIAN_POINT('Ctrl Pts',(21.9290133508093,4.36918038076055,38.23229255749));
#39523=CARTESIAN_POINT('Ctrl Pts',(21.9029529552375,4.35756703534153,38.4226467440222));
#39524=CARTESIAN_POINT('Ctrl Pts',(21.8916914845443,4.3538010728418,38.4831882853689));
#39525=CARTESIAN_POINT('Ctrl Pts',(21.8691069165198,4.34765100144082,38.5788896328528));
#39526=CARTESIAN_POINT('Ctrl Pts',(21.859635324769,4.34532202008999,38.6144435088058));
#39527=CARTESIAN_POINT('Ctrl Pts',(21.8460065451228,4.34225140838157,38.6602895395444));
#39528=CARTESIAN_POINT('Ctrl Pts',(21.8427686969458,4.34153950605068,38.6708485386371));
#39529=CARTESIAN_POINT('Ctrl Pts',(21.8373494684938,4.340375580395,38.6879945797138));
#39530=CARTESIAN_POINT('Ctrl Pts',(21.8352228701748,4.33992534350943,38.694598780567));
#39531=CARTESIAN_POINT('Ctrl Pts',(21.8310592407894,4.3390560883792,38.7072938836381));
#39532=CARTESIAN_POINT('Ctrl Pts',(21.8290273250354,4.33863724229716,38.713386376593));
#39533=CARTESIAN_POINT('Ctrl Pts',(21.8242957285344,4.33767396763443,38.7273410179269));
#39534=CARTESIAN_POINT('Ctrl Pts',(21.8215755920188,4.3371288737969,38.7351960459889));
#39535=CARTESIAN_POINT('Ctrl Pts',(21.8141875661497,4.33567096171994,38.756092911195));
#39536=CARTESIAN_POINT('Ctrl Pts',(21.8094299016325,4.33475520357829,38.7691022697902));
#39537=CARTESIAN_POINT('Ctrl Pts',(21.7642749665455,4.32626881146562,38.8885692907445));
#39538=CARTESIAN_POINT('Ctrl Pts',(21.7146740153783,4.31838631654346,38.9912869176095));
#39539=CARTESIAN_POINT('Ctrl Pts',(21.6177503413988,4.30499866869008,39.1536059286512));
#39540=CARTESIAN_POINT('Ctrl Pts',(21.5754389511386,4.29961028037633,39.2158822993459));
#39541=CARTESIAN_POINT('Ctrl Pts',(21.4757661322168,4.28797381560509,39.3455769904254));
#39542=CARTESIAN_POINT('Ctrl Pts',(21.4171758110747,4.28175231499799,39.4118553150817));
#39543=CARTESIAN_POINT('Ctrl Pts',(21.3478531271193,4.27521459194621,39.4801865658333));
#39544=CARTESIAN_POINT('Ctrl Pts',(21.3414212306577,4.27461522385891,39.4864386385234));
#39545=CARTESIAN_POINT('Ctrl Pts',(21.3317216674679,4.27372240785382,39.4957363303852));
#39546=CARTESIAN_POINT('Ctrl Pts',(21.3284867614135,4.2734264618551,39.4988157238562));
#39547=CARTESIAN_POINT('Ctrl Pts',(21.3226579274001,4.27289651133477,39.5043258882336));
#39548=CARTESIAN_POINT('Ctrl Pts',(21.3200679614774,4.27266219866563,39.5067607369466));
#39549=CARTESIAN_POINT('Ctrl Pts',(21.3144080112681,4.2721526803333,39.5120523083578));
#39550=CARTESIAN_POINT('Ctrl Pts',(21.3113354454917,4.27187769004966,39.5149061777545));
#39551=CARTESIAN_POINT('Ctrl Pts',(21.3027750743043,4.27111591751082,39.5228054094895));
#39552=CARTESIAN_POINT('Ctrl Pts',(21.2972672210801,4.27063073813734,39.5278290825652));
#39553=CARTESIAN_POINT('Ctrl Pts',(21.2678904883271,4.26806824552355,39.5543130749083));
#39554=CARTESIAN_POINT('Ctrl Pts',(21.2435163190861,4.26602991525139,39.5752085495293));
#39555=CARTESIAN_POINT('Ctrl Pts',(21.2044588721818,4.26287767657497,39.6070353572671));
#39556=CARTESIAN_POINT('Ctrl Pts',(21.1901235277678,4.2617437771043,39.6183816290915));
#39557=CARTESIAN_POINT('Ctrl Pts',(21.1670523668197,4.25995138218209,39.6361146885293));
#39558=CARTESIAN_POINT('Ctrl Pts',(21.1584206669402,4.25928785530989,39.6426344766061));
#39559=CARTESIAN_POINT('Ctrl Pts',(21.0527369742636,4.25124336914657,39.721073338999));
#39560=CARTESIAN_POINT('Ctrl Pts',(20.9491887758372,4.24415496626519,39.7837984905317));
#39561=CARTESIAN_POINT('Ctrl Pts',(20.7806899345176,4.23287103583038,39.8653536938381));
#39562=CARTESIAN_POINT('Ctrl Pts',(20.7194811566678,4.22882190487687,39.8911717373543));
#39563=CARTESIAN_POINT('Ctrl Pts',(20.6206182379638,4.22225575545189,39.9269861548686));
#39564=CARTESIAN_POINT('Ctrl Pts',(20.5837820304635,4.21980417738075,39.9390877145324));
#39565=CARTESIAN_POINT('Ctrl Pts',(20.5358204633695,4.21659443345015,39.9532580827717));
#39566=CARTESIAN_POINT('Ctrl Pts',(20.5250052674994,4.2158695191197,39.9563508695044));
#39567=CARTESIAN_POINT('Ctrl Pts',(20.5074331657714,4.21468962242291,39.961210064743));
#39568=CARTESIAN_POINT('Ctrl Pts',(20.5006925242289,4.21423652111762,39.9630347063014));
#39569=CARTESIAN_POINT('Ctrl Pts',(20.4877476869706,4.21336536606425,39.9664634512382));
#39570=CARTESIAN_POINT('Ctrl Pts',(20.4815451035329,4.21294750406135,39.9680733209807));
#39571=CARTESIAN_POINT('Ctrl Pts',(20.4673716744068,4.21199158792222,39.9716767303187));
#39572=CARTESIAN_POINT('Ctrl Pts',(20.4593959259106,4.21145290244669,39.9736502994404));
#39573=CARTESIAN_POINT('Ctrl Pts',(20.4382601031204,4.2100232353587,39.9787372134501));
#39574=CARTESIAN_POINT('Ctrl Pts',(20.42507967225,4.20912949103839,39.981763186927));
#39575=CARTESIAN_POINT('Ctrl Pts',(20.3214640492965,4.20208506045868,40.0044071980833));
#39576=CARTESIAN_POINT('Ctrl Pts',(20.229768955051,4.19573243692902,40.0176307021517));
#39577=CARTESIAN_POINT('Ctrl Pts',(19.9779362599118,4.17799848806848,40.0356248046861));
#39578=CARTESIAN_POINT('Ctrl Pts',(19.8175932114207,4.16635202614621,40.0271366259504));
#39579=CARTESIAN_POINT('Ctrl Pts',(19.6315140946171,4.15333098510131,39.9938337962496));
#39580=CARTESIAN_POINT('Ctrl Pts',(19.6030046674812,4.15135218311773,39.9880633574922));
#39581=CARTESIAN_POINT('Ctrl Pts',(19.5678434950929,4.14894058054307,39.9801148345455));
#39582=CARTESIAN_POINT('Ctrl Pts',(19.5610604139643,4.14847669313282,39.9785428074112));
#39583=CARTESIAN_POINT('Ctrl Pts',(19.5503551106908,4.14774685554124,39.9760006270133));
#39584=CARTESIAN_POINT('Ctrl Pts',(19.5464272522642,4.14747956020597,39.9750548371428));
#39585=CARTESIAN_POINT('Ctrl Pts',(19.5390282997567,4.14697701039571,39.9732486318485));
#39586=CARTESIAN_POINT('Ctrl Pts',(19.5355566683336,4.14674161409593,39.9723909145936));
#39587=CARTESIAN_POINT('Ctrl Pts',(19.5276093306862,4.1462036373515,39.9704039453093));
#39588=CARTESIAN_POINT('Ctrl Pts',(19.5231352799169,4.14590142676041,39.9692682800802));
#39589=CARTESIAN_POINT('Ctrl Pts',(19.511227158127,4.14509869132121,39.9662000602069));
#39590=CARTESIAN_POINT('Ctrl Pts',(19.5038003875913,4.14459974024977,39.9642391222873));
#39591=CARTESIAN_POINT('Ctrl Pts',(19.4497188737165,4.14097742868771,39.9496135470395));
#39592=CARTESIAN_POINT('Ctrl Pts',(19.403538669408,4.13794424025762,39.9352423184952));
#39593=CARTESIAN_POINT('Ctrl Pts',(19.2286555086251,4.12651739352343,39.873518457891));
#39594=CARTESIAN_POINT('Ctrl Pts',(19.1045937590485,4.11851291204389,39.8142324447551));
#39595=CARTESIAN_POINT('Ctrl Pts',(18.9342427767939,4.10642791696285,39.7092454047518));
#39596=CARTESIAN_POINT('Ctrl Pts',(18.8822802126492,4.10257805189969,39.6735980176834));
#39597=CARTESIAN_POINT('Ctrl Pts',(18.8024027811172,4.09630430654009,39.6128452939391));
#39598=CARTESIAN_POINT('Ctrl Pts',(18.7733145362388,4.09393850633659,39.5893563914937));
#39599=CARTESIAN_POINT('Ctrl Pts',(18.7364936118458,4.09082606188915,39.5578125819219));
#39600=CARTESIAN_POINT('Ctrl Pts',(18.7281215207411,4.09011018212417,39.5505140614705));
#39601=CARTESIAN_POINT('Ctrl Pts',(18.7146124517329,4.08894137578081,39.5385304088354));
#39602=CARTESIAN_POINT('Ctrl Pts',(18.709436875754,4.0884902643654,39.5338890147518));
#39603=CARTESIAN_POINT('Ctrl Pts',(18.6995318221263,4.08762044365133,39.5249092125008));
#39604=CARTESIAN_POINT('Ctrl Pts',(18.6947986773494,4.08720191255303,39.5205749720512));
#39605=CARTESIAN_POINT('Ctrl Pts',(18.6840069619233,4.08624095344394,39.5105933076828));
#39606=CARTESIAN_POINT('Ctrl Pts',(18.6779629909669,4.08569787083798,39.5049303538213));
#39607=CARTESIAN_POINT('Ctrl Pts',(18.6619837517628,4.08424884318147,39.489764043791));
#39608=CARTESIAN_POINT('Ctrl Pts',(18.6521134399902,4.08334001453743,39.4801932410899));
#39609=CARTESIAN_POINT('Ctrl Pts',(18.5482248853404,4.07362454576865,39.377279842162));
#39610=CARTESIAN_POINT('Ctrl Pts',(18.463976987028,4.06438730890076,39.2746128333193));
#39611=CARTESIAN_POINT('Ctrl Pts',(18.3330469446396,4.04749993939522,39.0766360533751));
#39612=CARTESIAN_POINT('Ctrl Pts',(18.2824058367384,4.03995694287053,38.9845463062223));
#39613=CARTESIAN_POINT('Ctrl Pts',(18.2222187684088,4.02970522874001,38.8502155841056));
#39614=CARTESIAN_POINT('Ctrl Pts',(18.2062052112214,4.0268035576142,38.8110769433286));
#39615=CARTESIAN_POINT('Ctrl Pts',(18.1887866336923,4.02344994537789,38.7641603745008));
#39616=CARTESIAN_POINT('Ctrl Pts',(18.1861277177054,4.02293190793254,38.7568639203817));
#39617=CARTESIAN_POINT('Ctrl Pts',(18.18209354727,4.02213655403118,38.7455822604908));
#39618=CARTESIAN_POINT('Ctrl Pts',(18.1806872117192,4.02185746843808,38.7416083736819));
#39619=CARTESIAN_POINT('Ctrl Pts',(18.1781194327421,4.02134455089018,38.7342762659293));
#39620=CARTESIAN_POINT('Ctrl Pts',(18.1769542493074,4.02111050661599,38.7309194672511));
#39621=CARTESIAN_POINT('Ctrl Pts',(18.1743542712047,4.0205853091986,38.7233618008505));
#39622=CARTESIAN_POINT('Ctrl Pts',(18.1729247008032,4.02029446404498,38.7191591991306));
#39623=CARTESIAN_POINT('Ctrl Pts',(18.1693003873996,4.0195516512404,38.7083827061063));
#39624=CARTESIAN_POINT('Ctrl Pts',(18.1671265174731,4.01910087231834,38.7018017856725));
#39625=CARTESIAN_POINT('Ctrl Pts',(18.1544639546345,4.01644280918484,38.6627634873682));
#39626=CARTESIAN_POINT('Ctrl Pts',(18.1448013836846,4.0142800591071,38.6300419561242));
#39627=CARTESIAN_POINT('Ctrl Pts',(18.1318640824568,4.01114533297078,38.5815285709754));
#39628=CARTESIAN_POINT('Ctrl Pts',(18.127911811724,4.01014796905676,38.5659264033361));
#39629=CARTESIAN_POINT('Ctrl Pts',(18.12166518197,4.00849958209285,38.5399030247195));
#39630=CARTESIAN_POINT('Ctrl Pts',(18.1192612623421,4.0078452027334,38.5295092163879));
#39631=CARTESIAN_POINT('Ctrl Pts',(18.0864220122501,3.99860538724657,38.3819578687861));
#39632=CARTESIAN_POINT('Ctrl Pts',(18.0709715023171,3.990411626189,38.2418930328489));
#39633=CARTESIAN_POINT('Ctrl Pts',(18.0708133507936,3.97704079803533,38.0218888399083));
#39634=CARTESIAN_POINT('Ctrl Pts',(18.0756701924695,3.97211873391506,37.9424724237382));
#39635=CARTESIAN_POINT('Ctrl Pts',(18.0870228991789,3.96619961696205,37.8505321041372));
#39636=CARTESIAN_POINT('Ctrl Pts',(18.0887685376542,3.96535505979258,37.8374930421612));
#39637=CARTESIAN_POINT('Ctrl Pts',(18.0918178427118,3.96397762631338,37.8163618973671));
#39638=CARTESIAN_POINT('Ctrl Pts',(18.0930399808263,3.96344730292806,37.8082583325577));
#39639=CARTESIAN_POINT('Ctrl Pts',(18.095306441344,3.96250076037313,37.7938533013139));
#39640=CARTESIAN_POINT('Ctrl Pts',(18.0963305019229,3.96208518347924,37.7875487334658));
#39641=CARTESIAN_POINT('Ctrl Pts',(18.0985529863079,3.96120792316165,37.7742827799156));
#39642=CARTESIAN_POINT('Ctrl Pts',(18.0997583715633,3.96074602610255,37.7673226718487));
#39643=CARTESIAN_POINT('Ctrl Pts',(18.1030464125094,3.95952155342855,37.7489380395507));
#39644=CARTESIAN_POINT('Ctrl Pts',(18.1051940225579,3.95875694007456,37.7375255718641));
#39645=CARTESIAN_POINT('Ctrl Pts',(18.1156931406398,3.9551745548734,37.684377835485));
#39646=CARTESIAN_POINT('Ctrl Pts',(18.1253207915251,3.95231676982322,37.6429097398547));
#39647=CARTESIAN_POINT('Ctrl Pts',(18.17940113469,3.93805261648679,37.4406049801355));
#39648=CARTESIAN_POINT('Ctrl Pts',(18.243217800543,3.92603020671464,37.2857025341727));
#39649=CARTESIAN_POINT('Ctrl Pts',(18.3408459147008,3.91211244182069,37.1153042894467));
#39650=CARTESIAN_POINT('Ctrl Pts',(18.3561433708184,3.9100263589118,37.0899735523866));
#39651=CARTESIAN_POINT('Ctrl Pts',(18.3878201486455,3.90590107481111,37.0401480252906));
#39652=CARTESIAN_POINT('Ctrl Pts',(18.4041904291212,3.90386220833471,37.0156559200628));
#39653=CARTESIAN_POINT('Ctrl Pts',(18.4327579898231,3.90046761559812,36.9749641939155));
#39654=CARTESIAN_POINT('Ctrl Pts',(18.4446610693517,3.89909752675677,36.9585649493338));
#39655=CARTESIAN_POINT('Ctrl Pts',(18.4606563544544,3.89731662600097,36.9372426953686));
#39656=CARTESIAN_POINT('Ctrl Pts',(18.4645172768703,3.89689121337132,36.932148888612));
#39657=CARTESIAN_POINT('Ctrl Pts',(18.4707826805114,3.89620813275404,36.9239675775284));
#39658=CARTESIAN_POINT('Ctrl Pts',(18.4731713234128,3.8959493914636,36.9208680896699));
#39659=CARTESIAN_POINT('Ctrl Pts',(18.4777842585066,3.89545296259651,36.9149198949708));
#39660=CARTESIAN_POINT('Ctrl Pts',(18.4800071305063,3.89521518462695,36.912070163743));
#39661=CARTESIAN_POINT('Ctrl Pts',(18.4852977000073,3.89465262446539,36.9053267936235));
#39662=CARTESIAN_POINT('Ctrl Pts',(18.4883724463787,3.89432833679257,36.9014386673542));
#39663=CARTESIAN_POINT('Ctrl Pts',(18.4986882039736,3.89324902140899,36.8884968646558));
#39664=CARTESIAN_POINT('Ctrl Pts',(18.5059960069998,3.8924985530324,36.8794963987493));
#39665=CARTESIAN_POINT('Ctrl Pts',(18.5237112512491,3.89071130191849,36.8580754285004));
#39666=CARTESIAN_POINT('Ctrl Pts',(18.5341950690072,3.88967939715213,36.8457189098154));
#39667=CARTESIAN_POINT('Ctrl Pts',(18.5740379519883,3.88584646319466,36.7999409272007));
#39668=CARTESIAN_POINT('Ctrl Pts',(18.6043961770208,3.88310177944765,36.7674040820889));
#39669=CARTESIAN_POINT('Ctrl Pts',(18.7572310768449,3.869938882807,36.6145591389673));
#39670=CARTESIAN_POINT('Ctrl Pts',(18.8942622520232,3.85999975198645,36.5099193007882));
#39671=CARTESIAN_POINT('Ctrl Pts',(19.0835316410962,3.84647620676696,36.4018330473647));
#39672=CARTESIAN_POINT('Ctrl Pts',(19.1245385067943,3.84356252770913,36.3803337860971));
#39673=CARTESIAN_POINT('Ctrl Pts',(19.177390605636,3.83980747959394,36.355004803175));
#39674=CARTESIAN_POINT('Ctrl Pts',(19.188555370052,3.83901429386234,36.3497851406876));
#39675=CARTESIAN_POINT('Ctrl Pts',(19.2064040899856,3.83774598759691,36.3416481410624));
#39676=CARTESIAN_POINT('Ctrl Pts',(19.2130560237657,3.83727325202138,36.3386610479307));
#39677=CARTESIAN_POINT('Ctrl Pts',(19.2255340378444,3.83638628934142,36.3331425127215));
#39678=CARTESIAN_POINT('Ctrl Pts',(19.2313560130903,3.83597237758754,36.3306019874924));
#39679=CARTESIAN_POINT('Ctrl Pts',(19.2443854937682,3.83504583251551,36.3249927776994));
#39680=CARTESIAN_POINT('Ctrl Pts',(19.251599324856,3.83453269855067,36.3219391608706));
#39681=CARTESIAN_POINT('Ctrl Pts',(19.2728556870746,3.83302014159584,36.3130936111078));
#39682=CARTESIAN_POINT('Ctrl Pts',(19.2869479973391,3.83201665617838,36.3074236100906));
#39683=CARTESIAN_POINT('Ctrl Pts',(19.3318333028841,3.82881750908881,36.2899771627739));
#39684=CARTESIAN_POINT('Ctrl Pts',(19.3628434160786,3.82660281497636,36.2788305312031));
#39685=CARTESIAN_POINT('Ctrl Pts',(19.3941042587802,3.8243647438501,36.2684889004782));
#39686=CARTESIAN_POINT('',(18.0708708501867,3.80900185377495,38.0984559108978));
#39687=CARTESIAN_POINT('Ctrl Pts',(19.3941040086362,3.65343403802913,36.2684889832302));
#39688=CARTESIAN_POINT('Ctrl Pts',(19.3851461582278,3.6540316240628,36.2714523973751));
#39689=CARTESIAN_POINT('Ctrl Pts',(19.376209716234,3.65462626174559,36.274481640278));
#39690=CARTESIAN_POINT('Ctrl Pts',(19.2143176168196,3.665377095241,36.3306869478762));
#39691=CARTESIAN_POINT('Ctrl Pts',(19.0686201053574,3.67474886595825,36.4028525906517));
#39692=CARTESIAN_POINT('Ctrl Pts',(18.8591032064564,3.68995776020145,36.5418287318295));
#39693=CARTESIAN_POINT('Ctrl Pts',(18.7881024655457,3.69546934998093,36.5963895351481));
#39694=CARTESIAN_POINT('Ctrl Pts',(18.7110812495807,3.7020398960586,36.6645865436071));
#39695=CARTESIAN_POINT('Ctrl Pts',(18.7011084297453,3.70290282511424,36.6736045393984));
#39696=CARTESIAN_POINT('Ctrl Pts',(18.6852114632913,3.70429859839293,36.6882844507502));
#39697=CARTESIAN_POINT('Ctrl Pts',(18.6792275888118,3.70482870432481,36.6938812558347));
#39698=CARTESIAN_POINT('Ctrl Pts',(18.6686299225227,3.70577609535566,36.7039207416122));
#39699=CARTESIAN_POINT('Ctrl Pts',(18.6640022332416,3.70619274445471,36.7083486268206));
#39700=CARTESIAN_POINT('Ctrl Pts',(18.6551197200089,3.70699823954631,36.716932768572));
#39701=CARTESIAN_POINT('Ctrl Pts',(18.650861893487,3.7073869444375,36.7210858248666));
#39702=CARTESIAN_POINT('Ctrl Pts',(18.6397221004987,3.70841080590348,36.7320524938786));
#39703=CARTESIAN_POINT('Ctrl Pts',(18.632872186243,3.7090473648826,36.738898285045));
#39704=CARTESIAN_POINT('Ctrl Pts',(18.6066950002682,3.71150734331433,36.7654566848019));
#39705=CARTESIAN_POINT('Ctrl Pts',(18.5877409668395,3.71334674823657,36.7855309162192));
#39706=CARTESIAN_POINT('Ctrl Pts',(18.5412428655149,3.71801112839031,36.8369440007918));
#39707=CARTESIAN_POINT('Ctrl Pts',(18.5142735756319,3.72085817615058,36.8687813375002));
#39708=CARTESIAN_POINT('Ctrl Pts',(18.443101699652,3.7287742189638,36.9585462645469));
#39709=CARTESIAN_POINT('Ctrl Pts',(18.4011174950201,3.73391154060393,37.0181395350112));
#39710=CARTESIAN_POINT('Ctrl Pts',(18.2898554733521,3.74888281311257,37.196739959117));
#39711=CARTESIAN_POINT('Ctrl Pts',(18.2298021928285,3.75881332750799,37.3209760806627));
#39712=CARTESIAN_POINT('Ctrl Pts',(18.1787739075928,3.76907883473651,37.4637035632299));
#39713=CARTESIAN_POINT('Ctrl Pts',(18.174214655466,3.77001787057233,37.4769064769561));
#39714=CARTESIAN_POINT('Ctrl Pts',(18.1680585730791,3.77131608307844,37.4953815436534));
#39715=CARTESIAN_POINT('Ctrl Pts',(18.1663404446504,3.77168189194893,37.5006123905705));
#39716=CARTESIAN_POINT('Ctrl Pts',(18.163613323029,3.7722681245345,37.509036596841));
#39717=CARTESIAN_POINT('Ctrl Pts',(18.1625902257339,3.77248935809529,37.5122253041435));
#39718=CARTESIAN_POINT('Ctrl Pts',(18.160462785769,3.77295212726625,37.5189157755266));
#39719=CARTESIAN_POINT('Ctrl Pts',(18.1593601307929,3.77319355900465,37.5224180485165));
#39720=CARTESIAN_POINT('Ctrl Pts',(18.1566982254109,3.77378032214086,37.5309578815979));
#39721=CARTESIAN_POINT('Ctrl Pts',(18.1551496031556,3.77412503928215,37.5359987769598));
#39722=CARTESIAN_POINT('Ctrl Pts',(18.1497028783146,3.77534978853889,37.553990803865));
#39723=CARTESIAN_POINT('Ctrl Pts',(18.1459202150976,3.77622341707248,37.5669768702197));
#39724=CARTESIAN_POINT('Ctrl Pts',(18.1233332138771,3.78159423302404,37.6476703710395));
#39725=CARTESIAN_POINT('Ctrl Pts',(18.108101300561,3.78591400750198,37.716331040995));
#39726=CARTESIAN_POINT('Ctrl Pts',(18.0795757838454,3.79650422848749,37.8890643503315));
#39727=CARTESIAN_POINT('Ctrl Pts',(18.0709545923284,3.80268017310218,37.9936686640546));
#39728=CARTESIAN_POINT('Ctrl Pts',(18.0708706194525,3.80900133785267,38.0984540347479));
#39729=CARTESIAN_POINT('Ctrl Pts',(18.0708706179307,3.80900145248059,38.0984559349242));
#39730=CARTESIAN_POINT('Ctrl Pts',(18.0707947923802,3.81471634261588,38.1931911243054));
#39731=CARTESIAN_POINT('Ctrl Pts',(18.0776971394593,3.82053333068208,38.2877941798662));
#39732=CARTESIAN_POINT('Ctrl Pts',(18.093157633927,3.82729189732055,38.3926103313709));
#39733=CARTESIAN_POINT('Ctrl Pts',(18.0948928930901,3.8280110044117,38.4037030091995));
#39734=CARTESIAN_POINT('Ctrl Pts',(18.0979441529452,3.82921372139165,38.4221520597585));
#39735=CARTESIAN_POINT('Ctrl Pts',(18.0992062626677,3.82969565035746,38.4295171626478));
#39736=CARTESIAN_POINT('Ctrl Pts',(18.1015682108665,3.83057042720451,38.4428351554627));
#39737=CARTESIAN_POINT('Ctrl Pts',(18.1026533446979,3.8309628094676,38.4487905819368));
#39738=CARTESIAN_POINT('Ctrl Pts',(18.1049217777222,3.83176423758432,38.4609162787321));
#39739=CARTESIAN_POINT('Ctrl Pts',(18.1061072243265,3.832173346761,38.4670860682454));
#39740=CARTESIAN_POINT('Ctrl Pts',(18.1087603598732,3.83306837939916,38.4805395996859));
#39741=CARTESIAN_POINT('Ctrl Pts',(18.1102400285953,3.83355467649597,38.4878208493566));
#39742=CARTESIAN_POINT('Ctrl Pts',(18.1144090411457,3.83489067886773,38.5077454834846));
#39743=CARTESIAN_POINT('Ctrl Pts',(18.1171834174452,3.83574306760818,38.520370486736));
#39744=CARTESIAN_POINT('Ctrl Pts',(18.1320954752845,3.84014542221406,38.5851177975624));
#39745=CARTESIAN_POINT('Ctrl Pts',(18.146270338236,3.843759680657,38.6367420093424));
#39746=CARTESIAN_POINT('Ctrl Pts',(18.1686210206925,3.84880017406108,38.7066200778223));
#39747=CARTESIAN_POINT('Ctrl Pts',(18.1749621381135,3.85017258128813,38.7254387618747));
#39748=CARTESIAN_POINT('Ctrl Pts',(18.1963508949265,3.85462350888188,38.7858177604959));
#39749=CARTESIAN_POINT('Ctrl Pts',(18.2125360145041,3.8577301327015,38.8269582009965));
#39750=CARTESIAN_POINT('Ctrl Pts',(18.2820911310179,3.87010975576839,38.9873537031444));
#39751=CARTESIAN_POINT('Ctrl Pts',(18.3461018488333,3.87955491100009,39.1016133572993));
#39752=CARTESIAN_POINT('Ctrl Pts',(18.4417131540731,3.8910842723752,39.237788599667));
#39753=CARTESIAN_POINT('Ctrl Pts',(18.4630685339686,3.89352810661431,39.2664745437915));
#39754=CARTESIAN_POINT('Ctrl Pts',(18.4898015691682,3.89641905347886,39.3003742029435));
#39755=CARTESIAN_POINT('Ctrl Pts',(18.4944262063977,3.89691338464032,39.3061695917191));
#39756=CARTESIAN_POINT('Ctrl Pts',(18.5016846572643,3.89768010947562,39.3151587650595));
#39757=CARTESIAN_POINT('Ctrl Pts',(18.5042954709908,3.8979540806697,39.3183709013594));
#39758=CARTESIAN_POINT('Ctrl Pts',(18.5091708857992,3.89846229136008,39.3243299320042));
#39759=CARTESIAN_POINT('Ctrl Pts',(18.511432730272,3.89869671310012,39.3270789355076));
#39760=CARTESIAN_POINT('Ctrl Pts',(18.5165954776466,3.89922874309039,39.3333183600506));
#39761=CARTESIAN_POINT('Ctrl Pts',(18.5195010916272,3.89952600685379,39.3368048097913));
#39762=CARTESIAN_POINT('Ctrl Pts',(18.5284184699448,3.90043184171811,39.3474283285124));
#39763=CARTESIAN_POINT('Ctrl Pts',(18.5344698474112,3.90103763008039,39.3545321895879));
#39764=CARTESIAN_POINT('Ctrl Pts',(18.6041366317163,3.90791462501313,39.435123700652));
#39765=CARTESIAN_POINT('Ctrl Pts',(18.6731767948973,3.91381742707861,39.5037576541927));
#39766=CARTESIAN_POINT('Ctrl Pts',(18.8137574594692,3.92491061097863,39.6238287961646));
#39767=CARTESIAN_POINT('Ctrl Pts',(18.8842096715816,3.93010199453674,39.6761463789056));
#39768=CARTESIAN_POINT('Ctrl Pts',(19.0105557631346,3.93917167817195,39.7572405920793));
#39769=CARTESIAN_POINT('Ctrl Pts',(19.064741284564,3.94299216359648,39.7884124033291));
#39770=CARTESIAN_POINT('Ctrl Pts',(19.1422607324923,3.94843825056907,39.8281297797831));
#39771=CARTESIAN_POINT('Ctrl Pts',(19.1643932457876,3.94999080473494,39.8389394631922));
#39772=CARTESIAN_POINT('Ctrl Pts',(19.203375459722,3.9527253816497,39.8570626117074));
#39773=CARTESIAN_POINT('Ctrl Pts',(19.2201341844663,3.95390099984628,39.8645648053796));
#39774=CARTESIAN_POINT('Ctrl Pts',(19.2447328591887,3.95562774081858,39.8751577519031));
#39775=CARTESIAN_POINT('Ctrl Pts',(19.2524903583109,3.95617245320859,39.8784383121204));
#39776=CARTESIAN_POINT('Ctrl Pts',(19.2662200143533,3.95713691605105,39.8841387303443));
#39777=CARTESIAN_POINT('Ctrl Pts',(19.2721833177304,3.95755595060967,39.8865796796629));
#39778=CARTESIAN_POINT('Ctrl Pts',(19.2837683311647,3.95837032232637,39.8912541262576));
#39779=CARTESIAN_POINT('Ctrl Pts',(19.2893885444216,3.95876553555612,39.8934911502654));
#39780=CARTESIAN_POINT('Ctrl Pts',(19.3028244097915,3.95971072190131,39.8987659841149));
#39781=CARTESIAN_POINT('Ctrl Pts',(19.3106494769708,3.96026150286192,39.9017793210725));
#39782=CARTESIAN_POINT('Ctrl Pts',(19.3388505279036,3.96224773221152,39.9124285968339));
#39783=CARTESIAN_POINT('Ctrl Pts',(19.3593350813199,3.96369283888489,39.9197704359376));
#39784=CARTESIAN_POINT('Ctrl Pts',(19.5242615405982,3.97535100038137,39.9757516728927));
#39785=CARTESIAN_POINT('Ctrl Pts',(19.6738541567207,3.98613112942657,40.0074544589115));
#39786=CARTESIAN_POINT('Ctrl Pts',(19.9070093673327,4.00283686335771,40.0286213644422));
#39787=CARTESIAN_POINT('Ctrl Pts',(19.9888295576126,4.00866730234184,40.0308300080046));
#39788=CARTESIAN_POINT('Ctrl Pts',(20.1062599411118,4.01680959273827,40.0265327607195));
#39789=CARTESIAN_POINT('Ctrl Pts',(20.1419322031541,4.01925231262961,40.0242336924855));
#39790=CARTESIAN_POINT('Ctrl Pts',(20.1849044448613,4.02214212305744,40.0202624455215));
#39791=CARTESIAN_POINT('Ctrl Pts',(20.1922824105571,4.02263638976483,40.0195377027788));
#39792=CARTESIAN_POINT('Ctrl Pts',(20.2037730102829,4.02340303664124,40.0183420573855));
#39793=CARTESIAN_POINT('Ctrl Pts',(20.2078885184056,4.02367699382209,40.0179004284812));
#39794=CARTESIAN_POINT('Ctrl Pts',(20.2155410339602,4.02418519201142,40.0170543270868));
#39795=CARTESIAN_POINT('Ctrl Pts',(20.219078310005,4.02441961518055,40.0166533136512));
#39796=CARTESIAN_POINT('Ctrl Pts',(20.2271229430049,4.02495166568013,40.0157187490872));
#39797=CARTESIAN_POINT('Ctrl Pts',(20.231629532756,4.02524894841625,40.0151790823415));
#39798=CARTESIAN_POINT('Ctrl Pts',(20.2453970696942,4.02615489862516,40.0134811052951));
#39799=CARTESIAN_POINT('Ctrl Pts',(20.2546517202256,4.02676078232643,40.0122714692245));
#39800=CARTESIAN_POINT('Ctrl Pts',(20.3442221218273,4.03259786305619,39.9999023083397));
#39801=CARTESIAN_POINT('Ctrl Pts',(20.4237787133241,4.03757387118289,39.9837549595009));
#39802=CARTESIAN_POINT('Ctrl Pts',(20.6603214717497,4.05236056551573,39.919992832387));
#39803=CARTESIAN_POINT('Ctrl Pts',(20.8124617553576,4.0619192798298,39.857356961039));
#39804=CARTESIAN_POINT('Ctrl Pts',(20.9889775521523,4.07459972680413,39.7568066109195));
#39805=CARTESIAN_POINT('Ctrl Pts',(21.0224967928877,4.07708250928336,39.7363327028243));
#39806=CARTESIAN_POINT('Ctrl Pts',(21.0648245507893,4.08032759491892,39.7086699172734));
#39807=CARTESIAN_POINT('Ctrl Pts',(21.0742282376522,4.08105571654924,39.7024056637775));
#39808=CARTESIAN_POINT('Ctrl Pts',(21.0893629683993,4.08223955071998,39.6921305855099));
#39809=CARTESIAN_POINT('Ctrl Pts',(21.0951282713931,4.08269335858177,39.6881705025905));
#39810=CARTESIAN_POINT('Ctrl Pts',(21.1061314609013,4.08356500088651,39.6805242075244));
#39811=CARTESIAN_POINT('Ctrl Pts',(21.1113727840046,4.08398263882805,39.6768430843576));
#39812=CARTESIAN_POINT('Ctrl Pts',(21.1232772356027,4.08493683001412,39.6683934278243));
#39813=CARTESIAN_POINT('Ctrl Pts',(21.129928474271,4.08547400663796,39.6636084330832));
#39814=CARTESIAN_POINT('Ctrl Pts',(21.1474138524656,4.08689705256441,39.6508593781358));
#39815=CARTESIAN_POINT('Ctrl Pts',(21.15819540032,4.08778564381312,39.6428242799398));
#39816=CARTESIAN_POINT('Ctrl Pts',(21.2400747733902,4.09462105085333,39.5804605951504));
#39817=CARTESIAN_POINT('Ctrl Pts',(21.3073887318384,4.10075615692725,39.5213653705352));
#39818=CARTESIAN_POINT('Ctrl Pts',(21.4844053032464,4.11839680302824,39.3427151607361));
#39819=CARTESIAN_POINT('Ctrl Pts',(21.5834939711443,4.13019984127311,39.2137071533373));
#39820=CARTESIAN_POINT('Ctrl Pts',(21.6804686634817,4.14344449952014,39.0478775849321));
#39821=CARTESIAN_POINT('Ctrl Pts',(21.6950409003734,4.14549206611985,39.021565753956));
#39822=CARTESIAN_POINT('Ctrl Pts',(21.7122572772988,4.14797524146931,38.988688409879));
#39823=CARTESIAN_POINT('Ctrl Pts',(21.7154875763281,4.14844412489215,38.982436656508));
#39824=CARTESIAN_POINT('Ctrl Pts',(21.720526001411,4.14918002380946,38.9725533164912));
#39825=CARTESIAN_POINT('Ctrl Pts',(21.7223569652164,4.14944842153987,38.9689335399071));
#39826=CARTESIAN_POINT('Ctrl Pts',(21.7257790516253,4.14995186101042,38.9621148334923));
#39827=CARTESIAN_POINT('Ctrl Pts',(21.7273726869371,4.15018705136142,38.958917296267));
#39828=CARTESIAN_POINT('Ctrl Pts',(21.7309928787426,4.1507230545483,38.9516027631778));
#39829=CARTESIAN_POINT('Ctrl Pts',(21.7330136341461,4.15102350724563,38.9474829540736));
#39830=CARTESIAN_POINT('Ctrl Pts',(21.7383371160596,4.15181849474477,38.9365310585155));
#39831=CARTESIAN_POINT('Ctrl Pts',(21.741614303752,4.15231150348907,38.9296865447176));
#39832=CARTESIAN_POINT('Ctrl Pts',(21.7645455375516,4.15578831687783,38.881059317478));
#39833=CARTESIAN_POINT('Ctrl Pts',(21.782736079792,4.1586899264795,38.8385983155602));
#39834=CARTESIAN_POINT('Ctrl Pts',(21.8483775526835,4.16992840428705,38.6687770040998));
#39835=CARTESIAN_POINT('Ctrl Pts',(21.8838432672033,4.17786655621265,38.5372034155286));
#39836=CARTESIAN_POINT('Ctrl Pts',(21.9191137959813,4.19141067832588,38.315421440436));
#39837=CARTESIAN_POINT('Ctrl Pts',(21.9269846003561,4.19684608140065,38.2270104531669));
#39838=CARTESIAN_POINT('Ctrl Pts',(21.9291537598222,4.20376805584826,38.1179970318635));
#39839=CARTESIAN_POINT('Ctrl Pts',(21.9292362129113,4.2050715705259,38.0976111477534));
#39840=CARTESIAN_POINT('Ctrl Pts',(21.9288915150063,4.20695322516967,38.068411605514));
#39841=CARTESIAN_POINT('Ctrl Pts',(21.928726988708,4.20752322980213,38.0595957660128));
#39842=CARTESIAN_POINT('Ctrl Pts',(21.9283366924082,4.20851543935505,38.0443030012272));
#39843=CARTESIAN_POINT('Ctrl Pts',(21.9281387086835,4.20893677564073,38.0378254607376));
#39844=CARTESIAN_POINT('Ctrl Pts',(21.9276948829095,4.20974960126028,38.0253615982893));
#39845=CARTESIAN_POINT('Ctrl Pts',(21.9274537837915,4.21014093835591,38.0193751738267));
#39846=CARTESIAN_POINT('Ctrl Pts',(21.9268183977011,4.21106741450524,38.0052370052318));
#39847=CARTESIAN_POINT('Ctrl Pts',(21.9264002623773,4.21160328901597,37.9970864996381));
#39848=CARTESIAN_POINT('Ctrl Pts',(21.9247554625591,4.2134849361767,37.9685637064755));
#39849=CARTESIAN_POINT('Ctrl Pts',(21.9232572733435,4.21483909494981,37.9482090373677));
#39850=CARTESIAN_POINT('Ctrl Pts',(21.9064037448299,4.22746569907763,37.760064279581));
#39851=CARTESIAN_POINT('Ctrl Pts',(21.8694524115591,4.23945025086013,37.5949698099316));
#39852=CARTESIAN_POINT('Ctrl Pts',(21.7871829664574,4.25651136278032,37.3702429510733));
#39853=CARTESIAN_POINT('Ctrl Pts',(21.7591590766849,4.26154278820361,37.3050603489156));
#39854=CARTESIAN_POINT('Ctrl Pts',(21.7129866767364,4.26871480059313,37.2121380036875));
#39855=CARTESIAN_POINT('Ctrl Pts',(21.6976142696946,4.27095650673691,37.1830875789581));
#39856=CARTESIAN_POINT('Ctrl Pts',(21.677961535863,4.2736404054824,37.1481386985485));
#39857=CARTESIAN_POINT('Ctrl Pts',(21.674381497976,4.2741224216295,37.1418552007371));
#39858=CARTESIAN_POINT('Ctrl Pts',(21.6687168063217,4.27487423995726,37.1320415392366));
#39859=CARTESIAN_POINT('Ctrl Pts',(21.6666561360965,4.27514552381159,37.128497716805));
#39860=CARTESIAN_POINT('Ctrl Pts',(21.6627821554753,4.2756513815485,37.1218840704373));
#39861=CARTESIAN_POINT('Ctrl Pts',(21.6609716506212,4.27588612158526,37.1188127373699));
#39862=CARTESIAN_POINT('Ctrl Pts',(21.6568070868866,4.27642228579682,37.1117925481952));
#39863=CARTESIAN_POINT('Ctrl Pts',(21.6544474228948,4.27672334401686,37.1078470798733));
#39864=CARTESIAN_POINT('Ctrl Pts',(21.6482260141954,4.2775100801253,37.0975285085451));
#39865=CARTESIAN_POINT('Ctrl Pts',(21.644341362562,4.27799431976521,37.0911692050837));
#39866=CARTESIAN_POINT('Ctrl Pts',(21.6175784991601,4.28128425784461,37.0479228137583));
#39867=CARTESIAN_POINT('Ctrl Pts',(21.5934958457844,4.28401739571738,37.0117912588766));
#39868=CARTESIAN_POINT('Ctrl Pts',(21.5534248197869,4.28827490104779,36.955859006142));
#39869=CARTESIAN_POINT('Ctrl Pts',(21.5382305669739,4.28982961080912,36.9355112308473));
#39870=CARTESIAN_POINT('Ctrl Pts',(21.4486015717401,4.29870298450599,36.8202989404192));
#39871=CARTESIAN_POINT('Ctrl Pts',(21.3658040358976,4.30577897366711,36.7322783520488));
#39872=CARTESIAN_POINT('Ctrl Pts',(21.2133281107126,4.31806957201341,36.5979328302725));
#39873=CARTESIAN_POINT('Ctrl Pts',(21.147888554101,4.32315217372693,36.5473505450703));
#39874=CARTESIAN_POINT('Ctrl Pts',(21.0631302496849,4.32964939455875,36.4901296304019));
#39875=CARTESIAN_POINT('Ctrl Pts',(21.0466807556305,4.33090631266937,36.4793865712917));
#39876=CARTESIAN_POINT('Ctrl Pts',(21.022725075516,4.33273243435239,36.464258134442));
#39877=CARTESIAN_POINT('Ctrl Pts',(21.0153484750424,4.33329415957168,36.4596690879567));
#39878=CARTESIAN_POINT('Ctrl Pts',(21.0024342418164,4.33427667781277,36.4517555210775));
#39879=CARTESIAN_POINT('Ctrl Pts',(20.9969104008234,4.3346966501722,36.448408669644));
#39880=CARTESIAN_POINT('Ctrl Pts',(20.9862025156749,4.33551026580209,36.4419941377709));
#39881=CARTESIAN_POINT('Ctrl Pts',(20.9810206986211,4.33590377303715,36.438922870964));
#39882=CARTESIAN_POINT('Ctrl Pts',(20.9686756167973,4.3368407782313,36.4316838463642));
#39883=CARTESIAN_POINT('Ctrl Pts',(20.9614997588273,4.33738505222762,36.4275379079875));
#39884=CARTESIAN_POINT('Ctrl Pts',(20.9359092066987,4.33932484826928,36.4129717865646));
#39885=CARTESIAN_POINT('Ctrl Pts',(20.9173506101544,4.34072945105316,36.4028087809869));
#39886=CARTESIAN_POINT('Ctrl Pts',(20.756386023795,4.35289808897262,36.3180732612595));
#39887=CARTESIAN_POINT('Ctrl Pts',(20.6053678323279,4.36430167294635,36.2612798463929));
#39888=CARTESIAN_POINT('Ctrl Pts',(20.3752160984411,4.38118371141086,36.2061872339147));
#39889=CARTESIAN_POINT('Ctrl Pts',(20.3003486242425,4.38658789881675,36.1928801400193));
#39890=CARTESIAN_POINT('Ctrl Pts',(20.1908774864044,4.39421567876447,36.1800310086192));
#39891=CARTESIAN_POINT('Ctrl Pts',(20.1567649979087,4.39655398616931,36.1769450777623));
#39892=CARTESIAN_POINT('Ctrl Pts',(20.1152795055091,4.39933707090263,36.1743035562436));
#39893=CARTESIAN_POINT('Ctrl Pts',(20.107970298142,4.39982513317179,36.1738799162987));
#39894=CARTESIAN_POINT('Ctrl Pts',(20.0965453393124,4.40058427269459,36.173282968261));
#39895=CARTESIAN_POINT('Ctrl Pts',(20.0924312397086,4.40085687836332,36.1730812187198));
#39896=CARTESIAN_POINT('Ctrl Pts',(20.0847577217977,4.4013638820609,36.1727295527508));
#39897=CARTESIAN_POINT('Ctrl Pts',(20.0811985701908,4.40159845418485,36.1725763203838));
#39898=CARTESIAN_POINT('Ctrl Pts',(20.0730749645417,4.40213253328741,36.172249116207));
#39899=CARTESIAN_POINT('Ctrl Pts',(20.068510309905,4.40243168509094,36.1720814957827));
#39900=CARTESIAN_POINT('Ctrl Pts',(20.0565955241875,4.40321016756088,36.1716863381664));
#39901=CARTESIAN_POINT('Ctrl Pts',(20.0492445272754,4.40368810854533,36.1714846092153));
#39902=CARTESIAN_POINT('Ctrl Pts',(20.0004644558289,4.40684509281832,36.1704250657989));
#39903=CARTESIAN_POINT('Ctrl Pts',(19.9590146427892,4.40945807098029,36.1708601835775));
#39904=CARTESIAN_POINT('Ctrl Pts',(19.9019037469233,4.41300153502812,36.1733015947855));
#39905=CARTESIAN_POINT('Ctrl Pts',(19.8862082919163,4.41396942925759,36.1741648333168));
#39906=CARTESIAN_POINT('Ctrl Pts',(19.7264549288851,4.42377583884161,36.1849110474046));
#39907=CARTESIAN_POINT('Ctrl Pts',(19.5839246020199,4.43218535577949,36.2107466641812));
#39908=CARTESIAN_POINT('Ctrl Pts',(19.4283607395475,4.44206076905504,36.2574215664436));
#39909=CARTESIAN_POINT('Ctrl Pts',(19.4111917622181,4.44316001812163,36.2628360542198));
#39910=CARTESIAN_POINT('Ctrl Pts',(19.3941039894965,4.44426476764078,36.2684889895619));
#39911=CARTESIAN_POINT('Origin',(20.,-1.3495818343519,38.1));
#39912=CARTESIAN_POINT('',(19.3941040111825,5.40852741588127,36.2684889823878));
#39913=CARTESIAN_POINT('',(19.3941040060237,5.23819447890751,36.2684889840944));
#39914=CARTESIAN_POINT('',(19.3941040087494,-1.3495818343519,36.2684889831927));
#39915=CARTESIAN_POINT('',(18.0708700373369,4.77280515976688,38.1003795462754));
#39916=CARTESIAN_POINT('Ctrl Pts',(19.3941040111825,5.40852741588127,36.2684889823878));
#39917=CARTESIAN_POINT('Ctrl Pts',(19.3991880386128,5.40816538004886,36.2668070968859));
#39918=CARTESIAN_POINT('Ctrl Pts',(19.4042794078024,5.40780435168272,36.2651462681862));
#39919=CARTESIAN_POINT('Ctrl Pts',(19.4182817146625,5.40681577153768,36.2606430827172));
#39920=CARTESIAN_POINT('Ctrl Pts',(19.4272063677185,5.40619047202091,36.2578443344489));
#39921=CARTESIAN_POINT('Ctrl Pts',(19.4404955126092,5.40526684166842,36.2537828077251));
#39922=CARTESIAN_POINT('Ctrl Pts',(19.4448445160974,5.40496575700304,36.2524704110074));
#39923=CARTESIAN_POINT('Ctrl Pts',(19.452610240741,5.40443028746982,36.2501568488366));
#39924=CARTESIAN_POINT('Ctrl Pts',(19.4560251273567,5.40419556585668,36.249149770754));
#39925=CARTESIAN_POINT('Ctrl Pts',(19.463413492578,5.40368934441415,36.2469930960361));
#39926=CARTESIAN_POINT('Ctrl Pts',(19.4673878774805,5.40341803749983,36.2458468256842));
#39927=CARTESIAN_POINT('Ctrl Pts',(19.4784833004892,5.40266333395217,36.242685363713));
#39928=CARTESIAN_POINT('Ctrl Pts',(19.4856123876216,5.40218152877578,36.2406983260948));
#39929=CARTESIAN_POINT('Ctrl Pts',(19.5270290774137,5.39939953049861,36.2294110067447));
#39930=CARTESIAN_POINT('Ctrl Pts',(19.5615594513908,5.39714775831503,36.2210175763786));
#39931=CARTESIAN_POINT('Ctrl Pts',(19.6754367559842,5.38988300878024,36.1966477094285));
#39932=CARTESIAN_POINT('Ctrl Pts',(19.755563058445,5.38502298326522,36.1847078517655));
#39933=CARTESIAN_POINT('Ctrl Pts',(19.9892148545015,5.37100147069778,36.1647978810955));
#39934=CARTESIAN_POINT('Ctrl Pts',(20.1432110042299,5.36189891966423,36.1700756734619));
#39935=CARTESIAN_POINT('Ctrl Pts',(20.3163850670617,5.35079429111706,36.1968674091198));
#39936=CARTESIAN_POINT('Ctrl Pts',(20.3377654206367,5.34940903980329,36.2005454389709));
#39937=CARTESIAN_POINT('Ctrl Pts',(20.367306935802,5.34747333968377,36.206141951392));
#39938=CARTESIAN_POINT('Ctrl Pts',(20.3755249855877,5.34693251874736,36.2077543301815));
#39939=CARTESIAN_POINT('Ctrl Pts',(20.389657692763,5.34599832276291,36.2106228545689));
#39940=CARTESIAN_POINT('Ctrl Pts',(20.3955774703059,5.345605761296,36.211853401133));
#39941=CARTESIAN_POINT('Ctrl Pts',(20.407795319013,5.34479291347448,36.2144531099749));
#39942=CARTESIAN_POINT('Ctrl Pts',(20.4140925016412,5.34437251192991,36.2158260443658));
#39943=CARTESIAN_POINT('Ctrl Pts',(20.4287796832729,5.34338853929661,36.219105381491));
#39944=CARTESIAN_POINT('Ctrl Pts',(20.4371639901137,5.34282419148356,36.2210363961933));
#39945=CARTESIAN_POINT('Ctrl Pts',(20.4641954662249,5.34099600686718,36.2274528152222));
#39946=CARTESIAN_POINT('Ctrl Pts',(20.4827882596725,5.33972512874099,36.2321601135299));
#39947=CARTESIAN_POINT('Ctrl Pts',(20.5775418096149,5.33317740889568,36.2576589345189));
#39948=CARTESIAN_POINT('Ctrl Pts',(20.6524352235758,5.32776143054545,36.2828317214629));
#39949=CARTESIAN_POINT('Ctrl Pts',(20.8244499607132,5.31476284712281,36.3526553247381));
#39950=CARTESIAN_POINT('Ctrl Pts',(20.9198261878247,5.3071043875358,36.4009272180223));
#39951=CARTESIAN_POINT('Ctrl Pts',(21.0833401702788,5.29345537040106,36.5015048252585));
#39952=CARTESIAN_POINT('Ctrl Pts',(21.1529342694767,5.28745766014602,36.5509490243489));
#39953=CARTESIAN_POINT('Ctrl Pts',(21.2262930487584,5.28109591982131,36.6107600549694));
#39954=CARTESIAN_POINT('Ctrl Pts',(21.2335081166738,5.28046981538039,36.6167306414235));
#39955=CARTESIAN_POINT('Ctrl Pts',(21.2441599536157,5.27954523057099,36.6256766895956));
#39956=CARTESIAN_POINT('Ctrl Pts',(21.2476300144534,5.27924398825386,36.6286120287744));
#39957=CARTESIAN_POINT('Ctrl Pts',(21.253799918635,5.27870834755838,36.6338686969156));
#39958=CARTESIAN_POINT('Ctrl Pts',(21.256503733473,5.2784736115598,36.6361852568228));
#39959=CARTESIAN_POINT('Ctrl Pts',(21.2623335794094,5.27796748288926,36.641208175672));
#39960=CARTESIAN_POINT('Ctrl Pts',(21.2654573212146,5.2776962824748,36.6439170966567));
#39961=CARTESIAN_POINT('Ctrl Pts',(21.2741421257917,5.27694217628809,36.6514976502051));
#39962=CARTESIAN_POINT('Ctrl Pts',(21.279684002884,5.27646085788835,36.6563913026208));
#39963=CARTESIAN_POINT('Ctrl Pts',(21.3115989454433,5.27368739919953,36.6849014090007));
#39964=CARTESIAN_POINT('Ctrl Pts',(21.33734801797,5.27144333296209,36.7092101241971));
#39965=CARTESIAN_POINT('Ctrl Pts',(21.4193583595566,5.26421625782154,36.7910181642371));
#39966=CARTESIAN_POINT('Ctrl Pts',(21.4726982577235,5.25938439338078,36.8513312674988));
#39967=CARTESIAN_POINT('Ctrl Pts',(21.6168920359138,5.24534938687466,37.0365159122747));
#39968=CARTESIAN_POINT('Ctrl Pts',(21.6967120389538,5.23620868997918,37.1691400404125));
#39969=CARTESIAN_POINT('Ctrl Pts',(21.7687537429784,5.22506217988023,37.329596580366));
#39970=CARTESIAN_POINT('Ctrl Pts',(21.7772875536383,5.22367973924915,37.3494934217528));
#39971=CARTESIAN_POINT('Ctrl Pts',(21.7886528771772,5.22174734839289,37.3772735934065));
#39972=CARTESIAN_POINT('Ctrl Pts',(21.791770835588,5.22120698238419,37.3850385724048));
#39973=CARTESIAN_POINT('Ctrl Pts',(21.7970539114562,5.22027336167576,37.3984471994491));
#39974=CARTESIAN_POINT('Ctrl Pts',(21.7992432202646,5.21988091822332,37.4040812363545));
#39975=CARTESIAN_POINT('Ctrl Pts',(21.8037125515931,5.2190681166288,37.4157448271036));
#39976=CARTESIAN_POINT('Ctrl Pts',(21.8059888997665,5.21864764242066,37.4217756988706));
#39977=CARTESIAN_POINT('Ctrl Pts',(21.8112351841841,5.2176631552338,37.4358887101227));
#39978=CARTESIAN_POINT('Ctrl Pts',(21.8141813016587,5.21709836309307,37.4439794984682));
#39979=CARTESIAN_POINT('Ctrl Pts',(21.823526929673,5.21526727872232,37.470189434586));
#39980=CARTESIAN_POINT('Ctrl Pts',(21.8297097400797,5.21399391392181,37.4883840801368));
#39981=CARTESIAN_POINT('Ctrl Pts',(21.8599896001415,5.20742419681477,37.5820622514077));
#39982=CARTESIAN_POINT('Ctrl Pts',(21.8796883574583,5.20198765216723,37.6588768843063));
#39983=CARTESIAN_POINT('Ctrl Pts',(21.9148823678888,5.18890137058507,37.8424016046207));
#39984=CARTESIAN_POINT('Ctrl Pts',(21.9262707062528,5.18117351364258,37.9496339572141));
#39985=CARTESIAN_POINT('Ctrl Pts',(21.9305178212104,5.1675522919379,38.1412273996601));
#39986=CARTESIAN_POINT('Ctrl Pts',(21.9268924371506,5.16164723017443,38.2252508842666));
#39987=CARTESIAN_POINT('Ctrl Pts',(21.9167865730074,5.15537112069426,38.3180810335139));
#39988=CARTESIAN_POINT('Ctrl Pts',(21.9157062698766,5.1547455644404,38.3273754601042));
#39989=CARTESIAN_POINT('Ctrl Pts',(21.914000984888,5.15382162964296,38.341170954119));
#39990=CARTESIAN_POINT('Ctrl Pts',(21.9134276764655,5.15352049468112,38.3456780968006));
#39991=CARTESIAN_POINT('Ctrl Pts',(21.9123767133476,5.15298497055235,38.3537134981451));
#39992=CARTESIAN_POINT('Ctrl Pts',(21.9119052106441,5.15275024436098,38.3572424909046));
#39993=CARTESIAN_POINT('Ctrl Pts',(21.9108648716343,5.15224405256711,38.3648680880695));
#39994=CARTESIAN_POINT('Ctrl Pts',(21.9102926320763,5.1519727796697,38.368964165555));
#39995=CARTESIAN_POINT('Ctrl Pts',(21.9086600405253,5.15121826693924,38.3803821320283));
#39996=CARTESIAN_POINT('Ctrl Pts',(21.9075707218813,5.15073661725777,38.3876999054512));
#39997=CARTESIAN_POINT('Ctrl Pts',(21.9010125764314,5.14795735063021,38.4300803265439));
#39998=CARTESIAN_POINT('Ctrl Pts',(21.8946188116473,5.14570804350205,38.4649955927218));
#39999=CARTESIAN_POINT('Ctrl Pts',(21.870530159364,5.13845536235766,38.5787301842942));
#40000=CARTESIAN_POINT('Ctrl Pts',(21.8488484789114,5.13360436001436,38.6566211905362));
#40001=CARTESIAN_POINT('Ctrl Pts',(21.7718904546084,5.11957855216328,38.8782007162131));
#40002=CARTESIAN_POINT('Ctrl Pts',(21.704253625311,5.11046379542079,39.0168999175403));
#40003=CARTESIAN_POINT('Ctrl Pts',(21.6091173859968,5.0993457601127,39.164309069245));
#40004=CARTESIAN_POINT('Ctrl Pts',(21.5970556067822,5.09796139676457,39.1823242977118));
#40005=CARTESIAN_POINT('Ctrl Pts',(21.5799185485579,5.09602674192398,39.2070095011182));
#40006=CARTESIAN_POINT('Ctrl Pts',(21.5750992730607,5.09548606449814,39.2138558847679));
#40007=CARTESIAN_POINT('Ctrl Pts',(21.5667235417695,5.09455205000147,39.2255916007818));
#40008=CARTESIAN_POINT('Ctrl Pts',(21.5631883589015,5.09415952577516,39.2304960244514));
#40009=CARTESIAN_POINT('Ctrl Pts',(21.5558367501928,5.09334669260483,39.2405946290237));
#40010=CARTESIAN_POINT('Ctrl Pts',(21.5520172342859,5.09292626819478,39.2457864564574));
#40011=CARTESIAN_POINT('Ctrl Pts',(21.543037332928,5.09194213351084,39.2578654533845));
#40012=CARTESIAN_POINT('Ctrl Pts',(21.5378567697963,5.09137764574495,39.264737382631));
#40013=CARTESIAN_POINT('Ctrl Pts',(21.5209758615354,5.08954854810378,39.2868206545022));
#40014=CARTESIAN_POINT('Ctrl Pts',(21.5090947730772,5.08827688707479,39.3018917414638));
#40015=CARTESIAN_POINT('Ctrl Pts',(21.4471388807125,5.081722245921,39.3781152364297));
#40016=CARTESIAN_POINT('Ctrl Pts',(21.3935710607686,5.0762997974627,39.4363181945111));
#40017=CARTESIAN_POINT('Ctrl Pts',(21.2594148184122,5.06327242541221,39.5652207857936));
#40018=CARTESIAN_POINT('Ctrl Pts',(21.1762041270946,5.05559087341416,39.6328205580282));
#40019=CARTESIAN_POINT('Ctrl Pts',(21.0774565754292,5.04709028615795,39.7002460795997));
#40020=CARTESIAN_POINT('Ctrl Pts',(21.0670190235063,5.04619911305068,39.7072245010125));
#40021=CARTESIAN_POINT('Ctrl Pts',(20.9958672822816,5.04017643008372,39.7537970694446));
#40022=CARTESIAN_POINT('Ctrl Pts',(20.9330238544696,5.03511094492634,39.7900489264387));
#40023=CARTESIAN_POINT('Ctrl Pts',(20.8600341311524,5.02961846174217,39.8268379082042));
#40024=CARTESIAN_POINT('Ctrl Pts',(20.8517562293733,5.02900104103948,39.8309359323856));
#40025=CARTESIAN_POINT('Ctrl Pts',(20.8393842972494,5.02808675963082,39.836950484352));
#40026=CARTESIAN_POINT('Ctrl Pts',(20.835312597504,5.02778722399254,39.8389122603063));
#40027=CARTESIAN_POINT('Ctrl Pts',(20.8280228471142,5.02725343063717,39.8423930050124));
#40028=CARTESIAN_POINT('Ctrl Pts',(20.8248074634435,5.02701884477712,39.8439173914519));
#40029=CARTESIAN_POINT('Ctrl Pts',(20.817830389544,5.02651168629267,39.8472015502006));
#40030=CARTESIAN_POINT('Ctrl Pts',(20.8140672379939,5.02623931314037,39.8489580715139));
#40031=CARTESIAN_POINT('Ctrl Pts',(20.8035134062977,5.02547862131503,39.8538428267433));
#40032=CARTESIAN_POINT('Ctrl Pts',(20.7967100787733,5.02499193530327,39.856943798148));
#40033=CARTESIAN_POINT('Ctrl Pts',(20.7563064467096,5.02212234113683,39.8750769120927));
#40034=CARTESIAN_POINT('Ctrl Pts',(20.7222969509855,5.0197914882729,39.8891855766013));
#40035=CARTESIAN_POINT('Ctrl Pts',(20.6074214476066,5.01213089552774,39.9330309380568));
#40036=CARTESIAN_POINT('Ctrl Pts',(20.5249668171731,5.00697376221909,39.9583260107477));
#40037=CARTESIAN_POINT('Ctrl Pts',(20.2985948255472,4.99308047694332,40.0114939398307));
#40038=CARTESIAN_POINT('Ctrl Pts',(20.1527711204213,4.98437252386747,40.0286323320604));
#40039=CARTESIAN_POINT('Ctrl Pts',(19.9843492298928,4.97370358268398,40.029192758108));
#40040=CARTESIAN_POINT('Ctrl Pts',(19.9622804120588,4.97229465559702,40.0288874549252));
#40041=CARTESIAN_POINT('Ctrl Pts',(19.9317928362042,4.97033115840127,40.0279422878542));
#40042=CARTESIAN_POINT('Ctrl Pts',(19.9233652031772,4.96978658820653,40.0276256863591));
#40043=CARTESIAN_POINT('Ctrl Pts',(19.9088841305744,4.96884764690859,40.026986559511));
#40044=CARTESIAN_POINT('Ctrl Pts',(19.9028295875198,4.96845410868939,40.0266907410753));
#40045=CARTESIAN_POINT('Ctrl Pts',(19.8903491526946,4.96764085612944,40.0260219830605));
#40046=CARTESIAN_POINT('Ctrl Pts',(19.8839235394651,4.96722103375196,40.0256454089933));
#40047=CARTESIAN_POINT('Ctrl Pts',(19.8689673897648,4.96624120850582,40.0246937709874));
#40048=CARTESIAN_POINT('Ctrl Pts',(19.860438605458,4.96568044855747,40.024094142762));
#40049=CARTESIAN_POINT('Ctrl Pts',(19.8330882180428,4.96387556747299,40.0219884319284));
#40050=CARTESIAN_POINT('Ctrl Pts',(19.8142851176624,4.96262465351862,40.0202627463547));
#40051=CARTESIAN_POINT('Ctrl Pts',(19.7192938011134,4.95625210490988,40.0101365527305));
#40052=CARTESIAN_POINT('Ctrl Pts',(19.6436383609901,4.95099958533525,39.9974776316555));
#40053=CARTESIAN_POINT('Ctrl Pts',(19.4862357178023,4.93970717476183,39.9613943682751));
#40054=CARTESIAN_POINT('Ctrl Pts',(19.4048730934031,4.93365443209155,39.9369989096747));
#40055=CARTESIAN_POINT('Ctrl Pts',(19.2221401898552,4.91973806694476,39.8687909955374));
#40056=CARTESIAN_POINT('Ctrl Pts',(19.1223734372587,4.91189504265054,39.821471747952));
#40057=CARTESIAN_POINT('Ctrl Pts',(19.0192827156919,4.90387420619512,39.7612705672334));
#40058=CARTESIAN_POINT('Ctrl Pts',(19.0114135771843,4.90326259359369,39.7565998859226));
#40059=CARTESIAN_POINT('Ctrl Pts',(18.9997223945682,4.90235521155407,39.7495476778188));
#40060=CARTESIAN_POINT('Ctrl Pts',(18.9958751114022,4.90205682467886,39.7472085594865));
#40061=CARTESIAN_POINT('Ctrl Pts',(18.9890760845084,4.90152992900205,39.7430421312622));
#40062=CARTESIAN_POINT('Ctrl Pts',(18.9861210599646,4.90130107177643,39.7412203092905));
#40063=CARTESIAN_POINT('Ctrl Pts',(18.9797363722117,4.9008069180052,39.7372602177558));
#40064=CARTESIAN_POINT('Ctrl Pts',(18.976308514043,4.9005418079512,39.7351191495283));
#40065=CARTESIAN_POINT('Ctrl Pts',(18.9692168010084,4.89999368540055,39.7306585654015));
#40066=CARTESIAN_POINT('Ctrl Pts',(18.9655539828095,4.89971077855935,39.7283374339005));
#40067=CARTESIAN_POINT('Ctrl Pts',(18.9562632785317,4.89899359971221,39.7224059048746));
#40068=CARTESIAN_POINT('Ctrl Pts',(18.950646225,4.89856038749363,39.7187785277426));
#40069=CARTESIAN_POINT('Ctrl Pts',(18.9344906281144,4.89731516510938,39.7082261490912));
#40070=CARTESIAN_POINT('Ctrl Pts',(18.9240007615181,4.89650759034226,39.7012267877368));
#40071=CARTESIAN_POINT('Ctrl Pts',(18.8837340273822,4.89340818782832,39.6737844039996));
#40072=CARTESIAN_POINT('Ctrl Pts',(18.8544632186173,4.89115635348185,39.6526084161405));
#40073=CARTESIAN_POINT('Ctrl Pts',(18.6825985095421,4.87783010040515,39.5207645270164));
#40074=CARTESIAN_POINT('Ctrl Pts',(18.5555166480364,4.86744540559465,39.3913538853965));
#40075=CARTESIAN_POINT('Ctrl Pts',(18.4175652353201,4.85309467892754,39.2045874550899));
#40076=CARTESIAN_POINT('Ctrl Pts',(18.3885465122739,4.84985078677518,39.1618051392593));
#40077=CARTESIAN_POINT('Ctrl Pts',(18.35453675329,4.84572370455568,39.1070534604185));
#40078=CARTESIAN_POINT('Ctrl Pts',(18.3478998601058,4.84490138031002,39.0961280457177));
#40079=CARTESIAN_POINT('Ctrl Pts',(18.3375945820565,4.84359697460574,39.0787775562806));
#40080=CARTESIAN_POINT('Ctrl Pts',(18.3338536573346,4.8431175178173,39.0723958250589));
#40081=CARTESIAN_POINT('Ctrl Pts',(18.3269724457064,4.84222435823489,39.0605007114706));
#40082=CARTESIAN_POINT('Ctrl Pts',(18.3238224657101,4.84181101045498,39.054993029345));
#40083=CARTESIAN_POINT('Ctrl Pts',(18.3169098517817,4.84089384334767,39.0427668876078));
#40084=CARTESIAN_POINT('Ctrl Pts',(18.3131601737517,4.84038957097797,39.0360412646298));
#40085=CARTESIAN_POINT('Ctrl Pts',(18.3024426141714,4.83892836677434,39.0165441288778));
#40086=CARTESIAN_POINT('Ctrl Pts',(18.2955789367443,4.83796778011384,39.003716237477));
#40087=CARTESIAN_POINT('Ctrl Pts',(18.2427058215877,4.8303671046717,38.902153598844));
#40088=CARTESIAN_POINT('Ctrl Pts',(18.2035182023266,4.82349015899611,38.8100567514915));
#40089=CARTESIAN_POINT('Ctrl Pts',(18.1185161939014,4.80472129942341,38.5574958819093));
#40090=CARTESIAN_POINT('Ctrl Pts',(18.0860555955714,4.79257447840611,38.3934294727711));
#40091=CARTESIAN_POINT('Ctrl Pts',(18.0739063613322,4.7800373981577,38.2096236511995));
#40092=CARTESIAN_POINT('Ctrl Pts',(18.0729840017851,4.77884665265958,38.1919969931562));
#40093=CARTESIAN_POINT('Ctrl Pts',(18.0720702781831,4.77726412508938,38.1683095854994));
#40094=CARTESIAN_POINT('Ctrl Pts',(18.0718653881356,4.77686141086359,38.1622585953465));
#40095=CARTESIAN_POINT('Ctrl Pts',(18.0715882886031,4.7762312450856,38.1527519949349));
#40096=CARTESIAN_POINT('Ctrl Pts',(18.0714968750493,4.77600275151252,38.1492970500773));
#40097=CARTESIAN_POINT('Ctrl Pts',(18.0713331534435,4.77554829423259,38.1424092147729));
#40098=CARTESIAN_POINT('Ctrl Pts',(18.0712607265042,4.77532233398187,38.1389764229896));
#40099=CARTESIAN_POINT('Ctrl Pts',(18.0711324168621,4.77486506854656,38.1320135525227));
#40100=CARTESIAN_POINT('Ctrl Pts',(18.071077059447,4.77463379472688,38.1284835167032));
#40101=CARTESIAN_POINT('Ctrl Pts',(18.070974109491,4.77411359661182,38.1205251656839));
#40102=CARTESIAN_POINT('Ctrl Pts',(18.0709320739607,4.77382497325852,38.1160967804167));
#40103=CARTESIAN_POINT('Ctrl Pts',(18.0708825280288,4.77329258062598,38.1079054148909));
#40104=CARTESIAN_POINT('Ctrl Pts',(18.0708707776788,4.77304859236824,38.1041425018261));
#40105=CARTESIAN_POINT('Ctrl Pts',(18.0708700373369,4.77280515976688,38.1003795462754));
#40106=CARTESIAN_POINT('Ctrl Pts',(18.0708700375362,4.77280522521772,38.1003805580074));
#40107=CARTESIAN_POINT('Ctrl Pts',(18.0708659381183,4.7714608743111,38.0795997316186));
#40108=CARTESIAN_POINT('Ctrl Pts',(18.0711976193021,4.77013355924366,38.0588190267461));
#40109=CARTESIAN_POINT('Ctrl Pts',(18.074831050733,4.76298387999448,37.945738140098));
#40110=CARTESIAN_POINT('Ctrl Pts',(18.0844224177032,4.75742956583471,37.8537511740746));
#40111=CARTESIAN_POINT('Ctrl Pts',(18.115987995365,4.74662860232346,37.6759454899839));
#40112=CARTESIAN_POINT('Ctrl Pts',(18.1373451636114,4.74139091150783,37.5902551835509));
#40113=CARTESIAN_POINT('Ctrl Pts',(18.1868297277635,4.73161359693041,37.4372586891911));
#40114=CARTESIAN_POINT('Ctrl Pts',(18.2130484885359,4.72712347764275,37.3695104302234));
#40115=CARTESIAN_POINT('Ctrl Pts',(18.2505950579448,4.72133855539074,37.2866971946763));
#40116=CARTESIAN_POINT('Ctrl Pts',(18.2584080737755,4.72016375086269,37.270098421495));
#40117=CARTESIAN_POINT('Ctrl Pts',(18.2701642514357,4.71843591550264,37.2460197536588));
#40118=CARTESIAN_POINT('Ctrl Pts',(18.2739219028291,4.71788927179635,37.2384500148661));
#40119=CARTESIAN_POINT('Ctrl Pts',(18.2806221909896,4.71692420705392,37.2251721623131));
#40120=CARTESIAN_POINT('Ctrl Pts',(18.2835438385288,4.71650652039566,37.2194535561385));
#40121=CARTESIAN_POINT('Ctrl Pts',(18.2892925807152,4.71569065020415,37.2083387452328));
#40122=CARTESIAN_POINT('Ctrl Pts',(18.2921167933324,4.71529257131145,37.2029411286855));
#40123=CARTESIAN_POINT('Ctrl Pts',(18.2997688409181,4.71422122988123,37.1884837081666));
#40124=CARTESIAN_POINT('Ctrl Pts',(18.3046434530014,4.71354632791796,37.1794490148496));
#40125=CARTESIAN_POINT('Ctrl Pts',(18.3229109258643,4.71104442305891,37.1462290184723));
#40126=CARTESIAN_POINT('Ctrl Pts',(18.3367505631413,4.70920166940098,37.1222945102947));
#40127=CARTESIAN_POINT('Ctrl Pts',(18.3528646417998,4.70711193484323,37.0957593724653));
#40128=CARTESIAN_POINT('Ctrl Pts',(18.3546378323777,4.70688270825547,37.0928567811197));
#40129=CARTESIAN_POINT('Ctrl Pts',(18.4417382973849,4.69565830386941,36.9511232431792));
#40130=CARTESIAN_POINT('Ctrl Pts',(18.5442928323567,4.6840110782204,36.8236793464117));
#40131=CARTESIAN_POINT('Ctrl Pts',(18.7274353646957,4.66590323811408,36.6472522025695));
#40132=CARTESIAN_POINT('Ctrl Pts',(18.7976941549391,4.65945113761711,36.588589507283));
#40133=CARTESIAN_POINT('Ctrl Pts',(18.8775045924654,4.65283130777619,36.5310528679023));
#40134=CARTESIAN_POINT('Ctrl Pts',(18.8831751334614,4.6523646207483,36.5270113591505));
#40135=CARTESIAN_POINT('Ctrl Pts',(18.8925059175718,4.65160282285846,36.5204370148893));
#40136=CARTESIAN_POINT('Ctrl Pts',(18.8961532054959,4.65130656698276,36.5178860275668));
#40137=CARTESIAN_POINT('Ctrl Pts',(18.9031995789978,4.65073719188104,36.5129938792128));
#40138=CARTESIAN_POINT('Ctrl Pts',(18.9065974090099,4.6504639582083,36.5106509616404));
#40139=CARTESIAN_POINT('Ctrl Pts',(18.9100169678687,4.65019032563652,36.5083092175733));
#40140=CARTESIAN_POINT('Ctrl Pts',(18.9100311645579,4.65018918964293,36.5082994958344));
#40141=CARTESIAN_POINT('Ctrl Pts',(18.9100596875963,4.65018690732738,36.5082799641273));
#40142=CARTESIAN_POINT('Ctrl Pts',(18.9100740139145,4.65018576100832,36.5082701541854));
#40143=CARTESIAN_POINT('Ctrl Pts',(18.9101027990276,4.65018345781774,36.5082504441591));
#40144=CARTESIAN_POINT('Ctrl Pts',(18.9101172577129,4.65018230095543,36.5082405441551));
#40145=CARTESIAN_POINT('Ctrl Pts',(18.9101463102378,4.65017997646543,36.5082206521868));
#40146=CARTESIAN_POINT('Ctrl Pts',(18.910160904294,4.65017880882086,36.5082106600798));
#40147=CARTESIAN_POINT('Ctrl Pts',(18.9101902306377,4.65017646252155,36.5081905818154));
#40148=CARTESIAN_POINT('Ctrl Pts',(18.9102049627863,4.65017528387839,36.5081804957587));
#40149=CARTESIAN_POINT('Ctrl Pts',(18.9102345682621,4.65017291534747,36.5081602275939));
#40150=CARTESIAN_POINT('Ctrl Pts',(18.9102494417545,4.65017172544699,36.5081500453785));
#40151=CARTESIAN_POINT('Ctrl Pts',(18.9102793332182,4.65016933413889,36.5081295826545));
#40152=CARTESIAN_POINT('Ctrl Pts',(18.9102943509284,4.65016813275265,36.5081193023305));
#40153=CARTESIAN_POINT('Ctrl Pts',(18.9103245340155,4.65016571821952,36.5080986412252));
#40154=CARTESIAN_POINT('Ctrl Pts',(18.9103396993734,4.65016450507465,36.5080882604629));
#40155=CARTESIAN_POINT('Ctrl Pts',(18.9103701810668,4.65016206676097,36.5080673962331));
#40156=CARTESIAN_POINT('Ctrl Pts',(18.9103854972447,4.65016084160528,36.5080569128798));
#40157=CARTESIAN_POINT('Ctrl Pts',(18.9104162836217,4.6501583790281,36.5080358414039));
#40158=CARTESIAN_POINT('Ctrl Pts',(18.9104317542608,4.65015714157195,36.5080252529866));
#40159=CARTESIAN_POINT('Ctrl Pts',(18.9104628534336,4.65015465408568,36.5080039687516));
#40160=CARTESIAN_POINT('Ctrl Pts',(18.9104784815412,4.6501534040902,36.5079932732322));
#40161=CARTESIAN_POINT('Ctrl Pts',(18.9105098989393,4.65015089126395,36.5079717725629));
#40162=CARTESIAN_POINT('Ctrl Pts',(18.9105256887033,4.6501496283959,36.5079609670958));
#40163=CARTESIAN_POINT('Ctrl Pts',(18.9105574331311,4.650147089529,36.5079392440086));
#40164=CARTESIAN_POINT('Ctrl Pts',(18.9105733878038,4.65014581353005,36.5079283263897));
#40165=CARTESIAN_POINT('Ctrl Pts',(18.910605466169,4.65014324807367,36.5079063762012));
#40166=CARTESIAN_POINT('Ctrl Pts',(18.9106215896509,4.65014195863372,36.5078953437833));
#40167=CARTESIAN_POINT('Ctrl Pts',(18.910654009238,4.65013936600904,36.5078731615538));
#40168=CARTESIAN_POINT('Ctrl Pts',(18.9106703057407,4.65013806279318,36.507862011478));
#40169=CARTESIAN_POINT('Ctrl Pts',(18.9107030758268,4.6501354422622,36.5078395909064));
#40170=CARTESIAN_POINT('Ctrl Pts',(18.9107195489025,4.65013412498835,36.5078283207659));
#40171=CARTESIAN_POINT('Ctrl Pts',(18.9107526761783,4.65013147602005,36.5078056573225));
#40172=CARTESIAN_POINT('Ctrl Pts',(18.9107693305324,4.65013014431397,36.5077942639224));
#40173=CARTESIAN_POINT('Ctrl Pts',(18.9108028243766,4.65012746616255,36.5077713512406));
#40174=CARTESIAN_POINT('Ctrl Pts',(18.9108196641439,4.65012611969576,36.5077598317777));
#40175=CARTESIAN_POINT('Ctrl Pts',(18.9136961643979,4.64989612733629,36.5057921911733));
#40176=CARTESIAN_POINT('Ctrl Pts',(18.9165610486414,4.64966801310293,36.5038438046669));
#40177=CARTESIAN_POINT('Ctrl Pts',(18.923219567189,4.64914001170268,36.4993415825901));
#40178=CARTESIAN_POINT('Ctrl Pts',(18.9270170416057,4.64884051157304,36.4967935124357));
#40179=CARTESIAN_POINT('Ctrl Pts',(18.9382979926108,4.64795550385276,36.4892821352962));
#40180=CARTESIAN_POINT('Ctrl Pts',(18.9458072294981,4.64737249428316,36.4843574645493));
#40181=CARTESIAN_POINT('Ctrl Pts',(19.045155588486,4.63973533297612,36.4201908855883));
#40182=CARTESIAN_POINT('Ctrl Pts',(19.1418482235563,4.63314897649412,36.368795374594));
#40183=CARTESIAN_POINT('Ctrl Pts',(19.2921450377107,4.62337030233198,36.3046139053964));
#40184=CARTESIAN_POINT('Ctrl Pts',(19.3427625414602,4.62015039871559,36.2854736404772));
#40185=CARTESIAN_POINT('Ctrl Pts',(19.3941040488142,4.61690666843697,36.2684889699386));
#40186=CARTESIAN_POINT('Ctrl Pts',(19.3941039894965,4.44426476764078,36.2684889895619));
#40187=CARTESIAN_POINT('Ctrl Pts',(19.342277380928,4.44761543374737,36.2856341419474));
#40188=CARTESIAN_POINT('Ctrl Pts',(19.2911978070745,4.45101761072027,36.3049726973428));
#40189=CARTESIAN_POINT('Ctrl Pts',(19.2241346286758,4.45565854241324,36.3336727032339));
#40190=CARTESIAN_POINT('Ctrl Pts',(19.2073710249909,4.45683350062566,36.3411314816783));
#40191=CARTESIAN_POINT('Ctrl Pts',(19.1830448952451,4.4585615195637,36.352373511768));
#40192=CARTESIAN_POINT('Ctrl Pts',(19.1753964688773,4.45910819119435,36.3559693241574));
#40193=CARTESIAN_POINT('Ctrl Pts',(19.1619785271181,4.46007328703411,36.3623855987767));
#40194=CARTESIAN_POINT('Ctrl Pts',(19.1561989663204,4.46049097670208,36.3651848483913));
#40195=CARTESIAN_POINT('Ctrl Pts',(19.1449643782537,4.46130683904334,36.3706955874682));
#40196=CARTESIAN_POINT('Ctrl Pts',(19.1395079999423,4.46170490701279,36.3734041636602));
#40197=CARTESIAN_POINT('Ctrl Pts',(19.1248917813527,4.46277618548764,36.3807462275481));
#40198=CARTESIAN_POINT('Ctrl Pts',(19.1157560450749,4.46345103507833,36.3854270065885));
#40199=CARTESIAN_POINT('Ctrl Pts',(19.0821602772416,4.46595251512275,36.4029800291943));
#40200=CARTESIAN_POINT('Ctrl Pts',(19.0579413626133,4.46779488933996,36.4163040868929));
#40201=CARTESIAN_POINT('Ctrl Pts',(19.0283577232081,4.47009545444076,36.4334176875645));
#40202=CARTESIAN_POINT('Ctrl Pts',(19.0227141205297,4.47053661958971,36.436720821322));
#40203=CARTESIAN_POINT('Ctrl Pts',(18.8723464484676,4.48235256536877,36.5257587411399));
#40204=CARTESIAN_POINT('Ctrl Pts',(18.7394577072785,4.49441976552719,36.6300168299211));
#40205=CARTESIAN_POINT('Ctrl Pts',(18.5806972833031,4.51054637765621,36.792111353641));
#40206=CARTESIAN_POINT('Ctrl Pts',(18.5415308272271,4.5146892878991,36.8359345002157));
#40207=CARTESIAN_POINT('Ctrl Pts',(18.4859577526585,4.52075047293521,36.9041433057419));
#40208=CARTESIAN_POINT('Ctrl Pts',(18.4680088508538,4.52273981546695,36.9272252953545));
#40209=CARTESIAN_POINT('Ctrl Pts',(18.446435470455,4.52516240532702,36.9563092860602));
#40210=CARTESIAN_POINT('Ctrl Pts',(18.4423108607557,4.52562707034779,36.9619333298244));
#40211=CARTESIAN_POINT('Ctrl Pts',(18.4358437074141,4.52635785116144,36.9708525375414));
#40212=CARTESIAN_POINT('Ctrl Pts',(18.4334809164361,4.52662531785492,36.9741328403451));
#40213=CARTESIAN_POINT('Ctrl Pts',(18.4290478014908,4.52712800397608,36.9803283824271));
#40214=CARTESIAN_POINT('Ctrl Pts',(18.4269752952509,4.52736336629001,36.9832419153261));
#40215=CARTESIAN_POINT('Ctrl Pts',(18.4222482479448,4.52790102807053,36.989926474489));
#40216=CARTESIAN_POINT('Ctrl Pts',(18.419599121025,4.52820295922552,36.9937012672988));
#40217=CARTESIAN_POINT('Ctrl Pts',(18.412582147445,4.52900446264744,37.0037765323985));
#40218=CARTESIAN_POINT('Ctrl Pts',(18.4082382242734,4.52950246876849,37.0100936812771));
#40219=CARTESIAN_POINT('Ctrl Pts',(18.3769791101784,4.53310085410958,37.0561377576694));
#40220=CARTESIAN_POINT('Ctrl Pts',(18.3515142958922,4.5361124003198,37.0968345348454));
#40221=CARTESIAN_POINT('Ctrl Pts',(18.3213839965201,4.53983806415834,37.1492392644417));
#40222=CARTESIAN_POINT('Ctrl Pts',(18.3152809186123,4.54060195138256,37.1600961269484));
#40223=CARTESIAN_POINT('Ctrl Pts',(18.3034703547882,4.54210017000668,37.1815908145188));
#40224=CARTESIAN_POINT('Ctrl Pts',(18.2977567494189,4.54283465246564,37.192224591303));
#40225=CARTESIAN_POINT('Ctrl Pts',(18.2232987221485,4.55254578243759,37.3339760846133));
#40226=CARTESIAN_POINT('Ctrl Pts',(18.1697706234556,4.56117957338409,37.4725272174811));
#40227=CARTESIAN_POINT('Ctrl Pts',(18.1171271108378,4.57406590158306,37.675571076523));
#40228=CARTESIAN_POINT('Ctrl Pts',(18.1045166643854,4.57792289396945,37.7360055646947));
#40229=CARTESIAN_POINT('Ctrl Pts',(18.0927790913086,4.58270641230505,37.8097924337942));
#40230=CARTESIAN_POINT('Ctrl Pts',(18.0908642036136,4.58354381987234,37.8226689278753));
#40231=CARTESIAN_POINT('Ctrl Pts',(18.0880691824803,4.58486190149556,37.8428668340428));
#40232=CARTESIAN_POINT('Ctrl Pts',(18.0871004317981,4.58533979580818,37.8501757507832));
#40233=CARTESIAN_POINT('Ctrl Pts',(18.0854560257531,4.58619002910327,37.8631529770334));
#40234=CARTESIAN_POINT('Ctrl Pts',(18.0847635831155,4.58656183773636,37.8688191013864));
#40235=CARTESIAN_POINT('Ctrl Pts',(18.083224381568,4.58742130389915,37.8818958515913));
#40236=CARTESIAN_POINT('Ctrl Pts',(18.0823954379501,4.58790951242751,37.8893084435798));
#40237=CARTESIAN_POINT('Ctrl Pts',(18.0802342125939,4.5892557559151,37.9097048808603));
#40238=CARTESIAN_POINT('Ctrl Pts',(18.0789906993057,4.59011654245713,37.9226975370993));
#40239=CARTESIAN_POINT('Ctrl Pts',(18.0731723313726,4.59464386352464,37.9907663842874));
#40240=CARTESIAN_POINT('Ctrl Pts',(18.0708343488707,4.59837915537304,38.0460028132912));
#40241=CARTESIAN_POINT('Ctrl Pts',(18.0709498218806,4.6105497491215,38.2229377848043));
#40242=CARTESIAN_POINT('Ctrl Pts',(18.0825413521376,4.61923104985422,38.3443233771193));
#40243=CARTESIAN_POINT('Ctrl Pts',(18.1175539347502,4.63247233532486,38.5266582564846));
#40244=CARTESIAN_POINT('Ctrl Pts',(18.1327481058244,4.63702310965439,38.5888882362978));
#40245=CARTESIAN_POINT('Ctrl Pts',(18.1628406294784,4.64437027935933,38.6900072829057));
#40246=CARTESIAN_POINT('Ctrl Pts',(18.1759523338027,4.64721803189036,38.7293757661469));
#40247=CARTESIAN_POINT('Ctrl Pts',(18.1928726174228,4.65049360651855,38.7751942585372));
#40248=CARTESIAN_POINT('Ctrl Pts',(18.1954603018088,4.65098481885081,38.7820800140119));
#40249=CARTESIAN_POINT('Ctrl Pts',(18.1997188412586,4.65177747286423,38.7932179858108));
#40250=CARTESIAN_POINT('Ctrl Pts',(18.2013654968813,4.65208028268403,38.7974792840132));
#40251=CARTESIAN_POINT('Ctrl Pts',(18.2043231834156,4.65261763016177,38.8050532027856));
#40252=CARTESIAN_POINT('Ctrl Pts',(18.2056282656372,4.65285251413309,38.8083680738398));
#40253=CARTESIAN_POINT('Ctrl Pts',(18.2084619366215,4.65335774364732,38.8155074330495));
#40254=CARTESIAN_POINT('Ctrl Pts',(18.2099935888636,4.65362790338111,38.819330638968));
#40255=CARTESIAN_POINT('Ctrl Pts',(18.2142811644712,4.65437618159171,38.8299344961409));
#40256=CARTESIAN_POINT('Ctrl Pts',(18.2170634865512,4.65485275228769,38.8367045007419));
#40257=CARTESIAN_POINT('Ctrl Pts',(18.2330687612004,4.65754471675089,38.8750270634534));
#40258=CARTESIAN_POINT('Ctrl Pts',(18.2470916078546,4.65971528021714,38.9062415701925));
#40259=CARTESIAN_POINT('Ctrl Pts',(18.294849317494,4.66659047889873,39.005404080609));
#40260=CARTESIAN_POINT('Ctrl Pts',(18.3317646423561,4.67116031697851,39.0717448757472));
#40261=CARTESIAN_POINT('Ctrl Pts',(18.4588856630847,4.68533373287125,39.2714952433936));
#40262=CARTESIAN_POINT('Ctrl Pts',(18.5619101512575,4.69483691691506,39.3958881181633));
#40263=CARTESIAN_POINT('Ctrl Pts',(18.694585457383,4.70637894286772,39.5205218948371));
#40264=CARTESIAN_POINT('Ctrl Pts',(18.7102319339443,4.70772955475721,39.5347431343674));
#40265=CARTESIAN_POINT('Ctrl Pts',(18.7323301588831,4.70962436014981,39.5541748073917));
#40266=CARTESIAN_POINT('Ctrl Pts',(18.7385869069945,4.71015945634237,39.5596054952692));
#40267=CARTESIAN_POINT('Ctrl Pts',(18.7494522552614,4.71108642096732,39.5689142831526));
#40268=CARTESIAN_POINT('Ctrl Pts',(18.754044429717,4.7114775050539,39.5728114436807));
#40269=CARTESIAN_POINT('Ctrl Pts',(18.7635989688621,4.71228981663906,39.5808432621517));
#40270=CARTESIAN_POINT('Ctrl Pts',(18.7685639931474,4.71271117049215,39.5849746247623));
#40271=CARTESIAN_POINT('Ctrl Pts',(18.7802574504655,4.71370180042368,39.5946056964064));
#40272=CARTESIAN_POINT('Ctrl Pts',(18.7870024393359,4.71427188478842,39.6000849937698));
#40273=CARTESIAN_POINT('Ctrl Pts',(18.8091275158877,4.71613775018829,39.6178115240582));
#40274=CARTESIAN_POINT('Ctrl Pts',(18.8246574318935,4.71744098423163,39.6298689143832));
#40275=CARTESIAN_POINT('Ctrl Pts',(18.9064990489981,4.72427808287934,39.6914288509686));
#40276=CARTESIAN_POINT('Ctrl Pts',(18.9757526096318,4.72996532305593,39.7368580035714));
#40277=CARTESIAN_POINT('Ctrl Pts',(19.1534151282146,4.744298405395,39.8377033741452));
#40278=CARTESIAN_POINT('Ctrl Pts',(19.2645636725165,4.75306117534925,39.887582050363));
#40279=CARTESIAN_POINT('Ctrl Pts',(19.4006362288088,4.76321379989973,39.9337929606624));
#40280=CARTESIAN_POINT('Ctrl Pts',(19.4217395676946,4.76477198998715,39.9405565682163));
#40281=CARTESIAN_POINT('Ctrl Pts',(19.4863777360521,4.76948675067154,39.9600515438007));
#40282=CARTESIAN_POINT('Ctrl Pts',(19.5302526670263,4.77260806761195,39.9716136827948));
#40283=CARTESIAN_POINT('Ctrl Pts',(19.5818610045382,4.77615794681975,39.9832841847271));
#40284=CARTESIAN_POINT('Ctrl Pts',(19.5892336646776,4.77666220547482,39.9849059823511));
#40285=CARTESIAN_POINT('Ctrl Pts',(19.6010915652467,4.77746842633347,39.9874415397527));
#40286=CARTESIAN_POINT('Ctrl Pts',(19.6055707784907,4.77777186968143,39.9883826666202));
#40287=CARTESIAN_POINT('Ctrl Pts',(19.6135509108052,4.7783104753695,39.9900297384878));
#40288=CARTESIAN_POINT('Ctrl Pts',(19.6170504853764,4.77854598533409,39.9907419128352));
#40289=CARTESIAN_POINT('Ctrl Pts',(19.6245364066285,4.77904828079251,39.992243684227));
#40290=CARTESIAN_POINT('Ctrl Pts',(19.6285232695767,4.77931490281072,39.9930304038639));
#40291=CARTESIAN_POINT('Ctrl Pts',(19.6394527850218,4.78004344960864,39.9951512451545));
#40292=CARTESIAN_POINT('Ctrl Pts',(19.6464004175966,4.7805039573514,39.9964598269787));
#40293=CARTESIAN_POINT('Ctrl Pts',(19.683379692014,4.78294192613025,40.0032145661169));
#40294=CARTESIAN_POINT('Ctrl Pts',(19.7135321584205,4.78488389977208,40.0079859888287));
#40295=CARTESIAN_POINT('Ctrl Pts',(19.9040046584549,4.79693521884287,40.0335092507176));
#40296=CARTESIAN_POINT('Ctrl Pts',(20.0663012845189,4.80629132519967,40.034758246382));
#40297=CARTESIAN_POINT('Ctrl Pts',(20.3155850214231,4.82147711394626,40.0052375149436));
#40298=CARTESIAN_POINT('Ctrl Pts',(20.4034554672686,4.82698233833473,39.9885826587018));
#40299=CARTESIAN_POINT('Ctrl Pts',(20.5028508970182,4.8335458410066,39.962488721553));
#40300=CARTESIAN_POINT('Ctrl Pts',(20.5158166831166,4.83440859713363,39.9589395894699));
#40301=CARTESIAN_POINT('Ctrl Pts',(20.5366228987346,4.83580414465906,39.9530098595545));
#40302=CARTESIAN_POINT('Ctrl Pts',(20.5444872513672,4.83633419921038,39.9507142688019));
#40303=CARTESIAN_POINT('Ctrl Pts',(20.5584732448124,4.837281531624,39.946534920405));
#40304=CARTESIAN_POINT('Ctrl Pts',(20.5646006122407,4.83769817376975,39.9446706276343));
#40305=CARTESIAN_POINT('Ctrl Pts',(20.5774003127164,4.83857193752337,39.9407064851533));
#40306=CARTESIAN_POINT('Ctrl Pts',(20.5840707243191,4.83902924403982,39.9386007920264));
#40307=CARTESIAN_POINT('Ctrl Pts',(20.6014880601843,4.84022853143058,39.9329981980774));
#40308=CARTESIAN_POINT('Ctrl Pts',(20.6122158399032,4.8409724020142,39.9294430947388));
#40309=CARTESIAN_POINT('Ctrl Pts',(20.6601016342244,4.84431664075935,39.9131057557495));
#40310=CARTESIAN_POINT('Ctrl Pts',(20.6968928428725,4.84695081894416,39.8992850338736));
#40311=CARTESIAN_POINT('Ctrl Pts',(20.8848668751928,4.86075879263345,39.8220418423178));
#40312=CARTESIAN_POINT('Ctrl Pts',(21.0279194483491,4.87253809144303,39.7406648473613));
#40313=CARTESIAN_POINT('Ctrl Pts',(21.2237036021823,4.88993102610018,39.5935383074111));
#40314=CARTESIAN_POINT('Ctrl Pts',(21.2853532811074,4.89561816039348,39.5408252320486));
#40315=CARTESIAN_POINT('Ctrl Pts',(21.3502080209599,4.90169210515697,39.4778853180082));
#40316=CARTESIAN_POINT('Ctrl Pts',(21.3568580220524,4.90231601697693,39.4713372911271));
#40317=CARTESIAN_POINT('Ctrl Pts',(21.3666711732614,4.90323800104945,39.4615333487666));
#40318=CARTESIAN_POINT('Ctrl Pts',(21.3698706523434,4.90353881316319,39.4583142318775));
#40319=CARTESIAN_POINT('Ctrl Pts',(21.3755593901868,4.90407398644391,39.4525500338436));
#40320=CARTESIAN_POINT('Ctrl Pts',(21.3780529864199,4.90430868284638,39.4500093323073));
#40321=CARTESIAN_POINT('Ctrl Pts',(21.3834307348243,4.90481506381943,39.4444995692016));
#40322=CARTESIAN_POINT('Ctrl Pts',(21.3863123623672,4.90508655433879,39.4415281302991));
#40323=CARTESIAN_POINT('Ctrl Pts',(21.3943285134723,4.90584229019585,39.4332087294934));
#40324=CARTESIAN_POINT('Ctrl Pts',(21.3994418735401,4.9063249370019,39.4278403393497));
#40325=CARTESIAN_POINT('Ctrl Pts',(21.4290270663364,4.90912179785404,39.3964188438827));
#40326=CARTESIAN_POINT('Ctrl Pts',(21.4528037903716,4.91138698408081,39.3697171795512));
#40327=CARTESIAN_POINT('Ctrl Pts',(21.5284992334853,4.91871768947291,39.2797975068625));
#40328=CARTESIAN_POINT('Ctrl Pts',(21.5771440251221,4.92362706595328,39.2139349292004));
#40329=CARTESIAN_POINT('Ctrl Pts',(21.7040033439792,4.93762555468609,39.0171284753932));
#40330=CARTESIAN_POINT('Ctrl Pts',(21.7710745324893,4.94666162442545,38.8797696853767));
#40331=CARTESIAN_POINT('Ctrl Pts',(21.828466368515,4.95769313693434,38.7154080938952));
#40332=CARTESIAN_POINT('Ctrl Pts',(21.8352936917446,4.95908303897571,38.694738082623));
#40333=CARTESIAN_POINT('Ctrl Pts',(21.844264745739,4.96102420973584,38.6659509144996));
#40334=CARTESIAN_POINT('Ctrl Pts',(21.8467076340912,4.96156577810975,38.6579281320697));
#40335=CARTESIAN_POINT('Ctrl Pts',(21.8508224571725,4.9625009188033,38.6440913381381));
#40336=CARTESIAN_POINT('Ctrl Pts',(21.8525195125849,4.96289367370031,38.6382848746909));
#40337=CARTESIAN_POINT('Ctrl Pts',(21.8559676899572,4.96370659672256,38.6262775008843));
#40338=CARTESIAN_POINT('Ctrl Pts',(21.8577151093522,4.96412687859823,38.6200756146));
#40339=CARTESIAN_POINT('Ctrl Pts',(21.8617203017572,4.96511000673922,38.6055827451913));
#40340=CARTESIAN_POINT('Ctrl Pts',(21.8639537999014,4.96567362573729,38.5972852521614));
#40341=CARTESIAN_POINT('Ctrl Pts',(21.8709776734886,4.96749706573402,38.5704791350283));
#40342=CARTESIAN_POINT('Ctrl Pts',(21.8755482414878,4.96876387709983,38.5519146164357));
#40343=CARTESIAN_POINT('Ctrl Pts',(21.8974678164881,4.97527571878104,38.4568149401438));
#40344=CARTESIAN_POINT('Ctrl Pts',(21.9104088242946,4.98065817330465,38.3793498136241));
#40345=CARTESIAN_POINT('Ctrl Pts',(21.9273014311957,4.99198917349072,38.2183621204622));
#40346=CARTESIAN_POINT('Ctrl Pts',(21.9306161324608,4.99794073320218,38.1349311393365));
#40347=CARTESIAN_POINT('Ctrl Pts',(21.9257731676811,5.0116994142719,37.942147511928));
#40348=CARTESIAN_POINT('Ctrl Pts',(21.9137194480088,5.01948543557693,37.8331603430171));
#40349=CARTESIAN_POINT('Ctrl Pts',(21.8907061079507,5.02745623692624,37.7167807508679));
#40350=CARTESIAN_POINT('Ctrl Pts',(21.8888638321568,5.02806892141685,37.7078010565084));
#40351=CARTESIAN_POINT('Ctrl Pts',(21.8860206207703,5.0289775767237,37.6944274716329));
#40352=CARTESIAN_POINT('Ctrl Pts',(21.8850682164858,5.02927617554833,37.6900235641458));
#40353=CARTESIAN_POINT('Ctrl Pts',(21.8833362569335,5.02980895967447,37.6821486447314));
#40354=CARTESIAN_POINT('Ctrl Pts',(21.882562524802,5.03004346791209,37.678676427575));
#40355=CARTESIAN_POINT('Ctrl Pts',(21.8808624579974,5.03055121418796,37.6711453597908));
#40356=CARTESIAN_POINT('Ctrl Pts',(21.8799325904454,5.03082424870648,37.6670873707968));
#40357=CARTESIAN_POINT('Ctrl Pts',(21.8772853829871,5.03158866436852,37.655704204242));
#40358=CARTESIAN_POINT('Ctrl Pts',(21.8755382930089,5.03207838698002,37.6483859177401));
#40359=CARTESIAN_POINT('Ctrl Pts',(21.8647948725178,5.03500438017196,37.6045212473273));
#40360=CARTESIAN_POINT('Ctrl Pts',(21.8547727083196,5.03738618161752,37.5682314730051));
#40361=CARTESIAN_POINT('Ctrl Pts',(21.7951628779253,5.04999507732401,37.374654458616));
#40362=CARTESIAN_POINT('Ctrl Pts',(21.7266213534196,5.05952158743345,37.2239147701008));
#40363=CARTESIAN_POINT('Ctrl Pts',(21.5982546892794,5.07433635976592,37.0167994864123));
#40364=CARTESIAN_POINT('Ctrl Pts',(21.5527245537006,5.07921281669275,36.9524872164008));
#40365=CARTESIAN_POINT('Ctrl Pts',(21.4951674091427,5.08508180599626,36.8809062997951));
#40366=CARTESIAN_POINT('Ctrl Pts',(21.4868337240754,5.08592494610814,36.8707561289538));
#40367=CARTESIAN_POINT('Ctrl Pts',(21.4731367890637,5.08730052057886,36.8544167595934));
#40368=CARTESIAN_POINT('Ctrl Pts',(21.4678365295584,5.08783041346588,36.8481751212059));
#40369=CARTESIAN_POINT('Ctrl Pts',(21.4583320402329,5.08877647267157,36.8371258957064));
#40370=CARTESIAN_POINT('Ctrl Pts',(21.4541433467099,5.08919199912621,36.8323050570223));
#40371=CARTESIAN_POINT('Ctrl Pts',(21.4452690711753,5.09006944711691,36.8221933573419));
#40372=CARTESIAN_POINT('Ctrl Pts',(21.4405782068667,5.09053158376879,36.8169072785704));
#40373=CARTESIAN_POINT('Ctrl Pts',(21.4280920831633,5.0917573746796,36.8029915983102));
#40374=CARTESIAN_POINT('Ctrl Pts',(21.4202477535029,5.09252307455564,36.7944066097323));
#40375=CARTESIAN_POINT('Ctrl Pts',(21.3832112425436,5.0961184610611,36.7546018966228));
#40376=CARTESIAN_POINT('Ctrl Pts',(21.3530663110709,5.09898851586971,36.724289105002));
#40377=CARTESIAN_POINT('Ctrl Pts',(21.2005296125092,5.11325680516196,36.5807693799915));
#40378=CARTESIAN_POINT('Ctrl Pts',(21.0648346954229,5.12526898369485,36.4827671092162));
#40379=CARTESIAN_POINT('Ctrl Pts',(20.8529616273825,5.14234243127466,36.3680893506393));
#40380=CARTESIAN_POINT('Ctrl Pts',(20.7856535134988,5.14753740641177,36.3365348787401));
#40381=CARTESIAN_POINT('Ctrl Pts',(20.7080770219719,5.15315252945747,36.305492973338));
#40382=CARTESIAN_POINT('Ctrl Pts',(20.6994431352856,5.15377239852827,36.3021101683576));
#40383=CARTESIAN_POINT('Ctrl Pts',(20.6865583914808,5.15468958591064,36.2971687201692));
#40384=CARTESIAN_POINT('Ctrl Pts',(20.6823260534746,5.15498960356391,36.295562634438));
#40385=CARTESIAN_POINT('Ctrl Pts',(20.6747561814766,5.15552391680469,36.2927204646941));
#40386=CARTESIAN_POINT('Ctrl Pts',(20.6714208535493,5.15575854321636,36.2914787086399));
#40387=CARTESIAN_POINT('Ctrl Pts',(20.6641910518689,5.15626540310884,36.2888097818465));
#40388=CARTESIAN_POINT('Ctrl Pts',(20.6602954151002,5.15653743918178,36.2873859414326));
#40389=CARTESIAN_POINT('Ctrl Pts',(20.6493873156038,5.15729623848541,36.2834389051495));
#40390=CARTESIAN_POINT('Ctrl Pts',(20.6423646856287,5.15778138212288,36.2809437303762));
#40391=CARTESIAN_POINT('Ctrl Pts',(20.600960135752,5.16062291662159,36.2665021714051));
#40392=CARTESIAN_POINT('Ctrl Pts',(20.5662575413089,5.16292843149796,36.2554891749415));
#40393=CARTESIAN_POINT('Ctrl Pts',(20.4500868132194,5.1704603187242,36.2222102143629));
#40394=CARTESIAN_POINT('Ctrl Pts',(20.3674658963873,5.17552060783291,36.2043091438547));
#40395=CARTESIAN_POINT('Ctrl Pts',(20.1368642148808,5.18945313932156,36.1699952007557));
#40396=CARTESIAN_POINT('Ctrl Pts',(19.9877791211154,5.19828839344691,36.1651887155832));
#40397=CARTESIAN_POINT('Ctrl Pts',(19.8177404989281,5.20909825597186,36.1793734285027));
#40398=CARTESIAN_POINT('Ctrl Pts',(19.7958865349046,5.21050048275683,36.1815728880997));
#40399=CARTESIAN_POINT('Ctrl Pts',(19.765716316612,5.2124561273091,36.1851306672613));
#40400=CARTESIAN_POINT('Ctrl Pts',(19.7573637124702,5.2129996512369,36.186171106377));
#40401=CARTESIAN_POINT('Ctrl Pts',(19.7430123168325,5.21393726686614,36.1880542422949));
#40402=CARTESIAN_POINT('Ctrl Pts',(19.7370101447233,5.21433053107951,36.1888705997918));
#40403=CARTESIAN_POINT('Ctrl Pts',(19.7246359191213,5.21514366437997,36.1906130198412));
#40404=CARTESIAN_POINT('Ctrl Pts',(19.7182644655896,5.2155636434842,36.1915427424207));
#40405=CARTESIAN_POINT('Ctrl Pts',(19.7034292212697,5.21654460516421,36.1937834110971));
#40406=CARTESIAN_POINT('Ctrl Pts',(19.6949693217924,5.217106350211,36.1951188509591));
#40407=CARTESIAN_POINT('Ctrl Pts',(19.6678076492659,5.2189176150415,36.1995920442451));
#40408=CARTESIAN_POINT('Ctrl Pts',(19.6491436320554,5.22017399527336,36.202949151489));
#40409=CARTESIAN_POINT('Ctrl Pts',(19.5546885209125,5.22659426539678,36.2213803976675));
#40410=CARTESIAN_POINT('Ctrl Pts',(19.47981183807,5.23189126104924,36.2407217802112));
#40411=CARTESIAN_POINT('Ctrl Pts',(19.4022328836949,5.23759496523851,36.2658148015992));
#40412=CARTESIAN_POINT('Ctrl Pts',(19.3981661044488,5.23789458476241,36.2671451706303));
#40413=CARTESIAN_POINT('Ctrl Pts',(19.3941040060237,5.23819447890751,36.2684889840944));
#40414=CARTESIAN_POINT('Origin',(20.,-1.3495818343519,38.1));
#40415=CARTESIAN_POINT('',(19.3941044301425,6.20523851046618,36.2684888437885));
#40416=CARTESIAN_POINT('',(19.3941040087491,6.0347666134114,36.2684889831928));
#40417=CARTESIAN_POINT('',(19.3941040087494,-1.3495818343519,36.2684889831927));
#40418=CARTESIAN_POINT('Ctrl Pts',(19.3941044301425,6.20523851046618,36.2684888437885));
#40419=CARTESIAN_POINT('Ctrl Pts',(19.4822432513283,6.19878335600331,36.2393309972159));
#40420=CARTESIAN_POINT('Ctrl Pts',(19.5724357244974,6.19216553628329,36.2165523121689));
#40421=CARTESIAN_POINT('Ctrl Pts',(19.7436130437267,6.17976140007284,36.1862740556517));
#40422=CARTESIAN_POINT('Ctrl Pts',(19.8240511750841,6.17399724520281,36.1772090783427));
#40423=CARTESIAN_POINT('Ctrl Pts',(19.9402921846074,6.16593451612745,36.1714672648057));
#40424=CARTESIAN_POINT('Ctrl Pts',(19.9758036483548,6.16350762489711,36.1706948235368));
#40425=CARTESIAN_POINT('Ctrl Pts',(20.0187183346558,6.16063396175617,36.1709466218819));
#40426=CARTESIAN_POINT('Ctrl Pts',(20.026117691962,6.16014061356754,36.1710326124547));
#40427=CARTESIAN_POINT('Ctrl Pts',(20.037652006817,6.15937507726548,36.1712330387734));
#40428=CARTESIAN_POINT('Ctrl Pts',(20.0417873028063,6.15910131937754,36.1713181997907));
#40429=CARTESIAN_POINT('Ctrl Pts',(20.0494816682068,6.15859329796945,36.1715014136885));
#40430=CARTESIAN_POINT('Ctrl Pts',(20.0530407063175,6.1583588534782,36.1715960182871));
#40431=CARTESIAN_POINT('Ctrl Pts',(20.0611405370733,6.15782650745258,36.171833764969));
#40432=CARTESIAN_POINT('Ctrl Pts',(20.0656810919062,6.15752895205417,36.1719830938511));
#40433=CARTESIAN_POINT('Ctrl Pts',(20.0795693041563,6.15662134580215,36.1724889658003));
#40434=CARTESIAN_POINT('Ctrl Pts',(20.0889151022645,6.15601409356413,36.172897466594));
#40435=CARTESIAN_POINT('Ctrl Pts',(20.181816670481,6.15000929031957,36.1776354396856));
#40436=CARTESIAN_POINT('Ctrl Pts',(20.2650216845902,6.14488360631636,36.1873290673491));
#40437=CARTESIAN_POINT('Ctrl Pts',(20.4534639566784,6.13333374171192,36.2218222269987));
#40438=CARTESIAN_POINT('Ctrl Pts',(20.5577667113382,6.12697587877511,36.250114066817));
#40439=CARTESIAN_POINT('Ctrl Pts',(20.7337013499291,6.11563504166003,36.3140783753764));
#40440=CARTESIAN_POINT('Ctrl Pts',(20.8064940554379,6.11074745710291,36.3457483472262));
#40441=CARTESIAN_POINT('Ctrl Pts',(20.8942502506202,6.10448479787618,36.3905472483516));
#40442=CARTESIAN_POINT('Ctrl Pts',(20.9112424539752,6.10325435372867,36.3995443644372));
#40443=CARTESIAN_POINT('Ctrl Pts',(20.9356471144982,6.101459859361,36.4129371060808));
#40444=CARTESIAN_POINT('Ctrl Pts',(20.9431694241123,6.10090292641884,36.4171309723042));
#40445=CARTESIAN_POINT('Ctrl Pts',(20.9562727041929,6.09992598348296,36.4245518123248));
#40446=CARTESIAN_POINT('Ctrl Pts',(20.9618660919218,6.09950676658568,36.4277566762275));
#40447=CARTESIAN_POINT('Ctrl Pts',(20.97267224793,6.0986925544318,36.4340204730334));
#40448=CARTESIAN_POINT('Ctrl Pts',(20.9778869171874,6.09829768551515,36.4370759903217));
#40449=CARTESIAN_POINT('Ctrl Pts',(20.99028491116,6.09735414688972,36.4444190342199));
#40450=CARTESIAN_POINT('Ctrl Pts',(20.9974548262675,6.09680467576843,36.4487288516537));
#40451=CARTESIAN_POINT('Ctrl Pts',(21.0230673571342,6.09482796197246,36.4643521581027));
#40452=CARTESIAN_POINT('Ctrl Pts',(21.041346803438,6.09339118124781,36.4759287421795));
#40453=CARTESIAN_POINT('Ctrl Pts',(21.1885466558558,6.08160266163336,36.5726589671292));
#40454=CARTESIAN_POINT('Ctrl Pts',(21.3069812570654,6.07066621435029,36.67269649903));
#40455=CARTESIAN_POINT('Ctrl Pts',(21.4668816674368,6.05391841409738,36.8445145378579));
#40456=CARTESIAN_POINT('Ctrl Pts',(21.5178484619017,6.0481979847951,36.9066336428185));
#40457=CARTESIAN_POINT('Ctrl Pts',(21.5854794326913,6.0401878291225,37.0004328849294));
#40458=CARTESIAN_POINT('Ctrl Pts',(21.6053687260439,6.0377714610864,37.029680181294));
#40459=CARTESIAN_POINT('Ctrl Pts',(21.6284304905822,6.03490853968064,37.0656831655258));
#40460=CARTESIAN_POINT('Ctrl Pts',(21.6323810986507,6.03441580686973,37.0719294139738));
#40461=CARTESIAN_POINT('Ctrl Pts',(21.6384855103003,6.03365101500111,37.0817049148649));
#40462=CARTESIAN_POINT('Ctrl Pts',(21.6406639780363,6.03337739100775,37.0852185654806));
#40463=CARTESIAN_POINT('Ctrl Pts',(21.6446976326068,6.03286948860585,37.0917713890723));
#40464=CARTESIAN_POINT('Ctrl Pts',(21.6465556829605,6.03263503002397,37.0948086660625));
#40465=CARTESIAN_POINT('Ctrl Pts',(21.6507668083596,6.03210248605153,37.1017354231787));
#40466=CARTESIAN_POINT('Ctrl Pts',(21.6531145481167,6.0318047478323,37.1056280812657));
#40467=CARTESIAN_POINT('Ctrl Pts',(21.6602587098763,6.03089602857227,37.1175686557316));
#40468=CARTESIAN_POINT('Ctrl Pts',(21.6650103716209,6.03028785615089,37.1256433913094));
#40469=CARTESIAN_POINT('Ctrl Pts',(21.7127721725587,6.02413249154624,37.2081771506125));
#40470=CARTESIAN_POINT('Ctrl Pts',(21.7508231573516,6.01887262410412,37.285408789996));
#40471=CARTESIAN_POINT('Ctrl Pts',(21.82036617698,6.00787961922313,37.4541505431114));
#40472=CARTESIAN_POINT('Ctrl Pts',(21.8503895024448,6.00217898479395,37.54600222832));
#40473=CARTESIAN_POINT('Ctrl Pts',(21.8941623185904,5.99110590989602,37.7241628826058));
#40474=CARTESIAN_POINT('Ctrl Pts',(21.9091746180942,5.98577008352513,37.8099069539371));
#40475=CARTESIAN_POINT('Ctrl Pts',(21.9204822979266,5.97896805468455,37.9164311892186));
#40476=CARTESIAN_POINT('Ctrl Pts',(21.9222973441895,5.97767752511486,37.9365294014957));
#40477=CARTESIAN_POINT('Ctrl Pts',(21.9244492596902,5.97581132781192,37.9654090669302));
#40478=CARTESIAN_POINT('Ctrl Pts',(21.9250419790922,5.97524360956797,37.9741705641129));
#40479=CARTESIAN_POINT('Ctrl Pts',(21.9259677356479,5.97425408224029,37.9893982066896));
#40480=CARTESIAN_POINT('Ctrl Pts',(21.9263280809159,5.97383312849229,37.9958625983837));
#40481=CARTESIAN_POINT('Ctrl Pts',(21.9269596492374,5.97302011059117,38.0083208515063));
#40482=CARTESIAN_POINT('Ctrl Pts',(21.9272354643227,5.97262819426452,38.0143144134008));
#40483=CARTESIAN_POINT('Ctrl Pts',(21.9278218463977,5.97169889575878,38.0284972345285));
#40484=CARTESIAN_POINT('Ctrl Pts',(21.9281081968538,5.97116076728817,38.0366873263278));
#40485=CARTESIAN_POINT('Ctrl Pts',(21.9289312386083,5.96926353659834,38.065480400967));
#40486=CARTESIAN_POINT('Ctrl Pts',(21.9291899241039,5.96789586467031,38.0860893198323));
#40487=CARTESIAN_POINT('Ctrl Pts',(21.9285399900468,5.95538031402947,38.2732858805206));
#40488=CARTESIAN_POINT('Ctrl Pts',(21.9063854731736,5.94353862930264,38.4390663180682));
#40489=CARTESIAN_POINT('Ctrl Pts',(21.8472899255557,5.92727732416627,38.659328776421));
#40490=CARTESIAN_POINT('Ctrl Pts',(21.828509872196,5.92290516627813,38.7179653710899));
#40491=CARTESIAN_POINT('Ctrl Pts',(21.7919583368256,5.9156333187595,38.8157250558177));
#40492=CARTESIAN_POINT('Ctrl Pts',(21.7756251084725,5.91269230318268,38.8553364594794));
#40493=CARTESIAN_POINT('Ctrl Pts',(21.7547764147761,5.9092992987042,38.901475521571));
#40494=CARTESIAN_POINT('Ctrl Pts',(21.7515246310143,5.90877945588525,38.9085572024044));
#40495=CARTESIAN_POINT('Ctrl Pts',(21.7464453256649,5.90798192555351,38.9194443842238));
#40496=CARTESIAN_POINT('Ctrl Pts',(21.7446481211574,5.90770245392579,38.9232638146796));
#40497=CARTESIAN_POINT('Ctrl Pts',(21.7413151072408,5.90718917043526,38.9302872260679));
#40498=CARTESIAN_POINT('Ctrl Pts',(21.7397829924394,5.90695514400767,38.9334928434621));
#40499=CARTESIAN_POINT('Ctrl Pts',(21.7363197172861,5.90643041405077,38.9406878372925));
#40500=CARTESIAN_POINT('Ctrl Pts',(21.7343836647681,5.90614001595643,38.94467479231));
#40501=CARTESIAN_POINT('Ctrl Pts',(21.7293949568701,5.90539911004154,38.954858678108));
#40502=CARTESIAN_POINT('Ctrl Pts',(21.7263226936957,5.90494978061176,38.9610460133503));
#40503=CARTESIAN_POINT('Ctrl Pts',(21.7080375700732,5.90231522966862,38.9973797637081));
#40504=CARTESIAN_POINT('Ctrl Pts',(21.6920674722899,5.90017363840033,39.0271411891221));
#40505=CARTESIAN_POINT('Ctrl Pts',(21.6049326071823,5.88919733066095,39.1797638940138));
#40506=CARTESIAN_POINT('Ctrl Pts',(21.5211403435531,5.88090984170965,39.2949222132794));
#40507=CARTESIAN_POINT('Ctrl Pts',(21.3546431338181,5.86604598799769,39.4775088090038));
#40508=CARTESIAN_POINT('Ctrl Pts',(21.2776090012152,5.85961472128681,39.5492409018788));
#40509=CARTESIAN_POINT('Ctrl Pts',(21.1836064877648,5.85196384181909,39.6234282148855));
#40510=CARTESIAN_POINT('Ctrl Pts',(21.1719856048784,5.85102143023252,39.6323862328502));
#40511=CARTESIAN_POINT('Ctrl Pts',(21.1540912960282,5.84957484812811,39.6458575395051));
#40512=CARTESIAN_POINT('Ctrl Pts',(21.1478908854923,5.84907443102439,39.6504672728417));
#40513=CARTESIAN_POINT('Ctrl Pts',(21.1365476259435,5.84816035969162,39.6587951509015));
#40514=CARTESIAN_POINT('Ctrl Pts',(21.1314137791914,5.84774718020282,39.6625254196853));
#40515=CARTESIAN_POINT('Ctrl Pts',(21.1202734470035,5.84685165847174,39.6705363293988));
#40516=CARTESIAN_POINT('Ctrl Pts',(21.1142606478879,5.84636898139062,39.6748079768821));
#40517=CARTESIAN_POINT('Ctrl Pts',(21.0978374765458,5.84505232226313,39.686334276449));
#40518=CARTESIAN_POINT('Ctrl Pts',(21.0873799348007,5.84421578333222,39.6935207641981));
#40519=CARTESIAN_POINT('Ctrl Pts',(21.0350226044427,5.84003595650712,39.728745679715));
#40520=CARTESIAN_POINT('Ctrl Pts',(20.9921092579191,5.83663591963841,39.7552349398685));
#40521=CARTESIAN_POINT('Ctrl Pts',(20.9257899008653,5.83141517878617,39.7926660815341));
#40522=CARTESIAN_POINT('Ctrl Pts',(20.9031185176103,5.829636314123,39.80487015761));
#40523=CARTESIAN_POINT('Ctrl Pts',(20.7681266099557,5.81908203876234,39.8740884677347));
#40524=CARTESIAN_POINT('Ctrl Pts',(20.6506893908832,5.8100236668565,39.9204413149286));
#40525=CARTESIAN_POINT('Ctrl Pts',(20.4765536923185,5.7971696661141,39.9701553630643));
#40526=CARTESIAN_POINT('Ctrl Pts',(20.4228898522023,5.79328772155628,39.9830160803579));
#40527=CARTESIAN_POINT('Ctrl Pts',(20.3411913455789,5.78756007788422,39.9989257549943));
#40528=CARTESIAN_POINT('Ctrl Pts',(20.3135219233485,5.78565141581237,40.0036897765092));
#40529=CARTESIAN_POINT('Ctrl Pts',(20.2789485652591,5.78331309348411,40.0088681580263));
#40530=CARTESIAN_POINT('Ctrl Pts',(20.2721349393605,5.78285450632853,40.009851440584));
#40531=CARTESIAN_POINT('Ctrl Pts',(20.2613316498728,5.78213110273757,40.0113514871298));
#40532=CARTESIAN_POINT('Ctrl Pts',(20.2573454636272,5.78186498003601,40.01189226989));
#40533=CARTESIAN_POINT('Ctrl Pts',(20.2498086164001,5.78136335539612,40.0128907517678));
#40534=CARTESIAN_POINT('Ctrl Pts',(20.2462584160669,5.78112771890116,40.0133510304608));
#40535=CARTESIAN_POINT('Ctrl Pts',(20.2380978357383,5.78058754836809,40.0143859491658));
#40536=CARTESIAN_POINT('Ctrl Pts',(20.2334866464242,5.78028339492254,40.0149538189731));
#40537=CARTESIAN_POINT('Ctrl Pts',(20.221144423303,5.77947206595061,40.016428524816));
#40538=CARTESIAN_POINT('Ctrl Pts',(20.2134097790597,5.77896651795911,40.017305248996));
#40539=CARTESIAN_POINT('Ctrl Pts',(20.1549888239815,5.77516845213332,40.0235693701652));
#40540=CARTESIAN_POINT('Ctrl Pts',(20.1041071307877,5.7719762708601,40.0269933563339));
#40541=CARTESIAN_POINT('Ctrl Pts',(20.0287861529177,5.76734349246639,40.0290691299038));
#40542=CARTESIAN_POINT('Ctrl Pts',(20.0044162800825,5.76585889800198,40.0292788586491));
#40543=CARTESIAN_POINT('Ctrl Pts',(19.8132179178463,5.75428047380752,40.0273013180944));
#40544=CARTESIAN_POINT('Ctrl Pts',(19.6473241436326,5.74457853297607,40.0039428669454));
#40545=CARTESIAN_POINT('Ctrl Pts',(19.4454861020688,5.73154157048244,39.9482065493981));
#40546=CARTESIAN_POINT('Ctrl Pts',(19.4048592104452,5.7288561049549,39.9355272067644));
#40547=CARTESIAN_POINT('Ctrl Pts',(19.3537229976297,5.7253820757576,39.9176917848358));
#40548=CARTESIAN_POINT('Ctrl Pts',(19.3427939927123,5.72463406497428,39.9137689055848));
#40549=CARTESIAN_POINT('Ctrl Pts',(19.3252748708879,5.72342579793691,39.9073014275896));
#40550=CARTESIAN_POINT('Ctrl Pts',(19.3186620421644,5.7229675953757,39.9048188371798));
#40551=CARTESIAN_POINT('Ctrl Pts',(19.3060957229741,5.72209275132529,39.900022280003));
#40552=CARTESIAN_POINT('Ctrl Pts',(19.3001397870552,5.72167633523702,39.8977149481714));
#40553=CARTESIAN_POINT('Ctrl Pts',(19.2865680407102,5.72072333692431,39.8923795818158));
#40554=CARTESIAN_POINT('Ctrl Pts',(19.2789598892179,5.72018612509789,39.8893325238756));
#40555=CARTESIAN_POINT('Ctrl Pts',(19.2591892385596,5.71878223835577,39.8812678275729));
#40556=CARTESIAN_POINT('Ctrl Pts',(19.2470584126493,5.71791302719372,39.8761741494971));
#40557=CARTESIAN_POINT('Ctrl Pts',(19.1619696801723,5.71175980833699,39.839417463353));
#40558=CARTESIAN_POINT('Ctrl Pts',(19.0909886049048,5.70632837801804,39.8033975502764));
#40559=CARTESIAN_POINT('Ctrl Pts',(18.9192101207218,5.69242054684472,39.7024275326795));
#40560=CARTESIAN_POINT('Ctrl Pts',(18.821858723836,5.68381081135653,39.6322728083569));
#40561=CARTESIAN_POINT('Ctrl Pts',(18.6902151316299,5.6714103984125,39.5174025295035));
#40562=CARTESIAN_POINT('Ctrl Pts',(18.6503438718174,5.66754044564485,39.4794910454738));
#40563=CARTESIAN_POINT('Ctrl Pts',(18.5926847037875,5.66182821534024,39.4197693562484));
#40564=CARTESIAN_POINT('Ctrl Pts',(18.5736650592451,5.65992333859906,39.3991906467642));
#40565=CARTESIAN_POINT('Ctrl Pts',(18.5505409397331,5.65758897922564,39.3730507922824));
#40566=CARTESIAN_POINT('Ctrl Pts',(18.546010099586,5.6571306841945,39.3678735189847));
#40567=CARTESIAN_POINT('Ctrl Pts',(18.5388746590869,5.65640763530124,39.3596314814215));
#40568=CARTESIAN_POINT('Ctrl Pts',(18.5362518332966,5.65614157730287,39.3565826817423));
#40569=CARTESIAN_POINT('Ctrl Pts',(18.5313121681438,5.65564000302225,39.3508043121125));
#40570=CARTESIAN_POINT('Ctrl Pts',(18.5289934211186,5.65540435258617,39.3480765280027));
#40571=CARTESIAN_POINT('Ctrl Pts',(18.5236819557448,5.65486405794854,39.3417927321904));
#40572=CARTESIAN_POINT('Ctrl Pts',(18.5206944845256,5.65455979494514,39.3382323491632));
#40573=CARTESIAN_POINT('Ctrl Pts',(18.5127343523278,5.6537479804716,39.328675762971));
#40574=CARTESIAN_POINT('Ctrl Pts',(18.5077850307439,5.65324205959919,39.3226601031099));
#40575=CARTESIAN_POINT('Ctrl Pts',(18.4706293960813,5.64943368896291,39.276937539467));
#40576=CARTESIAN_POINT('Ctrl Pts',(18.4399733439583,5.64623218931489,39.235990444263));
#40577=CARTESIAN_POINT('Ctrl Pts',(18.3341684526893,5.63476097894051,39.0822917690576));
#40578=CARTESIAN_POINT('Ctrl Pts',(18.2693209693156,5.62684882176493,38.9629290559913));
#40579=CARTESIAN_POINT('Ctrl Pts',(18.1937665496239,5.61491080162595,38.780381034055));
#40580=CARTESIAN_POINT('Ctrl Pts',(18.1728071869465,5.61111319388683,38.7219028036021));
#40581=CARTESIAN_POINT('Ctrl Pts',(18.1439119645423,5.60491643761425,38.627114534684));
#40582=CARTESIAN_POINT('Ctrl Pts',(18.1341410058778,5.60257352010517,38.5914086447976));
#40583=CARTESIAN_POINT('Ctrl Pts',(18.122790506048,5.59948706945885,38.5446904249656));
#40584=CARTESIAN_POINT('Ctrl Pts',(18.12027012231,5.59877365446295,38.5339131674132));
#40585=CARTESIAN_POINT('Ctrl Pts',(18.1163197655994,5.59760787276709,38.5163406565997));
#40586=CARTESIAN_POINT('Ctrl Pts',(18.1148334735088,5.59715730340966,38.5095582170079));
#40587=CARTESIAN_POINT('Ctrl Pts',(18.1120433268395,5.59628783481803,38.4964888169572));
#40588=CARTESIAN_POINT('Ctrl Pts',(18.1107341787303,5.5958691100482,38.4902030710009));
#40589=CARTESIAN_POINT('Ctrl Pts',(18.1078044650007,5.59490672312035,38.4757758942859));
#40590=CARTESIAN_POINT('Ctrl Pts',(18.1062050302295,5.59436239979195,38.4676303499996));
#40591=CARTESIAN_POINT('Ctrl Pts',(18.1020844522911,5.59290789353568,38.4459044806841));
#40592=CARTESIAN_POINT('Ctrl Pts',(18.0996565416603,5.59199479235371,38.4323071764955));
#40593=CARTESIAN_POINT('Ctrl Pts',(18.0796387155648,5.58394337882969,38.3127961029939));
#40594=CARTESIAN_POINT('Ctrl Pts',(18.070776073483,5.57652955287812,38.205629665528));
#40595=CARTESIAN_POINT('Ctrl Pts',(18.070936804357,5.56365420413341,38.0234158365994));
#40596=CARTESIAN_POINT('Ctrl Pts',(18.0753628644005,5.55829502373828,37.9486024083819));
#40597=CARTESIAN_POINT('Ctrl Pts',(18.0951992911711,5.54622044985506,37.780265021749));
#40598=CARTESIAN_POINT('Ctrl Pts',(18.1131734656301,5.53953413727261,37.6872212455289));
#40599=CARTESIAN_POINT('Ctrl Pts',(18.1403561849151,5.53254281768199,37.5868185160983));
#40600=CARTESIAN_POINT('Ctrl Pts',(18.1428707668839,5.53191635532452,37.5777918282836));
#40601=CARTESIAN_POINT('Ctrl Pts',(18.1467029012921,5.53099134614687,37.5644133243045));
#40602=CARTESIAN_POINT('Ctrl Pts',(18.1479701815966,5.53069003376427,37.5600474316597));
#40603=CARTESIAN_POINT('Ctrl Pts',(18.1502575293761,5.53015431696555,37.5522701150643));
#40604=CARTESIAN_POINT('Ctrl Pts',(18.1512716169498,5.5299195745406,37.5488570050266));
#40605=CARTESIAN_POINT('Ctrl Pts',(18.1534835300465,5.52941348695002,37.5414871777931));
#40606=CARTESIAN_POINT('Ctrl Pts',(18.1546846230418,5.52914233375021,37.5375315060078));
#40607=CARTESIAN_POINT('Ctrl Pts',(18.1580681568925,5.52838849234725,37.5265156934679));
#40608=CARTESIAN_POINT('Ctrl Pts',(18.1602784912671,5.52790738970793,37.5194640931869));
#40609=CARTESIAN_POINT('Ctrl Pts',(18.1732950888228,5.52513770503684,37.4787584376956));
#40610=CARTESIAN_POINT('Ctrl Pts',(18.184984928231,5.52289704418227,37.4453912751023));
#40611=CARTESIAN_POINT('Ctrl Pts',(18.2261779439051,5.51568656916191,37.3374175431053));
#40612=CARTESIAN_POINT('Ctrl Pts',(18.2594188211567,5.51086710659127,37.2643230285115));
#40613=CARTESIAN_POINT('Ctrl Pts',(18.3697477118434,5.49682607433729,37.0570661953431));
#40614=CARTESIAN_POINT('Ctrl Pts',(18.4585019598398,5.48766852923149,36.9298671068564));
#40615=CARTESIAN_POINT('Ctrl Pts',(18.5758871927758,5.47650353778058,36.7984958442563));
#40616=CARTESIAN_POINT('Ctrl Pts',(18.5905680500564,5.47512237199681,36.7826117224649));
#40617=CARTESIAN_POINT('Ctrl Pts',(18.6112921514894,5.47319148273305,36.7609320290025));
#40618=CARTESIAN_POINT('Ctrl Pts',(18.6171110815387,5.47265132370543,36.7549235133055));
#40619=CARTESIAN_POINT('Ctrl Pts',(18.6272014253716,5.47171796469598,36.7446391049315));
#40620=CARTESIAN_POINT('Ctrl Pts',(18.6314542309351,5.47132557490013,36.7403450588554));
#40621=CARTESIAN_POINT('Ctrl Pts',(18.6402850262368,5.47051279412684,36.7315120362935));
#40622=CARTESIAN_POINT('Ctrl Pts',(18.6448657255471,5.47009228668394,36.7269758876113));
#40623=CARTESIAN_POINT('Ctrl Pts',(18.6556197289896,5.46910756455982,36.7164327131544));
#40624=CARTESIAN_POINT('Ctrl Pts',(18.6618106603213,5.46854256960355,36.7104439423232));
#40625=CARTESIAN_POINT('Ctrl Pts',(18.6819542025523,5.46671016060605,36.6912176400474));
#40626=CARTESIAN_POINT('Ctrl Pts',(18.6960643609658,5.46543565969649,36.6781475935093));
#40627=CARTESIAN_POINT('Ctrl Pts',(18.7693934869399,5.45885587924319,36.6122334220224));
#40628=CARTESIAN_POINT('Ctrl Pts',(18.8316300572949,5.4534099229347,36.562875885249));
#40629=CARTESIAN_POINT('Ctrl Pts',(18.9853373531442,5.44028725917251,36.4557154231495));
#40630=CARTESIAN_POINT('Ctrl Pts',(19.0789820055309,5.4325315878804,36.4014902797712));
#40631=CARTESIAN_POINT('Ctrl Pts',(19.2473134335991,5.4193034660997,36.3220493428573));
#40632=CARTESIAN_POINT('Ctrl Pts',(19.3199273763348,5.4138095667175,36.2930279150429));
#40633=CARTESIAN_POINT('Ctrl Pts',(19.3941040111825,5.40852741588127,36.2684889823878));
#40634=CARTESIAN_POINT('',(18.0708696352982,5.3988988782065,38.1006192288316));
#40635=CARTESIAN_POINT('Ctrl Pts',(19.3941040060237,5.23819447890751,36.2684889840944));
#40636=CARTESIAN_POINT('Ctrl Pts',(19.3180587870711,5.24380869932756,36.2936460774039));
#40637=CARTESIAN_POINT('Ctrl Pts',(19.2436543448456,5.24952393634133,36.3235148555594));
#40638=CARTESIAN_POINT('Ctrl Pts',(19.0720726325909,5.26308032836566,36.4051333609403));
#40639=CARTESIAN_POINT('Ctrl Pts',(18.9770259977916,5.27090122199522,36.4607464563682));
#40640=CARTESIAN_POINT('Ctrl Pts',(18.8797410055104,5.278903014203,36.5294439590056));
#40641=CARTESIAN_POINT('Ctrl Pts',(18.8722947274666,5.27951537793363,36.5347820218623));
#40642=CARTESIAN_POINT('Ctrl Pts',(18.8612442407492,5.28042365209288,36.5428236548198));
#40643=CARTESIAN_POINT('Ctrl Pts',(18.857611147912,5.28072218736542,36.5454870341925));
#40644=CARTESIAN_POINT('Ctrl Pts',(18.8512123172242,5.28124779628259,36.550212492777));
#40645=CARTESIAN_POINT('Ctrl Pts',(18.8484427580593,5.28147522588062,36.5522692815515));
#40646=CARTESIAN_POINT('Ctrl Pts',(18.845664805945,5.28170327521311,36.55434388787));
#40647=CARTESIAN_POINT('Ctrl Pts',(18.8456509506368,5.28170441262985,36.5543542354623));
#40648=CARTESIAN_POINT('Ctrl Pts',(18.845623427101,5.28170667210218,36.5543747915057));
#40649=CARTESIAN_POINT('Ctrl Pts',(18.8456097587989,5.28170779416393,36.5543850000047));
#40650=CARTESIAN_POINT('Ctrl Pts',(18.8455826057029,5.28171002321967,36.5544052805061));
#40651=CARTESIAN_POINT('Ctrl Pts',(18.8455691208838,5.28171113021578,36.5544153525199));
#40652=CARTESIAN_POINT('Ctrl Pts',(18.8455423305775,5.28171332948321,36.5544353631481));
#40653=CARTESIAN_POINT('Ctrl Pts',(18.84552902539,5.28171442172997,36.5544453015313));
#40654=CARTESIAN_POINT('Ctrl Pts',(18.8455025920378,5.2817165916884,36.5544650466013));
#40655=CARTESIAN_POINT('Ctrl Pts',(18.845489463514,5.28171766942958,36.5544748535494));
#40656=CARTESIAN_POINT('Ctrl Pts',(18.8454633789171,5.28171981075229,36.5544943391433));
#40657=CARTESIAN_POINT('Ctrl Pts',(18.8454504232254,5.28172087430256,36.5545040174976));
#40658=CARTESIAN_POINT('Ctrl Pts',(18.8454246820194,5.28172298743017,36.5545232475819));
#40659=CARTESIAN_POINT('Ctrl Pts',(18.8454118961795,5.28172403703428,36.5545327995487));
#40660=CARTESIAN_POINT('Ctrl Pts',(18.8453864913349,5.28172612254409,36.5545517793351));
#40661=CARTESIAN_POINT('Ctrl Pts',(18.8453738721528,5.28172715846437,36.554561207281));
#40662=CARTESIAN_POINT('Ctrl Pts',(18.8453487973774,5.28172921687311,36.5545799414322));
#40663=CARTESIAN_POINT('Ctrl Pts',(18.8453363417272,5.28173023936627,36.5545892476736));
#40664=CARTESIAN_POINT('Ctrl Pts',(18.8453115910356,5.28173227116552,36.5546077406242));
#40665=CARTESIAN_POINT('Ctrl Pts',(18.8452992959989,5.28173328047124,36.5546169273236));
#40666=CARTESIAN_POINT('Ctrl Pts',(18.8420006721966,5.28200406581114,36.5570816795884));
#40667=CARTESIAN_POINT('Ctrl Pts',(18.8387221471511,5.28227311036255,36.5595477495515));
#40668=CARTESIAN_POINT('Ctrl Pts',(18.8319311333881,5.28283026786957,36.5646898756521));
#40669=CARTESIAN_POINT('Ctrl Pts',(18.8284199111907,5.28311826687096,36.5673675745606));
#40670=CARTESIAN_POINT('Ctrl Pts',(18.8194628901142,5.28385284418345,36.5742470711878));
#40671=CARTESIAN_POINT('Ctrl Pts',(18.8140302584486,5.28429828707388,36.5784660230361));
#40672=CARTESIAN_POINT('Ctrl Pts',(18.798297929349,5.28558834868718,36.5908191186834));
#40673=CARTESIAN_POINT('Ctrl Pts',(18.7880583086152,5.28642813795777,36.5990295949475));
#40674=CARTESIAN_POINT('Ctrl Pts',(18.7526196625938,5.28933823752594,36.6280446321233));
#40675=CARTESIAN_POINT('Ctrl Pts',(18.7278648618391,5.29137757418001,36.6493853872163));
#40676=CARTESIAN_POINT('Ctrl Pts',(18.5880166134659,5.30301704850862,36.7762813920258));
#40677=CARTESIAN_POINT('Ctrl Pts',(18.4855340531755,5.31207123245999,36.8948743762722));
#40678=CARTESIAN_POINT('Ctrl Pts',(18.3776507371344,5.32385523265671,37.0555291130434));
#40679=CARTESIAN_POINT('Ctrl Pts',(18.3577412832574,5.3261494613199,37.0871216027717));
#40680=CARTESIAN_POINT('Ctrl Pts',(18.317133253641,5.33111965503504,37.1559067487322));
#40681=CARTESIAN_POINT('Ctrl Pts',(18.2967239919146,5.33380288792504,37.1932459157702));
#40682=CARTESIAN_POINT('Ctrl Pts',(18.2721130645705,5.33730601563086,37.2420396577662));
#40683=CARTESIAN_POINT('Ctrl Pts',(18.2667614041317,5.33808572160354,37.2529030932484));
#40684=CARTESIAN_POINT('Ctrl Pts',(18.2584030466508,5.33933293788077,37.2702807280347));
#40685=CARTESIAN_POINT('Ctrl Pts',(18.2553297364744,5.33979814769447,37.2767626785326));
#40686=CARTESIAN_POINT('Ctrl Pts',(18.249866856376,5.34063717813907,37.2884524863122));
#40687=CARTESIAN_POINT('Ctrl Pts',(18.2474641884693,5.34101054424518,37.2936541588725));
#40688=CARTESIAN_POINT('Ctrl Pts',(18.2418856455968,5.34188775818746,37.3058741807215));
#40689=CARTESIAN_POINT('Ctrl Pts',(18.2387285838179,5.34239224043633,37.3129009619827));
#40690=CARTESIAN_POINT('Ctrl Pts',(18.2297248228618,5.34385465559077,37.3332663724761));
#40691=CARTESIAN_POINT('Ctrl Pts',(18.2239870805046,5.34481625270566,37.3466523057182));
#40692=CARTESIAN_POINT('Ctrl Pts',(18.179837001073,5.35245761640374,37.4529611091737));
#40693=CARTESIAN_POINT('Ctrl Pts',(18.1485976195904,5.35937720480023,37.5486779431821));
#40694=CARTESIAN_POINT('Ctrl Pts',(18.0889769732398,5.37723970142802,37.7951195524543));
#40695=CARTESIAN_POINT('Ctrl Pts',(18.0708211705784,5.38836245992606,37.94760092491));
#40696=CARTESIAN_POINT('Ctrl Pts',(18.070870098622,5.39889951889677,38.1006168544168));
#40697=CARTESIAN_POINT('Ctrl Pts',(18.070870099365,5.39889967859844,38.1006191735561));
#40698=CARTESIAN_POINT('Ctrl Pts',(18.0708758483007,5.40013312137755,38.1185308618298));
#40699=CARTESIAN_POINT('Ctrl Pts',(18.0711310585434,5.40135730436667,38.1364424185093));
#40700=CARTESIAN_POINT('Ctrl Pts',(18.0719614696151,5.40335315052469,38.1659065598357));
#40701=CARTESIAN_POINT('Ctrl Pts',(18.0723911311066,5.40413133583061,38.1774616899035));
#40702=CARTESIAN_POINT('Ctrl Pts',(18.0731479842833,5.40522773943072,38.1938471596201));
#40703=CARTESIAN_POINT('Ctrl Pts',(18.0733894908621,5.40555030754759,38.1986809360689));
#40704=CARTESIAN_POINT('Ctrl Pts',(18.0738420528639,5.40611074099713,38.2071029344015));
#40705=CARTESIAN_POINT('Ctrl Pts',(18.0740449489794,5.40634903990194,38.2106915436682));
#40706=CARTESIAN_POINT('Ctrl Pts',(18.0744579567,5.40681019046718,38.2176511966592));
#40707=CARTESIAN_POINT('Ctrl Pts',(18.074666894603,5.40703310640091,38.2210223059762));
#40708=CARTESIAN_POINT('Ctrl Pts',(18.075102271927,5.40747772334534,38.2277602428641));
#40709=CARTESIAN_POINT('Ctrl Pts',(18.0753286918662,5.40769942559883,38.2311270348945));
#40710=CARTESIAN_POINT('Ctrl Pts',(18.0759570893528,5.40829032588631,38.2401186445076));
#40711=CARTESIAN_POINT('Ctrl Pts',(18.0763749018921,5.40865865077766,38.245742376939));
#40712=CARTESIAN_POINT('Ctrl Pts',(18.0779785913214,5.40998890025745,38.2661183044184));
#40713=CARTESIAN_POINT('Ctrl Pts',(18.079309594352,5.41094314272288,38.2808590177023));
#40714=CARTESIAN_POINT('Ctrl Pts',(18.0834634488418,5.41356290889723,38.3216192853597));
#40715=CARTESIAN_POINT('Ctrl Pts',(18.0866464121309,5.41521142985344,38.3475997807835));
#40716=CARTESIAN_POINT('Ctrl Pts',(18.1123867324077,5.42651647163107,38.5273191130625));
#40717=CARTESIAN_POINT('Ctrl Pts',(18.152919352461,5.43552899386554,38.6779169439124));
#40718=CARTESIAN_POINT('Ctrl Pts',(18.2444468565024,5.45033123750452,38.9046866070681));
#40719=CARTESIAN_POINT('Ctrl Pts',(18.2834916888199,5.45582869757392,38.9849200305202));
#40720=CARTESIAN_POINT('Ctrl Pts',(18.3350382802463,5.46243534677084,39.0744986678629));
#40721=CARTESIAN_POINT('Ctrl Pts',(18.3422740423502,5.46334997999109,39.0867572212886));
#40722=CARTESIAN_POINT('Ctrl Pts',(18.3535977412813,5.46476264200826,39.1054652852563));
#40723=CARTESIAN_POINT('Ctrl Pts',(18.35758951867,5.46525718787271,39.1119726505313));
#40724=CARTESIAN_POINT('Ctrl Pts',(18.3649365830653,5.46616130031312,39.1237918004788));
#40725=CARTESIAN_POINT('Ctrl Pts',(18.3682794093943,5.46657040710039,39.1291112382836));
#40726=CARTESIAN_POINT('Ctrl Pts',(18.3756329817706,5.46746553320255,39.1406870686856));
#40727=CARTESIAN_POINT('Ctrl Pts',(18.3796540020045,5.46795192668774,39.1469367836803));
#40728=CARTESIAN_POINT('Ctrl Pts',(18.3907711961082,5.46928844498812,39.1639983383249));
#40729=CARTESIAN_POINT('Ctrl Pts',(18.3979400344247,5.47014125668199,39.1747621412021));
#40730=CARTESIAN_POINT('Ctrl Pts',(18.4353772815578,5.4745498315613,39.2297661961875));
#40731=CARTESIAN_POINT('Ctrl Pts',(18.4673692106458,5.47817010583034,39.272799139087));
#40732=CARTESIAN_POINT('Ctrl Pts',(18.5134914169344,5.48320397748046,39.3297242363422));
#40733=CARTESIAN_POINT('Ctrl Pts',(18.5261068954014,5.48456341285575,39.3448166691896));
#40734=CARTESIAN_POINT('Ctrl Pts',(18.6261196246063,5.4952053052101,39.4608141361822));
#40735=CARTESIAN_POINT('Ctrl Pts',(18.7235428738316,5.50482058275442,39.5525885494307));
#40736=CARTESIAN_POINT('Ctrl Pts',(18.8705854940537,5.5179285444647,39.6648060545403));
#40737=CARTESIAN_POINT('Ctrl Pts',(18.9127656915284,5.52154545008529,39.6944019052689));
#40738=CARTESIAN_POINT('Ctrl Pts',(18.9710987046413,5.52631309463113,39.7319385803451));
#40739=CARTESIAN_POINT('Ctrl Pts',(18.9862487934323,5.52753091123424,39.7413926853754));
#40740=CARTESIAN_POINT('Ctrl Pts',(19.0088560514611,5.52931580059844,39.7550678441187));
#40741=CARTESIAN_POINT('Ctrl Pts',(19.0162131404572,5.52989166956653,39.7594515108055));
#40742=CARTESIAN_POINT('Ctrl Pts',(19.0295865114951,5.53092912644573,39.7672997360742));
#40743=CARTESIAN_POINT('Ctrl Pts',(19.0355927230888,5.53139169342091,39.7707810617926));
#40744=CARTESIAN_POINT('Ctrl Pts',(19.0450865995588,5.53211740654303,39.7762156576));
#40745=CARTESIAN_POINT('Ctrl Pts',(19.0485616931984,5.53238189901771,39.7781905976965));
#40746=CARTESIAN_POINT('Ctrl Pts',(19.0520533045682,5.53264648385942,39.7801605934141));
#40747=CARTESIAN_POINT('Ctrl Pts',(19.0520636696433,5.53264726928643,39.7801664413479));
#40748=CARTESIAN_POINT('Ctrl Pts',(19.0520844520583,5.53264884408027,39.7801781664495));
#40749=CARTESIAN_POINT('Ctrl Pts',(19.0520948692226,5.53264963343369,39.780184043517));
#40750=CARTESIAN_POINT('Ctrl Pts',(19.0521157551074,5.53265121602636,39.7801958264824));
#40751=CARTESIAN_POINT('Ctrl Pts',(19.0521262249653,5.53265200935169,39.7802017330208));
#40752=CARTESIAN_POINT('Ctrl Pts',(19.0521483760127,5.53265368776555,39.7802142291936));
#40753=CARTESIAN_POINT('Ctrl Pts',(19.0521600563483,5.53265457278681,39.7802208183147));
#40754=CARTESIAN_POINT('Ctrl Pts',(19.0521836722353,5.53265636214071,39.780234140205));
#40755=CARTESIAN_POINT('Ctrl Pts',(19.0521956085007,5.53265726652686,39.7802408733698));
#40756=CARTESIAN_POINT('Ctrl Pts',(19.0550720166701,5.53287520274175,39.7818633949258));
#40757=CARTESIAN_POINT('Ctrl Pts',(19.0579405781833,5.53309175577294,39.7834718348901));
#40758=CARTESIAN_POINT('Ctrl Pts',(19.0647331726977,5.53360269576753,39.7872577328871));
#40759=CARTESIAN_POINT('Ctrl Pts',(19.0686606989361,5.53389667753351,39.7894288392055));
#40760=CARTESIAN_POINT('Ctrl Pts',(19.0805543489085,5.53478268062025,39.7959494767319));
#40761=CARTESIAN_POINT('Ctrl Pts',(19.0885437654327,5.53537209393245,39.8002565904101));
#40762=CARTESIAN_POINT('Ctrl Pts',(19.1530609736911,5.54008815712808,39.8344525155766));
#40763=CARTESIAN_POINT('Ctrl Pts',(19.2110191533079,5.54405698001466,39.8615738287022));
#40764=CARTESIAN_POINT('Ctrl Pts',(19.3813399937013,5.55526541653116,39.9311775281476));
#40765=CARTESIAN_POINT('Ctrl Pts',(19.4964545312734,5.56231026438453,39.9661177640241));
#40766=CARTESIAN_POINT('Ctrl Pts',(19.6761381419853,5.5733835185158,40.0028054669264));
#40767=CARTESIAN_POINT('Ctrl Pts',(19.7387845514535,5.57725465579278,40.0124122560933));
#40768=CARTESIAN_POINT('Ctrl Pts',(19.8391194556964,5.58355970276966,40.0227762821035));
#40769=CARTESIAN_POINT('Ctrl Pts',(19.8765548817508,5.58593477002806,40.0255420498551));
#40770=CARTESIAN_POINT('Ctrl Pts',(19.9251565513025,5.58905773563377,40.0277097086844));
#40771=CARTESIAN_POINT('Ctrl Pts',(19.9362717033187,5.58977460568774,40.0281091666567));
#40772=CARTESIAN_POINT('Ctrl Pts',(19.9543422733671,5.5909446265755,40.0286021637212));
#40773=CARTESIAN_POINT('Ctrl Pts',(19.9612959432389,5.59139595506338,40.028754242459));
#40774=CARTESIAN_POINT('Ctrl Pts',(19.9746660451756,5.59226591657799,40.0289743185801));
#40775=CARTESIAN_POINT('Ctrl Pts',(19.9810823026998,5.59268436990603,40.0290479128508));
#40776=CARTESIAN_POINT('Ctrl Pts',(19.9957735647982,5.59364475790508,40.029143117989));
#40777=CARTESIAN_POINT('Ctrl Pts',(20.0040485345194,5.59418734454889,40.0291434986057));
#40778=CARTESIAN_POINT('Ctrl Pts',(20.0260459265559,5.59563418678428,40.029002977985));
#40779=CARTESIAN_POINT('Ctrl Pts',(20.0397670742948,5.59654131220904,40.0287688930256));
#40780=CARTESIAN_POINT('Ctrl Pts',(20.1550606952596,5.60420392711273,40.0255711999786));
#40781=CARTESIAN_POINT('Ctrl Pts',(20.2562387416506,5.61120490286912,40.0147333841997));
#40782=CARTESIAN_POINT('Ctrl Pts',(20.4436840943488,5.62465253914239,39.9795298158322));
#40783=CARTESIAN_POINT('Ctrl Pts',(20.5300414479743,5.6310433905727,39.9570252858446));
#40784=CARTESIAN_POINT('Ctrl Pts',(20.6895375932326,5.64300963546121,39.9034251217219));
#40785=CARTESIAN_POINT('Ctrl Pts',(20.7629327994287,5.64858338844913,39.8736235593879));
#40786=CARTESIAN_POINT('Ctrl Pts',(20.8472400956338,5.65491695871823,39.8331857540802));
#40787=CARTESIAN_POINT('Ctrl Pts',(20.8601144796393,5.65588207762976,39.8268328667703));
#40788=CARTESIAN_POINT('Ctrl Pts',(20.8777320072592,5.65719870596666,39.8178935448074));
#40789=CARTESIAN_POINT('Ctrl Pts',(20.8825366028216,5.6575573530647,39.8154302242512));
#40790=CARTESIAN_POINT('Ctrl Pts',(20.8906134889532,5.65815947805892,39.8112462819061));
#40791=CARTESIAN_POINT('Ctrl Pts',(20.8938912620062,5.65840361349351,39.8095363805677));
#40792=CARTESIAN_POINT('Ctrl Pts',(20.9001073469168,5.65886615405571,39.8062708969972));
#40793=CARTESIAN_POINT('Ctrl Pts',(20.9030465758143,5.65908467367462,39.8047171296851));
#40794=CARTESIAN_POINT('Ctrl Pts',(20.9107280252094,5.65965530092272,39.8006310363675));
#40795=CARTESIAN_POINT('Ctrl Pts',(20.9154637449066,5.66000664326744,39.7980864498669));
#40796=CARTESIAN_POINT('Ctrl Pts',(20.9317864223115,5.66121625382766,39.7892278535447));
#40797=CARTESIAN_POINT('Ctrl Pts',(20.9433195096781,5.66206853811522,39.7828146076584));
#40798=CARTESIAN_POINT('Ctrl Pts',(21.0795538457874,5.67211860184255,39.7052175383931));
#40799=CARTESIAN_POINT('Ctrl Pts',(21.196017600816,5.68055720790592,39.6204324714698));
#40800=CARTESIAN_POINT('Ctrl Pts',(21.3964109581428,5.69680120294204,39.4371417801357));
#40801=CARTESIAN_POINT('Ctrl Pts',(21.4819803115996,5.70453913883986,39.3416277133483));
#40802=CARTESIAN_POINT('Ctrl Pts',(21.5663455485792,5.7136693137624,39.2262019470784));
#40803=CARTESIAN_POINT('Ctrl Pts',(21.5750863987229,5.71463594782367,39.2139443518821));
#40804=CARTESIAN_POINT('Ctrl Pts',(21.5881399291552,5.71611205694871,39.1951780906876));
#40805=CARTESIAN_POINT('Ctrl Pts',(21.5925581750365,5.71661753508635,39.1887432852019));
#40806=CARTESIAN_POINT('Ctrl Pts',(21.6004998562707,5.71753692526343,39.1770251127813));
#40807=CARTESIAN_POINT('Ctrl Pts',(21.6040365039909,5.71795033412957,39.1717507992725));
#40808=CARTESIAN_POINT('Ctrl Pts',(21.6115896604104,5.71884192049574,39.160365408868));
#40809=CARTESIAN_POINT('Ctrl Pts',(21.6155975802933,5.71932040924536,39.1542487799098));
#40810=CARTESIAN_POINT('Ctrl Pts',(21.6263159373185,5.72061477769129,39.1376864509129));
#40811=CARTESIAN_POINT('Ctrl Pts',(21.6329603796871,5.72143307177949,39.1271986587672));
#40812=CARTESIAN_POINT('Ctrl Pts',(21.6644309550074,5.72538709054735,39.0764474454335));
#40813=CARTESIAN_POINT('Ctrl Pts',(21.6878699205483,5.72857247786237,39.0353472563209));
#40814=CARTESIAN_POINT('Ctrl Pts',(21.7242511987213,5.73394578996075,38.965723751978));
#40815=CARTESIAN_POINT('Ctrl Pts',(21.738052750229,5.73610481513327,38.9376707474733));
#40816=CARTESIAN_POINT('Ctrl Pts',(21.8217739162041,5.75000267504645,38.7565137052161));
#40817=CARTESIAN_POINT('Ctrl Pts',(21.8720766019104,5.76226643378934,38.5951681773285));
#40818=CARTESIAN_POINT('Ctrl Pts',(21.9072842820847,5.77658140775331,38.3919734362554));
#40819=CARTESIAN_POINT('Ctrl Pts',(21.9126577120263,5.77917832794206,38.3544066993405));
#40820=CARTESIAN_POINT('Ctrl Pts',(21.9177670640176,5.78222489540596,38.309210193155));
#40821=CARTESIAN_POINT('Ctrl Pts',(21.9185701869868,5.78272774784621,38.3017123173458));
#40822=CARTESIAN_POINT('Ctrl Pts',(21.9197488176348,5.78350477372963,38.2900641889728));
#40823=CARTESIAN_POINT('Ctrl Pts',(21.9201548666475,5.78378059249129,38.2859172064261));
#40824=CARTESIAN_POINT('Ctrl Pts',(21.9208826378231,5.78429047111685,38.2782276668159));
#40825=CARTESIAN_POINT('Ctrl Pts',(21.9212079958109,5.78452472416589,38.2746855652051));
#40826=CARTESIAN_POINT('Ctrl Pts',(21.9219228477075,5.78505413959939,38.2666594767871));
#40827=CARTESIAN_POINT('Ctrl Pts',(21.922306447129,5.78534897129088,38.2621750229971));
#40828=CARTESIAN_POINT('Ctrl Pts',(21.9234216232755,5.78624008727771,38.2485778938532));
#40829=CARTESIAN_POINT('Ctrl Pts',(21.924104135412,5.78683371906063,38.2394611612914));
#40830=CARTESIAN_POINT('Ctrl Pts',(21.932180418756,5.79455311016005,38.1201989694553));
#40831=CARTESIAN_POINT('Ctrl Pts',(21.9301723148688,5.80120146158693,38.0096030486418));
#40832=CARTESIAN_POINT('Ctrl Pts',(21.9098718888338,5.81290228251413,37.8150715432262));
#40833=CARTESIAN_POINT('Ctrl Pts',(21.8954341166906,5.81795856576337,37.7310503273799));
#40834=CARTESIAN_POINT('Ctrl Pts',(21.8576407027621,5.82775202300741,37.5741428802481));
#40835=CARTESIAN_POINT('Ctrl Pts',(21.8354124924511,5.83245790202405,37.5011563819534));
#40836=CARTESIAN_POINT('Ctrl Pts',(21.8023844611312,5.83850211502345,37.4120266652434));
#40837=CARTESIAN_POINT('Ctrl Pts',(21.7955842961783,5.83970740846969,37.3944689585096));
#40838=CARTESIAN_POINT('Ctrl Pts',(21.785327833543,5.84147180180845,37.3690964383539));
#40839=CARTESIAN_POINT('Ctrl Pts',(21.782074749021,5.84202411927537,37.3612002472254));
#40840=CARTESIAN_POINT('Ctrl Pts',(21.7762786512293,5.8429957162594,37.3473924521641));
#40841=CARTESIAN_POINT('Ctrl Pts',(21.7737582694162,5.84341422908841,37.3414714455733));
#40842=CARTESIAN_POINT('Ctrl Pts',(21.7688051610563,5.84422911463879,37.3299950396324));
#40843=CARTESIAN_POINT('Ctrl Pts',(21.7663757668086,5.84462537059331,37.3244382772515));
#40844=CARTESIAN_POINT('Ctrl Pts',(21.760501062464,5.84557552158884,37.3111718343784));
#40845=CARTESIAN_POINT('Ctrl Pts',(21.7570312765878,5.84613024390353,37.3034731924908));
#40846=CARTESIAN_POINT('Ctrl Pts',(21.7442809250743,5.84814575762447,37.2756718762842));
#40847=CARTESIAN_POINT('Ctrl Pts',(21.7347052847342,5.84961658378573,37.2557072147597));
#40848=CARTESIAN_POINT('Ctrl Pts',(21.6599882317999,5.86078648508399,37.1065659452504));
#40849=CARTESIAN_POINT('Ctrl Pts',(21.5808558218101,5.87099035312545,36.9849432105268));
#40850=CARTESIAN_POINT('Ctrl Pts',(21.4333081790877,5.88754632416385,36.8058542820126));
#40851=CARTESIAN_POINT('Ctrl Pts',(21.373192692474,5.89379416816922,36.7422337980891));
#40852=CARTESIAN_POINT('Ctrl Pts',(21.2817034810973,5.90243389457611,36.6577253623186));
#40853=CARTESIAN_POINT('Ctrl Pts',(21.2537177505086,5.9049730145111,36.633332965432));
#40854=CARTESIAN_POINT('Ctrl Pts',(21.2192544383971,5.9079609395254,36.6050025648526));
#40855=CARTESIAN_POINT('Ctrl Pts',(21.2134375959729,5.90846065063173,36.6002773850281));
#40856=CARTESIAN_POINT('Ctrl Pts',(21.2043517295514,5.90923388039877,36.5929841586359));
#40857=CARTESIAN_POINT('Ctrl Pts',(21.2011017700371,5.90950901924342,36.5903926426322));
#40858=CARTESIAN_POINT('Ctrl Pts',(21.1950543718507,5.91001827957521,36.5856023425361));
#40859=CARTESIAN_POINT('Ctrl Pts',(21.1922592508739,5.91025259023174,36.5834008124568));
#40860=CARTESIAN_POINT('Ctrl Pts',(21.1859038388258,5.91078294755072,36.57842350782));
#40861=CARTESIAN_POINT('Ctrl Pts',(21.1823398917859,5.91107865852928,36.5756524944056));
#40862=CARTESIAN_POINT('Ctrl Pts',(21.1714753566938,5.91197508073917,36.5672662090657));
#40863=CARTESIAN_POINT('Ctrl Pts',(21.1641441225627,5.91257309287245,36.5616905853233));
#40864=CARTESIAN_POINT('Ctrl Pts',(21.1006849705012,5.91769327945025,36.5141414892252));
#40865=CARTESIAN_POINT('Ctrl Pts',(21.0423411681404,5.92202547657566,36.4751978863419));
#40866=CARTESIAN_POINT('Ctrl Pts',(20.8405689638211,5.93625292473153,36.3558712590347));
#40867=CARTESIAN_POINT('Ctrl Pts',(20.6890364644856,5.94579881061955,36.2906432455044));
#40868=CARTESIAN_POINT('Ctrl Pts',(20.4844856463549,5.95898810760875,36.2320696059507));
#40869=CARTESIAN_POINT('Ctrl Pts',(20.4374217475012,5.96203680082886,36.220491580796));
#40870=CARTESIAN_POINT('Ctrl Pts',(20.3781110988416,5.96591887000632,36.2082491447454));
#40871=CARTESIAN_POINT('Ctrl Pts',(20.3662248029209,5.96669881469924,36.2059121761912));
#40872=CARTESIAN_POINT('Ctrl Pts',(20.347265069235,5.96794632433479,36.2023696351068));
#40873=CARTESIAN_POINT('Ctrl Pts',(20.3402054209525,5.96841158688436,36.2010912872572));
#40874=CARTESIAN_POINT('Ctrl Pts',(20.3268681731558,5.9692920620867,36.1987529658753));
#40875=CARTESIAN_POINT('Ctrl Pts',(20.3205921221781,5.96970700474749,36.1976846273648));
#40876=CARTESIAN_POINT('Ctrl Pts',(20.306412999504,5.97064591576889,36.1953431517874));
#40877=CARTESIAN_POINT('Ctrl Pts',(20.2985070994508,5.97117044577746,36.1940881069593));
#40878=CARTESIAN_POINT('Ctrl Pts',(20.2782086909663,5.97251989372608,36.1909951725188));
#40879=CARTESIAN_POINT('Ctrl Pts',(20.2658058307352,5.97334703522875,36.1892287539085));
#40880=CARTESIAN_POINT('Ctrl Pts',(20.188383105047,5.97852727952747,36.1789705797588));
#40881=CARTESIAN_POINT('Ctrl Pts',(20.1229898042634,5.98297928611301,36.1736786299597));
#40882=CARTESIAN_POINT('Ctrl Pts',(19.9188178335748,5.99712366081145,36.1675945669214));
#40883=CARTESIAN_POINT('Ctrl Pts',(19.7801431764037,6.0071133681178,36.1784285868496));
#40884=CARTESIAN_POINT('Ctrl Pts',(19.5758830278839,6.02184670502054,36.216797957994));
#40885=CARTESIAN_POINT('Ctrl Pts',(19.5086436346707,6.02669149321243,36.2332123581034));
#40886=CARTESIAN_POINT('Ctrl Pts',(19.4295815711161,6.03227815320782,36.2570823786264));
#40887=CARTESIAN_POINT('Ctrl Pts',(19.4167786148593,6.03317925292829,36.2610939709181));
#40888=CARTESIAN_POINT('Ctrl Pts',(19.4007105215328,6.03430474293813,36.2663133385327));
#40889=CARTESIAN_POINT('Ctrl Pts',(19.3974058055968,6.03453593175069,36.2673966908421));
#40890=CARTESIAN_POINT('Ctrl Pts',(19.3941040087491,6.0347666134114,36.2684889831928));
#40891=CARTESIAN_POINT('Origin',(20.,-1.3495818343519,38.1));
#40892=CARTESIAN_POINT('',(19.394104010982,6.99874099840483,36.2684889824541));
#40893=CARTESIAN_POINT('',(19.3941039843085,6.82605087843334,36.2684889912782));
#40894=CARTESIAN_POINT('',(19.3941040087494,-1.3495818343519,36.2684889831927));
#40895=CARTESIAN_POINT('',(18.0708702248395,6.36356089767328,38.1009313909468));
#40896=CARTESIAN_POINT('Ctrl Pts',(19.394104010982,6.99874099840483,36.2684889824541));
#40897=CARTESIAN_POINT('Ctrl Pts',(19.3969825380143,6.99855649777902,36.2675367151915));
#40898=CARTESIAN_POINT('Ctrl Pts',(19.3998634709182,6.99837185025014,36.266591180833));
#40899=CARTESIAN_POINT('Ctrl Pts',(19.4294489278064,6.9964756380809,36.2569583233041));
#40900=CARTESIAN_POINT('Ctrl Pts',(19.4563368713021,6.9947523103515,36.2488486131989));
#40901=CARTESIAN_POINT('Ctrl Pts',(19.5306214382265,6.98997810224285,36.2282015816547));
#40902=CARTESIAN_POINT('Ctrl Pts',(19.5783310892964,6.98689693497634,36.2168801816735));
#40903=CARTESIAN_POINT('Ctrl Pts',(19.6387578306271,6.98295202472202,36.2049525394638));
#40904=CARTESIAN_POINT('Ctrl Pts',(19.6511217809934,6.98214268879871,36.2026374203114));
#40905=CARTESIAN_POINT('Ctrl Pts',(19.670745012419,6.98085437036893,36.1991613064221));
#40906=CARTESIAN_POINT('Ctrl Pts',(19.6779899539549,6.98037790445743,36.1979205816724));
#40907=CARTESIAN_POINT('Ctrl Pts',(19.6915042094846,6.97948754014319,36.1956856363961));
#40908=CARTESIAN_POINT('Ctrl Pts',(19.6977717016498,6.97907397921481,36.1946808922749));
#40909=CARTESIAN_POINT('Ctrl Pts',(19.7117095625718,6.9781528200299,36.1925170097395));
#40910=CARTESIAN_POINT('Ctrl Pts',(19.7193821615316,6.97764474828788,36.1913731741848));
#40911=CARTESIAN_POINT('Ctrl Pts',(19.7417343778093,6.97616162673869,36.1881785856046));
#40912=CARTESIAN_POINT('Ctrl Pts',(19.7564307212911,6.97518275070171,36.1862507379818));
#40913=CARTESIAN_POINT('Ctrl Pts',(19.8826959645587,6.96673876574513,36.1711653788264));
#40914=CARTESIAN_POINT('Ctrl Pts',(19.9951751024177,6.958970909739,36.1676097961494));
#40915=CARTESIAN_POINT('Ctrl Pts',(20.2313615024685,6.94223280054393,36.1807679512967));
#40916=CARTESIAN_POINT('Ctrl Pts',(20.3544560244407,6.93325909401283,36.1996471662492));
#40917=CARTESIAN_POINT('Ctrl Pts',(20.5165591029919,6.92159881364518,36.2408178029232));
#40918=CARTESIAN_POINT('Ctrl Pts',(20.5578763458919,6.91864371940896,36.2527949790388));
#40919=CARTESIAN_POINT('Ctrl Pts',(20.6058270547113,6.91526036063549,36.2684511004375));
#40920=CARTESIAN_POINT('Ctrl Pts',(20.6128787721056,6.91476399180772,36.2707986970317));
#40921=CARTESIAN_POINT('Ctrl Pts',(20.624264642262,6.91396467560942,36.2746624166818));
#40922=CARTESIAN_POINT('Ctrl Pts',(20.628607175102,6.9136603231646,36.2761533350788));
#40923=CARTESIAN_POINT('Ctrl Pts',(20.6363117517574,6.91312128537265,36.2788293274865));
#40924=CARTESIAN_POINT('Ctrl Pts',(20.6396758700575,6.91288624517374,36.2800082291756));
#40925=CARTESIAN_POINT('Ctrl Pts',(20.6469053502762,6.91238185347314,36.2825642071469));
#40926=CARTESIAN_POINT('Ctrl Pts',(20.6507695843416,6.91211268160553,36.2839442898876));
#40927=CARTESIAN_POINT('Ctrl Pts',(20.6614485842059,6.91136992831127,36.2877966781647));
#40928=CARTESIAN_POINT('Ctrl Pts',(20.6682539499171,6.910897857536,36.2902951147475));
#40929=CARTESIAN_POINT('Ctrl Pts',(20.7060775625588,6.90828031079725,36.3044236555528));
#40930=CARTESIAN_POINT('Ctrl Pts',(20.7368084816679,6.90617680768287,36.3168136627134));
#40931=CARTESIAN_POINT('Ctrl Pts',(20.8331328662127,6.89961154936868,36.3585652669897));
#40932=CARTESIAN_POINT('Ctrl Pts',(20.897416268238,6.89527099233744,36.390803976408));
#40933=CARTESIAN_POINT('Ctrl Pts',(21.1045964293148,6.88095703353016,36.509626238483));
#40934=CARTESIAN_POINT('Ctrl Pts',(21.2380230987505,6.87112558392545,36.611136333886));
#40935=CARTESIAN_POINT('Ctrl Pts',(21.3713356552431,6.85922844029134,36.7430165321513));
#40936=CARTESIAN_POINT('Ctrl Pts',(21.3857252286921,6.85791399777198,36.7577142069176));
#40937=CARTESIAN_POINT('Ctrl Pts',(21.4055105618989,6.85606206603671,36.7785804365622));
#40938=CARTESIAN_POINT('Ctrl Pts',(21.4111065399666,6.85553313681933,36.7845578949552));
#40939=CARTESIAN_POINT('Ctrl Pts',(21.4207355664862,6.85461393846064,36.7949754849916));
#40940=CARTESIAN_POINT('Ctrl Pts',(21.4247863042118,6.85422442247484,36.7993991693705));
#40941=CARTESIAN_POINT('Ctrl Pts',(21.4331672555705,6.85341256146144,36.8086378860833));
#40942=CARTESIAN_POINT('Ctrl Pts',(21.4374939804497,6.85299007768223,36.8134559680452));
#40943=CARTESIAN_POINT('Ctrl Pts',(21.4476356187059,6.85199178602018,36.8248643534782));
#40944=CARTESIAN_POINT('Ctrl Pts',(21.4534298761918,6.85141513348374,36.8314727467411));
#40945=CARTESIAN_POINT('Ctrl Pts',(21.4724059782312,6.84950548961063,36.8534158259916));
#40946=CARTESIAN_POINT('Ctrl Pts',(21.485391504689,6.84816455162974,36.8689177554752));
#40947=CARTESIAN_POINT('Ctrl Pts',(21.6122812323686,6.83471025071618,37.025327642816));
#40948=CARTESIAN_POINT('Ctrl Pts',(21.7060184952387,6.82175756306093,37.1813906103987));
#40949=CARTESIAN_POINT('Ctrl Pts',(21.811065691505,6.80257897925162,37.4296233467429));
#40950=CARTESIAN_POINT('Ctrl Pts',(21.839894841344,6.79634838858619,37.5133530302575));
#40951=CARTESIAN_POINT('Ctrl Pts',(21.8653146567028,6.78977242212699,37.6078295910765));
#40952=CARTESIAN_POINT('Ctrl Pts',(21.8676849226925,6.78914550667107,37.6169021649875));
#40953=CARTESIAN_POINT('Ctrl Pts',(21.8711063327219,6.78821996030603,37.6303998222863));
#40954=CARTESIAN_POINT('Ctrl Pts',(21.8722080901398,6.78791855925692,37.6348117547409));
#40955=CARTESIAN_POINT('Ctrl Pts',(21.8741447165574,6.78738274612209,37.642685210517));
#40956=CARTESIAN_POINT('Ctrl Pts',(21.8749856102546,6.78714799553545,37.6461451803262));
#40957=CARTESIAN_POINT('Ctrl Pts',(21.8767818734168,6.78664195979787,37.6536263467126));
#40958=CARTESIAN_POINT('Ctrl Pts',(21.8777338995115,6.78637086624412,37.6576482822989));
#40959=CARTESIAN_POINT('Ctrl Pts',(21.8803510883801,6.78561735930349,37.6688655820768));
#40960=CARTESIAN_POINT('Ctrl Pts',(21.8819878899519,6.78513652919693,37.6760675899872));
#40961=CARTESIAN_POINT('Ctrl Pts',(21.8912036071185,6.78237160188965,37.7177227250984));
#40962=CARTESIAN_POINT('Ctrl Pts',(21.8978782734341,6.78013523352681,37.7523716958706));
#40963=CARTESIAN_POINT('Ctrl Pts',(21.9165617854201,6.77294564065268,37.8660686897191));
#40964=CARTESIAN_POINT('Ctrl Pts',(21.9246097121476,6.76814177338919,37.9456869201821));
#40965=CARTESIAN_POINT('Ctrl Pts',(21.933671696441,6.75409309085649,38.1804205253587));
#40966=CARTESIAN_POINT('Ctrl Pts',(21.9209726281809,6.74491431598283,38.3353967079668));
#40967=CARTESIAN_POINT('Ctrl Pts',(21.8855412358311,6.73372605163393,38.5083423550071));
#40968=CARTESIAN_POINT('Ctrl Pts',(21.8808505259981,6.73234652151058,38.5294304020046));
#40969=CARTESIAN_POINT('Ctrl Pts',(21.8738547967794,6.73041755936212,38.5585636817234));
#40970=CARTESIAN_POINT('Ctrl Pts',(21.8718499714003,6.72987766646406,38.5666799016223));
#40971=CARTESIAN_POINT('Ctrl Pts',(21.8683053353252,6.72894464390395,38.5806394107818));
#40972=CARTESIAN_POINT('Ctrl Pts',(21.8667906967817,6.72855232306394,38.5864890155315));
#40973=CARTESIAN_POINT('Ctrl Pts',(21.8636032018085,6.72773956886715,38.5985651722654));
#40974=CARTESIAN_POINT('Ctrl Pts',(21.861926565001,6.72731901853094,38.6047906394163));
#40975=CARTESIAN_POINT('Ctrl Pts',(21.857936080698,6.72633399356797,38.6193171844776));
#40976=CARTESIAN_POINT('Ctrl Pts',(21.8555977703904,6.72576873723137,38.6276113422916));
#40977=CARTESIAN_POINT('Ctrl Pts',(21.8478552642206,6.72393462016671,38.6543863489355));
#40978=CARTESIAN_POINT('Ctrl Pts',(21.8422300733944,6.7226586541112,38.6728015473309));
#40979=CARTESIAN_POINT('Ctrl Pts',(21.8119580477984,6.71606588349043,38.7668409999778));
#40980=CARTESIAN_POINT('Ctrl Pts',(21.7829299582975,6.71060777549491,38.8409633722076));
#40981=CARTESIAN_POINT('Ctrl Pts',(21.7037027030375,6.69744168595572,39.0114289246818));
#40982=CARTESIAN_POINT('Ctrl Pts',(21.6497796241485,6.68965383587968,39.1057485432105));
#40983=CARTESIAN_POINT('Ctrl Pts',(21.5411951110403,6.67606128978428,39.2632386874165));
#40984=CARTESIAN_POINT('Ctrl Pts',(21.4898159376284,6.67024053973609,39.3283560046677));
#40985=CARTESIAN_POINT('Ctrl Pts',(21.4281513997816,6.66404252628375,39.3969246399541));
#40986=CARTESIAN_POINT('Ctrl Pts',(21.4218499535432,6.66341755326085,39.4038299968424));
#40987=CARTESIAN_POINT('Ctrl Pts',(21.4124126944714,6.6624943100908,39.4140219040444));
#40988=CARTESIAN_POINT('Ctrl Pts',(21.4093151843065,6.66219328940394,39.4173434996779));
#40989=CARTESIAN_POINT('Ctrl Pts',(21.4037686768452,6.66165788930268,39.4232493090076));
#40990=CARTESIAN_POINT('Ctrl Pts',(21.4013242352707,6.6614231734979,39.4258377050916));
#40991=CARTESIAN_POINT('Ctrl Pts',(21.3960237986257,6.66091691427163,39.431419252269));
#40992=CARTESIAN_POINT('Ctrl Pts',(21.3931653433328,6.66064556403257,39.4344099814424));
#40993=CARTESIAN_POINT('Ctrl Pts',(21.3851645586827,6.65989061743674,39.4427272682827));
#40994=CARTESIAN_POINT('Ctrl Pts',(21.3800010857659,6.65940861419971,39.4480335230369));
#40995=CARTESIAN_POINT('Ctrl Pts',(21.3498491593686,6.65662313134406,39.4786644069264));
#40996=CARTESIAN_POINT('Ctrl Pts',(21.3241926738326,6.65436821456068,39.5033254974281));
#40997=CARTESIAN_POINT('Ctrl Pts',(21.2378457610063,6.64708804678187,39.5818440786651));
#40998=CARTESIAN_POINT('Ctrl Pts',(21.1744363575599,6.64221649046842,39.6325878261729));
#40999=CARTESIAN_POINT('Ctrl Pts',(20.9825460307795,6.62820067217016,39.7672247193048));
#41000=CARTESIAN_POINT('Ctrl Pts',(20.8470495907457,6.61911393828452,39.8399815208395));
#41001=CARTESIAN_POINT('Ctrl Pts',(20.6841635625951,6.6080265344754,39.9038664818191));
#41002=CARTESIAN_POINT('Ctrl Pts',(20.66381679908,6.60663998564747,39.9114528040681));
#41003=CARTESIAN_POINT('Ctrl Pts',(20.6354485273231,6.60470275848451,39.9214878307396));
#41004=CARTESIAN_POINT('Ctrl Pts',(20.6275320908898,6.60416172820722,39.9242303088401));
#41005=CARTESIAN_POINT('Ctrl Pts',(20.6138713285764,6.60322726746436,39.928863340316));
#41006=CARTESIAN_POINT('Ctrl Pts',(20.6081354688641,6.60283465165433,39.9307786255385));
#41007=CARTESIAN_POINT('Ctrl Pts',(20.5962683568232,6.60202178234736,39.934679300877));
#41008=CARTESIAN_POINT('Ctrl Pts',(20.5901359785164,6.60160141406334,39.9366609963707));
#41009=CARTESIAN_POINT('Ctrl Pts',(20.5757966488048,6.60061767737159,39.9412155629398));
#41010=CARTESIAN_POINT('Ctrl Pts',(20.5675822441648,6.60005353335721,39.9437643347397));
#41011=CARTESIAN_POINT('Ctrl Pts',(20.5410123345249,6.59822667774027,39.9518140817853));
#41012=CARTESIAN_POINT('Ctrl Pts',(20.5225923083016,6.59695693911199,39.9570963825587));
#41013=CARTESIAN_POINT('Ctrl Pts',(20.4280209854922,6.59041928603718,39.982698152294));
#41014=CARTESIAN_POINT('Ctrl Pts',(20.3507641302908,6.58501271663675,39.9986089553149));
#41015=CARTESIAN_POINT('Ctrl Pts',(20.1675891288131,6.57205793162762,40.0247708492753));
#41016=CARTESIAN_POINT('Ctrl Pts',(20.0613624672085,6.56443508439255,40.0310776731067));
#41017=CARTESIAN_POINT('Ctrl Pts',(19.8692923521259,6.55077320081843,40.0266126605239));
#41018=CARTESIAN_POINT('Ctrl Pts',(19.7836365842105,6.54472917887144,40.0188828441445));
#41019=CARTESIAN_POINT('Ctrl Pts',(19.6895190004305,6.53832471488099,40.0040041670876));
#41020=CARTESIAN_POINT('Ctrl Pts',(19.6802762960399,6.53769837899685,40.002473937062));
#41021=CARTESIAN_POINT('Ctrl Pts',(19.6665657957742,6.53677351977116,40.0001012739759));
#41022=CARTESIAN_POINT('Ctrl Pts',(19.6620894083864,6.53647223214436,39.999310309833));
#41023=CARTESIAN_POINT('Ctrl Pts',(19.654111800291,6.53593654223697,39.9978715940657));
#41024=CARTESIAN_POINT('Ctrl Pts',(19.6506095459945,6.53570180208498,39.9972299664592));
#41025=CARTESIAN_POINT('Ctrl Pts',(19.6430445554174,6.53519569999051,39.9958223701336));
#41026=CARTESIAN_POINT('Ctrl Pts',(19.6389825078954,6.53492453011686,39.9950530387575));
#41027=CARTESIAN_POINT('Ctrl Pts',(19.6276655914382,6.53417059520872,39.9928719634991));
#41028=CARTESIAN_POINT('Ctrl Pts',(19.6204162199084,6.53368941637665,39.9914315584222));
#41029=CARTESIAN_POINT('Ctrl Pts',(19.5785277529631,6.53091839974047,39.9828580492342));
#41030=CARTESIAN_POINT('Ctrl Pts',(19.5440792115373,6.52867653703816,39.9748146324447));
#41031=CARTESIAN_POINT('Ctrl Pts',(19.4322136963471,6.52146020680714,39.9454288672245));
#41032=CARTESIAN_POINT('Ctrl Pts',(19.3559010866419,6.51663637029006,39.9201999162813));
#41033=CARTESIAN_POINT('Ctrl Pts',(19.1380268531737,6.50259686181839,39.8327450075071));
#41034=CARTESIAN_POINT('Ctrl Pts',(19.0021238529748,6.49344466030962,39.7582038205337));
#41035=CARTESIAN_POINT('Ctrl Pts',(18.8589846658551,6.48228591568714,39.6556652487622));
#41036=CARTESIAN_POINT('Ctrl Pts',(18.8416155327358,6.48090474431667,39.64277533204));
#41037=CARTESIAN_POINT('Ctrl Pts',(18.8178352584306,6.47897384847177,39.6244996042947));
#41038=CARTESIAN_POINT('Ctrl Pts',(18.8112364962756,6.47843368853627,39.6193596836539));
#41039=CARTESIAN_POINT('Ctrl Pts',(18.7999277945118,6.47750032837893,39.6104323169352));
#41040=CARTESIAN_POINT('Ctrl Pts',(18.7952018050785,6.47710793834776,39.6066653213515));
#41041=CARTESIAN_POINT('Ctrl Pts',(18.7856080547246,6.47630657305666,39.5989443248001));
#41042=CARTESIAN_POINT('Ctrl Pts',(18.7807417212316,6.47589753491458,39.5949886734358));
#41043=CARTESIAN_POINT('Ctrl Pts',(18.7695209755349,6.47494839202759,39.5857765430355));
#41044=CARTESIAN_POINT('Ctrl Pts',(18.7631808464915,6.47440760170953,39.580502935978));
#41045=CARTESIAN_POINT('Ctrl Pts',(18.7498597478808,6.47326173017266,39.569277395175));
#41046=CARTESIAN_POINT('Ctrl Pts',(18.7428870491596,6.47265627168856,39.5633160075158));
#41047=CARTESIAN_POINT('Ctrl Pts',(18.7243748144791,6.47103342299823,39.5472587970561));
#41048=CARTESIAN_POINT('Ctrl Pts',(18.7129128676791,6.47001243973116,39.5370749216743));
#41049=CARTESIAN_POINT('Ctrl Pts',(18.6781035098765,6.46686101442338,39.5053964916249));
#41050=CARTESIAN_POINT('Ctrl Pts',(18.655165055665,6.46471261591111,39.4834624698534));
#41051=CARTESIAN_POINT('Ctrl Pts',(18.5674150114258,6.45620484620139,39.3953096311315));
#41052=CARTESIAN_POINT('Ctrl Pts',(18.5068737927178,6.44968275297695,39.3250295020811));
#41053=CARTESIAN_POINT('Ctrl Pts',(18.3713312135895,6.43350636978183,39.1426407143452));
#41054=CARTESIAN_POINT('Ctrl Pts',(18.3025638048707,6.42380144561958,39.0264867065912));
#41055=CARTESIAN_POINT('Ctrl Pts',(18.2405727776872,6.41372738985213,38.8913008498265));
#41056=CARTESIAN_POINT('Ctrl Pts',(18.2348385626528,6.41277972647638,38.8784255353265));
#41057=CARTESIAN_POINT('Ctrl Pts',(18.2270529553291,6.41147163928579,38.860415591817));
#41058=CARTESIAN_POINT('Ctrl Pts',(18.2248819158808,6.41110445253878,38.8553336248158));
#41059=CARTESIAN_POINT('Ctrl Pts',(18.2214288496999,6.41051658635887,38.8471535723329));
#41060=CARTESIAN_POINT('Ctrl Pts',(18.2201330297544,6.4102950887833,38.8440613993401));
#41061=CARTESIAN_POINT('Ctrl Pts',(18.2174363673209,6.40983228791064,38.8375790855304));
#41062=CARTESIAN_POINT('Ctrl Pts',(18.2160371250829,6.40959108637183,38.8341883090793));
#41063=CARTESIAN_POINT('Ctrl Pts',(18.2126569354433,6.40900575680729,38.825930395567));
#41064=CARTESIAN_POINT('Ctrl Pts',(18.2106861675562,6.40866223586658,38.8210590684853));
#41065=CARTESIAN_POINT('Ctrl Pts',(18.2037584896539,6.40744639338624,38.8037319853082));
#41066=CARTESIAN_POINT('Ctrl Pts',(18.1989113963547,6.40658035292994,38.7912323319331));
#41067=CARTESIAN_POINT('Ctrl Pts',(18.1699016773208,6.40129418109856,38.714044720243));
#41068=CARTESIAN_POINT('Ctrl Pts',(18.1490937454587,6.39704547988534,38.6481413778059));
#41069=CARTESIAN_POINT('Ctrl Pts',(18.0914385626056,6.38305589527803,38.4243364055669));
#41070=CARTESIAN_POINT('Ctrl Pts',(18.0709484539361,6.37362273943145,38.2629622546331));
#41071=CARTESIAN_POINT('Ctrl Pts',(18.0708702248395,6.36356089767328,38.1009313909468));
#41072=CARTESIAN_POINT('Ctrl Pts',(18.0708702237818,6.36356076147475,38.1009291976744));
#41073=CARTESIAN_POINT('Ctrl Pts',(18.0708562063867,6.36175358491646,38.0718273444537));
#41074=CARTESIAN_POINT('Ctrl Pts',(18.0715007119562,6.35992981219923,38.0427297870862));
#41075=CARTESIAN_POINT('Ctrl Pts',(18.0736406571234,6.35690143396561,37.9949647470844));
#41076=CARTESIAN_POINT('Ctrl Pts',(18.0747501044797,6.35570839004714,37.976284505585));
#41077=CARTESIAN_POINT('Ctrl Pts',(18.0767324183429,6.35398389679972,37.9494983321484));
#41078=CARTESIAN_POINT('Ctrl Pts',(18.077385212855,6.35345921675814,37.9413767998481));
#41079=CARTESIAN_POINT('Ctrl Pts',(18.0786303395921,6.35252871628467,37.9270250030368));
#41080=CARTESIAN_POINT('Ctrl Pts',(18.0792015807072,6.35212355364348,37.9207929900014));
#41081=CARTESIAN_POINT('Ctrl Pts',(18.0803895083089,6.35132158265804,37.9084919591246));
#41082=CARTESIAN_POINT('Ctrl Pts',(18.0810046784413,6.35092482598635,37.9024228658381));
#41083=CARTESIAN_POINT('Ctrl Pts',(18.0822871368229,6.35013285896987,37.890341900644));
#41084=CARTESIAN_POINT('Ctrl Pts',(18.0829539354062,6.34973766824377,37.8843300460232));
#41085=CARTESIAN_POINT('Ctrl Pts',(18.0846123961175,6.34879259196734,37.8699931002906));
#41086=CARTESIAN_POINT('Ctrl Pts',(18.085630070801,6.34824189900749,37.861671198856));
#41087=CARTESIAN_POINT('Ctrl Pts',(18.0894829000983,6.34625631742746,37.8317835068272));
#41088=CARTESIAN_POINT('Ctrl Pts',(18.0926284098237,6.34481177875687,37.8102600687578));
#41089=CARTESIAN_POINT('Ctrl Pts',(18.1028322013195,6.3405779460009,37.7478361709861));
#41090=CARTESIAN_POINT('Ctrl Pts',(18.110846892159,6.33775966578563,37.7071067325128));
#41091=CARTESIAN_POINT('Ctrl Pts',(18.1485410876324,6.32621569665157,37.5435853421105));
#41092=CARTESIAN_POINT('Ctrl Pts',(18.1889312797888,6.31718958373903,37.423597660045));
#41093=CARTESIAN_POINT('Ctrl Pts',(18.2693947177375,6.30321180285362,37.2447678583331));
#41094=CARTESIAN_POINT('Ctrl Pts',(18.301478403927,6.29825939999035,37.1826982972689));
#41095=CARTESIAN_POINT('Ctrl Pts',(18.3533550519394,6.29118474245683,37.0944340600152));
#41096=CARTESIAN_POINT('Ctrl Pts',(18.3705603682652,6.28896418145649,37.0667869336636));
#41097=CARTESIAN_POINT('Ctrl Pts',(18.3924224547157,6.28630205199639,37.0335624740425));
#41098=CARTESIAN_POINT('Ctrl Pts',(18.3964202646315,6.28582139978791,37.0275604458819));
#41099=CARTESIAN_POINT('Ctrl Pts',(18.4027408403546,6.28507123328818,37.0181855510038));
#41100=CARTESIAN_POINT('Ctrl Pts',(18.4050407976533,6.28480024778613,37.0147974987346));
#41101=CARTESIAN_POINT('Ctrl Pts',(18.4093637939755,6.28429464473436,37.0084727519365));
#41102=CARTESIAN_POINT('Ctrl Pts',(18.4113841657191,6.28405986283447,37.0055343748968));
#41103=CARTESIAN_POINT('Ctrl Pts',(18.4160317686924,6.28352321064337,36.9988150035654));
#41104=CARTESIAN_POINT('Ctrl Pts',(18.4186643929506,6.2832217088112,36.995037804662));
#41105=CARTESIAN_POINT('Ctrl Pts',(18.4256064295058,6.28243304975194,36.985153233965));
#41106=CARTESIAN_POINT('Ctrl Pts',(18.4299379091413,6.28194734219636,36.9790613478903));
#41107=CARTESIAN_POINT('Ctrl Pts',(18.4599380788764,6.2786255817164,36.9373835301914));
#41108=CARTESIAN_POINT('Ctrl Pts',(18.4867812079084,6.27586369073988,36.9026540382753));
#41109=CARTESIAN_POINT('Ctrl Pts',(18.5304810475113,6.27162833310501,36.8499354817733));
#41110=CARTESIAN_POINT('Ctrl Pts',(18.5465353117829,6.27012270054339,36.8313047136528));
#41111=CARTESIAN_POINT('Ctrl Pts',(18.6743530848435,6.2584742901393,36.6885856107018));
#41112=CARTESIAN_POINT('Ctrl Pts',(18.8014415101232,6.24878708483426,36.5791809730441));
#41113=CARTESIAN_POINT('Ctrl Pts',(18.9679201675323,6.2364442271233,36.4698502029863));
#41114=CARTESIAN_POINT('Ctrl Pts',(18.9952419015739,6.23443105596157,36.4528697287211));
#41115=CARTESIAN_POINT('Ctrl Pts',(19.0363226672433,6.23141379058955,36.4287405328961));
#41116=CARTESIAN_POINT('Ctrl Pts',(19.0497646678353,6.23042803453266,36.4210613471948));
#41117=CARTESIAN_POINT('Ctrl Pts',(19.0713699993932,6.2288452218387,36.4090611628361));
#41118=CARTESIAN_POINT('Ctrl Pts',(19.0794746384419,6.22825182802206,36.4046354719387));
#41119=CARTESIAN_POINT('Ctrl Pts',(19.0949518123392,6.22711913397922,36.3963275677258));
#41120=CARTESIAN_POINT('Ctrl Pts',(19.1023183530476,6.22658022474019,36.3924345881853));
#41121=CARTESIAN_POINT('Ctrl Pts',(19.1153132812418,6.22562982141283,36.3856745166606));
#41122=CARTESIAN_POINT('Ctrl Pts',(19.1209310009561,6.22521904542373,36.3827870992462));
#41123=CARTESIAN_POINT('Ctrl Pts',(19.1319534649751,6.22441318341607,36.3771899922128));
#41124=CARTESIAN_POINT('Ctrl Pts',(19.1373569718154,6.22401818289392,36.3744780168223));
#41125=CARTESIAN_POINT('Ctrl Pts',(19.150274093921,6.22307401512768,36.368070858894));
#41126=CARTESIAN_POINT('Ctrl Pts',(19.1577991433123,6.22252404401851,36.364399130405));
#41127=CARTESIAN_POINT('Ctrl Pts',(19.1848963545166,6.22054371190507,36.3513951957271));
#41128=CARTESIAN_POINT('Ctrl Pts',(19.2046010206094,6.21910376725725,36.3423444270437));
#41129=CARTESIAN_POINT('Ctrl Pts',(19.2800002401795,6.21359222191381,36.309239503984));
#41130=CARTESIAN_POINT('Ctrl Pts',(19.3366154081508,6.20944891981682,36.2875072066427));
#41131=CARTESIAN_POINT('Ctrl Pts',(19.3941044301425,6.20523851046618,36.2684888437885));
#41132=CARTESIAN_POINT('Ctrl Pts',(19.3941040087491,6.0347666134114,36.2684889831928));
#41133=CARTESIAN_POINT('Ctrl Pts',(19.3924153457498,6.03488459268239,36.2690476225526));
#41134=CARTESIAN_POINT('Ctrl Pts',(19.3907274462916,6.03500243929733,36.2696086003447));
#41135=CARTESIAN_POINT('Ctrl Pts',(19.3855607656699,6.03536292103602,36.2713336987786));
#41136=CARTESIAN_POINT('Ctrl Pts',(19.3820844874754,6.03560511749658,36.2725054215932));
#41137=CARTESIAN_POINT('Ctrl Pts',(19.3754378577733,6.03606750803258,36.2747668846138));
#41138=CARTESIAN_POINT('Ctrl Pts',(19.3722669887204,6.03628779962772,36.2758549778093));
#41139=CARTESIAN_POINT('Ctrl Pts',(19.3638783399758,6.03686983846296,36.2787580310786));
#41140=CARTESIAN_POINT('Ctrl Pts',(19.3586654439502,6.03723076014707,36.2805871648327));
#41141=CARTESIAN_POINT('Ctrl Pts',(19.3401922360461,6.03850727993246,36.287158420741));
#41142=CARTESIAN_POINT('Ctrl Pts',(19.3269756848599,6.03941598046567,36.2920234581286));
#41143=CARTESIAN_POINT('Ctrl Pts',(19.1882219720687,6.04891937150135,36.3448313980802));
#41144=CARTESIAN_POINT('Ctrl Pts',(19.0679489723965,6.05685666503879,36.4056292305197));
#41145=CARTESIAN_POINT('Ctrl Pts',(18.8769423966935,6.07043508463694,36.5287269355388));
#41146=CARTESIAN_POINT('Ctrl Pts',(18.8026596233994,6.07600554504561,36.5845688921628));
#41147=CARTESIAN_POINT('Ctrl Pts',(18.6963411986952,6.08474835009224,36.6772067979981));
#41148=CARTESIAN_POINT('Ctrl Pts',(18.6611959560312,6.08778210198083,36.7102266764293));
#41149=CARTESIAN_POINT('Ctrl Pts',(18.6188283076276,6.09164743379935,36.7531319330377));
#41150=CARTESIAN_POINT('Ctrl Pts',(18.6104115764933,6.09242614981,36.7618173383008));
#41151=CARTESIAN_POINT('Ctrl Pts',(18.5971360218893,6.09367214953448,36.7757769720279));
#41152=CARTESIAN_POINT('Ctrl Pts',(18.59222388284,6.09413714064111,36.7810002386087));
#41153=CARTESIAN_POINT('Ctrl Pts',(18.5830050565253,6.09501738958114,36.7909131327815));
#41154=CARTESIAN_POINT('Ctrl Pts',(18.5786922345679,6.09543237910192,36.7955969449378));
#41155=CARTESIAN_POINT('Ctrl Pts',(18.5690050657556,6.09637178452624,36.8062224912053));
#41156=CARTESIAN_POINT('Ctrl Pts',(18.5636444142977,6.09689676448525,36.8121764980176));
#41157=CARTESIAN_POINT('Ctrl Pts',(18.5499819690965,6.09824813352873,36.8275426243712));
#41158=CARTESIAN_POINT('Ctrl Pts',(18.5417347582905,6.09907675688633,36.8370025594008));
#41159=CARTESIAN_POINT('Ctrl Pts',(18.4906860455431,6.10428813669584,36.8967244081054));
#41160=CARTESIAN_POINT('Ctrl Pts',(18.4504005192885,6.10877118961416,36.9490697399866));
#41161=CARTESIAN_POINT('Ctrl Pts',(18.3342219547872,6.1229271842419,37.1172117339158));
#41162=CARTESIAN_POINT('Ctrl Pts',(18.2680454643907,6.13289331917305,37.2391775512269));
#41163=CARTESIAN_POINT('Ctrl Pts',(18.1892710269677,6.14759263097347,37.430995708373));
#41164=CARTESIAN_POINT('Ctrl Pts',(18.1664939981097,6.15242742182652,37.4962087044611));
#41165=CARTESIAN_POINT('Ctrl Pts',(18.1435258249744,6.15800376285889,37.5753803112153));
#41166=CARTESIAN_POINT('Ctrl Pts',(18.1399257848916,6.15890394154564,37.5882909817938));
#41167=CARTESIAN_POINT('Ctrl Pts',(18.1351020252303,6.1601468724167,37.6063141609065));
#41168=CARTESIAN_POINT('Ctrl Pts',(18.1337643026059,6.16049577770303,37.6113953669916));
#41169=CARTESIAN_POINT('Ctrl Pts',(18.1315279963284,6.16108624932854,37.6200329361435));
#41170=CARTESIAN_POINT('Ctrl Pts',(18.1306187712523,6.16132841781359,37.6235864891544));
#41171=CARTESIAN_POINT('Ctrl Pts',(18.1288978593356,6.1617908092281,37.6303931674237));
#41172=CARTESIAN_POINT('Ctrl Pts',(18.1280845137114,6.16201112941796,37.633645831344));
#41173=CARTESIAN_POINT('Ctrl Pts',(18.1259529183884,6.16259334946537,37.6422657565937));
#41174=CARTESIAN_POINT('Ctrl Pts',(18.1246492342355,6.16295442280109,37.6476366406582));
#41175=CARTESIAN_POINT('Ctrl Pts',(18.1201022823649,6.16423202907998,37.6667265808073));
#41176=CARTESIAN_POINT('Ctrl Pts',(18.1169862338227,6.16514164902678,37.6804759019064));
#41177=CARTESIAN_POINT('Ctrl Pts',(18.0854605341825,6.17473626197454,37.8270145805573));
#41178=CARTESIAN_POINT('Ctrl Pts',(18.0709925084668,6.18275015076872,37.9624361503233));
#41179=CARTESIAN_POINT('Ctrl Pts',(18.0707504547577,6.19889168787557,38.2325285113259));
#41180=CARTESIAN_POINT('Ctrl Pts',(18.0846447830548,6.20698376711884,38.3664110565059));
#41181=CARTESIAN_POINT('Ctrl Pts',(18.115142026472,6.21642789560342,38.5111449305759));
#41182=CARTESIAN_POINT('Ctrl Pts',(18.1181051737762,6.21730575751372,38.5245015687808));
#41183=CARTESIAN_POINT('Ctrl Pts',(18.1230853481117,6.21872101409651,38.5458724250899));
#41184=CARTESIAN_POINT('Ctrl Pts',(18.1250122754564,6.21925554445668,38.5539073245145));
#41185=CARTESIAN_POINT('Ctrl Pts',(18.1285267788492,6.2202079998532,38.5681577620249));
#41186=CARTESIAN_POINT('Ctrl Pts',(18.1300938611968,6.22062526445002,38.5743782647217));
#41187=CARTESIAN_POINT('Ctrl Pts',(18.1334260860808,6.22149740723373,38.5873323682973));
#41188=CARTESIAN_POINT('Ctrl Pts',(18.1351967051138,6.22195245580394,38.5940644518317));
#41189=CARTESIAN_POINT('Ctrl Pts',(18.1398976831533,6.22313934278524,38.6115527440189));
#41190=CARTESIAN_POINT('Ctrl Pts',(18.1428848803213,6.22387299959467,38.6222932724997));
#41191=CARTESIAN_POINT('Ctrl Pts',(18.1564037328379,6.22710634532274,38.6693178346578));
#41192=CARTESIAN_POINT('Ctrl Pts',(18.1679062844646,6.22963714710759,38.7053117140126));
#41193=CARTESIAN_POINT('Ctrl Pts',(18.2017063989139,6.23654096026965,38.801265298302));
#41194=CARTESIAN_POINT('Ctrl Pts',(18.2259399042036,6.24097229274876,38.8604881714271));
#41195=CARTESIAN_POINT('Ctrl Pts',(18.2843857005264,6.25065853846148,38.9852458457732));
#41196=CARTESIAN_POINT('Ctrl Pts',(18.3195146560722,6.25592788052557,39.0502424464043));
#41197=CARTESIAN_POINT('Ctrl Pts',(18.4155554548618,6.26897584032833,39.2058814744104));
#41198=CARTESIAN_POINT('Ctrl Pts',(18.480607001194,6.27673412013774,39.2936871704458));
#41199=CARTESIAN_POINT('Ctrl Pts',(18.5588089938116,6.28468095471903,39.3824177556844));
#41200=CARTESIAN_POINT('Ctrl Pts',(18.5649275232683,6.28529451259804,39.3892609554051));
#41201=CARTESIAN_POINT('Ctrl Pts',(18.5741235995761,6.28620420562221,39.3993996196901));
#41202=CARTESIAN_POINT('Ctrl Pts',(18.5771641208377,6.28650297740116,39.4027282690302));
#41203=CARTESIAN_POINT('Ctrl Pts',(18.5826248340687,6.28703594744584,39.4086645300142));
#41204=CARTESIAN_POINT('Ctrl Pts',(18.5850405876477,6.28727046961003,39.4112761246983));
#41205=CARTESIAN_POINT('Ctrl Pts',(18.5902976961603,6.28777810565677,39.4169279733381));
#41206=CARTESIAN_POINT('Ctrl Pts',(18.5931416609419,6.28805101677287,39.4199657143436));
#41207=CARTESIAN_POINT('Ctrl Pts',(18.6011491802895,6.28881473758255,39.4284635542596));
#41208=CARTESIAN_POINT('Ctrl Pts',(18.6063349122859,6.2893038935846,39.4339027920374));
#41209=CARTESIAN_POINT('Ctrl Pts',(18.6375738094868,6.29221925231093,39.4662877640944));
#41210=CARTESIAN_POINT('Ctrl Pts',(18.6643779831421,6.29459144546651,39.4925019413635));
#41211=CARTESIAN_POINT('Ctrl Pts',(18.8118854198438,6.30708656797443,39.6285814363745));
#41212=CARTESIAN_POINT('Ctrl Pts',(18.9454059379836,6.31652146295659,39.7235822546358));
#41213=CARTESIAN_POINT('Ctrl Pts',(19.1602762438589,6.33132737354187,39.8386453368161));
#41214=CARTESIAN_POINT('Ctrl Pts',(19.2335471627387,6.33630939637897,39.8721656899719));
#41215=CARTESIAN_POINT('Ctrl Pts',(19.3210007377107,6.34229448586038,39.9057343108539));
#41216=CARTESIAN_POINT('Ctrl Pts',(19.3333578820995,6.34314091934746,39.9103327518375));
#41217=CARTESIAN_POINT('Ctrl Pts',(19.353478882323,6.34452081226978,39.9175863965942));
#41218=CARTESIAN_POINT('Ctrl Pts',(19.3612143839237,6.3450517035695,39.9203194219588));
#41219=CARTESIAN_POINT('Ctrl Pts',(19.3750038410649,6.34599888200213,39.9250926465547));
#41220=CARTESIAN_POINT('Ctrl Pts',(19.3810509771349,6.34641452366576,39.9271522850192));
#41221=CARTESIAN_POINT('Ctrl Pts',(19.3938014044893,6.3472915317714,39.9314244861788));
#41222=CARTESIAN_POINT('Ctrl Pts',(19.4005068201136,6.34775310989018,39.9336303637375));
#41223=CARTESIAN_POINT('Ctrl Pts',(19.4182545319478,6.34897583634393,39.9393610638052));
#41224=CARTESIAN_POINT('Ctrl Pts',(19.4293166143379,6.34973901202268,39.942823208032));
#41225=CARTESIAN_POINT('Ctrl Pts',(19.4809164504446,6.35330431016608,39.9584634588844));
#41226=CARTESIAN_POINT('Ctrl Pts',(19.5218140549906,6.35614598200241,39.9694041526698));
#41227=CARTESIAN_POINT('Ctrl Pts',(19.7257394025522,6.37040474666933,40.0168275346694));
#41228=CARTESIAN_POINT('Ctrl Pts',(19.8926510531193,6.38244064369203,40.0333661841339));
#41229=CARTESIAN_POINT('Ctrl Pts',(20.084132292508,6.39601778788669,40.0274513122304));
#41230=CARTESIAN_POINT('Ctrl Pts',(20.1086859465943,6.39775255875644,40.0262227895227));
#41231=CARTESIAN_POINT('Ctrl Pts',(20.1839352872724,6.40303891500762,40.021014248904));
#41232=CARTESIAN_POINT('Ctrl Pts',(20.234507149808,6.40654984343746,40.0154987229859));
#41233=CARTESIAN_POINT('Ctrl Pts',(20.2925005129333,6.41048567206385,40.0068420287788));
#41234=CARTESIAN_POINT('Ctrl Pts',(20.3001876062294,6.41100551834678,40.0056469974378));
#41235=CARTESIAN_POINT('Ctrl Pts',(20.3124524482004,6.41183175378452,40.0036642551742));
#41236=CARTESIAN_POINT('Ctrl Pts',(20.3170348469129,6.4121397408633,40.0029064705798));
#41237=CARTESIAN_POINT('Ctrl Pts',(20.3251441379302,6.41268345948663,40.0015353430346));
#41238=CARTESIAN_POINT('Ctrl Pts',(20.3286721138405,6.41291956321877,40.0009287239807));
#41239=CARTESIAN_POINT('Ctrl Pts',(20.3361617800509,6.41341983947269,39.9996194362067));
#41240=CARTESIAN_POINT('Ctrl Pts',(20.3401229617851,6.4136838653726,39.9989141940544));
#41241=CARTESIAN_POINT('Ctrl Pts',(20.3508590523441,6.41439800407227,39.9969680863164));
#41242=CARTESIAN_POINT('Ctrl Pts',(20.3576296493254,6.41484679211334,39.995703308153));
#41243=CARTESIAN_POINT('Ctrl Pts',(20.3920031054282,6.41711788613702,39.9890914799765));
#41244=CARTESIAN_POINT('Ctrl Pts',(20.4194951326837,6.41891021558487,39.9831773919318));
#41245=CARTESIAN_POINT('Ctrl Pts',(20.500634210205,6.42415471412786,39.9638574839136));
#41246=CARTESIAN_POINT('Ctrl Pts',(20.5538475661347,6.42753519603736,39.9487436672612));
#41247=CARTESIAN_POINT('Ctrl Pts',(20.7260955463525,6.43849555357931,39.8917144899666));
#41248=CARTESIAN_POINT('Ctrl Pts',(20.8416699216903,6.44589826019209,39.8404160061377));
#41249=CARTESIAN_POINT('Ctrl Pts',(20.9730659132591,6.45510858215605,39.7659246609078));
#41250=CARTESIAN_POINT('Ctrl Pts',(20.9944812377571,6.45663603130124,39.7532299446848));
#41251=CARTESIAN_POINT('Ctrl Pts',(21.0588621673574,6.46131908710018,39.7133621661541));
#41252=CARTESIAN_POINT('Ctrl Pts',(21.1010019702986,6.4645112798347,39.6849039496161));
#41253=CARTESIAN_POINT('Ctrl Pts',(21.152216244641,6.46858039504897,39.6472886020495));
#41254=CARTESIAN_POINT('Ctrl Pts',(21.1623912665049,6.46939854483727,39.6396593205907));
#41255=CARTESIAN_POINT('Ctrl Pts',(21.1783522365477,6.47069778003746,39.6274433089104));
#41256=CARTESIAN_POINT('Ctrl Pts',(21.1841886830538,6.47117627572589,39.6229229185147));
#41257=CARTESIAN_POINT('Ctrl Pts',(21.1949934417558,6.47206852959698,39.6144548516959));
#41258=CARTESIAN_POINT('Ctrl Pts',(21.1999685155384,6.47248193837844,39.6105159329763));
#41259=CARTESIAN_POINT('Ctrl Pts',(21.2109515732944,6.47340035410799,39.6017318053974));
#41260=CARTESIAN_POINT('Ctrl Pts',(21.2169500703856,6.47390582053495,39.596874961873));
#41261=CARTESIAN_POINT('Ctrl Pts',(21.2342373659457,6.47537390118965,39.582705245994));
#41262=CARTESIAN_POINT('Ctrl Pts',(21.2454493413206,6.47634022362391,39.573299915237));
#41263=CARTESIAN_POINT('Ctrl Pts',(21.3350452538048,6.48417929660206,39.4963874547551));
#41264=CARTESIAN_POINT('Ctrl Pts',(21.4079773607664,6.49130657952638,39.4228140938249));
#41265=CARTESIAN_POINT('Ctrl Pts',(21.5691750418778,6.50894102404585,39.2316918563823));
#41266=CARTESIAN_POINT('Ctrl Pts',(21.6506117544955,6.51958108201855,39.1092161832616));
#41267=CARTESIAN_POINT('Ctrl Pts',(21.7316093264231,6.53186055955177,38.9509090444608));
#41268=CARTESIAN_POINT('Ctrl Pts',(21.7451527554998,6.5339891562698,38.9227753002168));
#41269=CARTESIAN_POINT('Ctrl Pts',(21.7610493532698,6.53657473306921,38.887592713206));
#41270=CARTESIAN_POINT('Ctrl Pts',(21.764051843853,6.53706723884324,38.8808445447603));
#41271=CARTESIAN_POINT('Ctrl Pts',(21.7686919029858,6.53783475536267,38.870252531614));
#41272=CARTESIAN_POINT('Ctrl Pts',(21.7703558274569,6.53811131081077,38.8664204167139));
#41273=CARTESIAN_POINT('Ctrl Pts',(21.7734130145284,6.53862186502006,38.8593164573071));
#41274=CARTESIAN_POINT('Ctrl Pts',(21.7748096683001,6.53885606130442,38.8560461917807));
#41275=CARTESIAN_POINT('Ctrl Pts',(21.7779479273725,6.53938448183763,38.8486413370029));
#41276=CARTESIAN_POINT('Ctrl Pts',(21.7796841538721,6.53967838069398,38.84450453147));
#41277=CARTESIAN_POINT('Ctrl Pts',(21.784886732932,6.5405638858627,38.8319864529696));
#41278=CARTESIAN_POINT('Ctrl Pts',(21.7883084868077,6.54115288848041,38.8235866088795));
#41279=CARTESIAN_POINT('Ctrl Pts',(21.8282370117301,6.54810932172744,38.7235551423908));
#41280=CARTESIAN_POINT('Ctrl Pts',(21.8577290836442,6.554095747652,38.6292636440085));
#41281=CARTESIAN_POINT('Ctrl Pts',(21.9182577004232,6.57026759237785,38.366548313251));
#41282=CARTESIAN_POINT('Ctrl Pts',(21.9343237842355,6.58031252440966,38.1956380298044));
#41283=CARTESIAN_POINT('Ctrl Pts',(21.9268808664875,6.59243998359089,38.0047181805862));
#41284=CARTESIAN_POINT('Ctrl Pts',(21.9257806745749,6.59372798174598,37.984599637778));
#41285=CARTESIAN_POINT('Ctrl Pts',(21.9237961428244,6.59554796944844,37.9564148556313));
#41286=CARTESIAN_POINT('Ctrl Pts',(21.9231756988274,6.59607177819576,37.9483308832298));
#41287=CARTESIAN_POINT('Ctrl Pts',(21.9220093075626,6.59698454629142,37.9342938969484));
#41288=CARTESIAN_POINT('Ctrl Pts',(21.9214866114551,6.597372778139,37.9283390212939));
#41289=CARTESIAN_POINT('Ctrl Pts',(21.9203386528133,6.59818436631446,37.9159235338434));
#41290=CARTESIAN_POINT('Ctrl Pts',(21.9197084451105,6.59860787199287,37.9094634656307));
#41291=CARTESIAN_POINT('Ctrl Pts',(21.9181393054785,6.59961292899109,37.894177404606));
#41292=CARTESIAN_POINT('Ctrl Pts',(21.9171720459524,6.60019535717728,37.8853545300361));
#41293=CARTESIAN_POINT('Ctrl Pts',(21.9137434073348,6.60214409576965,37.8559545081229));
#41294=CARTESIAN_POINT('Ctrl Pts',(21.9110114139541,6.60351880772404,37.8354109784664));
#41295=CARTESIAN_POINT('Ctrl Pts',(21.8944252373989,6.61102023562796,37.7244065303495));
#41296=CARTESIAN_POINT('Ctrl Pts',(21.8744802719041,6.61733593801558,37.6349873096741));
#41297=CARTESIAN_POINT('Ctrl Pts',(21.8290520563024,6.62850910535385,37.4830633363604));
#41298=CARTESIAN_POINT('Ctrl Pts',(21.8064962470292,6.63329635554364,37.4198434506485));
#41299=CARTESIAN_POINT('Ctrl Pts',(21.7382113517549,6.64596207811006,37.2559849758262));
#41300=CARTESIAN_POINT('Ctrl Pts',(21.6870465986893,6.65382287075045,37.1578642603265));
#41301=CARTESIAN_POINT('Ctrl Pts',(21.6228529276574,6.66185894270065,37.0569398439116));
#41302=CARTESIAN_POINT('Ctrl Pts',(21.6178921769758,6.66246990713955,37.0492616758687));
#41303=CARTESIAN_POINT('Ctrl Pts',(21.610407764078,6.66337651834278,37.0378561088854));
#41304=CARTESIAN_POINT('Ctrl Pts',(21.6079254190054,6.66367477616622,37.034101946727));
#41305=CARTESIAN_POINT('Ctrl Pts',(21.6034576768009,6.66420719412797,37.0273963043614));
#41306=CARTESIAN_POINT('Ctrl Pts',(21.6014772412968,6.66444167530487,37.0244416075902));
#41307=CARTESIAN_POINT('Ctrl Pts',(21.597159029628,6.66494964071831,37.0180374525871));
#41308=CARTESIAN_POINT('Ctrl Pts',(21.5948182518101,6.66522291994315,37.014590093821));
#41309=CARTESIAN_POINT('Ctrl Pts',(21.5882098491243,6.66598871408783,37.0049251615507));
#41310=CARTESIAN_POINT('Ctrl Pts',(21.5839168519323,6.66647956085422,36.998724903855));
#41311=CARTESIAN_POINT('Ctrl Pts',(21.5578019877073,6.66942681066192,36.9614765330277));
#41312=CARTESIAN_POINT('Ctrl Pts',(21.5351025064472,6.67182781979418,36.9310502671716));
#41313=CARTESIAN_POINT('Ctrl Pts',(21.4068722995287,6.68467074625443,36.7693549997406));
#41314=CARTESIAN_POINT('Ctrl Pts',(21.2853906179317,6.69438597509941,36.6516602986869));
#41315=CARTESIAN_POINT('Ctrl Pts',(21.0898457991599,6.70922243218139,36.5064436146901));
#41316=CARTESIAN_POINT('Ctrl Pts',(21.026977675166,6.71388326505895,36.4652215265284));
#41317=CARTESIAN_POINT('Ctrl Pts',(20.9505947929873,6.71951462871796,36.421285808312));
#41318=CARTESIAN_POINT('Ctrl Pts',(20.9392528776285,6.72034993335725,36.4149137065468));
#41319=CARTESIAN_POINT('Ctrl Pts',(20.9207011621815,6.72171522934197,36.4047364900179));
#41320=CARTESIAN_POINT('Ctrl Pts',(20.9135300398068,6.72224274214559,36.4008614355108));
#41321=CARTESIAN_POINT('Ctrl Pts',(20.9007008892524,6.72318614104143,36.394033647902));
#41322=CARTESIAN_POINT('Ctrl Pts',(20.8950523276208,6.72360140062074,36.3910633084924));
#41323=CARTESIAN_POINT('Ctrl Pts',(20.8830996229841,6.72447993502907,36.3848534030222));
#41324=CARTESIAN_POINT('Ctrl Pts',(20.8767921698609,6.72494343330415,36.3816204488361));
#41325=CARTESIAN_POINT('Ctrl Pts',(20.8600067989423,6.72617669585088,36.3731334000601));
#41326=CARTESIAN_POINT('Ctrl Pts',(20.8494986980836,6.72694855056616,36.3679399837416));
#41327=CARTESIAN_POINT('Ctrl Pts',(20.7995298994961,6.7306185211545,36.3438080121611));
#41328=CARTESIAN_POINT('Ctrl Pts',(20.7594822495647,6.73355907401936,36.3261216090152));
#41329=CARTESIAN_POINT('Ctrl Pts',(20.5649423056006,6.7478520140779,36.2480018109363));
#41330=CARTESIAN_POINT('Ctrl Pts',(20.4037004351795,6.75980643622934,36.2063089830673));
#41331=CARTESIAN_POINT('Ctrl Pts',(20.2097082455715,6.77365943589982,36.1820725319764));
#41332=CARTESIAN_POINT('Ctrl Pts',(20.1801774725054,6.77575146542181,36.1790732646532));
#41333=CARTESIAN_POINT('Ctrl Pts',(20.105119644705,6.78101002760199,36.1731963022452));
#41334=CARTESIAN_POINT('Ctrl Pts',(20.0595346626624,6.78414930483095,36.1712493620381));
#41335=CARTESIAN_POINT('Ctrl Pts',(20.0063538130482,6.78771748109636,36.1708656267592));
#41336=CARTESIAN_POINT('Ctrl Pts',(19.9987876208153,6.78822290733504,36.1708555430706));
#41337=CARTESIAN_POINT('Ctrl Pts',(19.9866394294548,6.78903062921709,36.1709108244885));
#41338=CARTESIAN_POINT('Ctrl Pts',(19.9820574745272,6.78933441461749,36.1709479999817));
#41339=CARTESIAN_POINT('Ctrl Pts',(19.973904007766,6.78987340278675,36.1710432056767));
#41340=CARTESIAN_POINT('Ctrl Pts',(19.9703324782879,6.79010895503195,36.1710948301874));
#41341=CARTESIAN_POINT('Ctrl Pts',(19.9627011060732,6.7906110873571,36.1712263385148));
#41342=CARTESIAN_POINT('Ctrl Pts',(19.9586413729366,6.79087750527097,36.1713091202974));
#41343=CARTESIAN_POINT('Ctrl Pts',(19.9475285786086,6.79160491737153,36.1715708248523));
#41344=CARTESIAN_POINT('Ctrl Pts',(19.940476103195,6.7920645018859,36.1717756242876));
#41345=CARTESIAN_POINT('Ctrl Pts',(19.9031192317641,6.7944888001296,36.1730655966357));
#41346=CARTESIAN_POINT('Ctrl Pts',(19.8728404986087,6.79641849654678,36.1748265562644));
#41347=CARTESIAN_POINT('Ctrl Pts',(19.6900069828533,6.80792484381989,36.1897927338462));
#41348=CARTESIAN_POINT('Ctrl Pts',(19.5394462013061,6.81682141895203,36.2204072326804));
#41349=CARTESIAN_POINT('Ctrl Pts',(19.3941039843085,6.82605087843334,36.2684889912782));
#41350=CARTESIAN_POINT('Origin',(20.,-1.3495818343519,38.1));
#41351=CARTESIAN_POINT('',(19.3941040087786,7.78970911166913,36.2684889831831));
#41352=CARTESIAN_POINT('',(19.3941039249488,7.61899517246903,36.2684890109154));
#41353=CARTESIAN_POINT('',(19.3941040087494,-1.3495818343519,36.2684889831927));
#41354=CARTESIAN_POINT('Ctrl Pts',(19.3941040087786,7.78970911166913,36.2684889831831));
#41355=CARTESIAN_POINT('Ctrl Pts',(19.4230126969859,7.78774471398743,36.258925481716));
#41356=CARTESIAN_POINT('Ctrl Pts',(19.4521461268376,7.78581628133123,36.2500469832411));
#41357=CARTESIAN_POINT('Ctrl Pts',(19.6276793992675,7.77443388166182,36.2010638067059));
#41358=CARTESIAN_POINT('Ctrl Pts',(19.778196168021,7.76561309781924,36.1776592354544));
#41359=CARTESIAN_POINT('Ctrl Pts',(19.993800511059,7.75259056793529,36.1698209562425));
#41360=CARTESIAN_POINT('Ctrl Pts',(20.0577593062877,7.7486852247433,36.1706756581785));
#41361=CARTESIAN_POINT('Ctrl Pts',(20.1465170279916,7.74312723625945,36.176279399263));
#41362=CARTESIAN_POINT('Ctrl Pts',(20.1714460431282,7.74155115483903,36.178340728086));
#41363=CARTESIAN_POINT('Ctrl Pts',(20.2147597009781,7.73878222709422,36.1827717548401));
#41364=CARTESIAN_POINT('Ctrl Pts',(20.2331636391685,7.73759608322611,36.1849228337826));
#41365=CARTESIAN_POINT('Ctrl Pts',(20.2600533771323,7.7358477247745,36.1884590911738));
#41366=CARTESIAN_POINT('Ctrl Pts',(20.2685658146254,7.73529199963571,36.1896364732427));
#41367=CARTESIAN_POINT('Ctrl Pts',(20.2834466841576,7.73431645791239,36.1917961186455));
#41368=CARTESIAN_POINT('Ctrl Pts',(20.2898186365916,7.73389742750038,36.192753494751));
#41369=CARTESIAN_POINT('Ctrl Pts',(20.3021631373224,7.73308304861369,36.1946715273263));
#41370=CARTESIAN_POINT('Ctrl Pts',(20.3081362057648,7.7326878239966,36.1956283903512));
#41371=CARTESIAN_POINT('Ctrl Pts',(20.3223785646891,7.73174258593293,36.1979787224022));
#41372=CARTESIAN_POINT('Ctrl Pts',(20.3306434076751,7.73119176444531,36.1993980394044));
#41373=CARTESIAN_POINT('Ctrl Pts',(20.3603236649083,7.72920524485176,36.2046944670424));
#41374=CARTESIAN_POINT('Ctrl Pts',(20.3816816932292,7.72775988479655,36.2088799016885));
#41375=CARTESIAN_POINT('Ctrl Pts',(20.551998112266,7.71610235860834,36.245258706986));
#41376=CARTESIAN_POINT('Ctrl Pts',(20.6967076181939,7.70532324178521,36.2946335874514));
#41377=CARTESIAN_POINT('Ctrl Pts',(20.9078023955057,7.68861802501816,36.3958510862184));
#41378=CARTESIAN_POINT('Ctrl Pts',(20.979216010006,7.68278709749047,36.43585866317));
#41379=CARTESIAN_POINT('Ctrl Pts',(21.0778848972642,7.67464421960516,36.4996925540394));
#41380=CARTESIAN_POINT('Ctrl Pts',(21.1073482681718,7.67220138205543,36.5199367143199));
#41381=CARTESIAN_POINT('Ctrl Pts',(21.1422253643214,7.66931145066091,36.5453557538087));
#41382=CARTESIAN_POINT('Ctrl Pts',(21.1481913287944,7.66881717619672,36.5497567313529));
#41383=CARTESIAN_POINT('Ctrl Pts',(21.1574485520769,7.66805051947128,36.5566683640855));
#41384=CARTESIAN_POINT('Ctrl Pts',(21.1607572718816,7.66777656013919,36.5591553466708));
#41385=CARTESIAN_POINT('Ctrl Pts',(21.1668968388472,7.66726835928274,36.5638011203408));
#41386=CARTESIAN_POINT('Ctrl Pts',(21.1697296882758,7.66703393558903,36.565957077828));
#41387=CARTESIAN_POINT('Ctrl Pts',(21.1761607081506,7.66650188554795,36.5708796171302));
#41388=CARTESIAN_POINT('Ctrl Pts',(21.1797550877829,7.66620460378654,36.573651058704));
#41389=CARTESIAN_POINT('Ctrl Pts',(21.1907105251123,7.66529866200773,36.5821600527802));
#41390=CARTESIAN_POINT('Ctrl Pts',(21.1980398904273,7.66469278567903,36.5879384637449));
#41391=CARTESIAN_POINT('Ctrl Pts',(21.2686271188624,7.65885664728795,36.6444243296691));
#41392=CARTESIAN_POINT('Ctrl Pts',(21.328679728693,7.65388148180971,36.69902570664));
#41393=CARTESIAN_POINT('Ctrl Pts',(21.4991950218246,7.63909506227624,36.8749222947905));
#41394=CARTESIAN_POINT('Ctrl Pts',(21.5978002372821,7.62953592665228,37.0066406178803));
#41395=CARTESIAN_POINT('Ctrl Pts',(21.6979262792275,7.61685468145044,37.1834131199225));
#41396=CARTESIAN_POINT('Ctrl Pts',(21.7162338915729,7.61437157300214,37.2181689227193));
#41397=CARTESIAN_POINT('Ctrl Pts',(21.7384256352827,7.61112611704723,37.2636110058272));
#41398=CARTESIAN_POINT('Ctrl Pts',(21.7432947640213,7.61039796083964,37.2738077730408));
#41399=CARTESIAN_POINT('Ctrl Pts',(21.7510323788957,7.60921408339267,37.2903846047971));
#41400=CARTESIAN_POINT('Ctrl Pts',(21.7539562839535,7.60876026708288,37.2967386278816));
#41401=CARTESIAN_POINT('Ctrl Pts',(21.7594912811617,7.60788861732658,37.308941209074));
#41402=CARTESIAN_POINT('Ctrl Pts',(21.762107932661,7.60747098043067,37.3147871554894));
#41403=CARTESIAN_POINT('Ctrl Pts',(21.7680054797587,7.60651680382135,37.3281410020875));
#41404=CARTESIAN_POINT('Ctrl Pts',(21.7712677350643,7.60597964080494,37.335656951136));
#41405=CARTESIAN_POINT('Ctrl Pts',(21.7797567241083,7.60455665716292,37.355561054979));
#41406=CARTESIAN_POINT('Ctrl Pts',(21.7849019178352,7.60366811498294,37.3679832870108));
#41407=CARTESIAN_POINT('Ctrl Pts',(21.8232800470759,7.59683475678498,37.4634518742567));
#41408=CARTESIAN_POINT('Ctrl Pts',(21.850825779465,7.59070178190031,37.5486531220211));
#41409=CARTESIAN_POINT('Ctrl Pts',(21.9113620256374,7.57306914979581,37.7926417097495));
#41410=CARTESIAN_POINT('Ctrl Pts',(21.93041106278,7.56127227350689,37.954110541793));
#41411=CARTESIAN_POINT('Ctrl Pts',(21.9288120879362,7.54802517561317,38.1462245611227));
#41412=CARTESIAN_POINT('Ctrl Pts',(21.9278532836705,7.54597075764192,38.1763855181439));
#41413=CARTESIAN_POINT('Ctrl Pts',(21.9257983507026,7.54348046433386,38.2135468536062));
#41414=CARTESIAN_POINT('Ctrl Pts',(21.925370899014,7.54301109256027,38.2205781097167));
#41415=CARTESIAN_POINT('Ctrl Pts',(21.9246365057137,7.54227460081027,38.2316561641678));
#41416=CARTESIAN_POINT('Ctrl Pts',(21.924355297013,7.54200609495356,38.2357045183563));
#41417=CARTESIAN_POINT('Ctrl Pts',(21.9238025165188,7.54150256630001,38.243315025211));
#41418=CARTESIAN_POINT('Ctrl Pts',(21.9235338278765,7.54126739423347,38.2468772694404));
#41419=CARTESIAN_POINT('Ctrl Pts',(21.9228976054047,7.54073157685276,38.2550109285403));
#41420=CARTESIAN_POINT('Ctrl Pts',(21.9225236649204,7.54043129075335,38.2595817900932));
#41421=CARTESIAN_POINT('Ctrl Pts',(21.9214884661334,7.53963703787592,38.2717034716854));
#41422=CARTESIAN_POINT('Ctrl Pts',(21.9207989927734,7.53914459266156,38.2792518942869));
#41423=CARTESIAN_POINT('Ctrl Pts',(21.9156354300128,7.53569593464765,38.3323277917265));
#41424=CARTESIAN_POINT('Ctrl Pts',(21.9095872325823,7.53282036885576,38.3776916909528));
#41425=CARTESIAN_POINT('Ctrl Pts',(21.8969598457538,7.52816053162149,38.4520916390105));
#41426=CARTESIAN_POINT('Ctrl Pts',(21.891312511511,7.52634787714815,38.4812640697539));
#41427=CARTESIAN_POINT('Ctrl Pts',(21.8496300210549,7.51447880651155,38.6727632104032));
#41428=CARTESIAN_POINT('Ctrl Pts',(21.7934138616941,7.50480974887611,38.8299701959233));
#41429=CARTESIAN_POINT('Ctrl Pts',(21.6980519299293,7.49177164635131,39.0165329025731));
#41430=CARTESIAN_POINT('Ctrl Pts',(21.6770801214077,7.48904318534393,39.0543661448218));
#41431=CARTESIAN_POINT('Ctrl Pts',(21.6488557882827,7.48552071744568,39.1014756354968));
#41432=CARTESIAN_POINT('Ctrl Pts',(21.6427649132515,7.48476868932577,39.1114357562944));
#41433=CARTESIAN_POINT('Ctrl Pts',(21.6328370844093,7.48355548590444,39.1273440043834));
#41434=CARTESIAN_POINT('Ctrl Pts',(21.6290570830942,7.48309639493977,39.1333274724774));
#41435=CARTESIAN_POINT('Ctrl Pts',(21.6218049030694,7.48222087314776,39.1446684502722));
#41436=CARTESIAN_POINT('Ctrl Pts',(21.6183388804184,7.48180467344617,39.1500298001021));
#41437=CARTESIAN_POINT('Ctrl Pts',(21.6103768379123,7.48085359794733,39.1622126639468));
#41438=CARTESIAN_POINT('Ctrl Pts',(21.6058639924296,7.48031810175956,39.1690229828651));
#41439=CARTESIAN_POINT('Ctrl Pts',(21.5940187761205,7.47892161695727,39.1866542935384));
#41440=CARTESIAN_POINT('Ctrl Pts',(21.586619541847,7.4780581357376,39.1974296458053));
#41441=CARTESIAN_POINT('Ctrl Pts',(21.5350728529737,7.47210153402634,39.2708849824906));
#41442=CARTESIAN_POINT('Ctrl Pts',(21.4873381480004,7.46687179953347,39.3309520066939));
#41443=CARTESIAN_POINT('Ctrl Pts',(21.3247116535933,7.44989620428154,39.5122839007502));
#41444=CARTESIAN_POINT('Ctrl Pts',(21.1976178620949,7.43773581989172,39.6215487755451));
#41445=CARTESIAN_POINT('Ctrl Pts',(21.0264369449429,7.42352657459739,39.7338297968724));
#41446=CARTESIAN_POINT('Ctrl Pts',(20.9942104714587,7.42093818392172,39.7536379934182));
#41447=CARTESIAN_POINT('Ctrl Pts',(20.9548884581443,7.41790026069237,39.7762420311942));
#41448=CARTESIAN_POINT('Ctrl Pts',(20.9483348721752,7.41739786522942,39.7799584189666));
#41449=CARTESIAN_POINT('Ctrl Pts',(20.9381243182724,7.41662139101009,39.7856697986326));
#41450=CARTESIAN_POINT('Ctrl Pts',(20.9344824664119,7.41634567060427,39.7876914490923));
#41451=CARTESIAN_POINT('Ctrl Pts',(20.9277183437048,7.41583588100278,39.7914177146214));
#41452=CARTESIAN_POINT('Ctrl Pts',(20.9245979323305,7.41560161920572,39.7931254751081));
#41453=CARTESIAN_POINT('Ctrl Pts',(20.9175168784157,7.41507206632435,39.7969754298185));
#41454=CARTESIAN_POINT('Ctrl Pts',(20.9135534560911,7.41477710665685,39.7991123904749));
#41455=CARTESIAN_POINT('Ctrl Pts',(20.9015118714846,7.41388522189775,39.8055505439311));
#41456=CARTESIAN_POINT('Ctrl Pts',(20.8934104074271,7.41329095603541,39.8098082244071));
#41457=CARTESIAN_POINT('Ctrl Pts',(20.7875959009987,7.40560014134168,39.8644610173593));
#41458=CARTESIAN_POINT('Ctrl Pts',(20.6857626506532,7.39897702969677,39.9064791998961));
#41459=CARTESIAN_POINT('Ctrl Pts',(20.5004882688963,7.38735285650232,39.9649833880569));
#41460=CARTESIAN_POINT('Ctrl Pts',(20.4185096237902,7.38234690261566,39.9850731475136));
#41461=CARTESIAN_POINT('Ctrl Pts',(20.2593509724105,7.37254537929997,40.0131796453236));
#41462=CARTESIAN_POINT('Ctrl Pts',(20.1824884283243,7.3677761810364,40.0220341285599));
#41463=CARTESIAN_POINT('Ctrl Pts',(20.0863681876826,7.36165585469403,40.0272889954938));
#41464=CARTESIAN_POINT('Ctrl Pts',(20.0674149459046,7.36044174228542,40.0280449995559));
#41465=CARTESIAN_POINT('Ctrl Pts',(20.0398913045798,7.3586667876857,40.0287365319039));
#41466=CARTESIAN_POINT('Ctrl Pts',(20.0313272267653,7.35811284442608,40.0288946385582));
#41467=CARTESIAN_POINT('Ctrl Pts',(20.0163238336893,7.35713936671488,40.0290716812621));
#41468=CARTESIAN_POINT('Ctrl Pts',(20.0098849012368,7.35672060823672,40.0291154206134));
#41469=CARTESIAN_POINT('Ctrl Pts',(19.9973887161276,7.35590597034463,40.0291377421304));
#41470=CARTESIAN_POINT('Ctrl Pts',(19.9913315388288,7.35551021109596,40.0291200334071));
#41471=CARTESIAN_POINT('Ctrl Pts',(19.9768585878334,7.35456242449169,40.0290095555435));
#41472=CARTESIAN_POINT('Ctrl Pts',(19.9684431981106,7.35400957913339,40.0288902391794));
#41473=CARTESIAN_POINT('Ctrl Pts',(19.9380761385364,7.35200815222015,40.0282609071548));
#41474=CARTESIAN_POINT('Ctrl Pts',(19.9161334800788,7.35054971827324,40.0274311998574));
#41475=CARTESIAN_POINT('Ctrl Pts',(19.7456109979168,7.3391161381636,40.0180660080172));
#41476=CARTESIAN_POINT('Ctrl Pts',(19.5984827814038,7.32860336248275,39.9927382953995));
#41477=CARTESIAN_POINT('Ctrl Pts',(19.3460420923254,7.30982728066361,39.9185049272692));
#41478=CARTESIAN_POINT('Ctrl Pts',(19.2393999249786,7.30166031560354,39.8765456286366));
#41479=CARTESIAN_POINT('Ctrl Pts',(19.1267825489578,7.29316669671472,39.8202228854585));
#41480=CARTESIAN_POINT('Ctrl Pts',(19.1165166563092,7.29239384012503,39.814973087192));
#41481=CARTESIAN_POINT('Ctrl Pts',(19.1019149817705,7.29129722365943,39.807340129858));
#41482=CARTESIAN_POINT('Ctrl Pts',(19.0975405844668,7.29096904076219,39.8050319714454));
#41483=CARTESIAN_POINT('Ctrl Pts',(19.0899867307905,7.29040298210571,39.8010089522017));
#41484=CARTESIAN_POINT('Ctrl Pts',(19.0868031436998,7.29016461995074,39.7993019473119));
#41485=CARTESIAN_POINT('Ctrl Pts',(19.0801769267375,7.28966894987765,39.795725042058));
#41486=CARTESIAN_POINT('Ctrl Pts',(19.0767351891742,7.28941174175044,39.7938535928878));
#41487=CARTESIAN_POINT('Ctrl Pts',(19.0676755382886,7.28873528887928,39.7888915793258));
#41488=CARTESIAN_POINT('Ctrl Pts',(19.0620672317395,7.28831713989765,39.7857834361775));
#41489=CARTESIAN_POINT('Ctrl Pts',(19.0386555577091,7.28657368165367,39.7726556032465));
#41490=CARTESIAN_POINT('Ctrl Pts',(19.0209956565235,7.28526363540196,39.7623809672485));
#41491=CARTESIAN_POINT('Ctrl Pts',(18.8495753242944,7.27256392490519,39.6589681490693));
#41492=CARTESIAN_POINT('Ctrl Pts',(18.7093634829027,7.26223916762675,39.5450382152355));
#41493=CARTESIAN_POINT('Ctrl Pts',(18.5348842806202,7.24668935585623,39.3573091193895));
#41494=CARTESIAN_POINT('Ctrl Pts',(18.4862063126742,7.24196969904699,39.2982557971383));
#41495=CARTESIAN_POINT('Ctrl Pts',(18.4300544974328,7.2359089241463,39.2212356234614));
#41496=CARTESIAN_POINT('Ctrl Pts',(18.4191690306801,7.23470170576816,39.2058352547844));
#41497=CARTESIAN_POINT('Ctrl Pts',(18.4036816765768,7.23293500594798,39.1832282286636));
#41498=CARTESIAN_POINT('Ctrl Pts',(18.3988989299972,7.23238233227348,39.1761463398843));
#41499=CARTESIAN_POINT('Ctrl Pts',(18.390596921988,7.2314103227781,39.163675566912));
#41500=CARTESIAN_POINT('Ctrl Pts',(18.3870572560425,7.23099175567487,39.1583003742815));
#41501=CARTESIAN_POINT('Ctrl Pts',(18.3802354280521,7.23017692355542,39.1478272990366));
#41502=CARTESIAN_POINT('Ctrl Pts',(18.3769502672998,7.2297807760512,39.1427314519655));
#41503=CARTESIAN_POINT('Ctrl Pts',(18.3691505209555,7.2288311428582,39.1305065444558));
#41504=CARTESIAN_POINT('Ctrl Pts',(18.3646586127115,7.22827683193276,39.1233632320293));
#41505=CARTESIAN_POINT('Ctrl Pts',(18.3485719635192,7.22626443299498,39.0974048525123));
#41506=CARTESIAN_POINT('Ctrl Pts',(18.3372542684254,7.22479635076791,39.078420953867));
#41507=CARTESIAN_POINT('Ctrl Pts',(18.2538315067474,7.21356262649922,38.9328614891025));
#41508=CARTESIAN_POINT('Ctrl Pts',(18.1959591830902,7.20328439919121,38.7987014536748));
#41509=CARTESIAN_POINT('Ctrl Pts',(18.128606725356,7.18670973272714,38.5763850893056));
#41510=CARTESIAN_POINT('Ctrl Pts',(18.1090930374798,7.1805169530177,38.4918266803268));
#41511=CARTESIAN_POINT('Ctrl Pts',(18.089468470469,7.17194250095033,38.3697704880633));
#41512=CARTESIAN_POINT('Ctrl Pts',(18.0846531340135,7.16941577907992,38.3331387204966));
#41513=CARTESIAN_POINT('Ctrl Pts',(18.0801304978588,7.16644044969123,38.2889435349048));
#41514=CARTESIAN_POINT('Ctrl Pts',(18.0794119457004,7.16594142321738,38.2814940627911));
#41515=CARTESIAN_POINT('Ctrl Pts',(18.0783619472562,7.16516902052696,38.269902944553));
#41516=CARTESIAN_POINT('Ctrl Pts',(18.0780005072943,7.1648940295849,38.2657641914529));
#41517=CARTESIAN_POINT('Ctrl Pts',(18.0773543193479,7.16438490233174,38.2580784772877));
#41518=CARTESIAN_POINT('Ctrl Pts',(18.0770660172333,7.16415057773019,38.2545319273491));
#41519=CARTESIAN_POINT('Ctrl Pts',(18.0764339646257,7.1636200097953,38.2464809591786));
#41520=CARTESIAN_POINT('Ctrl Pts',(18.0760962226889,7.16332410325244,38.2419761265905));
#41521=CARTESIAN_POINT('Ctrl Pts',(18.0752621293534,7.16255961258323,38.230300977487));
#41522=CARTESIAN_POINT('Ctrl Pts',(18.0747900144612,7.16209233758744,38.2231289199796));
#41523=CARTESIAN_POINT('Ctrl Pts',(18.0720535910561,7.15914553965016,38.1776853798842));
#41524=CARTESIAN_POINT('Ctrl Pts',(18.0708903152333,7.15672246204862,38.1393531677313));
#41525=CARTESIAN_POINT('Ctrl Pts',(18.0707754377414,7.1430649112224,37.9196737203836));
#41526=CARTESIAN_POINT('Ctrl Pts',(18.0962469105642,7.1326570053055,37.7392203046852));
#41527=CARTESIAN_POINT('Ctrl Pts',(18.1638473325454,7.11769897865133,37.5050411594644));
#41528=CARTESIAN_POINT('Ctrl Pts',(18.1840397598923,7.11380488429277,37.445997082769));
#41529=CARTESIAN_POINT('Ctrl Pts',(18.2116104883321,7.10902623318341,37.3765652001304));
#41530=CARTESIAN_POINT('Ctrl Pts',(18.2162764396768,7.1082330330214,37.3651359281783));
#41531=CARTESIAN_POINT('Ctrl Pts',(18.2241265677736,7.10692306561753,37.3464223365102));
#41532=CARTESIAN_POINT('Ctrl Pts',(18.2272466940099,7.10640845094331,37.3391114042222));
#41533=CARTESIAN_POINT('Ctrl Pts',(18.2329449077133,7.10547925514718,37.325984933877));
#41534=CARTESIAN_POINT('Ctrl Pts',(18.23550675901,7.10506522834411,37.3201624382943));
#41535=CARTESIAN_POINT('Ctrl Pts',(18.2410339823489,7.10417977470255,37.3077670154533));
#41536=CARTESIAN_POINT('Ctrl Pts',(18.2440074969725,7.10370807562761,37.3011978467766));
#41537=CARTESIAN_POINT('Ctrl Pts',(18.2521436981349,7.10242973736881,37.2834881081571));
#41538=CARTESIAN_POINT('Ctrl Pts',(18.2573759618329,7.10162072896155,37.27238005624));
#41539=CARTESIAN_POINT('Ctrl Pts',(18.2847069418369,7.09745972558659,37.2157650187585));
#41540=CARTESIAN_POINT('Ctrl Pts',(18.3084816677062,7.0940502655181,37.1710938129257));
#41541=CARTESIAN_POINT('Ctrl Pts',(18.4255917714032,7.07813408772557,36.9704873588428));
#41542=CARTESIAN_POINT('Ctrl Pts',(18.5389110605227,7.06491952083453,36.8273021522816));
#41543=CARTESIAN_POINT('Ctrl Pts',(18.7076702204365,7.04859360054267,36.6668036412418));
#41544=CARTESIAN_POINT('Ctrl Pts',(18.7461954943087,7.0450547075126,36.632981468767));
#41545=CARTESIAN_POINT('Ctrl Pts',(18.7920828898353,7.04109136945516,36.5958259546593));
#41546=CARTESIAN_POINT('Ctrl Pts',(18.7981699951251,7.04057052010409,36.5909579369317));
#41547=CARTESIAN_POINT('Ctrl Pts',(18.8079347495209,7.03974299810826,36.5832453699829));
#41548=CARTESIAN_POINT('Ctrl Pts',(18.8115933892912,7.0394347198947,36.5803770540618));
#41549=CARTESIAN_POINT('Ctrl Pts',(18.8180879950552,7.03889067085551,36.5753231857247));
#41550=CARTESIAN_POINT('Ctrl Pts',(18.820919720074,7.03865452627345,36.5731322684188));
#41551=CARTESIAN_POINT('Ctrl Pts',(18.826944673017,7.03815436717077,36.5684974942798));
#41552=CARTESIAN_POINT('Ctrl Pts',(18.8301394429978,7.03789049823434,36.5660557366406));
#41553=CARTESIAN_POINT('Ctrl Pts',(18.8388183851344,7.0371772311926,36.5594653198336));
#41554=CARTESIAN_POINT('Ctrl Pts',(18.8443172075076,7.03672915234368,36.5553359167372));
#41555=CARTESIAN_POINT('Ctrl Pts',(18.8722988427606,7.03446772340112,36.5345558563376));
#41556=CARTESIAN_POINT('Ctrl Pts',(18.8951212230816,7.032684045757,36.5183652906138));
#41557=CARTESIAN_POINT('Ctrl Pts',(18.9637202267152,7.02747385495932,36.4719099168097));
#41558=CARTESIAN_POINT('Ctrl Pts',(19.0104468233388,7.02411792483307,36.4430936893475));
#41559=CARTESIAN_POINT('Ctrl Pts',(19.165318497745,7.01339605634237,36.3564768397933));
#41560=CARTESIAN_POINT('Ctrl Pts',(19.2777463335862,7.00619900177139,36.3069821443026));
#41561=CARTESIAN_POINT('Ctrl Pts',(19.394104010982,6.99874099840483,36.2684889824541));
#41562=CARTESIAN_POINT('',(18.0708706407966,6.98311453081294,38.1007530932072));
#41563=CARTESIAN_POINT('Ctrl Pts',(19.3941039843085,6.82605087843334,36.2684889912782));
#41564=CARTESIAN_POINT('Ctrl Pts',(19.3858528029974,6.82657484143018,36.2712186270038));
#41565=CARTESIAN_POINT('Ctrl Pts',(19.3776184331728,6.82709973804903,36.2740045622803));
#41566=CARTESIAN_POINT('Ctrl Pts',(19.2849251791949,6.83303300897787,36.3060656240963));
#41567=CARTESIAN_POINT('Ctrl Pts',(19.2025922685194,6.83854103777915,36.3411167380629));
#41568=CARTESIAN_POINT('Ctrl Pts',(19.1110112470517,6.84510809905579,36.3878602602958));
#41569=CARTESIAN_POINT('Ctrl Pts',(19.0990949656175,6.84597139340104,36.3941003559776));
#41570=CARTESIAN_POINT('Ctrl Pts',(19.0800254104803,6.84736764354507,36.4043418767981));
#41571=CARTESIAN_POINT('Ctrl Pts',(19.0728305429145,6.8478978580011,36.4082652363379));
#41572=CARTESIAN_POINT('Ctrl Pts',(19.060214048235,6.84883374352925,36.4152496673183));
#41573=CARTESIAN_POINT('Ctrl Pts',(19.0547817974993,6.8492387238008,36.4182913847059));
#41574=CARTESIAN_POINT('Ctrl Pts',(19.0434579570639,6.85008720746342,36.4247042196473));
#41575=CARTESIAN_POINT('Ctrl Pts',(19.0375692551277,6.85053088187969,36.4280802378942));
#41576=CARTESIAN_POINT('Ctrl Pts',(19.0255918218128,6.85143834971552,36.4350311981593));
#41577=CARTESIAN_POINT('Ctrl Pts',(19.0195046599771,6.85190222782742,36.43860862685));
#41578=CARTESIAN_POINT('Ctrl Pts',(19.0046459956348,6.85304121002375,36.4474511739059));
#41579=CARTESIAN_POINT('Ctrl Pts',(18.9958965524585,6.85371762520485,36.4527527579495));
#41580=CARTESIAN_POINT('Ctrl Pts',(18.9719116545613,6.85558793663787,36.4675481155321));
#41581=CARTESIAN_POINT('Ctrl Pts',(18.9567662206135,6.85678699571189,36.47718514733));
#41582=CARTESIAN_POINT('Ctrl Pts',(18.8305710747376,6.86693285706205,36.5599797255668));
#41583=CARTESIAN_POINT('Ctrl Pts',(18.7272441820305,6.87629880461213,36.6442159180892));
#41584=CARTESIAN_POINT('Ctrl Pts',(18.5488978627026,6.89432033860499,36.8232134784334));
#41585=CARTESIAN_POINT('Ctrl Pts',(18.4724541005455,6.90290581454265,36.9157322605341));
#41586=CARTESIAN_POINT('Ctrl Pts',(18.3968573039755,6.91201507984912,37.0268319732218));
#41587=CARTESIAN_POINT('Ctrl Pts',(18.3887734687498,6.91299822987586,37.0390074392153));
#41588=CARTESIAN_POINT('Ctrl Pts',(18.3777786216145,6.91434690562991,37.0559828397409));
#41589=CARTESIAN_POINT('Ctrl Pts',(18.3747492691931,6.91471974381913,37.0607050008008));
#41590=CARTESIAN_POINT('Ctrl Pts',(18.3699338963258,6.91531431801821,37.0682837583883));
#41591=CARTESIAN_POINT('Ctrl Pts',(18.3681347126011,6.91553690649327,37.0711318890301));
#41592=CARTESIAN_POINT('Ctrl Pts',(18.3643995069793,6.91599990077081,37.077079212767));
#41593=CARTESIAN_POINT('Ctrl Pts',(18.3624648219408,6.91624021331643,37.0801792066211));
#41594=CARTESIAN_POINT('Ctrl Pts',(18.3578078552176,6.91681992784397,37.0876886004259));
#41595=CARTESIAN_POINT('Ctrl Pts',(18.3550944831485,6.91715875069488,37.0921035508282));
#41596=CARTESIAN_POINT('Ctrl Pts',(18.3456651142437,6.91834011585873,37.1075856579283));
#41597=CARTESIAN_POINT('Ctrl Pts',(18.3390425719821,6.91917683939054,37.1187097346776));
#41598=CARTESIAN_POINT('Ctrl Pts',(18.3001090547877,6.9241437771133,37.185631064587));
#41599=CARTESIAN_POINT('Ctrl Pts',(18.2704965689311,6.9281241885141,37.2429588914674));
#41600=CARTESIAN_POINT('Ctrl Pts',(18.1696011057843,6.94292279780581,37.4649113805477));
#41601=CARTESIAN_POINT('Ctrl Pts',(18.118518246039,6.95330957281582,37.637694948239));
#41602=CARTESIAN_POINT('Ctrl Pts',(18.0868252863435,6.96673918983442,37.8499060277107));
#41603=CARTESIAN_POINT('Ctrl Pts',(18.0825762337671,6.96897078751891,37.8848945998393));
#41604=CARTESIAN_POINT('Ctrl Pts',(18.0782348999335,6.97195645029124,37.9312137384344));
#41605=CARTESIAN_POINT('Ctrl Pts',(18.0772804609192,6.97268365675433,37.9424580463212));
#41606=CARTESIAN_POINT('Ctrl Pts',(18.0758945872619,6.97386636712201,37.9606809615308));
#41607=CARTESIAN_POINT('Ctrl Pts',(18.075402333959,6.97431997309735,37.9676547864593));
#41608=CARTESIAN_POINT('Ctrl Pts',(18.0745479911337,6.97517517715424,37.9807733015578));
#41609=CARTESIAN_POINT('Ctrl Pts',(18.0741773809398,6.97557650453005,37.9869173642128));
#41610=CARTESIAN_POINT('Ctrl Pts',(18.0734923732556,6.97638407949335,37.9992558201496));
#41611=CARTESIAN_POINT('Ctrl Pts',(18.073178432564,6.97679033638118,38.0054501643088));
#41612=CARTESIAN_POINT('Ctrl Pts',(18.0725289063486,6.97772140725912,38.0196170787916));
#41613=CARTESIAN_POINT('Ctrl Pts',(18.072212906941,6.97824682371792,38.0275903909346));
#41614=CARTESIAN_POINT('Ctrl Pts',(18.071220412909,6.98020917223027,38.0572884063515));
#41615=CARTESIAN_POINT('Ctrl Pts',(18.0708616452603,6.98165587447813,38.0790212731587));
#41616=CARTESIAN_POINT('Ctrl Pts',(18.0708701476231,6.98311378152447,38.1007546975382));
#41617=CARTESIAN_POINT('Ctrl Pts',(18.0708701470186,6.98311367775493,38.1007531506166));
#41618=CARTESIAN_POINT('Ctrl Pts',(18.0709451226708,6.99599621466959,38.2927967682577));
#41619=CARTESIAN_POINT('Ctrl Pts',(18.0996985916395,7.00983650789902,38.4837380098122));
#41620=CARTESIAN_POINT('Ctrl Pts',(18.1775359073487,7.02858094791619,38.7367556225892));
#41621=CARTESIAN_POINT('Ctrl Pts',(18.2028404352395,7.03366187836658,38.8050199547983));
#41622=CARTESIAN_POINT('Ctrl Pts',(18.2354352276877,7.03913218367775,38.8796986002796));
#41623=CARTESIAN_POINT('Ctrl Pts',(18.2389811590489,7.03971525543524,38.887674673867));
#41624=CARTESIAN_POINT('Ctrl Pts',(18.2444029712373,7.04058864085328,38.8996506370724));
#41625=CARTESIAN_POINT('Ctrl Pts',(18.2462385951028,7.04088129764717,38.9036684667384));
#41626=CARTESIAN_POINT('Ctrl Pts',(18.2494314268578,7.04138508451765,38.9105939324495));
#41627=CARTESIAN_POINT('Ctrl Pts',(18.2507820980219,7.04159660737534,38.9135045079869));
#41628=CARTESIAN_POINT('Ctrl Pts',(18.253872949792,7.04207703553061,38.9201217276398));
#41629=CARTESIAN_POINT('Ctrl Pts',(18.2556176703331,7.04234565868894,38.9238262027469));
#41630=CARTESIAN_POINT('Ctrl Pts',(18.2603876043567,7.04307320154476,38.9338708645408));
#41631=CARTESIAN_POINT('Ctrl Pts',(18.263435711834,7.04353074276029,38.9402002038676));
#41632=CARTESIAN_POINT('Ctrl Pts',(18.2783620745301,7.04573665027384,38.9707662782485));
#41633=CARTESIAN_POINT('Ctrl Pts',(18.2907141940179,7.04745771292089,38.9947699535155));
#41634=CARTESIAN_POINT('Ctrl Pts',(18.4017574022293,7.06213277724415,39.1998606076852));
#41635=CARTESIAN_POINT('Ctrl Pts',(18.5283992585239,7.07383150893857,39.364313140902));
#41636=CARTESIAN_POINT('Ctrl Pts',(18.7040178810975,7.08872703666962,39.5293984731066));
#41637=CARTESIAN_POINT('Ctrl Pts',(18.7299694634229,7.09089665352579,39.5525053762315));
#41638=CARTESIAN_POINT('Ctrl Pts',(18.769034327419,7.09412821904715,39.585440534307));
#41639=CARTESIAN_POINT('Ctrl Pts',(18.7816722336872,7.09516857750915,39.5958233506788));
#41640=CARTESIAN_POINT('Ctrl Pts',(18.801927124806,7.09682895698293,39.612037007154));
#41641=CARTESIAN_POINT('Ctrl Pts',(18.8094583841522,7.09744481993309,39.6179740382746));
#41642=CARTESIAN_POINT('Ctrl Pts',(18.8236245114228,7.09860064406508,39.6289711861119));
#41643=CARTESIAN_POINT('Ctrl Pts',(18.8302485728027,7.09914005916544,39.6340449058181));
#41644=CARTESIAN_POINT('Ctrl Pts',(18.8419404748374,7.10009044353685,39.6428805934953));
#41645=CARTESIAN_POINT('Ctrl Pts',(18.8469942857584,7.1005006888193,39.6466609877271));
#41646=CARTESIAN_POINT('Ctrl Pts',(18.8568340599231,7.10129840730382,39.6539463890965));
#41647=CARTESIAN_POINT('Ctrl Pts',(18.8616178239336,7.10168576380203,39.6574542582801));
#41648=CARTESIAN_POINT('Ctrl Pts',(18.8740318279235,7.10268980871408,39.6664695286179));
#41649=CARTESIAN_POINT('Ctrl Pts',(18.881686250106,7.10330777787923,39.6719432114814));
#41650=CARTESIAN_POINT('Ctrl Pts',(18.9076056374896,7.10539680513369,39.6901930538897));
#41651=CARTESIAN_POINT('Ctrl Pts',(18.9260513321061,7.10687763623885,39.7027082018218));
#41652=CARTESIAN_POINT('Ctrl Pts',(19.0620143709475,7.11775512283747,39.7915561260047));
#41653=CARTESIAN_POINT('Ctrl Pts',(19.1873009218152,7.12762216127692,39.8551881107461));
#41654=CARTESIAN_POINT('Ctrl Pts',(19.3576475400654,7.14061115860368,39.9195304164095));
#41655=CARTESIAN_POINT('Ctrl Pts',(19.3974247670469,7.14361211671348,39.9330877674157));
#41656=CARTESIAN_POINT('Ctrl Pts',(19.4936432251052,7.15076111878538,39.9624114271104));
#41657=CARTESIAN_POINT('Ctrl Pts',(19.5504261981082,7.15489197747742,39.976927782616));
#41658=CARTESIAN_POINT('Ctrl Pts',(19.6363569591627,7.16093783703543,39.9947711799202));
#41659=CARTESIAN_POINT('Ctrl Pts',(19.6650613478746,7.16292352358157,40.0000553709158));
#41660=CARTESIAN_POINT('Ctrl Pts',(19.7007583214694,7.16534230290854,40.0057926326559));
#41661=CARTESIAN_POINT('Ctrl Pts',(19.7076462975802,7.16580669843896,40.0068614153111));
#41662=CARTESIAN_POINT('Ctrl Pts',(19.7185372774929,7.16653715221506,40.0084909295829));
#41663=CARTESIAN_POINT('Ctrl Pts',(19.7225364264193,7.16680455936949,40.009076441252));
#41664=CARTESIAN_POINT('Ctrl Pts',(19.7300770239457,7.16730719778903,40.0101562578836));
#41665=CARTESIAN_POINT('Ctrl Pts',(19.733617964495,7.16754257157321,40.0106532793601));
#41666=CARTESIAN_POINT('Ctrl Pts',(19.7417303601146,7.16808034151931,40.0117689792453));
#41667=CARTESIAN_POINT('Ctrl Pts',(19.7463026649192,7.16838236883808,40.0123811074555));
#41668=CARTESIAN_POINT('Ctrl Pts',(19.758484353295,7.16918429667777,40.0139675022851));
#41669=CARTESIAN_POINT('Ctrl Pts',(19.7660975214228,7.16968262842431,40.0149128028862));
#41670=CARTESIAN_POINT('Ctrl Pts',(19.821492170406,7.17328920535012,40.0214556697545));
#41671=CARTESIAN_POINT('Ctrl Pts',(19.8694670976077,7.17630816033769,40.0253100999269));
#41672=CARTESIAN_POINT('Ctrl Pts',(19.931403883757,7.18012862032513,40.0279599789975));
#41673=CARTESIAN_POINT('Ctrl Pts',(19.9452737255619,7.18097918049418,40.0284035254081));
#41674=CARTESIAN_POINT('Ctrl Pts',(20.0763372416713,7.18897930323712,40.0311796406608));
#41675=CARTESIAN_POINT('Ctrl Pts',(20.1935132412684,7.1958648121822,40.0229761317434));
#41676=CARTESIAN_POINT('Ctrl Pts',(20.3755218295595,7.20697510283853,39.9934194593316));
#41677=CARTESIAN_POINT('Ctrl Pts',(20.4412072872112,7.21106939490562,39.9791990006346));
#41678=CARTESIAN_POINT('Ctrl Pts',(20.5437210434686,7.21770155986098,39.9513338088674));
#41679=CARTESIAN_POINT('Ctrl Pts',(20.581105888455,7.22017225540584,39.9399415907366));
#41680=CARTESIAN_POINT('Ctrl Pts',(20.6288020949996,7.22340365428764,39.923808573504));
#41681=CARTESIAN_POINT('Ctrl Pts',(20.6394549708123,7.22413053792766,39.920100854069));
#41682=CARTESIAN_POINT('Ctrl Pts',(20.6566557872662,7.22531285188686,39.9139444851462));
#41683=CARTESIAN_POINT('Ctrl Pts',(20.6632241124896,7.22576638665549,39.9115532541511));
#41684=CARTESIAN_POINT('Ctrl Pts',(20.6757868369142,7.22663783912198,39.9069022514233));
#41685=CARTESIAN_POINT('Ctrl Pts',(20.6817832705229,7.22705556215035,39.9046482110165));
#41686=CARTESIAN_POINT('Ctrl Pts',(20.6954316454362,7.22801041352389,39.8994400966851));
#41687=CARTESIAN_POINT('Ctrl Pts',(20.7030761551102,7.22854816829931,39.8964670193599));
#41688=CARTESIAN_POINT('Ctrl Pts',(20.7232293359044,7.2299737510969,39.8884807746029));
#41689=CARTESIAN_POINT('Ctrl Pts',(20.7357046576024,7.23086431665249,39.8833852064625));
#41690=CARTESIAN_POINT('Ctrl Pts',(20.830525979133,7.23769649664952,39.8434910170851));
#41691=CARTESIAN_POINT('Ctrl Pts',(20.9104048294238,7.24382600958484,39.8031421497736));
#41692=CARTESIAN_POINT('Ctrl Pts',(21.126345242012,7.26145560671731,39.6745231123822));
#41693=CARTESIAN_POINT('Ctrl Pts',(21.2544989827452,7.27325312490255,39.5744509597995));
#41694=CARTESIAN_POINT('Ctrl Pts',(21.3898939094768,7.28649995315475,39.4381506157628));
#41695=CARTESIAN_POINT('Ctrl Pts',(21.4106454898574,7.28855364428785,39.4162567006065));
#41696=CARTESIAN_POINT('Ctrl Pts',(21.4356004539932,7.29104318179648,39.3886595753161));
#41697=CARTESIAN_POINT('Ctrl Pts',(21.4402958797064,7.29151250106591,39.3834095009929));
#41698=CARTESIAN_POINT('Ctrl Pts',(21.4476510550319,7.29224892866684,39.3750942891025));
#41699=CARTESIAN_POINT('Ctrl Pts',(21.4503300093345,7.29251742248839,39.3720463387847));
#41700=CARTESIAN_POINT('Ctrl Pts',(21.4553493182554,7.29302094048996,39.3662992067547));
#41701=CARTESIAN_POINT('Ctrl Pts',(21.4576917654595,7.29325611387016,39.3636020086775));
#41702=CARTESIAN_POINT('Ctrl Pts',(21.4630244268615,7.29379194932174,39.3574271818331));
#41703=CARTESIAN_POINT('Ctrl Pts',(21.4660097391147,7.29409225208356,39.353945388403));
#41704=CARTESIAN_POINT('Ctrl Pts',(21.4738963060659,7.29488657974326,39.3446805615358));
#41705=CARTESIAN_POINT('Ctrl Pts',(21.4787759994876,7.29537908261486,39.3388791584424));
#41706=CARTESIAN_POINT('Ctrl Pts',(21.5130216006856,7.29884399537533,39.297674382362));
#41707=CARTESIAN_POINT('Ctrl Pts',(21.5411499254214,7.30173484522444,39.2612562076873));
#41708=CARTESIAN_POINT('Ctrl Pts',(21.5851969229477,7.30640260330273,39.1998043172763));
#41709=CARTESIAN_POINT('Ctrl Pts',(21.6018867570773,7.30820849952043,39.1753500662346));
#41710=CARTESIAN_POINT('Ctrl Pts',(21.7087264647854,7.32008957529816,39.0107959576731));
#41711=CARTESIAN_POINT('Ctrl Pts',(21.7809613327102,7.32977717791028,38.8599164126599));
#41712=CARTESIAN_POINT('Ctrl Pts',(21.8462808818332,7.34281454240508,38.6609151748142));
#41713=CARTESIAN_POINT('Ctrl Pts',(21.8582840242908,7.34551865650919,38.6197681966811));
#41714=CARTESIAN_POINT('Ctrl Pts',(21.8717921112903,7.3490136989711,38.5669821409585));
#41715=CARTESIAN_POINT('Ctrl Pts',(21.8745754704882,7.34976345918943,38.5556806158579));
#41716=CARTESIAN_POINT('Ctrl Pts',(21.8788847448866,7.35097387502627,38.5374753150206));
#41717=CARTESIAN_POINT('Ctrl Pts',(21.8804753007679,7.35143246362559,38.5305870142263));
#41718=CARTESIAN_POINT('Ctrl Pts',(21.8834304582037,7.35230759950435,38.5174602323339));
#41719=CARTESIAN_POINT('Ctrl Pts',(21.8848020185533,7.35272391888372,38.5112234011923));
#41720=CARTESIAN_POINT('Ctrl Pts',(21.887860698522,7.35367607038993,38.4969779880783));
#41721=CARTESIAN_POINT('Ctrl Pts',(21.889527861157,7.35421252807334,38.4889652921254));
#41722=CARTESIAN_POINT('Ctrl Pts',(21.8937345861478,7.35561316221726,38.4680814945215));
#41723=CARTESIAN_POINT('Ctrl Pts',(21.8961938929825,7.35647985571269,38.4551948411967));
#41724=CARTESIAN_POINT('Ctrl Pts',(21.9124042379086,7.36254472456089,38.3652822091085));
#41725=CARTESIAN_POINT('Ctrl Pts',(21.9215876540301,7.36788540887421,38.287517058924));
#41726=CARTESIAN_POINT('Ctrl Pts',(21.9354059469477,7.38487899077248,38.044280527458));
#41727=CARTESIAN_POINT('Ctrl Pts',(21.9235109431242,7.39692556273527,37.8786416431793));
#41728=CARTESIAN_POINT('Ctrl Pts',(21.8831495853239,7.41101825561416,37.6796311612153));
#41729=CARTESIAN_POINT('Ctrl Pts',(21.8745792757848,7.41359709236386,37.6429274420165));
#41730=CARTESIAN_POINT('Ctrl Pts',(21.8630132651908,7.41662532754928,37.5992198355335));
#41731=CARTESIAN_POINT('Ctrl Pts',(21.8610453548205,7.41712720679983,37.5919553254992));
#41732=CARTESIAN_POINT('Ctrl Pts',(21.8579227787256,7.41790305680837,37.5806900338326));
#41733=CARTESIAN_POINT('Ctrl Pts',(21.8567976164936,7.41817866508047,37.5766812588244));
#41734=CARTESIAN_POINT('Ctrl Pts',(21.8546870762952,7.41868835174971,37.5692542410238));
#41735=CARTESIAN_POINT('Ctrl Pts',(21.8537052306787,7.41892262209014,37.5658351099622));
#41736=CARTESIAN_POINT('Ctrl Pts',(21.8514585354851,7.4194523266521,37.5580921270005));
#41737=CARTESIAN_POINT('Ctrl Pts',(21.8501879969507,7.41974742864587,37.5537699858152));
#41738=CARTESIAN_POINT('Ctrl Pts',(21.8462873501272,7.42064017400587,37.5406704584045));
#41739=CARTESIAN_POINT('Ctrl Pts',(21.8436097897944,7.42123515059807,37.5319071674792));
#41740=CARTESIAN_POINT('Ctrl Pts',(21.808117864894,7.42890006571124,37.4186411624404));
#41741=CARTESIAN_POINT('Ctrl Pts',(21.7665180241971,7.43550018066607,37.3170813538788));
#41742=CARTESIAN_POINT('Ctrl Pts',(21.6783718978196,7.4470564462287,37.1452250043875));
#41743=CARTESIAN_POINT('Ctrl Pts',(21.6354378095822,7.4520184438928,37.0734181698498));
#41744=CARTESIAN_POINT('Ctrl Pts',(21.5435486302553,7.46182775610449,36.9402049872904));
#41745=CARTESIAN_POINT('Ctrl Pts',(21.4952393446977,7.46665292326438,36.8785565830981));
#41746=CARTESIAN_POINT('Ctrl Pts',(21.4306574021558,7.47284053338721,36.8057332562141));
#41747=CARTESIAN_POINT('Ctrl Pts',(21.417779815532,7.47406239039933,36.7916394382466));
#41748=CARTESIAN_POINT('Ctrl Pts',(21.3988092978767,7.47584661267469,36.7714862229735));
#41749=CARTESIAN_POINT('Ctrl Pts',(21.3928814395482,7.47640197587688,36.7652724626271));
#41750=CARTESIAN_POINT('Ctrl Pts',(21.3824342476616,7.47737709711229,36.7544667916662));
#41751=CARTESIAN_POINT('Ctrl Pts',(21.3779329992399,7.4777960710417,36.7498575216788));
#41752=CARTESIAN_POINT('Ctrl Pts',(21.3691596018897,7.47861049875699,36.7409631520696));
#41753=CARTESIAN_POINT('Ctrl Pts',(21.3648902094779,7.4790058294298,36.7366754296384));
#41754=CARTESIAN_POINT('Ctrl Pts',(21.3546515772088,7.47995157623165,36.7264891388185));
#41755=CARTESIAN_POINT('Ctrl Pts',(21.3486639215867,7.48050280239419,36.7206093358758));
#41756=CARTESIAN_POINT('Ctrl Pts',(21.326982973375,7.48249228792233,36.6995950315257));
#41757=CARTESIAN_POINT('Ctrl Pts',(21.3110722399557,7.48394024694469,36.6846882311464));
#41758=CARTESIAN_POINT('Ctrl Pts',(21.1824184618211,7.49555857838946,36.5681834691844));
#41759=CARTESIAN_POINT('Ctrl Pts',(21.0583168501463,7.5062906466541,36.4799619870505));
#41760=CARTESIAN_POINT('Ctrl Pts',(20.8530483154411,7.52298307926174,36.3677727958251));
#41761=CARTESIAN_POINT('Ctrl Pts',(20.778450239649,7.52884716119518,36.3329913917537));
#41762=CARTESIAN_POINT('Ctrl Pts',(20.6684626299568,7.53702977321516,36.2900316223206));
#41763=CARTESIAN_POINT('Ctrl Pts',(20.6347091761776,7.53948047198674,36.2779208355744));
#41764=CARTESIAN_POINT('Ctrl Pts',(20.5935839753904,7.54237841826551,36.2644467648996));
#41765=CARTESIAN_POINT('Ctrl Pts',(20.5865192814805,7.54287314567127,36.2621771707859));
#41766=CARTESIAN_POINT('Ctrl Pts',(20.5754921552711,7.54364034976065,36.2587046732253));
#41767=CARTESIAN_POINT('Ctrl Pts',(20.5715387422013,7.5439144070902,36.2574736994701));
#41768=CARTESIAN_POINT('Ctrl Pts',(20.5641791091952,7.54442269467029,36.2552080979581));
#41769=CARTESIAN_POINT('Ctrl Pts',(20.5607740206233,7.54465710767688,36.2541701792394));
#41770=CARTESIAN_POINT('Ctrl Pts',(20.5530228441907,7.54518901183027,36.2518309407373));
#41771=CARTESIAN_POINT('Ctrl Pts',(20.5486750336585,7.54548615914995,36.2505355244583));
#41772=CARTESIAN_POINT('Ctrl Pts',(20.5353790266784,7.54639128627431,36.2466250347177));
#41773=CARTESIAN_POINT('Ctrl Pts',(20.5264162470188,7.54699648967387,36.2440594278164));
#41774=CARTESIAN_POINT('Ctrl Pts',(20.4403978630993,7.55276072658779,36.2201098276846));
#41775=CARTESIAN_POINT('Ctrl Pts',(20.3620909182083,7.55767164189551,36.2034687248536));
#41776=CARTESIAN_POINT('Ctrl Pts',(20.1202135927457,7.57243785141414,36.1676018583233));
#41777=CARTESIAN_POINT('Ctrl Pts',(19.9550508868086,7.58202967028628,36.1643882268082));
#41778=CARTESIAN_POINT('Ctrl Pts',(19.7520416458881,7.59477220980439,36.1864605562292));
#41779=CARTESIAN_POINT('Ctrl Pts',(19.7127445987153,7.59727992024078,36.1919642210437));
#41780=CARTESIAN_POINT('Ctrl Pts',(19.6624717017945,7.60055322058162,36.2005933094492));
#41781=CARTESIAN_POINT('Ctrl Pts',(19.6513135329234,7.60128387631829,36.2026099855445));
#41782=CARTESIAN_POINT('Ctrl Pts',(19.6332937046177,7.60247082253156,36.2060311263591));
#41783=CARTESIAN_POINT('Ctrl Pts',(19.6264206683724,7.60292518959078,36.2073748172886));
#41784=CARTESIAN_POINT('Ctrl Pts',(19.6132785022379,7.60379722409308,36.2100185104325));
#41785=CARTESIAN_POINT('Ctrl Pts',(19.6070082179981,7.60421469129771,36.2113123589736));
#41786=CARTESIAN_POINT('Ctrl Pts',(19.5927455496838,7.60516754715848,36.2143295046778));
#41787=CARTESIAN_POINT('Ctrl Pts',(19.5847574899224,7.60570355301937,36.2160724380727));
#41788=CARTESIAN_POINT('Ctrl Pts',(19.5637203264854,7.6071214662114,36.2208028827239));
#41789=CARTESIAN_POINT('Ctrl Pts',(19.5506910091764,7.60800606408194,36.2238754906501));
#41790=CARTESIAN_POINT('Ctrl Pts',(19.4892970214218,7.61220539181532,36.2390297946192));
#41791=CARTESIAN_POINT('Ctrl Pts',(19.4413979263548,7.61557396157359,36.2528433227398));
#41792=CARTESIAN_POINT('Ctrl Pts',(19.3941039249488,7.61899517246903,36.2684890109154));
#41793=CARTESIAN_POINT('Origin',(20.,-1.3495818343519,38.1));
#41794=CARTESIAN_POINT('',(19.3941041019635,8.58595480644739,36.2684889523559));
#41795=CARTESIAN_POINT('',(19.3941040078119,8.41575742730426,36.2684889835028));
#41796=CARTESIAN_POINT('',(19.3941040087494,-1.3495818343519,36.2684889831927));
#41797=CARTESIAN_POINT('',(18.0708707679468,7.94955926345013,38.0982625861522));
#41798=CARTESIAN_POINT('Ctrl Pts',(19.3941041019635,8.58595480644739,36.2684889523559));
#41799=CARTESIAN_POINT('Ctrl Pts',(19.5043238617899,8.57774700749365,36.232026327439));
#41800=CARTESIAN_POINT('Ctrl Pts',(19.6176380959992,8.56937247835458,36.2055779375375));
#41801=CARTESIAN_POINT('Ctrl Pts',(19.7850254076397,8.55751279271299,36.1821568103993));
#41802=CARTESIAN_POINT('Ctrl Pts',(19.837658427954,8.5538586227368,36.1769859789215));
#41803=CARTESIAN_POINT('Ctrl Pts',(19.899036483125,8.5497314476424,36.1734946084228));
#41804=CARTESIAN_POINT('Ctrl Pts',(19.9076340194586,8.54915639541592,36.1730632631204));
#41805=CARTESIAN_POINT('Ctrl Pts',(19.9206797789185,8.54828875176964,36.1724962623643));
#41806=CARTESIAN_POINT('Ctrl Pts',(19.925125919035,8.5479939174509,36.1723184316234));
#41807=CARTESIAN_POINT('Ctrl Pts',(19.9331241524775,8.54746514442149,36.172026243011));
#41808=CARTESIAN_POINT('Ctrl Pts',(19.9366759626202,8.54723090377612,36.1719063161892));
#41809=CARTESIAN_POINT('Ctrl Pts',(19.9444328203213,8.54672059747401,36.1716658636416));
#41810=CARTESIAN_POINT('Ctrl Pts',(19.948637926966,8.54644475234078,36.1715492769608));
#41811=CARTESIAN_POINT('Ctrl Pts',(19.9605663728216,8.5456644564136,36.1712576052149));
#41812=CARTESIAN_POINT('Ctrl Pts',(19.9682905379219,8.54516177653989,36.1711151534359));
#41813=CARTESIAN_POINT('Ctrl Pts',(20.017461461831,8.54197711599725,36.1705037738062));
#41814=CARTESIAN_POINT('Ctrl Pts',(20.0589169041221,8.53936141876005,36.1713242933359));
#41815=CARTESIAN_POINT('Ctrl Pts',(20.2079179135493,8.53010681927217,36.1790830263577));
#41816=CARTESIAN_POINT('Ctrl Pts',(20.3148688809859,8.52373175893408,36.1936911955294));
#41817=CARTESIAN_POINT('Ctrl Pts',(20.5473984682729,8.50948737417836,36.2455666793631));
#41818=CARTESIAN_POINT('Ctrl Pts',(20.671519263033,8.50160823850721,36.2868196307428));
#41819=CARTESIAN_POINT('Ctrl Pts',(20.8030862588113,8.49240019764376,36.345923366389));
#41820=CARTESIAN_POINT('Ctrl Pts',(20.8155927443807,8.49151624699186,36.3517034475761));
#41821=CARTESIAN_POINT('Ctrl Pts',(20.8355243352645,8.49009305184941,36.3611755747837));
#41822=CARTESIAN_POINT('Ctrl Pts',(20.8429895623312,8.48955672380164,36.36478246585));
#41823=CARTESIAN_POINT('Ctrl Pts',(20.8561929276389,8.48860220064429,36.3712671020124));
#41824=CARTESIAN_POINT('Ctrl Pts',(20.8619404243843,8.48818467592202,36.3741255940601));
#41825=CARTESIAN_POINT('Ctrl Pts',(20.8738790821723,8.48731313620537,36.3801377433142));
#41826=CARTESIAN_POINT('Ctrl Pts',(20.8800676765594,8.48685895650295,36.383296264702));
#41827=CARTESIAN_POINT('Ctrl Pts',(20.8960886652151,8.48567684880896,36.3915824196914));
#41828=CARTESIAN_POINT('Ctrl Pts',(20.9058940384917,8.48494712963843,36.3967614650363));
#41829=CARTESIAN_POINT('Ctrl Pts',(20.9484084422549,8.48175550116334,36.4196878792799));
#41830=CARTESIAN_POINT('Ctrl Pts',(20.9806428129817,8.47926346246601,36.4382940256709));
#41831=CARTESIAN_POINT('Ctrl Pts',(21.0655832083181,8.47249507451684,36.4906552785584));
#41832=CARTESIAN_POINT('Ctrl Pts',(21.1172150874565,8.46816320792328,36.526060000138));
#41833=CARTESIAN_POINT('Ctrl Pts',(21.2768268029229,8.4540822400479,36.6473234756515));
#41834=CARTESIAN_POINT('Ctrl Pts',(21.3773552268127,8.44409944195503,36.7422645013639));
#41835=CARTESIAN_POINT('Ctrl Pts',(21.4982057141647,8.43108015010229,36.8837576728504));
#41836=CARTESIAN_POINT('Ctrl Pts',(21.5281279916781,8.42775725084318,36.9215724488586));
#41837=CARTESIAN_POINT('Ctrl Pts',(21.5611384527053,8.42400694206373,36.9666650110812));
#41838=CARTESIAN_POINT('Ctrl Pts',(21.5656352515864,8.42349412976692,36.9728852190596));
#41839=CARTESIAN_POINT('Ctrl Pts',(21.5727758183025,8.42267691897157,36.9828876186431));
#41840=CARTESIAN_POINT('Ctrl Pts',(21.5754432915877,8.42237097572814,36.9866526672662));
#41841=CARTESIAN_POINT('Ctrl Pts',(21.580153945673,8.42182956483748,36.9933524268374));
#41842=CARTESIAN_POINT('Ctrl Pts',(21.5822025049234,8.42159373604685,36.9962832893163));
#41843=CARTESIAN_POINT('Ctrl Pts',(21.5865488342371,8.42109258842567,37.002538527402));
#41844=CARTESIAN_POINT('Ctrl Pts',(21.5888443081796,8.42082742366053,37.0058644268811));
#41845=CARTESIAN_POINT('Ctrl Pts',(21.5950689002712,8.42010697281708,37.0149441013281));
#41846=CARTESIAN_POINT('Ctrl Pts',(21.5989773733471,8.41965305159049,37.0207120574181));
#41847=CARTESIAN_POINT('Ctrl Pts',(21.6190712611747,8.41731061792136,37.0507144936513));
#41848=CARTESIAN_POINT('Ctrl Pts',(21.6347382666792,8.41545437735998,37.0752937763059));
#41849=CARTESIAN_POINT('Ctrl Pts',(21.6801363133684,8.40995273702522,37.1502099358469));
#41850=CARTESIAN_POINT('Ctrl Pts',(21.7081441322808,8.40638759226898,37.2015547359169));
#41851=CARTESIAN_POINT('Ctrl Pts',(21.776756512613,8.39695350711334,37.3421837899237));
#41852=CARTESIAN_POINT('Ctrl Pts',(21.8129586838587,8.39116609073237,37.4334189104684));
#41853=CARTESIAN_POINT('Ctrl Pts',(21.8704881540301,8.37947960255212,37.6183672151824));
#41854=CARTESIAN_POINT('Ctrl Pts',(21.892066264344,8.37360205581332,37.7116990205948));
#41855=CARTESIAN_POINT('Ctrl Pts',(21.9087027030294,8.36662561413914,37.819676234784));
#41856=CARTESIAN_POINT('Ctrl Pts',(21.9106309678426,8.36575311868281,37.8331354061458));
#41857=CARTESIAN_POINT('Ctrl Pts',(21.9134987862395,8.36434486056527,37.8547800690763));
#41858=CARTESIAN_POINT('Ctrl Pts',(21.9145284757811,8.36381191662194,37.8629533138285));
#41859=CARTESIAN_POINT('Ctrl Pts',(21.9162663855726,8.36286127988631,37.877498763052));
#41860=CARTESIAN_POINT('Ctrl Pts',(21.9169952520846,8.36244423875731,37.8838684133398));
#41861=CARTESIAN_POINT('Ctrl Pts',(21.9184505209835,8.36157153711125,37.8971730385672));
#41862=CARTESIAN_POINT('Ctrl Pts',(21.9191711005266,8.36111570112041,37.9041085440699));
#41863=CARTESIAN_POINT('Ctrl Pts',(21.9209512196792,8.35992449192634,37.922195487088));
#41864=CARTESIAN_POINT('Ctrl Pts',(21.9219512473859,8.35918727559492,37.9333523869684));
#41865=CARTESIAN_POINT('Ctrl Pts',(21.9259410720916,8.35591574765227,37.9826944939233));
#41866=CARTESIAN_POINT('Ctrl Pts',(21.9278902407265,8.35334940818683,38.0209527923013));
#41867=CARTESIAN_POINT('Ctrl Pts',(21.9300777005635,8.34632041394812,38.1244639282722));
#41868=CARTESIAN_POINT('Ctrl Pts',(21.9281466273671,8.34179677456824,38.1897079067705));
#41869=CARTESIAN_POINT('Ctrl Pts',(21.9119630759648,8.32759887338222,38.3908385600846));
#41870=CARTESIAN_POINT('Ctrl Pts',(21.8865905501917,8.31771292971884,38.5253986675655));
#41871=CARTESIAN_POINT('Ctrl Pts',(21.8340415134774,8.30498030128192,38.6999379413452));
#41872=CARTESIAN_POINT('Ctrl Pts',(21.8193038167707,8.30183233295177,38.7432481670721));
#41873=CARTESIAN_POINT('Ctrl Pts',(21.800344524941,8.29825506306183,38.793079772646));
#41874=CARTESIAN_POINT('Ctrl Pts',(21.7976081074813,8.2977488385694,38.8001464677335));
#41875=CARTESIAN_POINT('Ctrl Pts',(21.793149068082,8.29694009020383,38.8114632833104));
#41876=CARTESIAN_POINT('Ctrl Pts',(21.79145284255,8.29663607067478,38.8157236183458));
#41877=CARTESIAN_POINT('Ctrl Pts',(21.7884081912497,8.29609681990817,38.8232920984344));
#41878=CARTESIAN_POINT('Ctrl Pts',(21.7870657502158,8.29586123793041,38.8266025897227));
#41879=CARTESIAN_POINT('Ctrl Pts',(21.78417854837,8.29535921432831,38.8336660922654));
#41880=CARTESIAN_POINT('Ctrl Pts',(21.7826311408557,8.29509293398203,38.8374179573399));
#41881=CARTESIAN_POINT('Ctrl Pts',(21.7783650062004,8.2943662885714,38.8476697811219));
#41882=CARTESIAN_POINT('Ctrl Pts',(21.7756224589712,8.29390732820784,38.8541598529635));
#41883=CARTESIAN_POINT('Ctrl Pts',(21.7609405293519,8.29149223060244,38.8883796567442));
#41884=CARTESIAN_POINT('Ctrl Pts',(21.7483862181402,8.28957079612882,38.9158430666385));
#41885=CARTESIAN_POINT('Ctrl Pts',(21.6644354330777,8.27751898720139,39.088642953745));
#41886=CARTESIAN_POINT('Ctrl Pts',(21.5756181452756,8.2681481117834,39.2248110979603));
#41887=CARTESIAN_POINT('Ctrl Pts',(21.4129456956631,8.25294054682854,39.4164826332059));
#41888=CARTESIAN_POINT('Ctrl Pts',(21.3504064705224,8.24742933032817,39.480558327958));
#41889=CARTESIAN_POINT('Ctrl Pts',(21.2736175760321,8.24085919584937,39.5490071091366));
#41890=CARTESIAN_POINT('Ctrl Pts',(21.2634878760538,8.23999627543739,39.5578483133369));
#41891=CARTESIAN_POINT('Ctrl Pts',(21.2470379612693,8.23860051268736,39.5719055713394));
#41892=CARTESIAN_POINT('Ctrl Pts',(21.2407753675681,8.23807040856352,39.5771886039425));
#41893=CARTESIAN_POINT('Ctrl Pts',(21.2295576066806,8.23712301863193,39.5865300773592));
#41894=CARTESIAN_POINT('Ctrl Pts',(21.2246154948986,8.23670636880961,39.5906040611266));
#41895=CARTESIAN_POINT('Ctrl Pts',(21.2142339902983,8.23583262089247,39.5990754809065));
#41896=CARTESIAN_POINT('Ctrl Pts',(21.2087907949658,8.23537533804722,39.6034680882857));
#41897=CARTESIAN_POINT('Ctrl Pts',(21.1944918067681,8.23417618426676,39.6148793901517));
#41898=CARTESIAN_POINT('Ctrl Pts',(21.1855981266558,8.2334324244053,39.6218499650206));
#41899=CARTESIAN_POINT('Ctrl Pts',(21.1455179644657,8.23008942259485,39.6526989121731));
#41900=CARTESIAN_POINT('Ctrl Pts',(21.113669740123,8.22745640142304,39.6756981461338));
#41901=CARTESIAN_POINT('Ctrl Pts',(20.9453939377219,8.21365157496461,39.7895677101796));
#41902=CARTESIAN_POINT('Ctrl Pts',(20.7985066684081,8.20187442244596,39.8637397452433));
#41903=CARTESIAN_POINT('Ctrl Pts',(20.5676366157588,8.18447987720601,39.9455089633555));
#41904=CARTESIAN_POINT('Ctrl Pts',(20.4895794820079,8.17878937098991,39.9677338732078));
#41905=CARTESIAN_POINT('Ctrl Pts',(20.4012275441371,8.17271228961747,39.9869674389053));
#41906=CARTESIAN_POINT('Ctrl Pts',(20.3920938312977,8.17208834801149,39.988886469251));
#41907=CARTESIAN_POINT('Ctrl Pts',(20.3784979744386,8.17116632810962,39.9916401454374));
#41908=CARTESIAN_POINT('Ctrl Pts',(20.374046397906,8.17086550965605,39.9925254158779));
#41909=CARTESIAN_POINT('Ctrl Pts',(20.3660976824715,8.17033032891322,39.9940770092554));
#41910=CARTESIAN_POINT('Ctrl Pts',(20.3626017936172,8.17009563135596,39.994749368672));
#41911=CARTESIAN_POINT('Ctrl Pts',(20.3550371918124,8.16958925218407,39.9961825549488));
#41912=CARTESIAN_POINT('Ctrl Pts',(20.350967894551,8.16931776459893,39.9969399640085));
#41913=CARTESIAN_POINT('Ctrl Pts',(20.3396035262588,8.16856204734921,39.9990173672848));
#41914=CARTESIAN_POINT('Ctrl Pts',(20.3323031407572,8.16807941608292,40.0003084337238));
#41915=CARTESIAN_POINT('Ctrl Pts',(20.2897666433618,8.16528284560933,40.0075783503781));
#41916=CARTESIAN_POINT('Ctrl Pts',(20.2543746645343,8.1630179222717,40.0126196157674));
#41917=CARTESIAN_POINT('Ctrl Pts',(20.137616068932,8.15568851912123,40.0259519936213));
#41918=CARTESIAN_POINT('Ctrl Pts',(20.0558569695587,8.15078011848537,40.0300547921389));
#41919=CARTESIAN_POINT('Ctrl Pts',(19.8217432050462,8.13678247125998,40.0269087340195));
#41920=CARTESIAN_POINT('Ctrl Pts',(19.6702065201761,8.12774637198454,40.0068253048993));
#41921=CARTESIAN_POINT('Ctrl Pts',(19.5015120977089,8.11671399412049,39.9637400008912));
#41922=CARTESIAN_POINT('Ctrl Pts',(19.4805018061017,8.11532323014771,39.9579931499158));
#41923=CARTESIAN_POINT('Ctrl Pts',(19.4515411756094,8.11338104506318,39.9495420634647));
#41924=CARTESIAN_POINT('Ctrl Pts',(19.443503894534,8.11283933775407,39.9471396827373));
#41925=CARTESIAN_POINT('Ctrl Pts',(19.4296974824988,8.11190402058982,39.9429145931875));
#41926=CARTESIAN_POINT('Ctrl Pts',(19.4239207403249,8.11151122886803,39.941117009981));
#41927=CARTESIAN_POINT('Ctrl Pts',(19.4120095652521,8.11069828916114,39.9373489921376));
#41928=CARTESIAN_POINT('Ctrl Pts',(19.4058763644345,8.11027802768853,39.935374941052));
#41929=CARTESIAN_POINT('Ctrl Pts',(19.3915887813023,8.10929505047052,39.9306971757378));
#41930=CARTESIAN_POINT('Ctrl Pts',(19.3834423932747,8.10873156271604,39.9279696588996));
#41931=CARTESIAN_POINT('Ctrl Pts',(19.3578325081119,8.10695042193203,39.9192044673199));
#41932=CARTESIAN_POINT('Ctrl Pts',(19.3404378154737,8.10572635532772,39.9129703985791));
#41933=CARTESIAN_POINT('Ctrl Pts',(19.2997750854902,8.10283030053294,39.8977346759945));
#41934=CARTESIAN_POINT('Ctrl Pts',(19.2765872613588,8.10115181742421,39.8885297897209));
#41935=CARTESIAN_POINT('Ctrl Pts',(19.1948651886159,8.09513808727592,39.8542393282697));
#41936=CARTESIAN_POINT('Ctrl Pts',(19.1374066323552,8.09072661572826,39.8267104481585));
#41937=CARTESIAN_POINT('Ctrl Pts',(18.9866601440702,8.07867597343489,39.7450826533235));
#41938=CARTESIAN_POINT('Ctrl Pts',(18.8963694330047,8.07092809282087,39.685923146009));
#41939=CARTESIAN_POINT('Ctrl Pts',(18.7944358694665,8.06175352749629,39.6061961412275));
#41940=CARTESIAN_POINT('Ctrl Pts',(18.7776006583842,8.06022353483445,39.5925654362329));
#41941=CARTESIAN_POINT('Ctrl Pts',(18.7192075297478,8.05487279304149,39.5436363421388));
#41942=CARTESIAN_POINT('Ctrl Pts',(18.6789156492351,8.05109995361925,39.5068591291709));
#41943=CARTESIAN_POINT('Ctrl Pts',(18.6340826937053,8.04685641959878,39.462309668044));
#41944=CARTESIAN_POINT('Ctrl Pts',(18.627974052236,8.04627720477758,39.4561572640619));
#41945=CARTESIAN_POINT('Ctrl Pts',(18.6187839150898,8.04540454477022,39.4467756313335));
#41946=CARTESIAN_POINT('Ctrl Pts',(18.6156719075951,8.04510881847644,39.4435766475875));
#41947=CARTESIAN_POINT('Ctrl Pts',(18.6101012582495,8.04457910116072,39.4378104049483));
#41948=CARTESIAN_POINT('Ctrl Pts',(18.6076385976061,8.04434480321825,39.4352471373061));
#41949=CARTESIAN_POINT('Ctrl Pts',(18.6022842959842,8.04383513139112,39.4296431754841));
#41950=CARTESIAN_POINT('Ctrl Pts',(18.5993954931506,8.0435599738941,39.4265998566203));
#41951=CARTESIAN_POINT('Ctrl Pts',(18.5934540935229,8.04299363446229,39.4202996231858));
#41952=CARTESIAN_POINT('Ctrl Pts',(18.5904028217868,8.0427025517503,39.4170414868729));
#41953=CARTESIAN_POINT('Ctrl Pts',(18.5753938953932,8.04126941148954,39.4009031044856));
#41954=CARTESIAN_POINT('Ctrl Pts',(18.5636008577102,8.04013914778588,39.3878699458196));
#41955=CARTESIAN_POINT('Ctrl Pts',(18.5025906254496,8.03425795952168,39.3185632808165));
#41956=CARTESIAN_POINT('Ctrl Pts',(18.4564920560797,8.02969456057786,39.2596193255185));
#41957=CARTESIAN_POINT('Ctrl Pts',(18.3757199594956,8.02114917717964,39.1429582792398));
#41958=CARTESIAN_POINT('Ctrl Pts',(18.3404180853368,8.01716121659139,39.0858173054875));
#41959=CARTESIAN_POINT('Ctrl Pts',(18.2915384516555,8.01107235717915,38.9966042327989));
#41960=CARTESIAN_POINT('Ctrl Pts',(18.2757308962805,8.00899469787192,38.9658152121036));
#41961=CARTESIAN_POINT('Ctrl Pts',(18.2220739328013,8.0014922378881,38.8540008388833));
#41962=CARTESIAN_POINT('Ctrl Pts',(18.1890441956011,7.99598224010357,38.770801246144));
#41963=CARTESIAN_POINT('Ctrl Pts',(18.1578234815548,7.98941345427972,38.6728079897337));
#41964=CARTESIAN_POINT('Ctrl Pts',(18.1538762281101,7.98855056705286,38.6599556432484));
#41965=CARTESIAN_POINT('Ctrl Pts',(18.1477402884673,7.98715484762477,38.6392064968878));
#41966=CARTESIAN_POINT('Ctrl Pts',(18.1454669677096,7.98662475336065,38.6313350298936));
#41967=CARTESIAN_POINT('Ctrl Pts',(18.1415060026377,7.98567737467784,38.6172848736708));
#41968=CARTESIAN_POINT('Ctrl Pts',(18.1397988466497,7.98526072619015,38.6111117746514));
#41969=CARTESIAN_POINT('Ctrl Pts',(18.1362917067912,7.98438697452295,38.5981795655669));
#41970=CARTESIAN_POINT('Ctrl Pts',(18.1344976828263,7.98392968656042,38.5914189497571));
#41971=CARTESIAN_POINT('Ctrl Pts',(18.1309354455492,7.98300025366973,38.5776943280537));
#41972=CARTESIAN_POINT('Ctrl Pts',(18.1291692933754,7.98252805065453,38.5707299061581));
#41973=CARTESIAN_POINT('Ctrl Pts',(18.1249100047128,7.98136049873711,38.5535317092141));
#41974=CARTESIAN_POINT('Ctrl Pts',(18.1224617233113,7.98066373097216,38.543287168561));
#41975=CARTESIAN_POINT('Ctrl Pts',(18.1120907649617,7.97759554651792,38.4982632812398));
#41976=CARTESIAN_POINT('Ctrl Pts',(18.1050501308199,7.9751965587917,38.4632900088296));
#41977=CARTESIAN_POINT('Ctrl Pts',(18.0801736801999,7.96524177593111,38.3191745791166));
#41978=CARTESIAN_POINT('Ctrl Pts',(18.0707712265503,7.95744052614099,38.2088079959635));
#41979=CARTESIAN_POINT('Ctrl Pts',(18.0708707823177,7.94955924721526,38.0982626501526));
#41980=CARTESIAN_POINT('Ctrl Pts',(18.070870782374,7.94955924275848,38.0982625876404));
#41981=CARTESIAN_POINT('Ctrl Pts',(18.0709815859836,7.94078785002418,37.9752322203734));
#41982=CARTESIAN_POINT('Ctrl Pts',(18.0828614324957,7.93195349740318,37.852480327936));
#41983=CARTESIAN_POINT('Ctrl Pts',(18.1083340720369,7.92290448633068,37.7215163541891));
#41984=CARTESIAN_POINT('Ctrl Pts',(18.1103936426356,7.92220566482815,37.7113643372776));
#41985=CARTESIAN_POINT('Ctrl Pts',(18.1137385923834,7.92112046666037,37.695531997144));
#41986=CARTESIAN_POINT('Ctrl Pts',(18.1149680546044,7.9207312744099,37.6898402382882));
#41987=CARTESIAN_POINT('Ctrl Pts',(18.1173347732318,7.92000005993563,37.6791190339692));
#41988=CARTESIAN_POINT('Ctrl Pts',(18.1184664562775,7.91965774266281,37.6740884258275));
#41989=CARTESIAN_POINT('Ctrl Pts',(18.1204335044086,7.91907509552119,37.665505278738));
#41990=CARTESIAN_POINT('Ctrl Pts',(18.1212588003677,7.91883420057298,37.6619504824603));
#41991=CARTESIAN_POINT('Ctrl Pts',(18.1228667344757,7.91837165805236,37.6551127672726));
#41992=CARTESIAN_POINT('Ctrl Pts',(18.1236479023097,7.91814992555382,37.6518295499347));
#41993=CARTESIAN_POINT('Ctrl Pts',(18.1257579088503,7.91755883881139,37.6430634973561));
#41994=CARTESIAN_POINT('Ctrl Pts',(18.1271022020726,7.9171903587158,37.6375843599501));
#41995=CARTESIAN_POINT('Ctrl Pts',(18.1320638058245,7.91585894591206,37.6177382214434));
#41996=CARTESIAN_POINT('Ctrl Pts',(18.1358226627571,7.91490371288157,37.6034066692696));
#41997=CARTESIAN_POINT('Ctrl Pts',(18.1677708597934,7.90719006023246,37.4870747125593));
#41998=CARTESIAN_POINT('Ctrl Pts',(18.204148434913,7.90083385062824,37.3874943423854));
#41999=CARTESIAN_POINT('Ctrl Pts',(18.2747788486434,7.89075936218746,37.2345059042281));
#42000=CARTESIAN_POINT('Ctrl Pts',(18.3037960780335,7.88703051799953,37.1789353164767));
#42001=CARTESIAN_POINT('Ctrl Pts',(18.3703464451564,7.87910091362658,37.0653339632387));
#42002=CARTESIAN_POINT('Ctrl Pts',(18.4083945412223,7.87489590375913,37.0077109572764));
#42003=CARTESIAN_POINT('Ctrl Pts',(18.4722980810083,7.86818748609389,36.9213801304051));
#42004=CARTESIAN_POINT('Ctrl Pts',(18.496066448591,7.86575820966751,36.8911983184067));
#42005=CARTESIAN_POINT('Ctrl Pts',(18.526062526012,7.86275908758027,36.8553634287931));
#42006=CARTESIAN_POINT('Ctrl Pts',(18.5314476544807,7.8622231558329,36.8490140382238));
#42007=CARTESIAN_POINT('Ctrl Pts',(18.5419589338391,7.86118172943429,36.8367820114995));
#42008=CARTESIAN_POINT('Ctrl Pts',(18.5470800139676,7.86067644661945,36.8308952177528));
#42009=CARTESIAN_POINT('Ctrl Pts',(18.5564334103579,7.85975726225025,36.8202740986713));
#42010=CARTESIAN_POINT('Ctrl Pts',(18.5606536791342,7.85934386276858,36.8155292730992));
#42011=CARTESIAN_POINT('Ctrl Pts',(18.5697858202491,7.85845212863475,36.8053635766621));
#42012=CARTESIAN_POINT('Ctrl Pts',(18.5747052401864,7.85797348184289,36.7999496495272));
#42013=CARTESIAN_POINT('Ctrl Pts',(18.5880636521978,7.85667827707741,36.7854153878082));
#42014=CARTESIAN_POINT('Ctrl Pts',(18.5965600490139,7.85585929943949,36.7763485184464));
#42015=CARTESIAN_POINT('Ctrl Pts',(18.6378971595286,7.85189707292522,36.7330813624471));
#42016=CARTESIAN_POINT('Ctrl Pts',(18.6719011617202,7.8487039128033,36.7000201709512));
#42017=CARTESIAN_POINT('Ctrl Pts',(18.7301387446341,7.84333611582928,36.6474299537151));
#42018=CARTESIAN_POINT('Ctrl Pts',(18.7536898745625,7.84119086968474,36.6271733793763));
#42019=CARTESIAN_POINT('Ctrl Pts',(18.9079821399129,7.82730307682844,36.5008163217202));
#42020=CARTESIAN_POINT('Ctrl Pts',(19.0516332880843,7.81503465768568,36.4116623921454));
#42021=CARTESIAN_POINT('Ctrl Pts',(19.2395528954832,7.80071797318077,36.3266700539577));
#42022=CARTESIAN_POINT('Ctrl Pts',(19.2745400062806,7.79812364025917,36.3120718235531));
#42023=CARTESIAN_POINT('Ctrl Pts',(19.3168457914446,7.79508904265377,36.2958665195112));
#42024=CARTESIAN_POINT('Ctrl Pts',(19.3237696483125,7.7945956247834,36.2932598958635));
#42025=CARTESIAN_POINT('Ctrl Pts',(19.3346679505942,7.79382422757316,36.2892284396604));
#42026=CARTESIAN_POINT('Ctrl Pts',(19.3386322802388,7.79354471350728,36.2877767466987));
#42027=CARTESIAN_POINT('Ctrl Pts',(19.3459416611282,7.7930313897028,36.2851273131224));
#42028=CARTESIAN_POINT('Ctrl Pts',(19.3492852351804,7.79279736515268,36.2839258067258));
#42029=CARTESIAN_POINT('Ctrl Pts',(19.3568065837667,7.79227268620333,36.2812464644663));
#42030=CARTESIAN_POINT('Ctrl Pts',(19.3609861317343,7.79198233695981,36.2797737858068));
#42031=CARTESIAN_POINT('Ctrl Pts',(19.3716916238459,7.79124163933946,36.2760430852694));
#42032=CARTESIAN_POINT('Ctrl Pts',(19.378224752771,7.7907924682265,36.2738056544388));
#42033=CARTESIAN_POINT('Ctrl Pts',(19.3878786242408,7.79013273249309,36.2705572605874));
#42034=CARTESIAN_POINT('Ctrl Pts',(19.39099001264,7.78992071334236,36.2695191477629));
#42035=CARTESIAN_POINT('Ctrl Pts',(19.3941040087786,7.78970911166913,36.2684889831831));
#42036=CARTESIAN_POINT('Ctrl Pts',(19.3941039249488,7.61899517246903,36.2684890109154));
#42037=CARTESIAN_POINT('Ctrl Pts',(19.3586316938068,7.62156120579377,36.2802238493905));
#42038=CARTESIAN_POINT('Ctrl Pts',(19.3234998481385,7.62415666268337,36.2929893809385));
#42039=CARTESIAN_POINT('Ctrl Pts',(19.2536533155114,7.62942160838414,36.3206925556468));
#42040=CARTESIAN_POINT('Ctrl Pts',(19.2189711935278,7.63208971719421,36.3356411464752));
#42041=CARTESIAN_POINT('Ctrl Pts',(19.1080276902565,7.64078330005079,36.3873721080101));
#42042=CARTESIAN_POINT('Ctrl Pts',(19.0337426739678,7.64685795126209,36.428157996141));
#42043=CARTESIAN_POINT('Ctrl Pts',(18.9093149896807,7.6572940756148,36.5075457740809));
#42044=CARTESIAN_POINT('Ctrl Pts',(18.8579360495256,7.66168780432595,36.5439807747048));
#42045=CARTESIAN_POINT('Ctrl Pts',(18.7983702275426,7.66680670373622,36.5907644504401));
#42046=CARTESIAN_POINT('Ctrl Pts',(18.7883928458919,7.66766497629147,36.5987624506049));
#42047=CARTESIAN_POINT('Ctrl Pts',(18.7745043179933,7.66886002723209,36.6101243409625));
#42048=CARTESIAN_POINT('Ctrl Pts',(18.7705262813082,7.66920235989128,36.613405394005));
#42049=CARTESIAN_POINT('Ctrl Pts',(18.7637554521478,7.66978502475229,36.6190356883718));
#42050=CARTESIAN_POINT('Ctrl Pts',(18.7609560986321,7.67002592212201,36.6213769629307));
#42051=CARTESIAN_POINT('Ctrl Pts',(18.7555808061493,7.67048846268244,36.625898641239));
#42052=CARTESIAN_POINT('Ctrl Pts',(18.7530039367423,7.67071019083023,36.6280778673513));
#42053=CARTESIAN_POINT('Ctrl Pts',(18.7461349381336,7.6713012526505,36.6339178785816));
#42054=CARTESIAN_POINT('Ctrl Pts',(18.7418530840003,7.67166971230568,36.6375907823627));
#42055=CARTESIAN_POINT('Ctrl Pts',(18.7263862548942,7.67300097523286,36.6509761846395));
#42056=CARTESIAN_POINT('Ctrl Pts',(18.7152967846964,7.67395608107763,36.6607989473222));
#42057=CARTESIAN_POINT('Ctrl Pts',(18.6251393306581,7.68173694111128,36.7425306317676));
#42058=CARTESIAN_POINT('Ctrl Pts',(18.5520481770638,7.68815230300334,36.8207788541916));
#42059=CARTESIAN_POINT('Ctrl Pts',(18.4159511999036,7.70128268318915,36.9931833118541));
#42060=CARTESIAN_POINT('Ctrl Pts',(18.3539904536605,7.70797585021229,37.0876244435952));
#42061=CARTESIAN_POINT('Ctrl Pts',(18.2750831872183,7.71827010430045,37.2344837131553));
#42062=CARTESIAN_POINT('Ctrl Pts',(18.2515430873667,7.72165710710516,37.2830825954596));
#42063=CARTESIAN_POINT('Ctrl Pts',(18.2250909000193,7.72591730070476,37.344091871434));
#42064=CARTESIAN_POINT('Ctrl Pts',(18.2202209540419,7.72672333120259,37.3556305032966));
#42065=CARTESIAN_POINT('Ctrl Pts',(18.2127042285737,7.72800289084248,37.3739358428489));
#42066=CARTESIAN_POINT('Ctrl Pts',(18.2099826763191,7.72847390568883,37.3806716233918));
#42067=CARTESIAN_POINT('Ctrl Pts',(18.2049519463818,7.72935933247641,37.3933279221979));
#42068=CARTESIAN_POINT('Ctrl Pts',(18.202633844324,7.72977343937215,37.3992448065409));
#42069=CARTESIAN_POINT('Ctrl Pts',(18.1975102418428,7.73070263018082,37.4125153275659));
#42070=CARTESIAN_POINT('Ctrl Pts',(18.1947204374632,7.73121822794328,37.4198748636532));
#42071=CARTESIAN_POINT('Ctrl Pts',(18.1877595115763,7.73252968738326,37.4385824735616));
#42072=CARTESIAN_POINT('Ctrl Pts',(18.1836499420549,7.73332756563794,37.4499529340829));
#42073=CARTESIAN_POINT('Ctrl Pts',(18.1603220784099,7.73799863950985,37.5164457983572));
#42074=CARTESIAN_POINT('Ctrl Pts',(18.1435087566353,7.7419496297835,37.5723738041094));
#42075=CARTESIAN_POINT('Ctrl Pts',(18.0903790690229,7.75694828596013,37.783385047107));
#42076=CARTESIAN_POINT('Ctrl Pts',(18.0707712491718,7.76846792857911,37.9420078297301));
#42077=CARTESIAN_POINT('Ctrl Pts',(18.0708800060321,7.78078995297317,38.1166703550642));
#42078=CARTESIAN_POINT('Ctrl Pts',(18.071075702115,7.78187746815421,38.1321391168821));
#42079=CARTESIAN_POINT('Ctrl Pts',(18.072653583882,7.78635212033722,38.1960623733451));
#42080=CARTESIAN_POINT('Ctrl Pts',(18.0756758369737,7.78969441522575,38.2444631726518));
#42081=CARTESIAN_POINT('Ctrl Pts',(18.0812865879851,7.79346390897368,38.3003508899143));
#42082=CARTESIAN_POINT('Ctrl Pts',(18.0821001007524,7.79397747374924,38.3079942735344));
#42083=CARTESIAN_POINT('Ctrl Pts',(18.0834754118244,7.79479565010707,38.32022120739));
#42084=CARTESIAN_POINT('Ctrl Pts',(18.0840080104782,7.79510181208791,38.3248078611891));
#42085=CARTESIAN_POINT('Ctrl Pts',(18.0849823240584,7.79564346882633,38.3329434414558));
#42086=CARTESIAN_POINT('Ctrl Pts',(18.0854174451735,7.79587932591216,38.3364931027698));
#42087=CARTESIAN_POINT('Ctrl Pts',(18.0863650356692,7.79638037569987,38.3440493696792));
#42088=CARTESIAN_POINT('Ctrl Pts',(18.0868802171628,7.79664541514752,38.3480555760486));
#42089=CARTESIAN_POINT('Ctrl Pts',(18.0883171843531,7.79736517283325,38.358959051455));
#42090=CARTESIAN_POINT('Ctrl Pts',(18.0892637228852,7.7978185306423,38.3658530814156));
#42091=CARTESIAN_POINT('Ctrl Pts',(18.094351515473,7.80015301513959,38.4014780511042));
#42092=CARTESIAN_POINT('Ctrl Pts',(18.0991038068631,7.80200213014189,38.4301197436843));
#42093=CARTESIAN_POINT('Ctrl Pts',(18.1342044229316,7.81386158498889,38.6156323398797));
#42094=CARTESIAN_POINT('Ctrl Pts',(18.1832979986906,7.82311917516696,38.768338216969));
#42095=CARTESIAN_POINT('Ctrl Pts',(18.2897698010846,7.83837582605186,38.9973617608906));
#42096=CARTESIAN_POINT('Ctrl Pts',(18.3348804051058,7.84408195910548,39.0785288867973));
#42097=CARTESIAN_POINT('Ctrl Pts',(18.3930550783681,7.85086812418052,39.1674519173422));
#42098=CARTESIAN_POINT('Ctrl Pts',(18.4005801785246,7.85173631361516,39.1786944872048));
#42099=CARTESIAN_POINT('Ctrl Pts',(18.4128654067826,7.85313895276415,39.1966375303944));
#42100=CARTESIAN_POINT('Ctrl Pts',(18.4175512824989,7.85367062009236,39.2033884824034));
#42101=CARTESIAN_POINT('Ctrl Pts',(18.425967735118,7.85461979460738,39.2153501928541));
#42102=CARTESIAN_POINT('Ctrl Pts',(18.4296814340584,7.85503665717784,39.2205727211558));
#42103=CARTESIAN_POINT('Ctrl Pts',(18.4374957954657,7.85590981789656,39.2314468272025));
#42104=CARTESIAN_POINT('Ctrl Pts',(18.4416012516541,7.85636629565479,39.2370948293684));
#42105=CARTESIAN_POINT('Ctrl Pts',(18.4523983592904,7.85756103300159,39.2517804366233));
#42106=CARTESIAN_POINT('Ctrl Pts',(18.4591384530764,7.85830115601384,39.2607819333021));
#42107=CARTESIAN_POINT('Ctrl Pts',(18.4894422001682,7.8616042419708,39.3005240140847));
#42108=CARTESIAN_POINT('Ctrl Pts',(18.5138483705593,7.86419999990527,39.3306078757362));
#42109=CARTESIAN_POINT('Ctrl Pts',(18.5824484584771,7.87133338803641,39.4101476780712));
#42110=CARTESIAN_POINT('Ctrl Pts',(18.6283107099915,7.87593427760172,39.4580891900262));
#42111=CARTESIAN_POINT('Ctrl Pts',(18.7186366342435,7.88467530151629,39.5432592612499));
#42112=CARTESIAN_POINT('Ctrl Pts',(18.7624900067744,7.88879468224539,39.5810327149036));
#42113=CARTESIAN_POINT('Ctrl Pts',(18.8969708433063,7.90099844007742,39.6867205179527));
#42114=CARTESIAN_POINT('Ctrl Pts',(18.99196122443,7.90909339899043,39.7487019663138));
#42115=CARTESIAN_POINT('Ctrl Pts',(19.1048612870469,7.91776954821747,39.8089431905946));
#42116=CARTESIAN_POINT('Ctrl Pts',(19.117955106181,7.91876205689514,39.8157380283094));
#42117=CARTESIAN_POINT('Ctrl Pts',(19.1361541024514,7.92012138055456,39.8249187044733));
#42118=CARTESIAN_POINT('Ctrl Pts',(19.1411933111216,7.9204956565443,39.8274331665379));
#42119=CARTESIAN_POINT('Ctrl Pts',(19.1492681495525,7.92109193924984,39.8314182776021));
#42120=CARTESIAN_POINT('Ctrl Pts',(19.1522967017462,7.92131480723831,39.8329030705573));
#42121=CARTESIAN_POINT('Ctrl Pts',(19.1586114276241,7.92177786740126,39.8359784433282));
#42122=CARTESIAN_POINT('Ctrl Pts',(19.1618982350409,7.92201796843548,39.8375676439365));
#42123=CARTESIAN_POINT('Ctrl Pts',(19.1698452839241,7.92259632252402,39.8413823171334));
#42124=CARTESIAN_POINT('Ctrl Pts',(19.1745100335469,7.92293400319681,39.843598446847));
#42125=CARTESIAN_POINT('Ctrl Pts',(19.1907991679223,7.92410710027106,39.851257066921));
#42126=CARTESIAN_POINT('Ctrl Pts',(19.2024692353943,7.92493680597711,39.8566024029281));
#42127=CARTESIAN_POINT('Ctrl Pts',(19.2721028443825,7.92982910343991,39.8876602255865));
#42128=CARTESIAN_POINT('Ctrl Pts',(19.3312582818133,7.9337467355615,39.9106213284525));
#42129=CARTESIAN_POINT('Ctrl Pts',(19.47148912599,7.94272248606554,39.9572383341591));
#42130=CARTESIAN_POINT('Ctrl Pts',(19.5531966324928,7.94772282703611,39.9785701205641));
#42131=CARTESIAN_POINT('Ctrl Pts',(19.6731237878737,7.95503154128503,40.0016099584103));
#42132=CARTESIAN_POINT('Ctrl Pts',(19.7104075910097,7.957298930454,40.0076437328257));
#42133=CARTESIAN_POINT('Ctrl Pts',(19.8341072206104,7.96485470963064,40.0239524149944));
#42134=CARTESIAN_POINT('Ctrl Pts',(19.9210308904941,7.97022248919688,40.0294751262779));
#42135=CARTESIAN_POINT('Ctrl Pts',(20.0214033533959,7.97663386841754,40.0290576662761));
#42136=CARTESIAN_POINT('Ctrl Pts',(20.0347820945742,7.97749266036616,40.0288628190695));
#42137=CARTESIAN_POINT('Ctrl Pts',(20.0563289978584,7.97888303197086,40.0283247694685));
#42138=CARTESIAN_POINT('Ctrl Pts',(20.0644990494948,7.97941190778711,40.0280687855412));
#42139=CARTESIAN_POINT('Ctrl Pts',(20.0790647209291,7.98035789671796,40.0275197312065));
#42140=CARTESIAN_POINT('Ctrl Pts',(20.0854610112012,7.98077438061481,40.0272467299766));
#42141=CARTESIAN_POINT('Ctrl Pts',(20.0988519696126,7.98164859907185,40.0266083938286));
#42142=CARTESIAN_POINT('Ctrl Pts',(20.1058462318858,7.98210652246107,40.0262367943975));
#42143=CARTESIAN_POINT('Ctrl Pts',(20.1241621666118,7.98330919578944,40.0251636254735));
#42144=CARTESIAN_POINT('Ctrl Pts',(20.1354798124313,7.9840558550888,40.0244002805033));
#42145=CARTESIAN_POINT('Ctrl Pts',(20.1863934508014,7.98743107601014,40.0205149351695));
#42146=CARTESIAN_POINT('Ctrl Pts',(20.2258915623011,7.99009422285054,40.016270529701));
#42147=CARTESIAN_POINT('Ctrl Pts',(20.428295209575,8.00398280930177,39.9881760861714));
#42148=CARTESIAN_POINT('Ctrl Pts',(20.5877741696179,8.01581788385942,39.944762637889));
#42149=CARTESIAN_POINT('Ctrl Pts',(20.8135054934771,8.03317028334888,39.8510356739615));
#42150=CARTESIAN_POINT('Ctrl Pts',(20.8852804194693,8.03877112835411,39.8158667835322));
#42151=CARTESIAN_POINT('Ctrl Pts',(20.9627759903949,8.04476476583556,39.7717331820617));
#42152=CARTESIAN_POINT('Ctrl Pts',(20.970842355216,8.04538791678101,39.7670616573996));
#42153=CARTESIAN_POINT('Ctrl Pts',(20.9827837220664,8.04630899831782,39.7600299066897));
#42154=CARTESIAN_POINT('Ctrl Pts',(20.986684622988,8.04660966112339,39.7577142670757));
#42155=CARTESIAN_POINT('Ctrl Pts',(20.993631982281,8.04714467256645,39.7535569879711));
#42156=CARTESIAN_POINT('Ctrl Pts',(20.9966815374143,8.04737935561046,39.7517206611203));
#42157=CARTESIAN_POINT('Ctrl Pts',(21.0032674203887,8.04788582565731,39.7477300100116));
#42158=CARTESIAN_POINT('Ctrl Pts',(21.0068018924797,8.04815741798161,39.7455727430906));
#42159=CARTESIAN_POINT('Ctrl Pts',(21.0166512489848,8.04891372522387,39.7395175708778));
#42160=CARTESIAN_POINT('Ctrl Pts',(21.0229507122316,8.04939683769124,39.7355945316549));
#42161=CARTESIAN_POINT('Ctrl Pts',(21.0595614304736,8.05220195870442,39.7125006690888));
#42162=CARTESIAN_POINT('Ctrl Pts',(21.0893582392945,8.05447460043281,39.692522482486));
#42163=CARTESIAN_POINT('Ctrl Pts',(21.1856139593697,8.06184216656047,39.6240180700438));
#42164=CARTESIAN_POINT('Ctrl Pts',(21.2495304216564,8.06677915040896,39.5720691320599));
#42165=CARTESIAN_POINT('Ctrl Pts',(21.4212818959306,8.08076508786182,39.4132039033355));
#42166=CARTESIAN_POINT('Ctrl Pts',(21.5200776652444,8.08976415563604,39.2974574445647));
#42167=CARTESIAN_POINT('Ctrl Pts',(21.6164070899917,8.10075490971927,39.1532075792018));
#42168=CARTESIAN_POINT('Ctrl Pts',(21.6282086252709,8.10214726928203,39.1348694105022));
#42169=CARTESIAN_POINT('Ctrl Pts',(21.6441179568364,8.10409132906229,39.1092022282616));
#42170=CARTESIAN_POINT('Ctrl Pts',(21.6484928544548,8.10463329051996,39.1020400684056));
#42171=CARTESIAN_POINT('Ctrl Pts',(21.6559413258108,8.10556892853469,39.0896653460847));
#42172=CARTESIAN_POINT('Ctrl Pts',(21.6590373902036,8.1059617856487,39.0844664079044));
#42173=CARTESIAN_POINT('Ctrl Pts',(21.6653792077322,8.10677475001872,39.073702293791));
#42174=CARTESIAN_POINT('Ctrl Pts',(21.6686216409256,8.10719497027218,39.0681352592644));
#42175=CARTESIAN_POINT('Ctrl Pts',(21.6761207125708,8.10817765932373,39.0551102831739));
#42176=CARTESIAN_POINT('Ctrl Pts',(21.6803555339772,8.10874089877448,39.0476400010277));
#42177=CARTESIAN_POINT('Ctrl Pts',(21.6938420896868,8.11056186847124,39.0234748735027));
#42178=CARTESIAN_POINT('Ctrl Pts',(21.7028957352163,8.1118265626218,39.0066713503215));
#42179=CARTESIAN_POINT('Ctrl Pts',(21.7477794305653,8.11831976181454,38.920322950688));
#42180=CARTESIAN_POINT('Ctrl Pts',(21.7796001965999,8.12368480579476,38.8487877032886));
#42181=CARTESIAN_POINT('Ctrl Pts',(21.8362631412043,8.13501029869256,38.6972180849379));
#42182=CARTESIAN_POINT('Ctrl Pts',(21.8604150401814,8.14097504914594,38.6170938619879));
#42183=CARTESIAN_POINT('Ctrl Pts',(21.9040327012736,8.15475497030959,38.4289423079409));
#42184=CARTESIAN_POINT('Ctrl Pts',(21.9196403105624,8.16254911679998,38.3202963550283));
#42185=CARTESIAN_POINT('Ctrl Pts',(21.9264663620621,8.17052696431,38.2017539819836));
#42186=CARTESIAN_POINT('Ctrl Pts',(21.9269279537935,8.17113941799179,38.192602300432));
#42187=CARTESIAN_POINT('Ctrl Pts',(21.9275192005714,8.17204779903873,38.1789467100881));
#42188=CARTESIAN_POINT('Ctrl Pts',(21.9276983061123,8.17234635213509,38.1744452365181));
#42189=CARTESIAN_POINT('Ctrl Pts',(21.927990618872,8.17287908712782,38.1663881387808));
#42190=CARTESIAN_POINT('Ctrl Pts',(21.9281097611104,8.17311359170593,38.162832803767));
#42191=CARTESIAN_POINT('Ctrl Pts',(21.9283470078961,8.17362136722873,38.1551154215447));
#42192=CARTESIAN_POINT('Ctrl Pts',(21.9284614727892,8.17389443445415,38.1509533250296));
#42193=CARTESIAN_POINT('Ctrl Pts',(21.928745006828,8.17465903431459,38.1392669975236));
#42194=CARTESIAN_POINT('Ctrl Pts',(21.9288835238361,8.17514890713363,38.1317419985071));
#42195=CARTESIAN_POINT('Ctrl Pts',(21.9294509794553,8.17807772840586,38.0865405224694));
#42196=CARTESIAN_POINT('Ctrl Pts',(21.9288201015081,8.18046208516254,38.0488559683224));
#42197=CARTESIAN_POINT('Ctrl Pts',(21.9194747838983,8.19310159733426,37.8460238356851));
#42198=CARTESIAN_POINT('Ctrl Pts',(21.8906565594837,8.202652775606,37.682488463203));
#42199=CARTESIAN_POINT('Ctrl Pts',(21.8179856199345,8.21747001524946,37.4499270471553));
#42200=CARTESIAN_POINT('Ctrl Pts',(21.7901244959107,8.22231803728569,37.3767306128295));
#42201=CARTESIAN_POINT('Ctrl Pts',(21.7524950502558,8.22815578990775,37.2934792233196));
#42202=CARTESIAN_POINT('Ctrl Pts',(21.7469699397382,8.22899804480771,37.2815803763392));
#42203=CARTESIAN_POINT('Ctrl Pts',(21.7378016523831,8.23037245836208,37.2623515319013));
#42204=CARTESIAN_POINT('Ctrl Pts',(21.7342323682332,8.23090208269006,37.254986610337));
#42205=CARTESIAN_POINT('Ctrl Pts',(21.7277948721757,8.23184784116408,37.2419159621177));
#42206=CARTESIAN_POINT('Ctrl Pts',(21.7249449730744,8.23226333695332,37.2362013112899));
#42207=CARTESIAN_POINT('Ctrl Pts',(21.7188803620385,8.23314090484524,37.2241901820371));
#42208=CARTESIAN_POINT('Ctrl Pts',(21.7156593130333,8.2336031929943,37.2178970266403));
#42209=CARTESIAN_POINT('Ctrl Pts',(21.7070437825133,8.23482981514142,37.2012900603284));
#42210=CARTESIAN_POINT('Ctrl Pts',(21.7015904915591,8.23559619972432,37.1910072497079));
#42211=CARTESIAN_POINT('Ctrl Pts',(21.6756244452469,8.23919979743906,37.1430978116501));
#42212=CARTESIAN_POINT('Ctrl Pts',(21.6539560314363,8.24207760377928,37.1061146783885));
#42213=CARTESIAN_POINT('Ctrl Pts',(21.5421081887488,8.25634853445262,36.9290155501603));
#42214=CARTESIAN_POINT('Ctrl Pts',(21.4352743836774,8.26835428211553,36.8002800804146));
#42215=CARTESIAN_POINT('Ctrl Pts',(21.2915027350888,8.28226363717272,36.6666660701462));
#42216=CARTESIAN_POINT('Ctrl Pts',(21.2692718390209,8.28435854278109,36.6469430187106));
#42217=CARTESIAN_POINT('Ctrl Pts',(21.2115692145182,8.28964055618312,36.5980849692795));
#42218=CARTESIAN_POINT('Ctrl Pts',(21.1754944732726,8.29279999932842,36.5696855723567));
#42219=CARTESIAN_POINT('Ctrl Pts',(21.1323217570056,8.29638805205321,36.538126961166));
#42220=CARTESIAN_POINT('Ctrl Pts',(21.1261792834721,8.29689414749572,36.5336921832167));
#42221=CARTESIAN_POINT('Ctrl Pts',(21.1162776361748,8.29770272955752,36.5266316967654));
#42222=CARTESIAN_POINT('Ctrl Pts',(21.1125350248994,8.29800671088129,36.5239830590709));
#42223=CARTESIAN_POINT('Ctrl Pts',(21.1058597288791,8.29854591831643,36.5192945949083));
#42224=CARTESIAN_POINT('Ctrl Pts',(21.1029307831459,8.29878149496404,36.51724954398));
#42225=CARTESIAN_POINT('Ctrl Pts',(21.0966618492847,8.29928353469675,36.5128982961346));
#42226=CARTESIAN_POINT('Ctrl Pts',(21.0933202644203,8.29954983636275,36.5105945041466));
#42227=CARTESIAN_POINT('Ctrl Pts',(21.0841569342351,8.30027660235733,36.5043195932789));
#42228=CARTESIAN_POINT('Ctrl Pts',(21.0783205894319,8.30073566119903,36.5003697525375));
#42229=CARTESIAN_POINT('Ctrl Pts',(21.0473497758358,8.30315221743393,36.4796562858718));
#42230=CARTESIAN_POINT('Ctrl Pts',(21.0218441318058,8.30507496225765,36.46345176615));
#42231=CARTESIAN_POINT('Ctrl Pts',(20.857311029446,8.31712672377891,36.3642660455556));
#42232=CARTESIAN_POINT('Ctrl Pts',(20.7086709131394,8.32649664374638,36.2984583172808));
#42233=CARTESIAN_POINT('Ctrl Pts',(20.4678683178965,8.34170282012976,36.2263297539923));
#42234=CARTESIAN_POINT('Ctrl Pts',(20.3805252277703,8.34721367131673,36.2066594666256));
#42235=CARTESIAN_POINT('Ctrl Pts',(20.2788501727,8.35378340003351,36.1910825296478));
#42236=CARTESIAN_POINT('Ctrl Pts',(20.2655394972315,8.35464630896633,36.1891854909047));
#42237=CARTESIAN_POINT('Ctrl Pts',(20.2440873889443,8.35604205597547,36.1863566075999));
#42238=CARTESIAN_POINT('Ctrl Pts',(20.2359577965741,8.35657215592866,36.1853372094417));
#42239=CARTESIAN_POINT('Ctrl Pts',(20.2214620496584,8.35751954013853,36.1836132594661));
#42240=CARTESIAN_POINT('Ctrl Pts',(20.2150983777735,8.35793618842828,36.1828885621943));
#42241=CARTESIAN_POINT('Ctrl Pts',(20.2017777893657,8.35880993490592,36.1814387671002));
#42242=CARTESIAN_POINT('Ctrl Pts',(20.1948203139704,8.35926721785211,36.1807197901899));
#42243=CARTESIAN_POINT('Ctrl Pts',(20.1766129680696,8.36046637585641,36.1789382872848));
#42244=CARTESIAN_POINT('Ctrl Pts',(20.1653575338497,8.36121013987433,36.177936754066));
#42245=CARTESIAN_POINT('Ctrl Pts',(20.1174891358582,8.36438422576868,36.1741008876191));
#42246=CARTESIAN_POINT('Ctrl Pts',(20.080810120225,8.36684368675126,36.1722135749258));
#42247=CARTESIAN_POINT('Ctrl Pts',(19.981685618553,8.37356887418159,36.1699469091807));
#42248=CARTESIAN_POINT('Ctrl Pts',(19.9192430039199,8.37789058335963,36.1715505362774));
#42249=CARTESIAN_POINT('Ctrl Pts',(19.6994584290954,8.39337083360433,36.1878881812139));
#42250=CARTESIAN_POINT('Ctrl Pts',(19.5440037610217,8.40486352406218,36.2188995139984));
#42251=CARTESIAN_POINT('Ctrl Pts',(19.3941040078119,8.41575742730426,36.2684889835028));
#42252=CARTESIAN_POINT('Origin',(20.,-1.3495818343519,38.1));
#42253=CARTESIAN_POINT('',(19.3941040511559,9.38044738890627,36.2684889691639));
#42254=CARTESIAN_POINT('',(19.3941038390373,9.20793124499895,36.2684890393365));
#42255=CARTESIAN_POINT('',(19.3941040087494,-1.3495818343519,36.2684889831927));
#42256=CARTESIAN_POINT('Ctrl Pts',(19.3941040511559,9.38044738890628,36.2684889691639));
#42257=CARTESIAN_POINT('Ctrl Pts',(19.4244038591954,9.37846238576415,36.2584652616171));
#42258=CARTESIAN_POINT('Ctrl Pts',(19.4549533095265,9.37645671543785,36.2491931539581));
#42259=CARTESIAN_POINT('Ctrl Pts',(19.5040072665787,9.37322083091372,36.2356251480271));
#42260=CARTESIAN_POINT('Ctrl Pts',(19.5223628701376,9.37200664483843,36.2308383933716));
#42261=CARTESIAN_POINT('Ctrl Pts',(19.5491051150438,9.37023160205265,36.2242842080849));
#42262=CARTESIAN_POINT('Ctrl Pts',(19.5574380363418,9.36967764525106,36.2223006540568));
#42263=CARTESIAN_POINT('Ctrl Pts',(19.5720576898282,9.36870415186853,36.2189233405878));
#42264=CARTESIAN_POINT('Ctrl Pts',(19.5783387501935,9.36828539133833,36.2175054294475));
#42265=CARTESIAN_POINT('Ctrl Pts',(19.590541821096,9.36747075547413,36.2148147979837));
#42266=CARTESIAN_POINT('Ctrl Pts',(19.5964629656583,9.36707500033364,36.2135384693337));
#42267=CARTESIAN_POINT('Ctrl Pts',(19.610625294456,9.36612723328662,36.2105554453514));
#42268=CARTESIAN_POINT('Ctrl Pts',(19.6188717728155,9.36557440345402,36.2088747643098));
#42269=CARTESIAN_POINT('Ctrl Pts',(19.648670885457,9.3635730919338,36.2030043548024));
#42270=CARTESIAN_POINT('Ctrl Pts',(19.6702829845787,9.36211475933806,36.1991288189235));
#42271=CARTESIAN_POINT('Ctrl Pts',(19.8388999266286,9.35067924359567,36.1718540324525));
#42272=CARTESIAN_POINT('Ctrl Pts',(19.9880738755674,9.34016418351602,36.165176695416));
#42273=CARTESIAN_POINT('Ctrl Pts',(20.2206175186628,9.32352888107175,36.1816720874378));
#42274=CARTESIAN_POINT('Ctrl Pts',(20.3042592883843,9.31750923899284,36.1931486498103));
#42275=CARTESIAN_POINT('Ctrl Pts',(20.4225175357811,9.30914071088895,36.2173570928217));
#42276=CARTESIAN_POINT('Ctrl Pts',(20.457938823403,9.30665359955468,36.2256580252604));
#42277=CARTESIAN_POINT('Ctrl Pts',(20.5003102661593,9.3037185581774,36.2368607913251));
#42278=CARTESIAN_POINT('Ctrl Pts',(20.5075027295189,9.30322175072343,36.2388070875614));
#42279=CARTESIAN_POINT('Ctrl Pts',(20.5186808416477,9.30245203076062,36.2419015253712));
#42280=CARTESIAN_POINT('Ctrl Pts',(20.5226742729832,9.30217752115653,36.2430209042437));
#42281=CARTESIAN_POINT('Ctrl Pts',(20.5300879647477,9.30166882767936,36.2451248092114));
#42282=CARTESIAN_POINT('Ctrl Pts',(20.5335090794663,9.30143445836815,36.2461059128876));
#42283=CARTESIAN_POINT('Ctrl Pts',(20.5412759195961,9.30090320582331,36.2483565592067));
#42284=CARTESIAN_POINT('Ctrl Pts',(20.545619896105,9.30060666298822,36.2496319331079));
#42285=CARTESIAN_POINT('Ctrl Pts',(20.5588495816369,9.29970520746404,36.2535667548162));
#42286=CARTESIAN_POINT('Ctrl Pts',(20.5677207967211,9.29910303843171,36.2562750505778));
#42287=CARTESIAN_POINT('Ctrl Pts',(20.6473669768653,9.29371462932592,36.2812196266964));
#42288=CARTESIAN_POINT('Ctrl Pts',(20.7168330279982,9.2891415070555,36.3074601151395));
#42289=CARTESIAN_POINT('Ctrl Pts',(20.9367400680525,9.27456410133199,36.405365234781));
#42290=CARTESIAN_POINT('Ctrl Pts',(21.0794427766388,9.26488110398889,36.4924947714893));
#42291=CARTESIAN_POINT('Ctrl Pts',(21.2426534575564,9.2518435705921,36.6237887336634));
#42292=CARTESIAN_POINT('Ctrl Pts',(21.2752090120273,9.24913342488915,36.6518187763585));
#42293=CARTESIAN_POINT('Ctrl Pts',(21.3153687305914,9.24563158594843,36.6888007450324));
#42294=CARTESIAN_POINT('Ctrl Pts',(21.3238653920219,9.24488126087871,36.6967684977933));
#42295=CARTESIAN_POINT('Ctrl Pts',(21.3374035244911,9.2436701501548,36.7096963006409));
#42296=CARTESIAN_POINT('Ctrl Pts',(21.3424908719135,9.24321143582419,36.7146080625331));
#42297=CARTESIAN_POINT('Ctrl Pts',(21.3521203777699,9.24233620254087,36.724008061369));
#42298=CARTESIAN_POINT('Ctrl Pts',(21.3566674914402,9.2419199122914,36.7284911056837));
#42299=CARTESIAN_POINT('Ctrl Pts',(21.366989178197,9.24096802738791,36.7387689145601));
#42300=CARTESIAN_POINT('Ctrl Pts',(21.3727492850227,9.24043180846375,36.7445779704189));
#42301=CARTESIAN_POINT('Ctrl Pts',(21.3876417101336,9.2390322069458,36.7597892553047));
#42302=CARTESIAN_POINT('Ctrl Pts',(21.3967153372187,9.2381663134145,36.769248104141));
#42303=CARTESIAN_POINT('Ctrl Pts',(21.4590011949815,9.23212919639442,36.8355171112266));
#42304=CARTESIAN_POINT('Ctrl Pts',(21.5088220041314,9.2268169889976,36.895402637748));
#42305=CARTESIAN_POINT('Ctrl Pts',(21.6530198036651,9.20982806213482,37.0917562660446));
#42306=CARTESIAN_POINT('Ctrl Pts',(21.7335086258486,9.19775235637622,37.2374626824317));
#42307=CARTESIAN_POINT('Ctrl Pts',(21.8082255479244,9.1836298125289,37.426735314335));
#42308=CARTESIAN_POINT('Ctrl Pts',(21.8210432808862,9.1810485131656,37.4622172763466));
#42309=CARTESIAN_POINT('Ctrl Pts',(21.8351623376683,9.17801777970067,37.5052072430586));
#42310=CARTESIAN_POINT('Ctrl Pts',(21.8374694895923,9.17751576643795,37.5123733253891));
#42311=CARTESIAN_POINT('Ctrl Pts',(21.8409875851325,9.17673975402923,37.5235239747351));
#42312=CARTESIAN_POINT('Ctrl Pts',(21.8422276448457,9.1764641162977,37.5274991688242));
#42313=CARTESIAN_POINT('Ctrl Pts',(21.8445031930614,9.1759544020594,37.5348777280876));
#42314=CARTESIAN_POINT('Ctrl Pts',(21.8455421306458,9.17572013343907,37.5382799133167));
#42315=CARTESIAN_POINT('Ctrl Pts',(21.8478753063466,9.17519046685254,37.5459966619202));
#42316=CARTESIAN_POINT('Ctrl Pts',(21.8491638452499,9.17489540090658,37.5503128882292));
#42317=CARTESIAN_POINT('Ctrl Pts',(21.8530268222574,9.17400287539873,37.5634200345114));
#42318=CARTESIAN_POINT('Ctrl Pts',(21.8555538227229,9.17340808067707,37.5722249699103));
#42319=CARTESIAN_POINT('Ctrl Pts',(21.8875096341518,9.1657370155284,37.6866371891619));
#42320=CARTESIAN_POINT('Ctrl Pts',(21.9079514847886,9.15913142827709,37.7945658202078));
#42321=CARTESIAN_POINT('Ctrl Pts',(21.9276361675249,9.14755927770369,37.9869735489237));
#42322=CARTESIAN_POINT('Ctrl Pts',(21.9307253218687,9.14258709039382,38.0707517429598));
#42323=CARTESIAN_POINT('Ctrl Pts',(21.926157940346,9.1327796939752,38.2324680106435));
#42324=CARTESIAN_POINT('Ctrl Pts',(21.9192241078182,9.12796760679228,38.3102591182425));
#42325=CARTESIAN_POINT('Ctrl Pts',(21.9047600020269,9.12179572070304,38.4062601017254));
#42326=CARTESIAN_POINT('Ctrl Pts',(21.9016409252653,9.120575668573,38.4250656321996));
#42327=CARTESIAN_POINT('Ctrl Pts',(21.8967141269301,9.11879360499452,38.4522665745052));
#42328=CARTESIAN_POINT('Ctrl Pts',(21.8951281530765,9.11823857150069,38.4607013977202));
#42329=CARTESIAN_POINT('Ctrl Pts',(21.8922533776101,9.1172638313924,38.4754480103079));
#42330=CARTESIAN_POINT('Ctrl Pts',(21.8909891383856,9.11684490698925,38.4817644959315));
#42331=CARTESIAN_POINT('Ctrl Pts',(21.8884757795538,9.11603042943014,38.4940030679972));
#42332=CARTESIAN_POINT('Ctrl Pts',(21.8872303786607,9.11563499870301,38.4999258481425));
#42333=CARTESIAN_POINT('Ctrl Pts',(21.8841904883848,9.11468877732292,38.5140522670446));
#42334=CARTESIAN_POINT('Ctrl Pts',(21.882370275238,9.11413717478833,38.5222501859118));
#42335=CARTESIAN_POINT('Ctrl Pts',(21.8756240450917,9.11214493212019,38.5517232489689));
#42336=CARTESIAN_POINT('Ctrl Pts',(21.8703905377779,9.11069455722079,38.5729255989421));
#42337=CARTESIAN_POINT('Ctrl Pts',(21.826096309839,9.09911620725388,38.7401202359833));
#42338=CARTESIAN_POINT('Ctrl Pts',(21.7703692472354,9.08843182462655,38.8811254707893));
#42339=CARTESIAN_POINT('Ctrl Pts',(21.6596033282708,9.07175209988574,39.0869626119126));
#42340=CARTESIAN_POINT('Ctrl Pts',(21.6157816893467,9.0658541105387,39.1571800352473));
#42341=CARTESIAN_POINT('Ctrl Pts',(21.5466253219692,9.05763089955311,39.2535970458031));
#42342=CARTESIAN_POINT('Ctrl Pts',(21.5248487100224,9.0551721954122,39.2822321471084));
#42343=CARTESIAN_POINT('Ctrl Pts',(21.497623200754,9.05226608806357,39.316027328985));
#42344=CARTESIAN_POINT('Ctrl Pts',(21.4929304428478,9.05177089933937,39.3217841108422));
#42345=CARTESIAN_POINT('Ctrl Pts',(21.4855688499592,9.05100313685232,39.3307091068223));
#42346=CARTESIAN_POINT('Ctrl Pts',(21.4829229222756,9.05072897880338,39.3338959927707));
#42347=CARTESIAN_POINT('Ctrl Pts',(21.4779840634496,9.05022060045816,39.3398057654878));
#42348=CARTESIAN_POINT('Ctrl Pts',(21.4756938816787,9.04998619681082,39.3425308027766));
#42349=CARTESIAN_POINT('Ctrl Pts',(21.4704690700792,9.04945443661566,39.3487128704998));
#42350=CARTESIAN_POINT('Ctrl Pts',(21.4675297905048,9.04915742313382,39.3521658971675));
#42351=CARTESIAN_POINT('Ctrl Pts',(21.4585175207047,9.04825311159094,39.3626780705615));
#42352=CARTESIAN_POINT('Ctrl Pts',(21.4524054609673,9.04764858263776,39.3697037660274));
#42353=CARTESIAN_POINT('Ctrl Pts',(21.3940139908399,9.04195253499656,39.4358502518299));
#42354=CARTESIAN_POINT('Ctrl Pts',(21.3381967541865,9.03710260876241,39.4917627707013));
#42355=CARTESIAN_POINT('Ctrl Pts',(21.1960911101685,9.02563331058928,39.6176317108342));
#42356=CARTESIAN_POINT('Ctrl Pts',(21.10689339749,9.01910525917784,39.6838647883179));
#42357=CARTESIAN_POINT('Ctrl Pts',(20.943689398834,9.00749882551336,39.7844962620863));
#42358=CARTESIAN_POINT('Ctrl Pts',(20.8722891876929,9.00252171477326,39.8225523536512));
#42359=CARTESIAN_POINT('Ctrl Pts',(20.7810406904025,8.99615139195069,39.8640564463471));
#42360=CARTESIAN_POINT('Ctrl Pts',(20.7632432124232,8.99490872858356,39.8718294108));
#42361=CARTESIAN_POINT('Ctrl Pts',(20.7373561356301,8.9930996289828,39.8826730662276));
#42362=CARTESIAN_POINT('Ctrl Pts',(20.7293580857635,8.99254047558438,39.8859602768648));
#42363=CARTESIAN_POINT('Ctrl Pts',(20.7153542311147,8.99156095217925,39.8916061259698));
#42364=CARTESIAN_POINT('Ctrl Pts',(20.7093581465315,8.99114138802137,39.8939886300791));
#42365=CARTESIAN_POINT('Ctrl Pts',(20.6977312563621,8.99032746428574,39.8985410934219));
#42366=CARTESIAN_POINT('Ctrl Pts',(20.6921019921489,8.98993323556966,39.9007148030457));
#42367=CARTESIAN_POINT('Ctrl Pts',(20.6786789094188,8.98899276374748,39.905825812679));
#42368=CARTESIAN_POINT('Ctrl Pts',(20.6708761364911,8.9884457311628,39.9087391004906));
#42369=CARTESIAN_POINT('Ctrl Pts',(20.6429493512222,8.98648648253201,39.9189604366463));
#42370=CARTESIAN_POINT('Ctrl Pts',(20.6227234672199,8.98506494653042,39.9259836689474));
#42371=CARTESIAN_POINT('Ctrl Pts',(20.4526192343711,8.97308376293558,39.9818957594698));
#42372=CARTESIAN_POINT('Ctrl Pts',(20.2974113932982,8.96191218739062,40.0125696590943));
#42373=CARTESIAN_POINT('Ctrl Pts',(20.0623679540216,8.94509792303987,40.0297018606919));
#42374=CARTESIAN_POINT('Ctrl Pts',(19.9842165924889,8.9395385470095,40.0306453615445));
#42375=CARTESIAN_POINT('Ctrl Pts',(19.8714624720214,8.93172264803946,40.0251575319472));
#42376=CARTESIAN_POINT('Ctrl Pts',(19.8367555490695,8.92934560012076,40.0225256929755));
#42377=CARTESIAN_POINT('Ctrl Pts',(19.7948191062741,8.92652285876029,40.0182016234981));
#42378=CARTESIAN_POINT('Ctrl Pts',(19.7875061362813,8.92603245473581,40.0174052857218));
#42379=CARTESIAN_POINT('Ctrl Pts',(19.7760980460962,8.92527048055544,40.0160969444762));
#42380=CARTESIAN_POINT('Ctrl Pts',(19.7719998068556,8.92499736372034,40.015613608824));
#42381=CARTESIAN_POINT('Ctrl Pts',(19.7643674621382,8.92448991011912,40.0146886296104));
#42382=CARTESIAN_POINT('Ctrl Pts',(19.760833063402,8.92425539620444,40.0142503540567));
#42383=CARTESIAN_POINT('Ctrl Pts',(19.7527794119199,8.92372209355355,40.013229024536));
#42384=CARTESIAN_POINT('Ctrl Pts',(19.748261004609,8.92342365594821,40.0126397462013));
#42385=CARTESIAN_POINT('Ctrl Pts',(19.7364926377775,8.92264826019279,40.0110625221561));
#42386=CARTESIAN_POINT('Ctrl Pts',(19.7292460535279,8.92217267375755,40.0100493182461));
#42387=CARTESIAN_POINT('Ctrl Pts',(19.681701635306,8.91906367903118,40.0031257283683));
#42388=CARTESIAN_POINT('Ctrl Pts',(19.6415905066323,8.91649406947823,39.9959811663601));
#42389=CARTESIAN_POINT('Ctrl Pts',(19.5921586802583,8.91336033079535,39.9855513124973));
#42390=CARTESIAN_POINT('Ctrl Pts',(19.5826002870814,8.91275592212322,39.9834584623849));
#42391=CARTESIAN_POINT('Ctrl Pts',(19.4397828752035,8.90374282818457,39.9510473811516));
#42392=CARTESIAN_POINT('Ctrl Pts',(19.3100921994943,8.89576331158421,39.9067240423076));
#42393=CARTESIAN_POINT('Ctrl Pts',(19.1297083245816,8.88374270018395,39.822792157683));
#42394=CARTESIAN_POINT('Ctrl Pts',(19.0745576891679,8.8799343561846,39.7938051795173));
#42395=CARTESIAN_POINT('Ctrl Pts',(18.9889509952811,8.87372177197631,39.7433800751516));
#42396=CARTESIAN_POINT('Ctrl Pts',(18.9575450559463,8.87137413994948,39.7236396039021));
#42397=CARTESIAN_POINT('Ctrl Pts',(18.9175255030823,8.868282332471,39.696845076736));
#42398=CARTESIAN_POINT('Ctrl Pts',(18.9083752869649,8.86756840773729,39.6906038831658));
#42399=CARTESIAN_POINT('Ctrl Pts',(18.8935758024318,8.86640200055295,39.6803215771954));
#42400=CARTESIAN_POINT('Ctrl Pts',(18.8878936333849,8.86595131912475,39.6763280811934));
#42401=CARTESIAN_POINT('Ctrl Pts',(18.8770006502491,8.86508177814535,39.668584149672));
#42402=CARTESIAN_POINT('Ctrl Pts',(18.8717867424945,8.86466309383263,39.6648382082713));
#42403=CARTESIAN_POINT('Ctrl Pts',(18.8598775001756,8.86370100407859,39.6561915326735));
#42404=CARTESIAN_POINT('Ctrl Pts',(18.8531949277063,8.86315693883525,39.6512735166657));
#42405=CARTESIAN_POINT('Ctrl Pts',(18.8354836532283,8.86170357276788,39.6380619777819));
#42406=CARTESIAN_POINT('Ctrl Pts',(18.8245120238657,8.86079136091972,39.6296930968732));
#42407=CARTESIAN_POINT('Ctrl Pts',(18.7298754388197,8.85281728693721,39.5558873317374));
#42408=CARTESIAN_POINT('Ctrl Pts',(18.6516716104444,8.84548606823654,39.4837731137147));
#42409=CARTESIAN_POINT('Ctrl Pts',(18.568921918506,8.83685000721198,39.3937607319565));
#42410=CARTESIAN_POINT('Ctrl Pts',(18.5581840611404,8.83571065882233,39.381783169043));
#42411=CARTESIAN_POINT('Ctrl Pts',(18.4991291495343,8.82934148227517,39.3142291477083));
#42412=CARTESIAN_POINT('Ctrl Pts',(18.4538760987799,8.82406482873878,39.2560564159517));
#42413=CARTESIAN_POINT('Ctrl Pts',(18.369825225448,8.81355272452002,39.1342169669674));
#42414=CARTESIAN_POINT('Ctrl Pts',(18.331161947731,8.80832711214604,39.07059594045));
#42415=CARTESIAN_POINT('Ctrl Pts',(18.2897378853471,8.80234892868185,38.9926028038602));
#42416=CARTESIAN_POINT('Ctrl Pts',(18.2833423872953,8.80141363314989,38.9802402708871));
#42417=CARTESIAN_POINT('Ctrl Pts',(18.2746817378842,8.80013077599138,38.9630457105301));
#42418=CARTESIAN_POINT('Ctrl Pts',(18.2723021807264,8.7997765373723,38.9582722476042));
#42419=CARTESIAN_POINT('Ctrl Pts',(18.2683126910433,8.79917969634672,38.9501853857593));
#42420=CARTESIAN_POINT('Ctrl Pts',(18.2666924084319,8.79893646156411,38.9468771575315));
#42421=CARTESIAN_POINT('Ctrl Pts',(18.2636225012257,8.79847403793311,38.9405634256781));
#42422=CARTESIAN_POINT('Ctrl Pts',(18.2621711889263,8.79825474225271,38.9375587828101));
#42423=CARTESIAN_POINT('Ctrl Pts',(18.2583735829543,8.79767907212881,38.9296442562446));
#42424=CARTESIAN_POINT('Ctrl Pts',(18.2560402339743,8.79732348947124,38.9247281398847));
#42425=CARTESIAN_POINT('Ctrl Pts',(18.2479539520215,8.79608436302568,38.9075034345863));
#42426=CARTESIAN_POINT('Ctrl Pts',(18.2423101114116,8.79520719849086,38.8951436548102));
#42427=CARTESIAN_POINT('Ctrl Pts',(18.1799165613098,8.78535596336925,38.7545930070958));
#42428=CARTESIAN_POINT('Ctrl Pts',(18.1371632352496,8.77710197449362,38.6206219757629));
#42429=CARTESIAN_POINT('Ctrl Pts',(18.0837672653261,8.76102929922204,38.3571566361323));
#42430=CARTESIAN_POINT('Ctrl Pts',(18.0708933042763,8.75326579097362,38.2289117854329));
#42431=CARTESIAN_POINT('Ctrl Pts',(18.0708670590945,8.74402192427518,38.0839284960393));
#42432=CARTESIAN_POINT('Ctrl Pts',(18.0710737457995,8.7429687848692,38.0675088299204));
#42433=CARTESIAN_POINT('Ctrl Pts',(18.0716948983203,8.74138762033962,38.0430148267056));
#42434=CARTESIAN_POINT('Ctrl Pts',(18.0719505535161,8.74086452035167,38.0349369245966));
#42435=CARTESIAN_POINT('Ctrl Pts',(18.0724986235123,8.73992602230705,38.0204913121164));
#42436=CARTESIAN_POINT('Ctrl Pts',(18.0727718557725,8.73951122603781,38.0141229583419));
#42437=CARTESIAN_POINT('Ctrl Pts',(18.0734174500292,8.73863052621088,38.0006368505826));
#42438=CARTESIAN_POINT('Ctrl Pts',(18.0737977061702,8.73816438323541,37.9935195873927));
#42439=CARTESIAN_POINT('Ctrl Pts',(18.0749181598952,8.73691660500432,37.9745245250183));
#42440=CARTESIAN_POINT('Ctrl Pts',(18.0757288334513,8.73613279111056,37.9626513458907));
#42441=CARTESIAN_POINT('Ctrl Pts',(18.0801953071342,8.73231274178848,37.9050787814133));
#42442=CARTESIAN_POINT('Ctrl Pts',(18.0853692480883,8.72922973673812,37.8595154430513));
#42443=CARTESIAN_POINT('Ctrl Pts',(18.1164982500365,8.71488274826938,37.6517283940498));
#42444=CARTESIAN_POINT('Ctrl Pts',(18.1614846170246,8.70304011542222,37.4930642508039));
#42445=CARTESIAN_POINT('Ctrl Pts',(18.2367485133002,8.68947005300853,37.3169070974939));
#42446=CARTESIAN_POINT('Ctrl Pts',(18.2480259964632,8.68754241184183,37.2919916546102));
#42447=CARTESIAN_POINT('Ctrl Pts',(18.2621790961266,8.68525000917455,37.2624137719484));
#42448=CARTESIAN_POINT('Ctrl Pts',(18.2645492727808,8.68487011077749,37.2575138234003));
#42449=CARTESIAN_POINT('Ctrl Pts',(18.2853959830184,8.6815637120522,37.2148779769429));
#42450=CARTESIAN_POINT('Ctrl Pts',(18.3050817046749,8.67867815729521,37.177741619172));
#42451=CARTESIAN_POINT('Ctrl Pts',(18.3296354828288,8.67536458103033,37.1348681721982));
#42452=CARTESIAN_POINT('Ctrl Pts',(18.3333414428768,8.67487152678297,37.1284824636091));
#42453=CARTESIAN_POINT('Ctrl Pts',(18.3394038990088,8.67407649207481,37.1181730850818));
#42454=CARTESIAN_POINT('Ctrl Pts',(18.3417378144184,8.67377313033206,37.1142363232365));
#42455=CARTESIAN_POINT('Ctrl Pts',(18.3459137970119,8.67323517877215,37.1072492322241));
#42456=CARTESIAN_POINT('Ctrl Pts',(18.3477503243465,8.67300023958734,37.1041956698814));
#42457=CARTESIAN_POINT('Ctrl Pts',(18.3517249614256,8.67249531340159,37.0976283767873));
#42458=CARTESIAN_POINT('Ctrl Pts',(18.3538658461293,8.6722255099855,37.0941163973641));
#42459=CARTESIAN_POINT('Ctrl Pts',(18.3598344350876,8.67147922719108,37.0843954122656));
#42460=CARTESIAN_POINT('Ctrl Pts',(18.3636861953476,8.6710042821337,37.0782011470955));
#42461=CARTESIAN_POINT('Ctrl Pts',(18.3855916359656,8.66833952165047,37.0434151242131));
#42462=CARTESIAN_POINT('Ctrl Pts',(18.4043607577609,8.66619348035324,37.0152780484829));
#42463=CARTESIAN_POINT('Ctrl Pts',(18.4667417501141,8.65943280195774,36.9268878564747));
#42464=CARTESIAN_POINT('Ctrl Pts',(18.5131034263716,8.65494784971253,36.8686538359602));
#42465=CARTESIAN_POINT('Ctrl Pts',(18.671523798129,8.64072457814127,36.6917017671893));
#42466=CARTESIAN_POINT('Ctrl Pts',(18.7952931434053,8.63110109067927,36.5844709369568));
#42467=CARTESIAN_POINT('Ctrl Pts',(18.9485086637306,8.61942861651755,36.4824873374328));
#42468=CARTESIAN_POINT('Ctrl Pts',(18.9661315180916,8.6180904710202,36.4711669356563));
#42469=CARTESIAN_POINT('Ctrl Pts',(18.9909491234143,8.61621042931289,36.4557898621723));
#42470=CARTESIAN_POINT('Ctrl Pts',(18.9979913069591,8.61567744333818,36.4514887854548));
#42471=CARTESIAN_POINT('Ctrl Pts',(19.0102136088123,8.61475313843034,36.4441311554727));
#42472=CARTESIAN_POINT('Ctrl Pts',(19.0153808667649,8.61436259313252,36.4410533789283));
#42473=CARTESIAN_POINT('Ctrl Pts',(19.0261318314719,8.61355044918303,36.4347177000761));
#42474=CARTESIAN_POINT('Ctrl Pts',(19.0317176833372,8.61312871997651,36.4314636049375));
#42475=CARTESIAN_POINT('Ctrl Pts',(19.0448791960044,8.61213552361083,36.4238845798414));
#42476=CARTESIAN_POINT('Ctrl Pts',(19.0524679949931,8.61156323599834,36.4195828651214));
#42477=CARTESIAN_POINT('Ctrl Pts',(19.0774180298089,8.60968276691568,36.405662669337));
#42478=CARTESIAN_POINT('Ctrl Pts',(19.0948980847875,8.60836696962201,36.396260889952));
#42479=CARTESIAN_POINT('Ctrl Pts',(19.1873279636243,8.601415661773,36.3483706546545));
#42480=CARTESIAN_POINT('Ctrl Pts',(19.2645848629636,8.59562094572606,36.3145582251576));
#42481=CARTESIAN_POINT('Ctrl Pts',(19.3604890961541,8.58845997117052,36.2798671695252));
#42482=CARTESIAN_POINT('Ctrl Pts',(19.3772604491198,8.5872091125392,36.2740611274072));
#42483=CARTESIAN_POINT('Ctrl Pts',(19.3941041019635,8.5859548064474,36.2684889523559));
#42484=CARTESIAN_POINT('',(18.0708705926165,8.57277459783182,38.0983183026454));
#42485=CARTESIAN_POINT('Ctrl Pts',(19.3941040078119,8.41575742730426,36.2684889835028));
#42486=CARTESIAN_POINT('Ctrl Pts',(19.3848991309847,8.41642638796206,36.2715341183276));
#42487=CARTESIAN_POINT('Ctrl Pts',(19.375715186781,8.41709286238427,36.274649315926));
#42488=CARTESIAN_POINT('Ctrl Pts',(19.3456867897387,8.4192679999204,36.2850882128645));
#42489=CARTESIAN_POINT('Ctrl Pts',(19.324945616991,8.42076405854974,36.2927002862353));
#42490=CARTESIAN_POINT('Ctrl Pts',(19.2981774761885,8.42268247904916,36.3030494338562));
#42491=CARTESIAN_POINT('Ctrl Pts',(19.292028396551,8.42312231425697,36.3054631784397));
#42492=CARTESIAN_POINT('Ctrl Pts',(19.2822123156983,8.42382293322785,36.3093746665292));
#42493=CARTESIAN_POINT('Ctrl Pts',(19.2785373869231,8.42408488937646,36.3108521740117));
#42494=CARTESIAN_POINT('Ctrl Pts',(19.2715337944116,8.42458343306352,36.3136930603939));
#42495=CARTESIAN_POINT('Ctrl Pts',(19.2682044333705,8.42482012882439,36.3150544142676));
#42496=CARTESIAN_POINT('Ctrl Pts',(19.2604867172502,8.42536814024514,36.3182353608926));
#42497=CARTESIAN_POINT('Ctrl Pts',(19.2561012544136,8.42567903862751,36.3200618600532));
#42498=CARTESIAN_POINT('Ctrl Pts',(19.242108999303,8.42666952907365,36.3259502331411));
#42499=CARTESIAN_POINT('Ctrl Pts',(19.232528182215,8.42734553221231,36.33007390978));
#42500=CARTESIAN_POINT('Ctrl Pts',(19.2098593523128,8.42894082442971,36.3400494795614));
#42501=CARTESIAN_POINT('Ctrl Pts',(19.1968020205997,8.42985638625897,36.3459700372146));
#42502=CARTESIAN_POINT('Ctrl Pts',(19.1501614706936,8.43311898507669,36.3677482185352));
#42503=CARTESIAN_POINT('Ctrl Pts',(19.1169699950115,8.43542625216121,36.3844300878864));
#42504=CARTESIAN_POINT('Ctrl Pts',(18.9892696182184,8.44432445756877,36.4533005999203));
#42505=CARTESIAN_POINT('Ctrl Pts',(18.8987238035524,8.45068962835837,36.5124269462432));
#42506=CARTESIAN_POINT('Ctrl Pts',(18.7224411708371,8.46409296921966,36.6499139954033));
#42507=CARTESIAN_POINT('Ctrl Pts',(18.6378743550572,8.47112546962341,36.7290462520064));
#42508=CARTESIAN_POINT('Ctrl Pts',(18.5516755013798,8.47938786456374,36.8256018110458));
#42509=CARTESIAN_POINT('Ctrl Pts',(18.5425584861293,8.48027690314834,36.8360384440502));
#42510=CARTESIAN_POINT('Ctrl Pts',(18.5281526999225,8.48170672774657,36.852892461833));
#42511=CARTESIAN_POINT('Ctrl Pts',(18.5227914972279,8.48224455341234,36.8592475177218));
#42512=CARTESIAN_POINT('Ctrl Pts',(18.5133620365193,8.48320080127514,36.8705727459033));
#42513=CARTESIAN_POINT('Ctrl Pts',(18.5092771777996,8.48361854477857,36.8755289822587));
#42514=CARTESIAN_POINT('Ctrl Pts',(18.5008317449632,8.48448959551847,36.8858808843018));
#42515=CARTESIAN_POINT('Ctrl Pts',(18.4964753806189,8.48494306278867,36.8912798500816));
#42516=CARTESIAN_POINT('Ctrl Pts',(18.4852616353359,8.48612125631757,36.9053317865503));
#42517=CARTESIAN_POINT('Ctrl Pts',(18.4784493250547,8.48684775159144,36.914020241056));
#42518=CARTESIAN_POINT('Ctrl Pts',(18.4497742969285,8.48995243895945,36.9512462462982));
#42519=CARTESIAN_POINT('Ctrl Pts',(18.4286382113707,8.49235857879415,36.9803318556644));
#42520=CARTESIAN_POINT('Ctrl Pts',(18.360446956283,8.50053748306687,37.0799071250089));
#42521=CARTESIAN_POINT('Ctrl Pts',(18.3172305370408,8.50644268603515,37.1528952376087));
#42522=CARTESIAN_POINT('Ctrl Pts',(18.2475280489201,8.51736527376308,37.2905409566783));
#42523=CARTESIAN_POINT('Ctrl Pts',(18.2194811459851,8.52234319012644,37.3542560202293));
#42524=CARTESIAN_POINT('Ctrl Pts',(18.1616715418693,8.53401414430814,37.5075640687818));
#42525=CARTESIAN_POINT('Ctrl Pts',(18.1349134168957,8.54067530251925,37.5981152197207));
#42526=CARTESIAN_POINT('Ctrl Pts',(18.1128933647926,8.54764374833379,37.6994267760442));
#42527=CARTESIAN_POINT('Ctrl Pts',(18.1109698776412,8.54827023232164,37.7085979485047));
#42528=CARTESIAN_POINT('Ctrl Pts',(18.1082125335167,8.54919526664416,37.7222389572455));
#42529=CARTESIAN_POINT('Ctrl Pts',(18.1073275641157,8.54949658276279,37.7266981445789));
#42530=CARTESIAN_POINT('Ctrl Pts',(18.1057775955158,8.55003230303361,37.7346553451855));
#42531=CARTESIAN_POINT('Ctrl Pts',(18.1051065111721,8.55026704521818,37.7381521021605));
#42532=CARTESIAN_POINT('Ctrl Pts',(18.1036771975485,8.55077312865774,37.7457127228023));
#42533=CARTESIAN_POINT('Ctrl Pts',(18.1029223498069,8.5510442779673,37.749777162634));
#42534=CARTESIAN_POINT('Ctrl Pts',(18.101395415165,8.55160094695933,37.7581486674295));
#42535=CARTESIAN_POINT('Ctrl Pts',(18.1006249048359,8.55188637835711,37.7624560000345));
#42536=CARTESIAN_POINT('Ctrl Pts',(18.0986976260184,8.5526121835612,37.7734455202549));
#42537=CARTESIAN_POINT('Ctrl Pts',(18.0975614133501,8.55305146036004,37.7801313194813));
#42538=CARTESIAN_POINT('Ctrl Pts',(18.0795216856533,8.560220281871,37.8897796796842));
#42539=CARTESIAN_POINT('Ctrl Pts',(18.070961640832,8.5665249751136,37.9939540363477));
#42540=CARTESIAN_POINT('Ctrl Pts',(18.0708707318637,8.57277491926653,38.0983196072232));
#42541=CARTESIAN_POINT('Ctrl Pts',(18.0708707330131,8.5727748402797,38.0983182882505));
#42542=CARTESIAN_POINT('Ctrl Pts',(18.070749004497,8.58113704941933,38.2379557992846));
#42543=CARTESIAN_POINT('Ctrl Pts',(18.0857878098588,8.58938279054467,38.3771880622356));
#42544=CARTESIAN_POINT('Ctrl Pts',(18.1230963197836,8.60024268730473,38.5471660746574));
#42545=CARTESIAN_POINT('Ctrl Pts',(18.1313644004084,8.60241260062862,38.580547285625));
#42546=CARTESIAN_POINT('Ctrl Pts',(18.1432112590839,8.60525678639379,38.623431275503));
#42547=CARTESIAN_POINT('Ctrl Pts',(18.1459793066124,8.60590534179989,38.6331528775391));
#42548=CARTESIAN_POINT('Ctrl Pts',(18.1513784890223,8.60714109316598,38.6515645933021));
#42549=CARTESIAN_POINT('Ctrl Pts',(18.1539948320585,8.60772780255918,38.6602587855167));
#42550=CARTESIAN_POINT('Ctrl Pts',(18.1585975142864,8.60873975400798,38.6751713239731));
#42551=CARTESIAN_POINT('Ctrl Pts',(18.1605542390729,8.60916402911885,38.6813987075839));
#42552=CARTESIAN_POINT('Ctrl Pts',(18.1643503649932,8.60997604842752,38.6932690791636));
#42553=CARTESIAN_POINT('Ctrl Pts',(18.1661842795609,8.61036360949216,38.6989137541779));
#42554=CARTESIAN_POINT('Ctrl Pts',(18.1709985031265,8.61136898667718,38.7135022040483));
#42555=CARTESIAN_POINT('Ctrl Pts',(18.1740183477367,8.61198809041072,38.7224326712289));
#42556=CARTESIAN_POINT('Ctrl Pts',(18.1844393840789,8.61408659738454,38.7525217759866));
#42557=CARTESIAN_POINT('Ctrl Pts',(18.1921436279316,8.61557590037894,38.7735727760014));
#42558=CARTESIAN_POINT('Ctrl Pts',(18.2475914471912,8.62589226262562,38.9172683532188));
#42559=CARTESIAN_POINT('Ctrl Pts',(18.3074018082523,8.63512920963893,39.0348597902583));
#42560=CARTESIAN_POINT('Ctrl Pts',(18.4173860652214,8.64959396410313,39.2054285540465));
#42561=CARTESIAN_POINT('Ctrl Pts',(18.4593751358328,8.6547045979383,39.263234528087));
#42562=CARTESIAN_POINT('Ctrl Pts',(18.531987846301,8.66281453450918,39.3523499195233));
#42563=CARTESIAN_POINT('Ctrl Pts',(18.5606412034207,8.66585735539084,39.3851796683715));
#42564=CARTESIAN_POINT('Ctrl Pts',(18.606682020665,8.67047890652087,39.4344577644889));
#42565=CARTESIAN_POINT('Ctrl Pts',(18.6233040037462,8.67209731613394,39.4515993414355));
#42566=CARTESIAN_POINT('Ctrl Pts',(18.6448687868715,8.67412940367131,39.4730275006471));
#42567=CARTESIAN_POINT('Ctrl Pts',(18.6495201242178,8.67456381686548,39.4776027113989));
#42568=CARTESIAN_POINT('Ctrl Pts',(18.6566110345848,8.67522007655582,39.4845071394238));
#42569=CARTESIAN_POINT('Ctrl Pts',(18.6590335932596,8.67544323160539,39.4868536433027));
#42570=CARTESIAN_POINT('Ctrl Pts',(18.6640220310874,8.67590056600051,39.4916601807315));
#42571=CARTESIAN_POINT('Ctrl Pts',(18.666588528428,8.67613468040881,39.4941194496579));
#42572=CARTESIAN_POINT('Ctrl Pts',(18.6723927952703,8.67666150327284,39.4996505224452));
#42573=CARTESIAN_POINT('Ctrl Pts',(18.675634428608,8.67695389491405,39.5027181859993));
#42574=CARTESIAN_POINT('Ctrl Pts',(18.685204629784,8.67781184124905,39.5117120316583));
#42575=CARTESIAN_POINT('Ctrl Pts',(18.6915626391734,8.67837507944434,39.5176069291249));
#42576=CARTESIAN_POINT('Ctrl Pts',(18.7381991707946,8.68245954925458,39.5602654245514));
#42577=CARTESIAN_POINT('Ctrl Pts',(18.7799849334239,8.6858662967866,39.5953531080771));
#42578=CARTESIAN_POINT('Ctrl Pts',(18.924186096177,8.69702459548907,39.7063646310801));
#42579=CARTESIAN_POINT('Ctrl Pts',(19.0326252067003,8.70448789627749,39.7739093515283));
#42580=CARTESIAN_POINT('Ctrl Pts',(19.2052572280039,8.71609845039306,39.8590208122445));
#42581=CARTESIAN_POINT('Ctrl Pts',(19.2649876174564,8.72006756913927,39.8848041988912));
#42582=CARTESIAN_POINT('Ctrl Pts',(19.3616063094172,8.72650973299399,39.9208372077941));
#42583=CARTESIAN_POINT('Ctrl Pts',(19.3976949994992,8.72892018185757,39.933091109892));
#42584=CARTESIAN_POINT('Ctrl Pts',(19.4448736679951,8.73208747244164,39.947566999168));
#42585=CARTESIAN_POINT('Ctrl Pts',(19.455654753367,8.73281230352817,39.9507720833908));
#42586=CARTESIAN_POINT('Ctrl Pts',(19.4731736494373,8.73399209720041,39.9558139225065));
#42587=CARTESIAN_POINT('Ctrl Pts',(19.4798945945483,8.73444517933215,39.9577087187482));
#42588=CARTESIAN_POINT('Ctrl Pts',(19.4928027209772,8.73531631965207,39.9612722911868));
#42589=CARTESIAN_POINT('Ctrl Pts',(19.4989882309744,8.73573418621684,39.9629468128287));
#42590=CARTESIAN_POINT('Ctrl Pts',(19.5131238880677,8.73669014368657,39.9666980810024));
#42591=CARTESIAN_POINT('Ctrl Pts',(19.5210791477153,8.73722886613063,39.9687549030615));
#42592=CARTESIAN_POINT('Ctrl Pts',(19.5421631522625,8.738658698237,39.9740626745617));
#42593=CARTESIAN_POINT('Ctrl Pts',(19.5553131721715,8.73955257163661,39.977226437254));
#42594=CARTESIAN_POINT('Ctrl Pts',(19.6587672497156,8.74660249150382,40.0009684417915));
#42595=CARTESIAN_POINT('Ctrl Pts',(19.750400094876,8.75296084105432,40.0151543159398));
#42596=CARTESIAN_POINT('Ctrl Pts',(20.0020530997806,8.77069677533662,40.0357444041683));
#42597=CARTESIAN_POINT('Ctrl Pts',(20.1624136223143,8.78233862110124,40.0289194047978));
#42598=CARTESIAN_POINT('Ctrl Pts',(20.3487489584781,8.79535381899516,39.9975672075715));
#42599=CARTESIAN_POINT('Ctrl Pts',(20.3772972232622,8.79733122699818,39.9920978235376));
#42600=CARTESIAN_POINT('Ctrl Pts',(20.4125182631042,8.79974137504841,39.984521078921));
#42601=CARTESIAN_POINT('Ctrl Pts',(20.4193158669378,8.80020515829813,39.9830202393171));
#42602=CARTESIAN_POINT('Ctrl Pts',(20.4300452655318,8.80093486901602,39.9805903184399));
#42603=CARTESIAN_POINT('Ctrl Pts',(20.4339824389206,8.80120214087178,39.9796856438431));
#42604=CARTESIAN_POINT('Ctrl Pts',(20.4413995565228,8.80170467110893,39.9779568091657));
#42605=CARTESIAN_POINT('Ctrl Pts',(20.4448800093189,8.80194007117429,39.9771353502433));
#42606=CARTESIAN_POINT('Ctrl Pts',(20.4528482502636,8.8024780878774,39.9752312738602));
#42607=CARTESIAN_POINT('Ctrl Pts',(20.4573344491471,8.80278033446005,39.9741422227101));
#42608=CARTESIAN_POINT('Ctrl Pts',(20.4692763458322,8.8035832302941,39.9711978239821));
#42609=CARTESIAN_POINT('Ctrl Pts',(20.4767250351528,8.80408230476811,39.9693140000673));
#42610=CARTESIAN_POINT('Ctrl Pts',(20.5310041663886,8.80770780715442,39.9552408946917));
#42611=CARTESIAN_POINT('Ctrl Pts',(20.5773769612004,8.81074388346939,39.9413367275625));
#42612=CARTESIAN_POINT('Ctrl Pts',(20.6340067761872,8.81443064499459,39.922006804528));
#42613=CARTESIAN_POINT('Ctrl Pts',(20.6447987662835,8.8151322727096,39.9182155942086));
#42614=CARTESIAN_POINT('Ctrl Pts',(20.7563313686681,8.82237940952885,39.8779164275811));
#42615=CARTESIAN_POINT('Ctrl Pts',(20.853901503815,8.82869497554362,39.8331700404347));
#42616=CARTESIAN_POINT('Ctrl Pts',(21.0449215969719,8.84185653653094,39.7255001694213));
#42617=CARTESIAN_POINT('Ctrl Pts',(21.1375897259241,8.84869277879936,39.662048752801));
#42618=CARTESIAN_POINT('Ctrl Pts',(21.2356696326248,8.85679948852639,39.5815136467512));
#42619=CARTESIAN_POINT('Ctrl Pts',(21.2470125584576,8.85775110702672,39.5719788673308));
#42620=CARTESIAN_POINT('Ctrl Pts',(21.2641238536013,8.85920891731446,39.5572555037967));
#42621=CARTESIAN_POINT('Ctrl Pts',(21.269972799541,8.85971126396723,39.5521610813264));
#42622=CARTESIAN_POINT('Ctrl Pts',(21.2805076733181,8.86062351311857,39.5428728977643));
#42623=CARTESIAN_POINT('Ctrl Pts',(21.2852041432915,8.86103291211857,39.5386912139283));
#42624=CARTESIAN_POINT('Ctrl Pts',(21.2953299090283,8.86192155003038,39.5295861987027));
#42625=CARTESIAN_POINT('Ctrl Pts',(21.3007517448856,8.86240112493821,39.5246547541177));
#42626=CARTESIAN_POINT('Ctrl Pts',(21.315334154858,8.86370126720918,39.5112386482854));
#42627=CARTESIAN_POINT('Ctrl Pts',(21.3244405434089,8.86452428553332,39.5026958672255));
#42628=CARTESIAN_POINT('Ctrl Pts',(21.3682107678858,8.86853518513463,39.4608284049176));
#42629=CARTESIAN_POINT('Ctrl Pts',(21.401700680364,8.87177446489907,39.4263065874626));
#42630=CARTESIAN_POINT('Ctrl Pts',(21.4538512339425,8.87710966042895,39.368365788667));
#42631=CARTESIAN_POINT('Ctrl Pts',(21.4733191800944,8.87917330927737,39.345698852864));
#42632=CARTESIAN_POINT('Ctrl Pts',(21.5715215036719,8.88996168302534,39.2258363954545));
#42633=CARTESIAN_POINT('Ctrl Pts',(21.6411886795515,8.89895774966858,39.1216076880706));
#42634=CARTESIAN_POINT('Ctrl Pts',(21.7261395517637,8.91171898264758,38.9631239835298));
#42635=CARTESIAN_POINT('Ctrl Pts',(21.7499435467515,8.9155720030314,38.9137808153142));
#42636=CARTESIAN_POINT('Ctrl Pts',(21.7826749066873,8.92126245519379,38.8378301643255));
#42637=CARTESIAN_POINT('Ctrl Pts',(21.7931745007223,8.92316197395149,38.8119329925777));
#42638=CARTESIAN_POINT('Ctrl Pts',(21.8055519995158,8.92549072161026,38.7793907413106));
#42639=CARTESIAN_POINT('Ctrl Pts',(21.8079612661913,8.92594860121751,38.772953093317));
#42640=CARTESIAN_POINT('Ctrl Pts',(21.8117251102374,8.92667114522577,38.762729842947));
#42641=CARTESIAN_POINT('Ctrl Pts',(21.8131023217205,8.9269371107392,38.7589527232692));
#42642=CARTESIAN_POINT('Ctrl Pts',(21.8156837402881,8.92743861232784,38.7518035993506));
#42643=CARTESIAN_POINT('Ctrl Pts',(21.8168903529345,8.92767428198447,38.7484325890233));
#42644=CARTESIAN_POINT('Ctrl Pts',(21.8196424737847,8.92821475154627,38.7406757740149));
#42645=CARTESIAN_POINT('Ctrl Pts',(21.8211815148747,8.92851916939472,38.7362877264286));
#42646=CARTESIAN_POINT('Ctrl Pts',(21.8252589615289,8.92933167171634,38.7245262917952));
#42647=CARTESIAN_POINT('Ctrl Pts',(21.8277685837473,8.92983812124188,38.7171429129602));
#42648=CARTESIAN_POINT('Ctrl Pts',(21.8464626821652,8.93366122788981,38.6610299493216));
#42649=CARTESIAN_POINT('Ctrl Pts',(21.8607422232866,8.93687605393367,38.6116820031645));
#42650=CARTESIAN_POINT('Ctrl Pts',(21.9032979656997,8.94780253537605,38.4390849951399));
#42651=CARTESIAN_POINT('Ctrl Pts',(21.9214243829713,8.95520991517982,38.3136682034745));
#42652=CARTESIAN_POINT('Ctrl Pts',(21.9313172375979,8.96836514029637,38.0954661817475));
#42653=CARTESIAN_POINT('Ctrl Pts',(21.9289038780743,8.9739946166648,38.0033896555581));
#42654=CARTESIAN_POINT('Ctrl Pts',(21.9179053219143,8.98115052821193,37.8911613108213));
#42655=CARTESIAN_POINT('Ctrl Pts',(21.9155444275347,8.9824789906151,37.8705138026597));
#42656=CARTESIAN_POINT('Ctrl Pts',(21.9116985871941,8.98439030799835,37.8410984296478));
#42657=CARTESIAN_POINT('Ctrl Pts',(21.9104858170327,8.98496466461387,37.8322959656726));
#42658=CARTESIAN_POINT('Ctrl Pts',(21.9082817397875,8.98596199478974,37.8170768460204));
#42659=CARTESIAN_POINT('Ctrl Pts',(21.9073187629761,8.98638407430636,37.8106561834941));
#42660=CARTESIAN_POINT('Ctrl Pts',(21.9054072741554,8.98719659460326,37.7983356435837));
#42661=CARTESIAN_POINT('Ctrl Pts',(21.9044637230924,8.98758687487998,37.7924350630936));
#42662=CARTESIAN_POINT('Ctrl Pts',(21.9019246921422,8.98860972958084,37.7770167898633));
#42663=CARTESIAN_POINT('Ctrl Pts',(21.9002851971068,8.9892436824687,37.7675066127627));
#42664=CARTESIAN_POINT('Ctrl Pts',(21.8943600199353,8.99144719419011,37.7346127670919));
#42665=CARTESIAN_POINT('Ctrl Pts',(21.8897136488818,8.99302804768908,37.71129708652));
#42666=CARTESIAN_POINT('Ctrl Pts',(21.8836364454197,8.99493685725024,37.6834927496696));
#42667=CARTESIAN_POINT('Ctrl Pts',(21.8826184102268,8.99525188702551,37.6789151286036));
#42668=CARTESIAN_POINT('Ctrl Pts',(21.8328060834032,9.01044251524392,37.4587244877102));
#42669=CARTESIAN_POINT('Ctrl Pts',(21.7473247955972,9.02662360429059,37.253110031045));
#42670=CARTESIAN_POINT('Ctrl Pts',(21.6068857344155,9.04486668649835,37.0317503188578));
#42671=CARTESIAN_POINT('Ctrl Pts',(21.583709448555,9.04769209480757,36.997682387957));
#42672=CARTESIAN_POINT('Ctrl Pts',(21.5549181370492,9.05096919408511,36.9581455331121));
#42673=CARTESIAN_POINT('Ctrl Pts',(21.5503407009979,9.05148363503288,36.9519382628826));
#42674=CARTESIAN_POINT('Ctrl Pts',(21.543210800634,9.05227465113135,36.9423901113885));
#42675=CARTESIAN_POINT('Ctrl Pts',(21.5406844993102,9.05255296574694,36.9390299298318));
#42676=CARTESIAN_POINT('Ctrl Pts',(21.5360021763646,9.05306515595803,36.9328442682106));
#42677=CARTESIAN_POINT('Ctrl Pts',(21.5338493456925,9.05329923938201,36.9300165073158));
#42678=CARTESIAN_POINT('Ctrl Pts',(21.5289814439366,9.05382538694573,36.9236590074866));
#42679=CARTESIAN_POINT('Ctrl Pts',(21.5262619649147,9.05411713792295,36.920132718477));
#42680=CARTESIAN_POINT('Ctrl Pts',(21.5182400788114,9.05497146061535,36.9098050610497));
#42681=CARTESIAN_POINT('Ctrl Pts',(21.5129041607175,9.05553174500311,36.9030296842318));
#42682=CARTESIAN_POINT('Ctrl Pts',(21.4742794605666,9.05953245837888,36.8546562166427));
#42683=CARTESIAN_POINT('Ctrl Pts',(21.4393220807361,9.06286367324542,36.8144129055365));
#42684=CARTESIAN_POINT('Ctrl Pts',(21.3876762214856,9.06748088874049,36.7597094537792));
#42685=CARTESIAN_POINT('Ctrl Pts',(21.3723411088095,9.06881691676788,36.7440118093443));
#42686=CARTESIAN_POINT('Ctrl Pts',(21.2380857010789,9.08025248628564,36.6111935025206));
#42687=CARTESIAN_POINT('Ctrl Pts',(21.1047047731269,9.08995843329927,36.5097078479521));
#42688=CARTESIAN_POINT('Ctrl Pts',(20.9230890044272,9.10299529583187,36.4055229008584));
#42689=CARTESIAN_POINT('Ctrl Pts',(20.8855679655936,9.10567556289841,36.3856152986424));
#42690=CARTESIAN_POINT('Ctrl Pts',(20.8369982689855,9.10914373137084,36.3618656246571));
#42691=CARTESIAN_POINT('Ctrl Pts',(20.8265282337326,9.10989125050262,36.3568625188116));
#42692=CARTESIAN_POINT('Ctrl Pts',(20.8096149755404,9.11109891262312,36.3489671570532));
#42693=CARTESIAN_POINT('Ctrl Pts',(20.8031997872061,9.11155700565227,36.3460152436993));
#42694=CARTESIAN_POINT('Ctrl Pts',(20.7909512363762,9.11243176533418,36.3404604293796));
#42695=CARTESIAN_POINT('Ctrl Pts',(20.7851208590442,9.11284820728739,36.3378511430763));
#42696=CARTESIAN_POINT('Ctrl Pts',(20.7717775677259,9.11380144044364,36.3319589474194));
#42697=CARTESIAN_POINT('Ctrl Pts',(20.764256508982,9.11433886238197,36.328694898489));
#42698=CARTESIAN_POINT('Ctrl Pts',(20.7446029372759,9.11574365899821,36.3203139600039));
#42699=CARTESIAN_POINT('Ctrl Pts',(20.7324386048686,9.11661357532109,36.3152732392011));
#42700=CARTESIAN_POINT('Ctrl Pts',(20.6461070447136,9.12279157365804,36.2805299582289));
#42701=CARTESIAN_POINT('Ctrl Pts',(20.5702189862095,9.12824847194836,36.2553393763607));
#42702=CARTESIAN_POINT('Ctrl Pts',(20.3346190373906,9.14526108929534,36.193062999274));
#42703=CARTESIAN_POINT('Ctrl Pts',(20.1715716519762,9.15718905139255,36.1715458474117));
#42704=CARTESIAN_POINT('Ctrl Pts',(19.9702403675266,9.17116011690922,36.1707343852393));
#42705=CARTESIAN_POINT('Ctrl Pts',(19.932705896441,9.17372881788065,36.1716786030518));
#42706=CARTESIAN_POINT('Ctrl Pts',(19.8877131282004,9.17674677200587,36.1741259814492));
#42707=CARTESIAN_POINT('Ctrl Pts',(19.8802085451391,9.17724810198117,36.174578204958));
#42708=CARTESIAN_POINT('Ctrl Pts',(19.8685538603466,9.17802328825103,36.1753489172515));
#42709=CARTESIAN_POINT('Ctrl Pts',(19.8644019241899,9.17829877766179,36.1756369779577));
#42710=CARTESIAN_POINT('Ctrl Pts',(19.8567027268409,9.1788083561495,36.1761961886969));
#42711=CARTESIAN_POINT('Ctrl Pts',(19.8531553137936,9.17904263646819,36.1764637119729));
#42712=CARTESIAN_POINT('Ctrl Pts',(19.8451149639858,9.17957250526819,36.177092436318));
#42713=CARTESIAN_POINT('Ctrl Pts',(19.8406225489198,9.17986776065101,36.1774595707885));
#42714=CARTESIAN_POINT('Ctrl Pts',(19.8269897691844,9.18076143135048,36.1786217983355));
#42715=CARTESIAN_POINT('Ctrl Pts',(19.8178535894194,9.18135717177682,36.1794663692121));
#42716=CARTESIAN_POINT('Ctrl Pts',(19.7409610406316,9.18634704018642,36.1871281474852));
#42717=CARTESIAN_POINT('Ctrl Pts',(19.6735951110742,9.19056193509964,36.1974643286947));
#42718=CARTESIAN_POINT('Ctrl Pts',(19.5349075608324,9.19916953874482,36.2263296784686));
#42719=CARTESIAN_POINT('Ctrl Pts',(19.4638576286326,9.20354104659619,36.2454132542409));
#42720=CARTESIAN_POINT('Ctrl Pts',(19.3941038390373,9.20793124499895,36.2684890393365));
#42721=CARTESIAN_POINT('Origin',(20.,-1.3495818343519,38.1));
#42722=CARTESIAN_POINT('',(19.394104010895,10.1712205940279,36.2684889824829));
#42723=CARTESIAN_POINT('',(19.3941040084883,9.99997597504684,36.2684889832791));
#42724=CARTESIAN_POINT('',(19.3941040087494,-1.3495818343519,36.2684889831927));
#42725=CARTESIAN_POINT('',(18.0708705563808,9.53609590521103,38.1014651490007));
#42726=CARTESIAN_POINT('Ctrl Pts',(19.394104010895,10.1712205940279,36.2684889824829));
#42727=CARTESIAN_POINT('Ctrl Pts',(19.4649959241567,10.1665882905303,36.2450366933651));
#42728=CARTESIAN_POINT('Ctrl Pts',(19.5372003889732,10.162104549311,36.2257166576543));
#42729=CARTESIAN_POINT('Ctrl Pts',(19.76068220923,10.1484606807009,36.1796277861682));
#42730=CARTESIAN_POINT('Ctrl Pts',(19.9141540621807,10.1393618920268,36.1666798877873));
#42731=CARTESIAN_POINT('Ctrl Pts',(20.0892165160705,10.1282613971371,36.1728119526785));
#42732=CARTESIAN_POINT('Ctrl Pts',(20.1108860438118,10.1268758742603,36.1739372851868));
#42733=CARTESIAN_POINT('Ctrl Pts',(20.140886959719,10.1249398545048,36.1760032303887));
#42734=CARTESIAN_POINT('Ctrl Pts',(20.1492386658252,10.1243989897188,36.1766330246421));
#42735=CARTESIAN_POINT('Ctrl Pts',(20.1636122185678,10.1234647382788,36.1778111020717));
#42736=CARTESIAN_POINT('Ctrl Pts',(20.1696361243812,10.1230721654309,36.1783333532301));
#42737=CARTESIAN_POINT('Ctrl Pts',(20.1820756803133,10.1222593131199,36.1794707651238));
#42738=CARTESIAN_POINT('Ctrl Pts',(20.188490894217,10.1218389185514,36.1800897738471));
#42739=CARTESIAN_POINT('Ctrl Pts',(20.2034619842848,10.1208549953831,36.1816101041192));
#42740=CARTESIAN_POINT('Ctrl Pts',(20.2120151179916,10.1202906902932,36.182536530369));
#42741=CARTESIAN_POINT('Ctrl Pts',(20.2396113324032,10.1184627843337,36.1857124920675));
#42742=CARTESIAN_POINT('Ctrl Pts',(20.2586266572917,10.1171921451402,36.1881886963173));
#42743=CARTESIAN_POINT('Ctrl Pts',(20.3556989931151,10.1106465368118,36.2023042936129));
#42744=CARTESIAN_POINT('Ctrl Pts',(20.4330159749597,10.1052325321538,36.2184407885767));
#42745=CARTESIAN_POINT('Ctrl Pts',(20.6119589365952,10.0922429472052,36.2674017054927));
#42746=CARTESIAN_POINT('Ctrl Pts',(20.7122841736996,10.0845917594271,36.3040158994054));
#42747=CARTESIAN_POINT('Ctrl Pts',(20.8865847804673,10.0709400513689,36.3845402034327));
#42748=CARTESIAN_POINT('Ctrl Pts',(20.9616535051949,10.0649328293062,36.4254669184944));
#42749=CARTESIAN_POINT('Ctrl Pts',(21.0416775986849,10.0585623095673,36.4762580101657));
#42750=CARTESIAN_POINT('Ctrl Pts',(21.049548402247,10.0579361551078,36.4813343677029));
#42751=CARTESIAN_POINT('Ctrl Pts',(21.0611836815631,10.0570115109919,36.4889592155716));
#42752=CARTESIAN_POINT('Ctrl Pts',(21.0649764788323,10.0567102588818,36.491463921545));
#42753=CARTESIAN_POINT('Ctrl Pts',(21.0717245704979,10.0561746075507,36.4959545895044));
#42754=CARTESIAN_POINT('Ctrl Pts',(21.0746832454251,10.0559398706551,36.4979353456665));
#42755=CARTESIAN_POINT('Ctrl Pts',(21.0810658284941,10.0554337477318,36.5022339576626));
#42756=CARTESIAN_POINT('Ctrl Pts',(21.0844877666132,10.0551625539207,36.5045546275588));
#42757=CARTESIAN_POINT('Ctrl Pts',(21.0940071958797,10.0544084847684,36.5110552361693));
#42758=CARTESIAN_POINT('Ctrl Pts',(21.1000882410997,10.0539271965464,36.5152593040997));
#42759=CARTESIAN_POINT('Ctrl Pts',(21.1351424913628,10.0511542661278,36.5397927082321));
#42760=CARTESIAN_POINT('Ctrl Pts',(21.1635781421165,10.0489106765686,36.5608828635199));
#42761=CARTESIAN_POINT('Ctrl Pts',(21.254653703138,10.0416859268719,36.6323996499693));
#42762=CARTESIAN_POINT('Ctrl Pts',(21.3147274912008,10.0368557999983,36.6859630531611));
#42763=CARTESIAN_POINT('Ctrl Pts',(21.4798171190979,10.0228199523344,36.8528060026792));
#42764=CARTESIAN_POINT('Ctrl Pts',(21.574782938254,10.0136768967401,36.9750982186026));
#42765=CARTESIAN_POINT('Ctrl Pts',(21.665304317528,10.0025277986846,37.1259503912495));
#42766=CARTESIAN_POINT('Ctrl Pts',(21.6761284926041,10.0011455352919,37.1446967357882));
#42767=CARTESIAN_POINT('Ctrl Pts',(21.6906959371529,9.99921335317547,37.1709360547496));
#42768=CARTESIAN_POINT('Ctrl Pts',(21.694709578797,9.99867301591924,37.1782776957265));
#42769=CARTESIAN_POINT('Ctrl Pts',(21.7015401442436,9.99773943156566,37.1909674215174));
#42770=CARTESIAN_POINT('Ctrl Pts',(21.7043799496864,9.99734699556814,37.1963031056026));
#42771=CARTESIAN_POINT('Ctrl Pts',(21.7101964736796,9.99653419687392,37.2073566598612));
#42772=CARTESIAN_POINT('Ctrl Pts',(21.7131696978256,9.99611371805557,37.2130762738291));
#42773=CARTESIAN_POINT('Ctrl Pts',(21.7200474771764,9.99512919826382,37.2264707324197));
#42774=CARTESIAN_POINT('Ctrl Pts',(21.7239293983343,9.99456437797395,37.234156982723));
#42775=CARTESIAN_POINT('Ctrl Pts',(21.7363085378277,9.99273310979356,37.2590811197142));
#42776=CARTESIAN_POINT('Ctrl Pts',(21.744599440101,9.9914595873496,37.2764196152406));
#42777=CARTESIAN_POINT('Ctrl Pts',(21.7857473129233,9.98488847437703,37.3658813017795));
#42778=CARTESIAN_POINT('Ctrl Pts',(21.8143921259442,9.9794506243686,37.4398469568211));
#42779=CARTESIAN_POINT('Ctrl Pts',(21.871046628862,9.96635915464611,37.6179963340078));
#42780=CARTESIAN_POINT('Ctrl Pts',(21.8950333370717,9.9586272905294,37.7231856738415));
#42781=CARTESIAN_POINT('Ctrl Pts',(21.9218704451539,9.94500781825628,37.9129166339437));
#42782=CARTESIAN_POINT('Ctrl Pts',(21.9281908260042,9.93910823600938,37.9967051917086));
#42783=CARTESIAN_POINT('Ctrl Pts',(21.9291267891915,9.93283719732254,38.090003750186));
#42784=CARTESIAN_POINT('Ctrl Pts',(21.9291525841898,9.93221167669767,38.0993601865164));
#42785=CARTESIAN_POINT('Ctrl Pts',(21.9290897784271,9.93128778414922,38.1132599052371));
#42786=CARTESIAN_POINT('Ctrl Pts',(21.9290532000281,9.93098665616662,38.1178031129038));
#42787=CARTESIAN_POINT('Ctrl Pts',(21.9289593299774,9.93045113961431,38.125906295107));
#42788=CARTESIAN_POINT('Ctrl Pts',(21.9289082332758,9.93021641405884,38.1294662714569));
#42789=CARTESIAN_POINT('Ctrl Pts',(21.9287764747286,9.92971021815369,38.1371614432153));
#42790=CARTESIAN_POINT('Ctrl Pts',(21.9286923706892,9.92943894053822,38.1412965176261));
#42791=CARTESIAN_POINT('Ctrl Pts',(21.928420731219,9.92868440134286,38.1528278205568));
#42792=CARTESIAN_POINT('Ctrl Pts',(21.928203942358,9.92820273009551,38.1602233859235));
#42793=CARTESIAN_POINT('Ctrl Pts',(21.9267005859875,9.92542308482274,38.2030877432137));
#42794=CARTESIAN_POINT('Ctrl Pts',(21.9244778427498,9.92317343600712,38.2385194939745));
#42795=CARTESIAN_POINT('Ctrl Pts',(21.9139970829203,9.9159190829748,38.3543312259466));
#42796=CARTESIAN_POINT('Ctrl Pts',(21.9016680714019,9.91106683073614,38.4342602797698));
#42797=CARTESIAN_POINT('Ctrl Pts',(21.8514305530821,9.8970416194577,38.6633715767694));
#42798=CARTESIAN_POINT('Ctrl Pts',(21.8006685042045,9.88792855439208,38.8090622710938));
#42799=CARTESIAN_POINT('Ctrl Pts',(21.7236352340713,9.87681237690304,38.9666569228625));
#42800=CARTESIAN_POINT('Ctrl Pts',(21.7137864337047,9.87542788984801,38.9859732735747));
#42801=CARTESIAN_POINT('Ctrl Pts',(21.6996860759464,9.87349308937315,39.0125129610778));
#42802=CARTESIAN_POINT('Ctrl Pts',(21.6957096331897,9.87295239194218,39.0198812408094));
#42803=CARTESIAN_POINT('Ctrl Pts',(21.6887795088047,9.87201835214705,39.0325250021952));
#42804=CARTESIAN_POINT('Ctrl Pts',(21.6858487375998,9.87162582273017,39.0378129566343));
#42805=CARTESIAN_POINT('Ctrl Pts',(21.6797422326439,9.87081298752134,39.0487097197133));
#42806=CARTESIAN_POINT('Ctrl Pts',(21.6765631534016,9.87039256630184,39.0543165572153));
#42807=CARTESIAN_POINT('Ctrl Pts',(21.6690740264862,9.8694084542222,39.0673719594894));
#42808=CARTESIAN_POINT('Ctrl Pts',(21.6647421442592,9.86884398597719,39.0748077774518));
#42809=CARTESIAN_POINT('Ctrl Pts',(21.6505906530725,9.86701501570477,39.098729828786));
#42810=CARTESIAN_POINT('Ctrl Pts',(21.6405750284971,9.86574346389546,39.1150981754499));
#42811=CARTESIAN_POINT('Ctrl Pts',(21.5880704421911,9.85918978854265,39.198098248913));
#42812=CARTESIAN_POINT('Ctrl Pts',(21.5417655895339,9.85376824297744,39.2622149037894));
#42813=CARTESIAN_POINT('Ctrl Pts',(21.42382340675,9.84074482274933,39.4060304183565));
#42814=CARTESIAN_POINT('Ctrl Pts',(21.3492198441774,9.83306642434861,39.4829648354101));
#42815=CARTESIAN_POINT('Ctrl Pts',(21.2046549156477,9.81942393050644,39.6091589882342));
#42816=CARTESIAN_POINT('Ctrl Pts',(21.1370525263523,9.81345144494535,39.660727217085));
#42817=CARTESIAN_POINT('Ctrl Pts',(21.0584688699067,9.80711368956272,39.7128464562181));
#42818=CARTESIAN_POINT('Ctrl Pts',(21.0506364875694,9.80648836383973,39.7179595234547));
#42819=CARTESIAN_POINT('Ctrl Pts',(21.0389451591874,9.80556470241084,39.7254710546045));
#42820=CARTESIAN_POINT('Ctrl Pts',(21.0351145726499,9.8052636126109,39.7279130860375));
#42821=CARTESIAN_POINT('Ctrl Pts',(21.0282664923011,9.80472813750468,39.7322448509045));
#42822=CARTESIAN_POINT('Ctrl Pts',(21.0252523671354,9.80449341542469,39.7341397788733));
#42823=CARTESIAN_POINT('Ctrl Pts',(21.0187251106484,9.80398719701102,39.738218182836));
#42824=CARTESIAN_POINT('Ctrl Pts',(21.0152102056271,9.80371589357096,39.7403987030064));
#42825=CARTESIAN_POINT('Ctrl Pts',(21.0053871895073,9.80296120951313,39.7464488821565));
#42826=CARTESIAN_POINT('Ctrl Pts',(20.9990637013461,9.80247942021881,39.750293624587));
#42827=CARTESIAN_POINT('Ctrl Pts',(20.9622601544136,9.79969770111211,39.7723814697535));
#42828=CARTESIAN_POINT('Ctrl Pts',(20.931300738835,9.79744618085657,39.7898176548111));
#42829=CARTESIAN_POINT('Ctrl Pts',(20.8283090852643,9.79018266543246,39.8441309247444));
#42830=CARTESIAN_POINT('Ctrl Pts',(20.7544333834276,9.78532356272082,39.8773353883116));
#42831=CARTESIAN_POINT('Ctrl Pts',(20.5349197014824,9.77130161209216,39.9598364114961));
#42832=CARTESIAN_POINT('Ctrl Pts',(20.3852352351913,9.76219781349318,39.9965015465132));
#42833=CARTESIAN_POINT('Ctrl Pts',(20.2112602955656,9.75109181437335,40.0176501751828));
#42834=CARTESIAN_POINT('Ctrl Pts',(20.1896847583094,9.74970665333064,40.0199043567324));
#42835=CARTESIAN_POINT('Ctrl Pts',(20.1597337905059,9.74777105946612,40.0225238114789));
#42836=CARTESIAN_POINT('Ctrl Pts',(20.1513865601794,9.74723025310996,40.0231991044382));
#42837=CARTESIAN_POINT('Ctrl Pts',(20.1370056597,9.74629607556473,40.0242683190484));
#42838=CARTESIAN_POINT('Ctrl Pts',(20.1309739989704,9.7459035178819,40.0246882668881));
#42839=CARTESIAN_POINT('Ctrl Pts',(20.1185088804897,9.74509067155156,40.0254972714536));
#42840=CARTESIAN_POINT('Ctrl Pts',(20.1120752556066,9.74467026768632,40.0258824555316));
#42841=CARTESIAN_POINT('Ctrl Pts',(20.0970487562776,9.74368627860025,40.0267065488306));
#42842=CARTESIAN_POINT('Ctrl Pts',(20.088454690224,9.74312191657721,40.0271202220249));
#42843=CARTESIAN_POINT('Ctrl Pts',(20.0606945402361,9.74129363927183,40.0282703670021));
#42844=CARTESIAN_POINT('Ctrl Pts',(20.0415206558564,9.74002268166886,40.0287784802007));
#42845=CARTESIAN_POINT('Ctrl Pts',(19.9433922951502,9.73347425938291,40.0299150673486));
#42846=CARTESIAN_POINT('Ctrl Pts',(19.8644702952461,9.72805762442425,40.025981678958));
#42847=CARTESIAN_POINT('Ctrl Pts',(19.6715366108952,9.71446481865499,40.0044484717718));
#42848=CARTESIAN_POINT('Ctrl Pts',(19.5584321425053,9.70618045046398,39.9814427942617));
#42849=CARTESIAN_POINT('Ctrl Pts',(19.3743846412666,9.69255631185649,39.9264886965181));
#42850=CARTESIAN_POINT('Ctrl Pts',(19.3020750178764,9.68717013762186,39.900099752653));
#42851=CARTESIAN_POINT('Ctrl Pts',(19.2230007051749,9.68137649435539,39.8657579258365));
#42852=CARTESIAN_POINT('Ctrl Pts',(19.2145015485332,9.68075509840767,39.8619935153268));
#42853=CARTESIAN_POINT('Ctrl Pts',(19.2019000544553,9.67983609853562,39.8563028115702));
#42854=CARTESIAN_POINT('Ctrl Pts',(19.1977769132116,9.67953578000136,39.8544233266439));
#42855=CARTESIAN_POINT('Ctrl Pts',(19.1904268798643,9.67900114077,39.8510415725895));
#42856=CARTESIAN_POINT('Ctrl Pts',(19.187197496407,9.6787664875804,39.8495448884342));
#42857=CARTESIAN_POINT('Ctrl Pts',(19.1802922818348,9.67826528684794,39.8463213640352));
#42858=CARTESIAN_POINT('Ctrl Pts',(19.1766177657984,9.67799890569718,39.8445918568131));
#42859=CARTESIAN_POINT('Ctrl Pts',(19.1665166372142,9.67726745677584,39.8397984735528));
#42860=CARTESIAN_POINT('Ctrl Pts',(19.1601014013035,9.67680383459057,39.8367105666686));
#42861=CARTESIAN_POINT('Ctrl Pts',(19.145729251475,9.67576692357286,39.8296944191807));
#42862=CARTESIAN_POINT('Ctrl Pts',(19.1377819946491,9.67519476332585,39.8257466250005));
#42863=CARTESIAN_POINT('Ctrl Pts',(19.113111069951,9.6734215000712,39.8132783914431));
#42864=CARTESIAN_POINT('Ctrl Pts',(19.0964838071241,9.67223058286875,39.8045683814513));
#42865=CARTESIAN_POINT('Ctrl Pts',(19.0311115708399,9.66755458028526,39.7690984584579));
#42866=CARTESIAN_POINT('Ctrl Pts',(18.9834029641842,9.66415558504402,39.7404773307421));
#42867=CARTESIAN_POINT('Ctrl Pts',(18.8350421150492,9.65341823802039,39.6425116137417));
#42868=CARTESIAN_POINT('Ctrl Pts',(18.7397166904998,9.64624241909166,39.5656587266026));
#42869=CARTESIAN_POINT('Ctrl Pts',(18.5976202782277,9.63415376555496,39.4269188401294));
#42870=CARTESIAN_POINT('Ctrl Pts',(18.5461681174707,9.62941539700512,39.3703358775547));
#42871=CARTESIAN_POINT('Ctrl Pts',(18.4900115667643,9.62369811854916,39.300686521365));
#42872=CARTESIAN_POINT('Ctrl Pts',(18.4819161749414,9.62285942838922,39.2904346591537));
#42873=CARTESIAN_POINT('Ctrl Pts',(18.4689295119072,9.62148968983956,39.2736406700217));
#42874=CARTESIAN_POINT('Ctrl Pts',(18.463974490419,9.62096114708986,39.2671481878404));
#42875=CARTESIAN_POINT('Ctrl Pts',(18.4552201706204,9.62001659735412,39.2555252439903));
#42876=CARTESIAN_POINT('Ctrl Pts',(18.4514048077431,9.61960122265204,39.2504069886976));
#42877=CARTESIAN_POINT('Ctrl Pts',(18.4434124302717,9.61872316185317,39.2395735189644));
#42878=CARTESIAN_POINT('Ctrl Pts',(18.4392413367565,9.61826025593173,39.2338540736025));
#42879=CARTESIAN_POINT('Ctrl Pts',(18.4282709743024,9.61703024767821,39.2186361680782));
#42880=CARTESIAN_POINT('Ctrl Pts',(18.4215264220232,9.61626107448402,39.209098805445));
#42881=CARTESIAN_POINT('Ctrl Pts',(18.3901798509238,9.61262382905547,39.1639070112198));
#42882=CARTESIAN_POINT('Ctrl Pts',(18.3666983929922,9.60971423449023,39.1274942298399));
#42883=CARTESIAN_POINT('Ctrl Pts',(18.281337322627,9.59838122471123,38.9847951859685));
#42884=CARTESIAN_POINT('Ctrl Pts',(18.2284540414812,9.58966000280737,38.8734860773268));
#42885=CARTESIAN_POINT('Ctrl Pts',(18.1688032042414,9.57717917568953,38.7090662829805));
#42886=CARTESIAN_POINT('Ctrl Pts',(18.1530600684469,9.57347048292888,38.6595145964407));
#42887=CARTESIAN_POINT('Ctrl Pts',(18.1340470662796,9.56838523903191,38.5900648133828));
#42888=CARTESIAN_POINT('Ctrl Pts',(18.1290585436424,9.56697651259576,38.5706612157791));
#42889=CARTESIAN_POINT('Ctrl Pts',(18.1134947759365,9.56232566692103,38.5059605850597));
#42890=CARTESIAN_POINT('Ctrl Pts',(18.1042545185894,9.55912236775163,38.4603551557423));
#42891=CARTESIAN_POINT('Ctrl Pts',(18.0954319979138,9.55549068614111,38.4069545475228));
#42892=CARTESIAN_POINT('Ctrl Pts',(18.0942369457064,9.55498272859598,38.3994454113471));
#42893=CARTESIAN_POINT('Ctrl Pts',(18.0923912445439,9.55417175310109,38.3873890902728));
#42894=CARTESIAN_POINT('Ctrl Pts',(18.0917123988027,9.55386722664874,38.3828463987725));
#42895=CARTESIAN_POINT('Ctrl Pts',(18.0905342963766,9.55332740788027,38.3747654478461));
#42896=CARTESIAN_POINT('Ctrl Pts',(18.0900286387866,9.55309176208119,38.371228178464));
#42897=CARTESIAN_POINT('Ctrl Pts',(18.0890687704878,9.55263666535322,38.3643777142746));
#42898=CARTESIAN_POINT('Ctrl Pts',(18.0886133485044,9.55241714493617,38.3610647594689));
#42899=CARTESIAN_POINT('Ctrl Pts',(18.0876307925645,9.55193545172768,38.3537767714693));
#42900=CARTESIAN_POINT('Ctrl Pts',(18.0871074311142,9.55167348782868,38.3498012327642));
#42901=CARTESIAN_POINT('Ctrl Pts',(18.0858454067869,9.55102810372736,38.3399781018139));
#42902=CARTESIAN_POINT('Ctrl Pts',(18.0851211340462,9.55064545435456,38.3341286546547));
#42903=CARTESIAN_POINT('Ctrl Pts',(18.0819461242232,9.54890974689848,38.3074855708987));
#42904=CARTESIAN_POINT('Ctrl Pts',(18.0798070880588,9.54757262754034,38.2866552908564));
#42905=CARTESIAN_POINT('Ctrl Pts',(18.0732936774698,9.54278424126604,38.2111472711882));
#42906=CARTESIAN_POINT('Ctrl Pts',(18.0709122189169,9.53941792722163,38.1563212933755));
#42907=CARTESIAN_POINT('Ctrl Pts',(18.0708705563808,9.53609590521103,38.1014651490007));
#42908=CARTESIAN_POINT('Ctrl Pts',(18.0708705582293,9.53609605247733,38.1014675807908));
#42909=CARTESIAN_POINT('Ctrl Pts',(18.0707475123805,9.52630106866043,37.9397242743709));
#42910=CARTESIAN_POINT('Ctrl Pts',(18.0909647819437,9.51688673489116,37.7786045611159));
#42911=CARTESIAN_POINT('Ctrl Pts',(18.1387402813931,9.50492507849212,37.5918503987071));
#42912=CARTESIAN_POINT('Ctrl Pts',(18.1471466991239,9.5029825872267,37.5620053481951));
#42913=CARTESIAN_POINT('Ctrl Pts',(18.1627822011627,9.49961511887058,37.5112186986139));
#42914=CARTESIAN_POINT('Ctrl Pts',(18.1696596305332,9.49820123441122,37.4901748373821));
#42915=CARTESIAN_POINT('Ctrl Pts',(18.1798769836897,9.49618870302921,37.4606426614083));
#42916=CARTESIAN_POINT('Ctrl Pts',(18.182917448527,9.49559985736207,37.4520520102845));
#42917=CARTESIAN_POINT('Ctrl Pts',(18.1882422042667,9.49458536469453,37.4373395004886));
#42918=CARTESIAN_POINT('Ctrl Pts',(18.1904969612513,9.49416069736462,37.4312070581813));
#42919=CARTESIAN_POINT('Ctrl Pts',(18.1948570029757,9.49334871223282,37.4195321702686));
#42920=CARTESIAN_POINT('Ctrl Pts',(18.1969567735783,9.49296158136236,37.4139877338231));
#42921=CARTESIAN_POINT('Ctrl Pts',(18.2024485930958,9.49195901337829,37.3996860044953));
#42922=CARTESIAN_POINT('Ctrl Pts',(18.2058790596842,9.49134230311789,37.3909437264771));
#42923=CARTESIAN_POINT('Ctrl Pts',(18.2176324755155,9.48926062737823,37.3616225052364));
#42924=CARTESIAN_POINT('Ctrl Pts',(18.2262464957679,9.48778597762043,37.3411628937835));
#42925=CARTESIAN_POINT('Ctrl Pts',(18.2930318561073,9.47671270814131,37.1898914672849));
#42926=CARTESIAN_POINT('Ctrl Pts',(18.3652402756797,9.46662090537987,37.0657933018514));
#42927=CARTESIAN_POINT('Ctrl Pts',(18.4920805803653,9.45142940711717,36.8947627891727));
#42928=CARTESIAN_POINT('Ctrl Pts',(18.5366881514936,9.4464400254975,36.8409778397677));
#42929=CARTESIAN_POINT('Ctrl Pts',(18.6092341047012,9.43894035552907,36.7625843765442));
#42930=CARTESIAN_POINT('Ctrl Pts',(18.635130367261,9.43636976574947,36.736166593274));
#42931=CARTESIAN_POINT('Ctrl Pts',(18.6720680551765,9.43286530381482,36.700591676009));
#42932=CARTESIAN_POINT('Ctrl Pts',(18.6824746359163,9.43189497741125,36.6907896361231));
#42933=CARTESIAN_POINT('Ctrl Pts',(18.7006119355222,9.43023429457237,36.674082535878));
#42934=CARTESIAN_POINT('Ctrl Pts',(18.708290979118,9.42954037513509,36.6671225545748));
#42935=CARTESIAN_POINT('Ctrl Pts',(18.7195805289102,9.42853398414788,36.6570546723713));
#42936=CARTESIAN_POINT('Ctrl Pts',(18.7231468886364,9.42821804744576,36.6538978688645));
#42937=CARTESIAN_POINT('Ctrl Pts',(18.7294285157419,9.42766509479738,36.6483789710895));
#42938=CARTESIAN_POINT('Ctrl Pts',(18.7321387537609,9.42742766441651,36.6460112210384));
#42939=CARTESIAN_POINT('Ctrl Pts',(18.7378414247173,9.42693049692422,36.641057256056));
#42940=CARTESIAN_POINT('Ctrl Pts',(18.7408351894679,9.42667087667347,36.6384726551028));
#42941=CARTESIAN_POINT('Ctrl Pts',(18.7488307319795,9.42598110222339,36.631612682091));
#42942=CARTESIAN_POINT('Ctrl Pts',(18.7538465256499,9.42555212272525,36.6273536154028));
#42943=CARTESIAN_POINT('Ctrl Pts',(18.7756221401123,9.4237053146275,36.6090541832584));
#42944=CARTESIAN_POINT('Ctrl Pts',(18.7925989584449,9.42230508157986,36.595272983099));
#42945=CARTESIAN_POINT('Ctrl Pts',(18.8136722356079,9.42060963220974,36.5787527779028));
#42946=CARTESIAN_POINT('Ctrl Pts',(18.8175488059204,9.42029947658223,36.5757376046465));
#42947=CARTESIAN_POINT('Ctrl Pts',(18.9576493762786,9.40915092542419,36.467624339207));
#42948=CARTESIAN_POINT('Ctrl Pts',(19.10732627959,9.39923735809111,36.3811939480628));
#42949=CARTESIAN_POINT('Ctrl Pts',(19.3084769628542,9.38604804867732,36.2985010871314));
#42950=CARTESIAN_POINT('Ctrl Pts',(19.3510383571465,9.38326871166235,36.2827358555299));
#42951=CARTESIAN_POINT('Ctrl Pts',(19.3941040511559,9.38044738890628,36.2684889691639));
#42952=CARTESIAN_POINT('Ctrl Pts',(19.3941038390373,9.20793124499895,36.2684890393365));
#42953=CARTESIAN_POINT('Ctrl Pts',(19.3501240934884,9.21069926390922,36.2830383156228));
#42954=CARTESIAN_POINT('Ctrl Pts',(19.3066595720485,9.21347421489961,36.2991746145473));
#42955=CARTESIAN_POINT('Ctrl Pts',(19.1874942354977,9.22127174790429,36.3483746531975));
#42956=CARTESIAN_POINT('Ctrl Pts',(19.1133014513578,9.22634940605603,36.3847390173774));
#42957=CARTESIAN_POINT('Ctrl Pts',(19.0246292538217,9.23284067912221,36.4354940588227));
#42958=CARTESIAN_POINT('Ctrl Pts',(19.0077381266876,9.23409693255132,36.4455077968246));
#42959=CARTESIAN_POINT('Ctrl Pts',(18.9836003409766,9.23592226083478,36.4603202351066));
#42960=CARTESIAN_POINT('Ctrl Pts',(18.9762282732511,9.23648386650944,36.4649130158542));
#42961=CARTESIAN_POINT('Ctrl Pts',(18.9634291409999,9.23746624533909,36.473007338139));
#42962=CARTESIAN_POINT('Ctrl Pts',(18.9579881373336,9.23788619852095,36.4764866665614));
#42963=CARTESIAN_POINT('Ctrl Pts',(18.9475059377085,9.23869982769704,36.4832640611803));
#42964=CARTESIAN_POINT('Ctrl Pts',(18.9424625107784,9.23909336789468,36.4865585524908));
#42965=CARTESIAN_POINT('Ctrl Pts',(18.9305160291075,9.24003053190812,36.4944423689675));
#42966=CARTESIAN_POINT('Ctrl Pts',(18.9236270063268,9.24057493237622,36.4990526412667));
#42967=CARTESIAN_POINT('Ctrl Pts',(18.8992506127762,9.24251561461815,36.5155942732559));
#42968=CARTESIAN_POINT('Ctrl Pts',(18.8819307013555,9.24392098794825,36.5277685591875));
#42969=CARTESIAN_POINT('Ctrl Pts',(18.734951916477,9.25608158223776,36.634737886082));
#42970=CARTESIAN_POINT('Ctrl Pts',(18.6174246854991,9.2674751429148,36.7450813449964));
#42971=CARTESIAN_POINT('Ctrl Pts',(18.4664009631485,9.28435420803083,36.9272248224959));
#42972=CARTESIAN_POINT('Ctrl Pts',(18.4213554586576,9.28976502358068,36.9885997210177));
#42973=CARTESIAN_POINT('Ctrl Pts',(18.361442343916,9.29740085717466,37.0812529312707));
#42974=CARTESIAN_POINT('Ctrl Pts',(18.3436038389566,9.29974083650397,37.110520896351));
#42975=CARTESIAN_POINT('Ctrl Pts',(18.3229101943336,9.3025256340672,37.1466029348882));
#42976=CARTESIAN_POINT('Ctrl Pts',(18.3193032091774,9.30301379832689,37.1529759867949));
#42977=CARTESIAN_POINT('Ctrl Pts',(18.3137239805373,9.30377306130415,37.162966002833));
#42978=CARTESIAN_POINT('Ctrl Pts',(18.3117269318189,9.30404568923033,37.1665689239666));
#42979=CARTESIAN_POINT('Ctrl Pts',(18.3080243513598,9.3045527124166,37.1732995886816));
#42980=CARTESIAN_POINT('Ctrl Pts',(18.3063159597765,9.30478728190548,37.1764256282661));
#42981=CARTESIAN_POINT('Ctrl Pts',(18.3024370637711,9.30532132677222,37.1835702462792));
#42982=CARTESIAN_POINT('Ctrl Pts',(18.300272167248,9.30562044715279,37.187591806487));
#42983=CARTESIAN_POINT('Ctrl Pts',(18.2946596981478,9.30639879380033,37.198106955948));
#42984=CARTESIAN_POINT('Ctrl Pts',(18.2912348885162,9.30687663117823,37.2046127061479));
#42985=CARTESIAN_POINT('Ctrl Pts',(18.2687690375852,9.31003148454768,37.247887103816));
#42986=CARTESIAN_POINT('Ctrl Pts',(18.2508772262192,9.31264253692699,37.2852441209302));
#42987=CARTESIAN_POINT('Ctrl Pts',(18.2278590751154,9.31618594056925,37.3375650386193));
#42988=CARTESIAN_POINT('Ctrl Pts',(18.2216943925456,9.31715562636448,37.3520563409197));
#42989=CARTESIAN_POINT('Ctrl Pts',(18.1694563902217,9.32557154291674,37.4791502036097));
#42990=CARTESIAN_POINT('Ctrl Pts',(18.1339517265813,9.33270997147971,37.5958062287506));
#42991=CARTESIAN_POINT('Ctrl Pts',(18.08945911872,9.34613947268664,37.8142821471299));
#42992=CARTESIAN_POINT('Ctrl Pts',(18.0770972984977,9.35234908399952,37.9149537258496));
#42993=CARTESIAN_POINT('Ctrl Pts',(18.0720603354054,9.35975131309222,38.0306902099867));
#42994=CARTESIAN_POINT('Ctrl Pts',(18.0715915218523,9.36068798874525,38.0452650025497));
#42995=CARTESIAN_POINT('Ctrl Pts',(18.0711275585347,9.36212757092115,38.0675490479106));
#42996=CARTESIAN_POINT('Ctrl Pts',(18.0710133057468,9.36262678064356,38.0752554998596));
#42997=CARTESIAN_POINT('Ctrl Pts',(18.0708946302922,9.36349964784425,38.0886922880725));
#42998=CARTESIAN_POINT('Ctrl Pts',(18.0708695531956,9.36387265932713,38.09442238259));
#42999=CARTESIAN_POINT('Ctrl Pts',(18.0708705727147,9.36471426490537,38.1073233343368));
#43000=CARTESIAN_POINT('Ctrl Pts',(18.0709111223382,9.36518330242469,38.114494074409));
#43001=CARTESIAN_POINT('Ctrl Pts',(18.0711275066883,9.36644699301404,38.1337610907952));
#43002=CARTESIAN_POINT('Ctrl Pts',(18.0713771447937,9.36724392313439,38.1458560553616));
#43003=CARTESIAN_POINT('Ctrl Pts',(18.0731898140528,9.37123704769623,38.2061742407294));
#43004=CARTESIAN_POINT('Ctrl Pts',(18.0764477118004,9.37448529224399,38.254325489858));
#43005=CARTESIAN_POINT('Ctrl Pts',(18.091252879719,9.38414275486742,38.3947285053799));
#43006=CARTESIAN_POINT('Ctrl Pts',(18.1076646370504,9.39068615082627,38.4863206825209));
#43007=CARTESIAN_POINT('Ctrl Pts',(18.1637587715744,9.40685838216643,38.7064504052619));
#43008=CARTESIAN_POINT('Ctrl Pts',(18.2103980126566,9.41653568545989,38.8327306887193));
#43009=CARTESIAN_POINT('Ctrl Pts',(18.2759986406667,9.42658321504773,38.9657712415146));
#43010=CARTESIAN_POINT('Ctrl Pts',(18.2823592781132,9.427529290171,38.9783227814374));
#43011=CARTESIAN_POINT('Ctrl Pts',(18.291406939334,9.4288355583237,38.9957024096441));
#43012=CARTESIAN_POINT('Ctrl Pts',(18.2939780404203,9.42920249014677,39.0005898782935));
#43013=CARTESIAN_POINT('Ctrl Pts',(18.2981434198537,9.42979005366411,39.0084260966459));
#43014=CARTESIAN_POINT('Ctrl Pts',(18.2997244337548,9.43001150196547,39.0113818034794));
#43015=CARTESIAN_POINT('Ctrl Pts',(18.3030520117823,9.43047429538931,39.0175639171299));
#43016=CARTESIAN_POINT('Ctrl Pts',(18.3048000854554,9.43071553836563,39.0207894801605));
#43017=CARTESIAN_POINT('Ctrl Pts',(18.3090759026668,9.43130112875833,39.0286258138788));
#43018=CARTESIAN_POINT('Ctrl Pts',(18.3116133407053,9.43164486778196,39.033231319371));
#43019=CARTESIAN_POINT('Ctrl Pts',(18.320697231118,9.43286233329601,39.0495604582404));
#43020=CARTESIAN_POINT('Ctrl Pts',(18.327347400683,9.43372975646454,39.0612263832182));
#43021=CARTESIAN_POINT('Ctrl Pts',(18.3690521875225,9.43903129738863,39.132642518273));
#43022=CARTESIAN_POINT('Ctrl Pts',(18.4071862134468,9.44329290629607,39.1905446988378));
#43023=CARTESIAN_POINT('Ctrl Pts',(18.5308569171335,9.45588991037731,39.3579501809029));
#43024=CARTESIAN_POINT('Ctrl Pts',(18.6251696972001,9.46401018240935,39.4603906310022));
#43025=CARTESIAN_POINT('Ctrl Pts',(18.7788142338452,9.47651626133117,39.5948288697938));
#43026=CARTESIAN_POINT('Ctrl Pts',(18.8301130726918,9.48058797385536,39.6353081805357));
#43027=CARTESIAN_POINT('Ctrl Pts',(18.8935671672071,9.48556432962506,39.6803498255568));
#43028=CARTESIAN_POINT('Ctrl Pts',(18.9038426363326,9.4863683165942,39.687494317102));
#43029=CARTESIAN_POINT('Ctrl Pts',(18.92079998754,9.48769247323145,39.6990415585192));
#43030=CARTESIAN_POINT('Ctrl Pts',(18.9274411413075,9.48821040876076,39.7035036838841));
#43031=CARTESIAN_POINT('Ctrl Pts',(18.9394158032488,9.48914322348645,39.7114416663877));
#43032=CARTESIAN_POINT('Ctrl Pts',(18.9447391513668,9.48955752978617,39.7149326989978));
#43033=CARTESIAN_POINT('Ctrl Pts',(18.9561005762446,9.4904410202715,39.7223033190187));
#43034=CARTESIAN_POINT('Ctrl Pts',(18.9621432050364,9.49091046348663,39.7261756782787));
#43035=CARTESIAN_POINT('Ctrl Pts',(18.9784523136573,9.4921763857583,39.7364992818736));
#43036=CARTESIAN_POINT('Ctrl Pts',(18.9887581036584,9.4929751558104,39.7428875161686));
#43037=CARTESIAN_POINT('Ctrl Pts',(19.0406676854646,9.49699330920741,39.7743911456416));
#43038=CARTESIAN_POINT('Ctrl Pts',(19.0831465328743,9.50026553160234,39.7980233223761));
#43039=CARTESIAN_POINT('Ctrl Pts',(19.2739225980985,9.51490566946668,39.894910734128));
#43040=CARTESIAN_POINT('Ctrl Pts',(19.4303813035583,9.52684801110277,39.9505165372845));
#43041=CARTESIAN_POINT('Ctrl Pts',(19.6593145691804,9.54341439066651,40.0000587903222));
#43042=CARTESIAN_POINT('Ctrl Pts',(19.7273979016863,9.54822056535423,40.011015509051));
#43043=CARTESIAN_POINT('Ctrl Pts',(19.8050739201912,9.55346924639649,40.0192787607443));
#43044=CARTESIAN_POINT('Ctrl Pts',(19.8142261826906,9.55408398824943,40.0201862501002));
#43045=CARTESIAN_POINT('Ctrl Pts',(19.8278775622705,9.55499508778264,40.0214413284848));
#43046=CARTESIAN_POINT('Ctrl Pts',(19.8323718113926,9.55529409381009,40.0218386258454));
#43047=CARTESIAN_POINT('Ctrl Pts',(19.8404125411351,9.55582731587694,40.02252101625));
#43048=CARTESIAN_POINT('Ctrl Pts',(19.843958442719,9.55606185711737,40.0228120677918));
#43049=CARTESIAN_POINT('Ctrl Pts',(19.8516508212141,9.55656934484548,40.0234220473183));
#43050=CARTESIAN_POINT('Ctrl Pts',(19.8557975207638,9.55684208958325,40.0237373772804));
#43051=CARTESIAN_POINT('Ctrl Pts',(19.8674284938225,9.55760487386947,40.0245840195274));
#43052=CARTESIAN_POINT('Ctrl Pts',(19.8749149954767,9.55809326623989,40.0250850886677));
#43053=CARTESIAN_POINT('Ctrl Pts',(19.9196068272948,9.56099437596235,40.0278144824805));
#43054=CARTESIAN_POINT('Ctrl Pts',(19.9568703169092,9.56335369628595,40.0290080389433));
#43055=CARTESIAN_POINT('Ctrl Pts',(20.1551208361316,9.57569958374174,40.0296094488459));
#43056=CARTESIAN_POINT('Ctrl Pts',(20.3155344280209,9.58501443592247,40.0099485250386));
#43057=CARTESIAN_POINT('Ctrl Pts',(20.5519671952843,9.59980926224643,39.9503337818635));
#43058=CARTESIAN_POINT('Ctrl Pts',(20.6308837347644,9.60492930420942,39.9249345229931));
#43059=CARTESIAN_POINT('Ctrl Pts',(20.7202482928829,9.61106662166177,39.8896817176314));
#43060=CARTESIAN_POINT('Ctrl Pts',(20.7325279212618,9.61191749704039,39.8846907531358));
#43061=CARTESIAN_POINT('Ctrl Pts',(20.7523424551433,9.61330321274557,39.8763983340653));
#43062=CARTESIAN_POINT('Ctrl Pts',(20.7599095249537,9.61383544877372,39.8731744757692));
#43063=CARTESIAN_POINT('Ctrl Pts',(20.773319057722,9.61478413761193,39.8673599054797));
#43064=CARTESIAN_POINT('Ctrl Pts',(20.7791697341692,9.61519993739894,39.8647883511207));
#43065=CARTESIAN_POINT('Ctrl Pts',(20.7914454097769,9.61607636742363,39.859319866422));
#43066=CARTESIAN_POINT('Ctrl Pts',(20.7978675153779,9.61653720475634,39.8564167087384));
#43067=CARTESIAN_POINT('Ctrl Pts',(20.8147636308329,9.61775586695601,39.8486669141415));
#43068=CARTESIAN_POINT('Ctrl Pts',(20.8252101779364,9.61851569503189,39.8437614238165));
#43069=CARTESIAN_POINT('Ctrl Pts',(20.8732730865031,9.6220415266545,39.820663423926));
#43070=CARTESIAN_POINT('Ctrl Pts',(20.9103336133401,9.62484601927103,39.801346747986));
#43071=CARTESIAN_POINT('Ctrl Pts',(21.0926750039765,9.63909265958647,39.6986429059937));
#43072=CARTESIAN_POINT('Ctrl Pts',(21.2272707971901,9.65116003616743,39.5977936628705));
#43073=CARTESIAN_POINT('Ctrl Pts',(21.354481044171,9.66375609817016,39.4736918323114));
#43074=CARTESIAN_POINT('Ctrl Pts',(21.3617790717965,9.66448314261507,39.4664574318117));
#43075=CARTESIAN_POINT('Ctrl Pts',(21.3817771862801,9.66648697180734,39.4463143298881));
#43076=CARTESIAN_POINT('Ctrl Pts',(21.3943540842626,9.66776031289888,39.433284360277));
#43077=CARTESIAN_POINT('Ctrl Pts',(21.4392335800274,9.67234696863018,39.3854583964633));
#43078=CARTESIAN_POINT('Ctrl Pts',(21.4704353312311,9.6756185948558,39.3496469023362));
#43079=CARTESIAN_POINT('Ctrl Pts',(21.5050923871608,9.67931811399798,39.3067716892547));
#43080=CARTESIAN_POINT('Ctrl Pts',(21.5098630480204,9.67982888795917,39.3007974786973));
#43081=CARTESIAN_POINT('Ctrl Pts',(21.5174504235336,9.68064348096734,39.2911792382944));
#43082=CARTESIAN_POINT('Ctrl Pts',(21.5202897642299,9.68094882949931,39.287553282802));
#43083=CARTESIAN_POINT('Ctrl Pts',(21.5253099315662,9.68148957070916,39.2810948090356));
#43084=CARTESIAN_POINT('Ctrl Pts',(21.5274959004492,9.68172532131815,39.2782663579121));
#43085=CARTESIAN_POINT('Ctrl Pts',(21.5321395100343,9.68222673180104,39.2722232942386));
#43086=CARTESIAN_POINT('Ctrl Pts',(21.5345948990082,9.68249223540639,39.2690070258332));
#43087=CARTESIAN_POINT('Ctrl Pts',(21.5412649181824,9.68321456880345,39.260212861489));
#43088=CARTESIAN_POINT('Ctrl Pts',(21.5454594271367,9.68367002167998,39.2546196753557));
#43089=CARTESIAN_POINT('Ctrl Pts',(21.5671680990639,9.68603427071463,39.2253419033744));
#43090=CARTESIAN_POINT('Ctrl Pts',(21.5841696012473,9.68791007500744,39.2012797802326));
#43091=CARTESIAN_POINT('Ctrl Pts',(21.6337956154844,9.69349178594968,39.1275154347867));
#43092=CARTESIAN_POINT('Ctrl Pts',(21.6646821873011,9.69711466392501,39.0766833731836));
#43093=CARTESIAN_POINT('Ctrl Pts',(21.7391969249331,9.7064840516289,38.9402138314247));
#43094=CARTESIAN_POINT('Ctrl Pts',(21.7788617621778,9.71215736207527,38.8526064159828));
#43095=CARTESIAN_POINT('Ctrl Pts',(21.8448967637367,9.72375810818517,38.6719857594255));
#43096=CARTESIAN_POINT('Ctrl Pts',(21.8711359817914,9.72967094720642,38.5792266550017));
#43097=CARTESIAN_POINT('Ctrl Pts',(21.8930569864779,9.73668660347681,38.4715683434059));
#43098=CARTESIAN_POINT('Ctrl Pts',(21.8956312137392,9.73755995052958,38.4582039560962));
#43099=CARTESIAN_POINT('Ctrl Pts',(21.899536911396,9.7389693187787,38.436704628201));
#43100=CARTESIAN_POINT('Ctrl Pts',(21.9009580567887,9.73950251404045,38.4285862858861));
#43101=CARTESIAN_POINT('Ctrl Pts',(21.9033922207678,9.74045343780786,38.4141364703876));
#43102=CARTESIAN_POINT('Ctrl Pts',(21.904425783656,9.74087051325671,38.4078085460165));
#43103=CARTESIAN_POINT('Ctrl Pts',(21.9065171595972,9.74174312251042,38.3945903448051));
#43104=CARTESIAN_POINT('Ctrl Pts',(21.9075692079511,9.74219883097318,38.3876992628191));
#43105=CARTESIAN_POINT('Ctrl Pts',(21.9102131191753,9.74338934335397,38.3697289006122));
#43106=CARTESIAN_POINT('Ctrl Pts',(21.9117459284203,9.74412598641252,38.3586413283726));
#43107=CARTESIAN_POINT('Ctrl Pts',(21.9180861499256,9.74739134347441,38.3096393981654));
#43108=CARTESIAN_POINT('Ctrl Pts',(21.9218624632354,9.74995193652486,38.2716026716396));
#43109=CARTESIAN_POINT('Ctrl Pts',(21.9290060262769,9.75696062438339,38.1686080392972));
#43110=CARTESIAN_POINT('Ctrl Pts',(21.9302220588169,9.76146926708123,38.1035552679438));
#43111=CARTESIAN_POINT('Ctrl Pts',(21.9237787942949,9.77570506015676,37.9013131273564));
#43112=CARTESIAN_POINT('Ctrl Pts',(21.9047630966813,9.78564853995499,37.7649225774155));
#43113=CARTESIAN_POINT('Ctrl Pts',(21.8604264278452,9.798403124821,37.5877398233219));
#43114=CARTESIAN_POINT('Ctrl Pts',(21.8478764530512,9.80152241654691,37.544166973035));
#43115=CARTESIAN_POINT('Ctrl Pts',(21.8314587178022,9.80507025048261,37.4938989527412));
#43116=CARTESIAN_POINT('Ctrl Pts',(21.8290735058185,9.80557439506994,37.4867385309838));
#43117=CARTESIAN_POINT('Ctrl Pts',(21.8251745025519,9.80638046926953,37.4752588248066));
#43118=CARTESIAN_POINT('Ctrl Pts',(21.8236872847086,9.80668387918572,37.470930695861));
#43119=CARTESIAN_POINT('Ctrl Pts',(21.8210121206036,9.80722244751244,37.4632346059124));
#43120=CARTESIAN_POINT('Ctrl Pts',(21.8198302094704,9.80745795336688,37.4598646080818));
#43121=CARTESIAN_POINT('Ctrl Pts',(21.8172832850434,9.8079602648716,37.4526665968217));
#43122=CARTESIAN_POINT('Ctrl Pts',(21.8159155341989,9.80822690691791,37.4488396154719));
#43123=CARTESIAN_POINT('Ctrl Pts',(21.8121349156973,9.80895556507878,37.4383659595681));
#43124=CARTESIAN_POINT('Ctrl Pts',(21.8096975521361,9.809416163433,37.4317281019501));
#43125=CARTESIAN_POINT('Ctrl Pts',(21.7965391787765,9.81185547899812,37.3964928766794));
#43126=CARTESIAN_POINT('Ctrl Pts',(21.7851760064855,9.81379866232296,37.3681378726281));
#43127=CARTESIAN_POINT('Ctrl Pts',(21.7094715498149,9.82584996041843,37.1914984530761));
#43128=CARTESIAN_POINT('Ctrl Pts',(21.6273749496718,9.835205202887,37.0515101290951));
#43129=CARTESIAN_POINT('Ctrl Pts',(21.4742835165198,9.85038971055659,36.8525983324099));
#43130=CARTESIAN_POINT('Ctrl Pts',(21.4149537175753,9.85589457628662,36.785684336338));
#43131=CARTESIAN_POINT('Ctrl Pts',(21.3416129671817,9.86245768215677,36.7137107427696));
#43132=CARTESIAN_POINT('Ctrl Pts',(21.3319207117148,9.86332042857703,36.7043960226969));
#43133=CARTESIAN_POINT('Ctrl Pts',(21.3161661976289,9.86471596343047,36.6895687841902));
#43134=CARTESIAN_POINT('Ctrl Pts',(21.3101646724415,9.86524601509756,36.6839921603347));
#43135=CARTESIAN_POINT('Ctrl Pts',(21.2994083428786,9.86619334422087,36.6741242915941));
#43136=CARTESIAN_POINT('Ctrl Pts',(21.2946673178167,9.86660998597644,36.6698181542562));
#43137=CARTESIAN_POINT('Ctrl Pts',(21.2847036890168,9.86748375082805,36.6608586180118));
#43138=CARTESIAN_POINT('Ctrl Pts',(21.2794770520499,9.8679410588422,36.6562098639211));
#43139=CARTESIAN_POINT('Ctrl Pts',(21.2657399517664,9.86914035445502,36.6441247795574));
#43140=CARTESIAN_POINT('Ctrl Pts',(21.2571893202924,9.86988423181042,36.6367347175733));
#43141=CARTESIAN_POINT('Ctrl Pts',(21.2186190101163,9.87322854541444,36.6039871532445));
#43142=CARTESIAN_POINT('Ctrl Pts',(21.1878955283131,9.87586279354813,36.5794768789033));
#43143=CARTESIAN_POINT('Ctrl Pts',(21.0252313208048,9.8896709579344,36.4576484044795));
#43144=CARTESIAN_POINT('Ctrl Pts',(20.8820395217641,9.90145038697358,36.376513317007));
#43145=CARTESIAN_POINT('Ctrl Pts',(20.6553671038989,9.91884322396282,36.2837949765454));
#43146=CARTESIAN_POINT('Ctrl Pts',(20.57851074932,9.92453015371424,36.257872082175));
#43147=CARTESIAN_POINT('Ctrl Pts',(20.4912302176463,9.9306039082824,36.2344377463513));
#43148=CARTESIAN_POINT('Ctrl Pts',(20.4821994595275,9.93122781836522,36.2320831552781));
#43149=CARTESIAN_POINT('Ctrl Pts',(20.4687518010566,9.93214980037734,36.2286809719913));
#43150=CARTESIAN_POINT('Ctrl Pts',(20.4643478815609,9.93245061215031,36.2275833258816));
#43151=CARTESIAN_POINT('Ctrl Pts',(20.4564828062857,9.93298578506149,36.2256524661782));
#43152=CARTESIAN_POINT('Ctrl Pts',(20.453023188383,9.93322048143339,36.2248132835683));
#43153=CARTESIAN_POINT('Ctrl Pts',(20.4455359639117,9.93372686260932,36.2230190745426));
#43154=CARTESIAN_POINT('Ctrl Pts',(20.4415076097524,9.93399835336069,36.2220674343853));
#43155=CARTESIAN_POINT('Ctrl Pts',(20.4302556048344,9.93475409051943,36.2194475187775));
#43156=CARTESIAN_POINT('Ctrl Pts',(20.4230252582531,9.93523673838637,36.2178078856434));
#43157=CARTESIAN_POINT('Ctrl Pts',(20.3808815217012,9.93803361802056,36.2085060240188));
#43158=CARTESIAN_POINT('Ctrl Pts',(20.3457674428849,9.94029882119903,36.2017730735065));
#43159=CARTESIAN_POINT('Ctrl Pts',(20.2297596889918,9.94762961023454,36.1828555795166));
#43160=CARTESIAN_POINT('Ctrl Pts',(20.1482729411872,9.95253904933887,36.1748377686137));
#43161=CARTESIAN_POINT('Ctrl Pts',(19.9142629416303,9.96653750933651,36.1667641825865));
#43162=CARTESIAN_POINT('Ctrl Pts',(19.7619420073179,9.97557349499058,36.179564193676));
#43163=CARTESIAN_POINT('Ctrl Pts',(19.5913941629291,9.98660491492779,36.2145139468371));
#43164=CARTESIAN_POINT('Ctrl Pts',(19.570145896334,9.98799482265803,36.2192443605353));
#43165=CARTESIAN_POINT('Ctrl Pts',(19.540828806502,9.98993600010771,36.2262938583384));
#43166=CARTESIAN_POINT('Ctrl Pts',(19.5326877089189,9.99047756939347,36.2283076884247));
#43167=CARTESIAN_POINT('Ctrl Pts',(19.5186972911352,9.99141271124057,36.2318654077675));
#43168=CARTESIAN_POINT('Ctrl Pts',(19.5128415785039,9.99180546637457,36.2333838575541));
#43169=CARTESIAN_POINT('Ctrl Pts',(19.5007637399878,9.99261838949213,36.2365764757403));
#43170=CARTESIAN_POINT('Ctrl Pts',(19.4945426735608,9.99303867122441,36.2382543236148));
#43171=CARTESIAN_POINT('Ctrl Pts',(19.4800451010952,9.99402179834448,36.2422424008804));
#43172=CARTESIAN_POINT('Ctrl Pts',(19.4717754453974,9.99458541646026,36.24457681111));
#43173=CARTESIAN_POINT('Ctrl Pts',(19.4451575598474,9.99640885071204,36.2522830479233));
#43174=CARTESIAN_POINT('Ctrl Pts',(19.4268739802495,9.99767565715358,36.2578722657269));
#43175=CARTESIAN_POINT('Ctrl Pts',(19.4038129569931,9.9992922053214,36.2652984767808));
#43176=CARTESIAN_POINT('Ctrl Pts',(19.3989552455726,9.99963378453239,36.2668841089014));
#43177=CARTESIAN_POINT('Ctrl Pts',(19.3941040084883,9.99997597504683,36.2684889832791));
#43178=CARTESIAN_POINT('Origin',(20.,-1.3495818343519,38.1));
#43179=CARTESIAN_POINT('',(19.394104009089,10.9665681892825,36.2684889830804));
#43180=CARTESIAN_POINT('',(19.3941039816494,10.7965035432258,36.2684889921579));
#43181=CARTESIAN_POINT('',(19.3941040087494,-1.3495818343519,36.2684889831927));
#43182=CARTESIAN_POINT('Ctrl Pts',(19.394104009089,10.9665681892825,36.2684889830804));
#43183=CARTESIAN_POINT('Ctrl Pts',(19.4101221984477,10.9653651090697,36.2631898848907));
#43184=CARTESIAN_POINT('Ctrl Pts',(19.4262144753514,10.9641606506422,36.258099414377));
#43185=CARTESIAN_POINT('Ctrl Pts',(19.5196416320679,10.9571968227119,36.2298897070823));
#43186=CARTESIAN_POINT('Ctrl Pts',(19.5982993265924,10.95144387542,36.2114304642891));
#43187=CARTESIAN_POINT('Ctrl Pts',(19.7128602090028,10.9433946150564,36.1920294699323));
#43188=CARTESIAN_POINT('Ctrl Pts',(19.747993522783,10.940970414967,36.1870718960526));
#43189=CARTESIAN_POINT('Ctrl Pts',(19.7905966448415,10.9380994983931,36.1822545757917));
#43190=CARTESIAN_POINT('Ctrl Pts',(19.7979519890166,10.9376063072648,36.1814656941188));
#43191=CARTESIAN_POINT('Ctrl Pts',(19.8094263256921,10.936840960956,36.1803017594435));
#43192=CARTESIAN_POINT('Ctrl Pts',(19.8135421967924,10.9365672372366,36.1798976202932));
#43193=CARTESIAN_POINT('Ctrl Pts',(19.8212038404275,10.9360592462178,36.1791701880052));
#43194=CARTESIAN_POINT('Ctrl Pts',(19.8247491746223,10.9358247981512,36.1788434780454));
#43195=CARTESIAN_POINT('Ctrl Pts',(19.8328211111554,10.9352924017041,36.1781221628661));
#43196=CARTESIAN_POINT('Ctrl Pts',(19.8373482090237,10.9349947997234,36.1777337339283));
#43197=CARTESIAN_POINT('Ctrl Pts',(19.8512032315691,10.934086909952,36.1765942572462));
#43198=CARTESIAN_POINT('Ctrl Pts',(19.860535454784,10.9334794233235,36.1758950707573));
#43199=CARTESIAN_POINT('Ctrl Pts',(19.9538653747992,10.9274410514853,36.1695852306295));
#43200=CARTESIAN_POINT('Ctrl Pts',(20.0381517457064,10.9222854391081,36.1694099671297));
#43201=CARTESIAN_POINT('Ctrl Pts',(20.229485091364,10.9107293279815,36.1815532947513));
#43202=CARTESIAN_POINT('Ctrl Pts',(20.3360223335846,10.9043925548724,36.1973201822815));
#43203=CARTESIAN_POINT('Ctrl Pts',(20.5177879137346,10.8930812134614,36.2399706261514));
#43204=CARTESIAN_POINT('Ctrl Pts',(20.5936885372475,10.8882011082911,36.2627887092187));
#43205=CARTESIAN_POINT('Ctrl Pts',(20.6859889230014,10.8819474425503,36.2968553043621));
#43206=CARTESIAN_POINT('Ctrl Pts',(20.7039100772579,10.8807180243232,36.303775582863));
#43207=CARTESIAN_POINT('Ctrl Pts',(20.7297086820844,10.878924756756,36.3141831225778));
#43208=CARTESIAN_POINT('Ctrl Pts',(20.7376712059795,10.8783680108792,36.3174574708248));
#43209=CARTESIAN_POINT('Ctrl Pts',(20.751556551582,10.8773912850768,36.3232763697998));
#43210=CARTESIAN_POINT('Ctrl Pts',(20.7574890771275,10.8769720971749,36.3257975299611));
#43211=CARTESIAN_POINT('Ctrl Pts',(20.7689601125839,10.8761578596574,36.3307404256888));
#43212=CARTESIAN_POINT('Ctrl Pts',(20.7745001015519,10.8757629359982,36.3331585562541));
#43213=CARTESIAN_POINT('Ctrl Pts',(20.787682648531,10.8748191356231,36.3389864744886));
#43214=CARTESIAN_POINT('Ctrl Pts',(20.7953145118461,10.8742694564744,36.3424200116768));
#43215=CARTESIAN_POINT('Ctrl Pts',(20.8226145052806,10.8722912389195,36.3549163629026));
#43216=CARTESIAN_POINT('Ctrl Pts',(20.8421514404493,10.8708531435323,36.3642602696513));
#43217=CARTESIAN_POINT('Ctrl Pts',(20.9995085046073,10.859082377676,36.4428012950546));
#43218=CARTESIAN_POINT('Ctrl Pts',(21.1287088513431,10.8481674527666,36.5279558749053));
#43219=CARTESIAN_POINT('Ctrl Pts',(21.3077920852644,10.8314256446526,36.6795430326499));
#43220=CARTESIAN_POINT('Ctrl Pts',(21.3659039263688,10.8256903006591,36.7353292535059));
#43221=CARTESIAN_POINT('Ctrl Pts',(21.4443266760484,10.8176622043977,36.8206576048344));
#43222=CARTESIAN_POINT('Ctrl Pts',(21.4675684444316,10.8152422396944,36.8473868264596));
#43223=CARTESIAN_POINT('Ctrl Pts',(21.4947587965076,10.8123756463806,36.880453624013));
#43224=CARTESIAN_POINT('Ctrl Pts',(21.4994219816135,10.8118827028729,36.886191552044));
#43225=CARTESIAN_POINT('Ctrl Pts',(21.5066414173815,10.811117656114,36.8951799748754));
#43226=CARTESIAN_POINT('Ctrl Pts',(21.5092203396905,10.8108439862713,36.8984120420991));
#43227=CARTESIAN_POINT('Ctrl Pts',(21.5140006069857,10.8103360431425,36.9044426420881));
#43228=CARTESIAN_POINT('Ctrl Pts',(21.516204575146,10.8101015894098,36.907238950739));
#43229=CARTESIAN_POINT('Ctrl Pts',(21.5212042455725,10.8095691133296,36.9136185877445));
#43230=CARTESIAN_POINT('Ctrl Pts',(21.5239950305894,10.8092714377985,36.9172056984092));
#43231=CARTESIAN_POINT('Ctrl Pts',(21.5324968523229,10.8083631002682,36.9282134856119));
#43232=CARTESIAN_POINT('Ctrl Pts',(21.538166663832,10.8077552434553,36.9356660442437));
#43233=CARTESIAN_POINT('Ctrl Pts',(21.5948052835147,10.8016584044776,37.0112492462203));
#43234=CARTESIAN_POINT('Ctrl Pts',(21.6412751425566,10.7964506823689,37.0826495425283));
#43235=CARTESIAN_POINT('Ctrl Pts',(21.735116451846,10.7848847107764,37.2501004817808));
#43236=CARTESIAN_POINT('Ctrl Pts',(21.7795162811571,10.7785857480623,37.3474839734465));
#43237=CARTESIAN_POINT('Ctrl Pts',(21.842318392228,10.7673260318283,37.5223806723267));
#43238=CARTESIAN_POINT('Ctrl Pts',(21.8644182278704,10.7624580138213,37.5982793183434));
#43239=CARTESIAN_POINT('Ctrl Pts',(21.8860265091716,10.7562188817615,37.6940263644846));
#43240=CARTESIAN_POINT('Ctrl Pts',(21.8899702747218,10.7549911231532,37.7128012079479));
#43241=CARTESIAN_POINT('Ctrl Pts',(21.895276363828,10.7531998403472,37.7400776425713));
#43242=CARTESIAN_POINT('Ctrl Pts',(21.8968628948534,10.752643397293,37.7485348483117));
#43243=CARTESIAN_POINT('Ctrl Pts',(21.8995387383085,10.7516670229008,37.7633448645011));
#43244=CARTESIAN_POINT('Ctrl Pts',(21.9006528994606,10.7512478818498,37.7696930931895));
#43245=CARTESIAN_POINT('Ctrl Pts',(21.9027505178823,10.7504336029172,37.7820069516984));
#43246=CARTESIAN_POINT('Ctrl Pts',(21.9037377846146,10.7500385903706,37.7879718632807));
#43247=CARTESIAN_POINT('Ctrl Pts',(21.9060254920436,10.7490943651428,37.802208965139));
#43248=CARTESIAN_POINT('Ctrl Pts',(21.9073001355414,10.7485443483725,37.8104851195592));
#43249=CARTESIAN_POINT('Ctrl Pts',(21.9116824559747,10.746563685114,37.8402249272867));
#43250=CARTESIAN_POINT('Ctrl Pts',(21.9144819238026,10.7451234508024,37.8617316650655));
#43251=CARTESIAN_POINT('Ctrl Pts',(21.934182036087,10.7333863479548,38.0359821081059));
#43252=CARTESIAN_POINT('Ctrl Pts',(21.9331346016458,10.7225117963139,38.1901711489178));
#43253=CARTESIAN_POINT('Ctrl Pts',(21.9036523115755,10.7057808353691,38.4227819587822));
#43254=CARTESIAN_POINT('Ctrl Pts',(21.8884517802785,10.700017110856,38.5022832903641));
#43255=CARTESIAN_POINT('Ctrl Pts',(21.8594594085048,10.6919548988771,38.6149894535106));
#43256=CARTESIAN_POINT('Ctrl Pts',(21.8496646697655,10.6895281109054,38.6491306146134));
#43257=CARTESIAN_POINT('Ctrl Pts',(21.8366960718268,10.686654553144,38.6900380073314));
#43258=CARTESIAN_POINT('Ctrl Pts',(21.8344193107956,10.6861612109778,38.6970788113017));
#43259=CARTESIAN_POINT('Ctrl Pts',(21.8308068323658,10.6853956819611,38.7080345440337));
#43260=CARTESIAN_POINT('Ctrl Pts',(21.8294989711216,10.6851219253832,38.7119584786884));
#43261=CARTESIAN_POINT('Ctrl Pts',(21.8270418403205,10.6846139051402,38.7192522479804));
#43262=CARTESIAN_POINT('Ctrl Pts',(21.8258958730318,10.6843794605122,38.7226230754436));
#43263=CARTESIAN_POINT('Ctrl Pts',(21.8232663861635,10.6838471125545,38.7302879346178));
#43264=CARTESIAN_POINT('Ctrl Pts',(21.8217770285472,10.6835495553709,38.7345799041406));
#43265=CARTESIAN_POINT('Ctrl Pts',(21.8171745878246,10.6826419382544,38.7476932770316));
#43266=CARTESIAN_POINT('Ctrl Pts',(21.8140124347702,10.6820346770347,38.7564974933627));
#43267=CARTESIAN_POINT('Ctrl Pts',(21.7819261411692,10.6760286253035,38.8438314656172));
#43268=CARTESIAN_POINT('Ctrl Pts',(21.7479809352931,10.6709018280553,38.920434311437));
#43269=CARTESIAN_POINT('Ctrl Pts',(21.6591398182736,10.6593517219655,39.0901683797451));
#43270=CARTESIAN_POINT('Ctrl Pts',(21.6011902314298,10.6529946338975,39.1813734606499));
#43271=CARTESIAN_POINT('Ctrl Pts',(21.4879315141877,10.6416548915286,39.3304034939366));
#43272=CARTESIAN_POINT('Ctrl Pts',(21.4360990455532,10.6367675934128,39.3905232593883));
#43273=CARTESIAN_POINT('Ctrl Pts',(21.3672910884871,10.6305052786167,39.4610390428862));
#43274=CARTESIAN_POINT('Ctrl Pts',(21.3536593352624,10.6292748737447,39.4745975987791));
#43275=CARTESIAN_POINT('Ctrl Pts',(21.3336312942754,10.6274804263415,39.4939312393025));
#43276=CARTESIAN_POINT('Ctrl Pts',(21.3273950924013,10.626923500559,39.4998710632389));
#43277=CARTESIAN_POINT('Ctrl Pts',(21.3164218113412,10.6259465659343,39.510183579809));
#43278=CARTESIAN_POINT('Ctrl Pts',(21.3117021632281,10.6255273501476,39.5145746878275));
#43279=CARTESIAN_POINT('Ctrl Pts',(21.3025150880464,10.6247131370261,39.5230367289546));
#43280=CARTESIAN_POINT('Ctrl Pts',(21.2980503587384,10.6243182660167,39.527110490231));
#43281=CARTESIAN_POINT('Ctrl Pts',(21.2873603558262,10.6233747173829,39.5367727223787));
#43282=CARTESIAN_POINT('Ctrl Pts',(21.2811177709472,10.6228252383072,39.542341774604));
#43283=CARTESIAN_POINT('Ctrl Pts',(21.2586001023722,10.6208484670549,39.5621684220729));
#43284=CARTESIAN_POINT('Ctrl Pts',(21.2421221437597,10.6194116361054,39.5761921378147));
#43285=CARTESIAN_POINT('Ctrl Pts',(21.1061191223381,10.6076260924644,39.6880492000287));
#43286=CARTESIAN_POINT('Ctrl Pts',(20.9754966135637,10.596693051929,39.7714627285026));
#43287=CARTESIAN_POINT('Ctrl Pts',(20.764000144649,10.5799460084695,39.8732159715951));
#43288=CARTESIAN_POINT('Ctrl Pts',(20.68952872574,10.5742230431937,39.9034807689238));
#43289=CARTESIAN_POINT('Ctrl Pts',(20.5798504460772,10.5662098364682,39.9402627397112));
#43290=CARTESIAN_POINT('Ctrl Pts',(20.5460117454975,10.5637928563546,39.950585057184));
#43291=CARTESIAN_POINT('Ctrl Pts',(20.5047797483321,10.5609293100268,39.9619330251845));
#43292=CARTESIAN_POINT('Ctrl Pts',(20.4976423031163,10.5604365413324,39.9638533545048));
#43293=CARTESIAN_POINT('Ctrl Pts',(20.4864954816977,10.5596717060532,39.9667838104939));
#43294=CARTESIAN_POINT('Ctrl Pts',(20.4824936912305,10.559398074251,39.967822124174));
#43295=CARTESIAN_POINT('Ctrl Pts',(20.4750392484167,10.5588901649145,39.9697307150923));
#43296=CARTESIAN_POINT('Ctrl Pts',(20.4715875576079,10.5586557071603,39.9706042901486));
#43297=CARTESIAN_POINT('Ctrl Pts',(20.4637236426423,10.5581231747591,39.9725713878697));
#43298=CARTESIAN_POINT('Ctrl Pts',(20.4593099662564,10.557825447223,39.9736588737963));
#43299=CARTESIAN_POINT('Ctrl Pts',(20.4457887087296,10.5569167930227,39.976939727686));
#43300=CARTESIAN_POINT('Ctrl Pts',(20.4366687937879,10.5563086743926,39.9790824056728));
#43301=CARTESIAN_POINT('Ctrl Pts',(20.3438462010594,10.5501641201339,40.0001783192774));
#43302=CARTESIAN_POINT('Ctrl Pts',(20.258970984391,10.5449138835771,40.0135950256768));
#43303=CARTESIAN_POINT('Ctrl Pts',(20.0676178241381,10.5333405997367,40.0308721477843));
#43304=CARTESIAN_POINT('Ctrl Pts',(19.9611539510819,10.52707329972,40.0316652488695));
#43305=CARTESIAN_POINT('Ctrl Pts',(19.776559284865,10.5158558966257,40.01776715696));
#43306=CARTESIAN_POINT('Ctrl Pts',(19.6983975116754,10.5109970366068,40.007037072446));
#43307=CARTESIAN_POINT('Ctrl Pts',(19.6023260564581,10.5047689158753,39.9877937534686));
#43308=CARTESIAN_POINT('Ctrl Pts',(19.5835928585912,10.5035424160711,39.9837502147542));
#43309=CARTESIAN_POINT('Ctrl Pts',(19.5565439798984,10.5017526388361,39.9774885605211));
#43310=CARTESIAN_POINT('Ctrl Pts',(19.54817761001,10.5011964256424,39.9754927514179));
#43311=CARTESIAN_POINT('Ctrl Pts',(19.5335663065199,10.5002203179191,39.9719037637646));
#43312=CARTESIAN_POINT('Ctrl Pts',(19.5273154437585,10.4998012123587,39.9703351036174));
#43313=CARTESIAN_POINT('Ctrl Pts',(19.5152148392156,10.4989869016947,39.9672339093337));
#43314=CARTESIAN_POINT('Ctrl Pts',(19.5093642051856,10.4985918214537,39.9657051320434));
#43315=CARTESIAN_POINT('Ctrl Pts',(19.4954254823834,10.4976472728008,39.9619928296369));
#43316=CARTESIAN_POINT('Ctrl Pts',(19.4873442940395,10.4970969990382,39.959784090925));
#43317=CARTESIAN_POINT('Ctrl Pts',(19.4583721185383,10.495114469747,39.9516622776921));
#43318=CARTESIAN_POINT('Ctrl Pts',(19.4375675667545,10.4936726028176,39.945449442693));
#43319=CARTESIAN_POINT('Ctrl Pts',(19.2707565096495,10.48195952663,39.8925522115349));
#43320=CARTESIAN_POINT('Ctrl Pts',(19.1307107244844,10.4711139029523,39.8289758729134));
#43321=CARTESIAN_POINT('Ctrl Pts',(18.9303191309305,10.454390838242,39.7074537961304));
#43322=CARTESIAN_POINT('Ctrl Pts',(18.8636653430635,10.4486068602331,39.6610477497868));
#43323=CARTESIAN_POINT('Ctrl Pts',(18.7722694426735,10.4405203199771,39.5884508856477));
#43324=CARTESIAN_POINT('Ctrl Pts',(18.7450257115796,10.4380886791583,39.5655539196107));
#43325=CARTESIAN_POINT('Ctrl Pts',(18.7128950501272,10.4352101693812,39.5369962492712));
#43326=CARTESIAN_POINT('Ctrl Pts',(18.7073894189618,10.4347165445197,39.5320458311687));
#43327=CARTESIAN_POINT('Ctrl Pts',(18.6988519857178,10.4339506735404,39.5242799993921));
#43328=CARTESIAN_POINT('Ctrl Pts',(18.6958005822549,10.4336768554702,39.5214863880075));
#43329=CARTESIAN_POINT('Ctrl Pts',(18.6901399592686,10.4331687805018,39.5162704211527));
#43330=CARTESIAN_POINT('Ctrl Pts',(18.6875284832723,10.4329343422743,39.5138506817323));
#43331=CARTESIAN_POINT('Ctrl Pts',(18.6816007977919,10.4324020849043,39.5083276349199));
#43332=CARTESIAN_POINT('Ctrl Pts',(18.6782888441936,10.4321046114337,39.5052198423452));
#43333=CARTESIAN_POINT('Ctrl Pts',(18.6697058281325,10.4313333749276,39.4971087249236));
#43334=CARTESIAN_POINT('Ctrl Pts',(18.6644519490188,10.4308609595768,39.4920872029184));
#43335=CARTESIAN_POINT('Ctrl Pts',(18.6306125887695,10.4278151097054,39.4593765033164));
#43336=CARTESIAN_POINT('Ctrl Pts',(18.6028590413918,10.4253025551288,39.4308358381864));
#43337=CARTESIAN_POINT('Ctrl Pts',(18.5643734789911,10.4217608851881,39.388726647215));
#43338=CARTESIAN_POINT('Ctrl Pts',(18.5529116337261,10.4206983190511,39.3758429250722));
#43339=CARTESIAN_POINT('Ctrl Pts',(18.4467379163231,10.4107624873512,39.2532262218638));
#43340=CARTESIAN_POINT('Ctrl Pts',(18.3645018310395,10.4023221614154,39.133297604032));
#43341=CARTESIAN_POINT('Ctrl Pts',(18.26250708063,10.3891048820596,38.9413677905178));
#43342=CARTESIAN_POINT('Ctrl Pts',(18.2321687264354,10.3846274852405,38.8755979885223));
#43343=CARTESIAN_POINT('Ctrl Pts',(18.1988738264377,10.3788578502581,38.7912471012287));
#43344=CARTESIAN_POINT('Ctrl Pts',(18.1923920902067,10.3776848655194,38.7741154617217));
#43345=CARTESIAN_POINT('Ctrl Pts',(18.1832795541511,10.3759592146978,38.7489535494239));
#43346=CARTESIAN_POINT('Ctrl Pts',(18.1804558798099,10.3754129125147,38.740993821054));
#43347=CARTESIAN_POINT('Ctrl Pts',(18.1755776566043,10.3744482396269,38.7269504753432));
#43348=CARTESIAN_POINT('Ctrl Pts',(18.1735010295625,10.3740306013608,38.7208746209553));
#43349=CARTESIAN_POINT('Ctrl Pts',(18.1695128566551,10.37321466642,38.7090127309221));
#43350=CARTESIAN_POINT('Ctrl Pts',(18.1675983146325,10.3728164736428,38.7032277765565));
#43351=CARTESIAN_POINT('Ctrl Pts',(18.1625292646284,10.3717444361701,38.6876643787747));
#43352=CARTESIAN_POINT('Ctrl Pts',(18.1594254516339,10.3710689481996,38.6778697521407));
#43353=CARTESIAN_POINT('Ctrl Pts',(18.1486411494774,10.3686519625019,38.6428694790411));
#43354=CARTESIAN_POINT('Ctrl Pts',(18.141399301703,10.3668963917609,38.6175327940379));
#43355=CARTESIAN_POINT('Ctrl Pts',(18.0921783046155,10.3539181838387,38.4309426067896));
#43356=CARTESIAN_POINT('Ctrl Pts',(18.0707382190134,10.3420192508737,38.2650273210922));
#43357=CARTESIAN_POINT('Ctrl Pts',(18.0709448114571,10.3235080837719,38.0051127617899));
#43358=CARTESIAN_POINT('Ctrl Pts',(18.0777953065008,10.3169155061858,37.9118750950458));
#43359=CARTESIAN_POINT('Ctrl Pts',(18.0927357498699,10.3100094244671,37.8102182461063));
#43360=CARTESIAN_POINT('Ctrl Pts',(18.0941660375926,10.3093828526717,37.8009560213759));
#43361=CARTESIAN_POINT('Ctrl Pts',(18.0963903565276,10.3084577137425,37.7872164463417));
#43362=CARTESIAN_POINT('Ctrl Pts',(18.0971327831626,10.3081563799409,37.7827310568363));
#43363=CARTESIAN_POINT('Ctrl Pts',(18.0984849245516,10.3076206398733,37.7747375636249));
#43364=CARTESIAN_POINT('Ctrl Pts',(18.0990884999661,10.3073858954797,37.7712284920566));
#43365=CARTESIAN_POINT('Ctrl Pts',(18.1004138069717,10.3068798204288,37.7636490823752));
#43366=CARTESIAN_POINT('Ctrl Pts',(18.1011389051305,10.3066086816481,37.7595793958716));
#43367=CARTESIAN_POINT('Ctrl Pts',(18.1031964946426,10.3058549211039,37.7482421125009));
#43368=CARTESIAN_POINT('Ctrl Pts',(18.1045576832612,10.305373884352,37.7409796975521));
#43369=CARTESIAN_POINT('Ctrl Pts',(18.1126684131882,10.3026053508087,37.6990384020968));
#43370=CARTESIAN_POINT('Ctrl Pts',(18.1203283513335,10.3003657286172,37.6645397877283));
#43371=CARTESIAN_POINT('Ctrl Pts',(18.1484474338735,10.2931603108146,37.5525338619101));
#43372=CARTESIAN_POINT('Ctrl Pts',(18.1727897677542,10.2883446256777,37.4760841470524));
#43373=CARTESIAN_POINT('Ctrl Pts',(18.257830253717,10.2743017478785,37.2572028192219));
#43374=CARTESIAN_POINT('Ctrl Pts',(18.3309650593214,10.2651390650128,37.1203170754948));
#43375=CARTESIAN_POINT('Ctrl Pts',(18.43205268078,10.253968439844,36.97592202711));
#43376=CARTESIAN_POINT('Ctrl Pts',(18.4447497331722,10.2525876669069,36.9584192394934));
#43377=CARTESIAN_POINT('Ctrl Pts',(18.4627619310325,10.2506572404359,36.9344479325156));
#43378=CARTESIAN_POINT('Ctrl Pts',(18.4678293250616,10.2501171452686,36.9277945905451));
#43379=CARTESIAN_POINT('Ctrl Pts',(18.4766326546844,10.2491838669968,36.9163906850465));
#43380=CARTESIAN_POINT('Ctrl Pts',(18.4803479753078,10.2487914937509,36.9116243011196));
#43381=CARTESIAN_POINT('Ctrl Pts',(18.4880728240719,10.247978719375,36.9018095588278));
#43382=CARTESIAN_POINT('Ctrl Pts',(18.4920853801294,10.2475582016561,36.896763690658));
#43383=CARTESIAN_POINT('Ctrl Pts',(18.5015185889721,10.2465734069415,36.8850225403936));
#43384=CARTESIAN_POINT('Ctrl Pts',(18.5069589115971,10.246008349327,36.8783433089318));
#43385=CARTESIAN_POINT('Ctrl Pts',(18.5246928589845,10.2441755309676,36.8568662571319));
#43386=CARTESIAN_POINT('Ctrl Pts',(18.5371628319802,10.2429006789327,36.842216219887));
#43387=CARTESIAN_POINT('Ctrl Pts',(18.6022186624103,10.2363177866212,36.7680632145053));
#43388=CARTESIAN_POINT('Ctrl Pts',(18.6582166143751,10.230868919598,36.7116690968204));
#43389=CARTESIAN_POINT('Ctrl Pts',(18.7983020392575,10.2177354878623,36.5870037778571));
#43390=CARTESIAN_POINT('Ctrl Pts',(18.8849791180935,10.2099717234808,36.5220388635909));
#43391=CARTESIAN_POINT('Ctrl Pts',(19.0472648203096,10.1963669467373,36.4204820220479));
#43392=CARTESIAN_POINT('Ctrl Pts',(19.1206945061303,10.1905116870977,36.3808984207502));
#43393=CARTESIAN_POINT('Ctrl Pts',(19.2049641320491,10.1842816895442,36.3422889943194));
#43394=CARTESIAN_POINT('Ctrl Pts',(19.2134943794653,10.1836564690104,36.3384555275738));
#43395=CARTESIAN_POINT('Ctrl Pts',(19.2262090591111,10.1827329323205,36.3328523632226));
#43396=CARTESIAN_POINT('Ctrl Pts',(19.2303722533585,10.1824318631306,36.3310352397469));
#43397=CARTESIAN_POINT('Ctrl Pts',(19.2378098716662,10.1818964103936,36.3278201444038));
#43398=CARTESIAN_POINT('Ctrl Pts',(19.2410817758008,10.181661690187,36.326416519583));
#43399=CARTESIAN_POINT('Ctrl Pts',(19.2481635832264,10.1811554596123,36.323401657706));
#43400=CARTESIAN_POINT('Ctrl Pts',(19.2519747800507,10.1808841422239,36.321793617562));
#43401=CARTESIAN_POINT('Ctrl Pts',(19.2626196094516,10.1801293799193,36.3173425745007));
#43402=CARTESIAN_POINT('Ctrl Pts',(19.269464565122,10.179647526862,36.3145265838545));
#43403=CARTESIAN_POINT('Ctrl Pts',(19.309269008668,10.1768646867237,36.2984184037044));
#43404=CARTESIAN_POINT('Ctrl Pts',(19.3425769949156,10.1746121548265,36.2859986408772));
#43405=CARTESIAN_POINT('Ctrl Pts',(19.3821662717714,10.172002320136,36.2724706186907));
#43406=CARTESIAN_POINT('Ctrl Pts',(19.388130481316,10.1716109234842,36.270465130908));
#43407=CARTESIAN_POINT('Ctrl Pts',(19.394104010895,10.1712205940279,36.2684889824829));
#43408=CARTESIAN_POINT('',(18.0708706529646,10.1603463946639,38.1015872324743));
#43409=CARTESIAN_POINT('Ctrl Pts',(19.3941040084883,9.99997597504683,36.2684889832791));
#43410=CARTESIAN_POINT('Ctrl Pts',(19.3745689141501,10.001353917181,36.2749515353715));
#43411=CARTESIAN_POINT('Ctrl Pts',(19.3551388044924,10.002741792661,36.2817261061457));
#43412=CARTESIAN_POINT('Ctrl Pts',(19.2733594970616,10.0086578068466,36.3117152820464));
#43413=CARTESIAN_POINT('Ctrl Pts',(19.2121307374123,10.0132746362667,36.3378339722369));
#43414=CARTESIAN_POINT('Ctrl Pts',(19.0358651373947,10.02709199074,36.4240496327043));
#43415=CARTESIAN_POINT('Ctrl Pts',(18.925402230502,10.0364680887741,36.4926407959781));
#43416=CARTESIAN_POINT('Ctrl Pts',(18.7827972608735,10.0490802422282,36.6025047087582));
#43417=CARTESIAN_POINT('Ctrl Pts',(18.7441478628999,10.052553720299,36.6347658671016));
#43418=CARTESIAN_POINT('Ctrl Pts',(18.7010434390228,10.0564526726847,36.6737059866913));
#43419=CARTESIAN_POINT('Ctrl Pts',(18.6953172141169,10.0569711560191,36.6789420867246));
#43420=CARTESIAN_POINT('Ctrl Pts',(18.6862182997434,10.0577956435505,36.6873635576435));
#43421=CARTESIAN_POINT('Ctrl Pts',(18.682825310752,10.0581032353062,36.6905267248648));
#43422=CARTESIAN_POINT('Ctrl Pts',(18.6768347457816,10.0586465064283,36.6961520467943));
#43423=CARTESIAN_POINT('Ctrl Pts',(18.6742325725197,10.058882555847,36.6986092283909));
#43424=CARTESIAN_POINT('Ctrl Pts',(18.6692154588179,10.0593377807267,36.7033732729611));
#43425=CARTESIAN_POINT('Ctrl Pts',(18.6667996806436,10.0595570289135,36.705679155066));
#43426=CARTESIAN_POINT('Ctrl Pts',(18.6600336273952,10.0601712880575,36.7121710752141));
#43427=CARTESIAN_POINT('Ctrl Pts',(18.6556969484201,10.0605652218622,36.7163713243501));
#43428=CARTESIAN_POINT('Ctrl Pts',(18.6377605635102,10.0621958357057,36.733907373454));
#43429=CARTESIAN_POINT('Ctrl Pts',(18.6243384616431,10.0634192160852,36.7474244032099));
#43430=CARTESIAN_POINT('Ctrl Pts',(18.589107196651,10.0666464094525,36.7839719241485));
#43431=CARTESIAN_POINT('Ctrl Pts',(18.5676613484233,10.0686277545001,36.8073459006618));
#43432=CARTESIAN_POINT('Ctrl Pts',(18.4922024140083,10.0757077884832,36.8937742541364));
#43433=CARTESIAN_POINT('Ctrl Pts',(18.4416941936894,10.0806607968453,36.9597724143537));
#43434=CARTESIAN_POINT('Ctrl Pts',(18.3191210866453,10.0938444526007,37.1433622856972));
#43435=CARTESIAN_POINT('Ctrl Pts',(18.2551440376971,10.1020733732418,37.2657450940994));
#43436=CARTESIAN_POINT('Ctrl Pts',(18.1965625550607,10.1122089605306,37.4146859204018));
#43437=CARTESIAN_POINT('Ctrl Pts',(18.1887447801219,10.1136353861665,37.4356232483476));
#43438=CARTESIAN_POINT('Ctrl Pts',(18.1781527163282,10.1156798811251,37.4655682096555));
#43439=CARTESIAN_POINT('Ctrl Pts',(18.1750777719302,10.1162880674129,37.4744681639007));
#43440=CARTESIAN_POINT('Ctrl Pts',(18.1701717254134,10.1172829679357,37.4890120746376));
#43441=CARTESIAN_POINT('Ctrl Pts',(18.1683012636492,10.1176683880984,37.4946426696896));
#43442=CARTESIAN_POINT('Ctrl Pts',(18.1644269700283,10.118479760742,37.5064877063497));
#43443=CARTESIAN_POINT('Ctrl Pts',(18.1624286585595,10.1189058875832,37.5127038613825));
#43444=CARTESIAN_POINT('Ctrl Pts',(18.1577241146364,10.1199277019056,37.5275973977282));
#43445=CARTESIAN_POINT('Ctrl Pts',(18.1550475978892,10.1205243465015,37.5362839313478));
#43446=CARTESIAN_POINT('Ctrl Pts',(18.1461042189783,10.1225717540805,37.566055401157));
#43447=CARTESIAN_POINT('Ctrl Pts',(18.1401368339267,10.1240321261214,37.5872277919941));
#43448=CARTESIAN_POINT('Ctrl Pts',(18.0921219256862,10.1366439167986,37.7694651422497));
#43449=CARTESIAN_POINT('Ctrl Pts',(18.0707337620348,10.1484844051065,37.9352093928769));
#43450=CARTESIAN_POINT('Ctrl Pts',(18.0708706529646,10.1603463946639,38.1015872324743));
#43451=CARTESIAN_POINT('Ctrl Pts',(18.0708706542009,10.1603465017403,38.1015887343413));
#43452=CARTESIAN_POINT('Ctrl Pts',(18.0709352769545,10.1659409537865,38.1800572656555));
#43453=CARTESIAN_POINT('Ctrl Pts',(18.0757874956902,10.1715085483743,38.258457138053));
#43454=CARTESIAN_POINT('Ctrl Pts',(18.0882688932751,10.1785084047994,38.3595647016621));
#43455=CARTESIAN_POINT('Ctrl Pts',(18.0915567020537,10.1800992157944,38.3827259361767));
#43456=CARTESIAN_POINT('Ctrl Pts',(18.0962288215372,10.1820772059349,38.411824968796));
#43457=CARTESIAN_POINT('Ctrl Pts',(18.0972208989003,10.182483780379,38.4178226012995));
#43458=CARTESIAN_POINT('Ctrl Pts',(18.0989271214245,10.1831610969617,38.4278431935512));
#43459=CARTESIAN_POINT('Ctrl Pts',(18.0996257176339,10.1834326583439,38.4318687042855));
#43460=CARTESIAN_POINT('Ctrl Pts',(18.1009219784398,10.1839262066194,38.4391998061884));
#43461=CARTESIAN_POINT('Ctrl Pts',(18.1015154959506,10.1841484203157,38.4425061003895));
#43462=CARTESIAN_POINT('Ctrl Pts',(18.1027559310396,10.1846051704734,38.4493138676983));
#43463=CARTESIAN_POINT('Ctrl Pts',(18.1034038984834,10.1848396354185,38.4528150555175));
#43464=CARTESIAN_POINT('Ctrl Pts',(18.1049014424658,10.1853722758184,38.4607834402523));
#43465=CARTESIAN_POINT('Ctrl Pts',(18.1057571206569,10.1856701035918,38.4652494334454));
#43466=CARTESIAN_POINT('Ctrl Pts',(18.1084254388448,10.1865793708479,38.4789144258778));
#43467=CARTESIAN_POINT('Ctrl Pts',(18.1102893895482,10.1871879967715,38.4881034396852));
#43468=CARTESIAN_POINT('Ctrl Pts',(18.1309504516299,10.1936640881798,38.5862801888146));
#43469=CARTESIAN_POINT('Ctrl Pts',(18.1559541064356,10.1992096620934,38.6738589164581));
#43470=CARTESIAN_POINT('Ctrl Pts',(18.2111499087872,10.2089186431627,38.8256239490101));
#43471=CARTESIAN_POINT('Ctrl Pts',(18.238866142833,10.2131048154481,38.8905203916707));
#43472=CARTESIAN_POINT('Ctrl Pts',(18.3079943050377,10.2224704338658,39.0305919247723));
#43473=CARTESIAN_POINT('Ctrl Pts',(18.350988892506,10.2276614763969,39.104810871593));
#43474=CARTESIAN_POINT('Ctrl Pts',(18.4194779264765,10.2353391129195,39.2067388905108));
#43475=CARTESIAN_POINT('Ctrl Pts',(18.4410688657087,10.2376888348495,39.2369496149498));
#43476=CARTESIAN_POINT('Ctrl Pts',(18.4702666225165,10.2407882426062,39.275407567422));
#43477=CARTESIAN_POINT('Ctrl Pts',(18.4770932736009,10.2415076630798,39.2842391016652));
#43478=CARTESIAN_POINT('Ctrl Pts',(18.4883028606127,10.2426808143607,39.2984835483605));
#43479=CARTESIAN_POINT('Ctrl Pts',(18.4926392082281,10.2431327042832,39.3039329292968));
#43480=CARTESIAN_POINT('Ctrl Pts',(18.5010257501155,10.2440030377826,39.3143557523066));
#43481=CARTESIAN_POINT('Ctrl Pts',(18.5050714342431,10.2444212978212,39.3193327177598));
#43482=CARTESIAN_POINT('Ctrl Pts',(18.5143814029875,10.2453802416169,39.3306697786118));
#43483=CARTESIAN_POINT('Ctrl Pts',(18.5196618191517,10.2459215706908,39.3370164051179));
#43484=CARTESIAN_POINT('Ctrl Pts',(18.5337857151164,10.2473628698212,39.3537722216733));
#43485=CARTESIAN_POINT('Ctrl Pts',(18.5426991516193,10.2482656749261,39.3641215661921));
#43486=CARTESIAN_POINT('Ctrl Pts',(18.6167985122066,10.2557172217791,39.4483326449094));
#43487=CARTESIAN_POINT('Ctrl Pts',(18.6874341208788,10.2624960425208,39.5171847300134));
#43488=CARTESIAN_POINT('Ctrl Pts',(18.8890225344465,10.2809959120808,39.6856354477209));
#43489=CARTESIAN_POINT('Ctrl Pts',(19.0279625851161,10.2929654556903,39.7744114923335));
#43490=CARTESIAN_POINT('Ctrl Pts',(19.1946612522752,10.305544866414,39.8531049257387));
#43491=CARTESIAN_POINT('Ctrl Pts',(19.2129901504729,10.3069046905234,39.8614093661923));
#43492=CARTESIAN_POINT('Ctrl Pts',(19.2369631539404,10.3086501048059,39.871822085772));
#43493=CARTESIAN_POINT('Ctrl Pts',(19.2424910805725,10.3090503143815,39.8741924843253));
#43494=CARTESIAN_POINT('Ctrl Pts',(19.2511160682032,10.3096711232071,39.8778432560461));
#43495=CARTESIAN_POINT('Ctrl Pts',(19.2542054710583,10.3098927716642,39.8791414523299));
#43496=CARTESIAN_POINT('Ctrl Pts',(19.2605897641369,10.3103493023631,39.8818046411333));
#43497=CARTESIAN_POINT('Ctrl Pts',(19.2638850113652,10.3105841085867,39.8831685281676));
#43498=CARTESIAN_POINT('Ctrl Pts',(19.2714468117089,10.3111210501096,39.8862737874096));
#43499=CARTESIAN_POINT('Ctrl Pts',(19.2757158306866,10.3114228154582,39.8880090142179));
#43500=CARTESIAN_POINT('Ctrl Pts',(19.2869382103075,10.3122126197885,39.8925237835756));
#43501=CARTESIAN_POINT('Ctrl Pts',(19.2939016905105,10.3126992022664,39.8952781991548));
#43502=CARTESIAN_POINT('Ctrl Pts',(19.3418611951529,10.3160276689795,39.9139264422164));
#43503=CARTESIAN_POINT('Ctrl Pts',(19.3833777536853,10.3187950940226,39.928456595436));
#43504=CARTESIAN_POINT('Ctrl Pts',(19.4486576654791,10.3230243920946,39.9488266307077));
#43505=CARTESIAN_POINT('Ctrl Pts',(19.4720937640836,10.3245188065941,39.9556544297385));
#43506=CARTESIAN_POINT('Ctrl Pts',(19.5566027997894,10.3298422263702,39.9785443261797));
#43507=CARTESIAN_POINT('Ctrl Pts',(19.6183277357985,10.333610152752,39.992050926724));
#43508=CARTESIAN_POINT('Ctrl Pts',(19.8199092623973,10.3458174644644,40.0258925883052));
#43509=CARTESIAN_POINT('Ctrl Pts',(19.9613398283213,10.354267903439,40.0339062768754));
#43510=CARTESIAN_POINT('Ctrl Pts',(20.1214528235252,10.3644604941376,40.0253978729783));
#43511=CARTESIAN_POINT('Ctrl Pts',(20.1405194323251,10.3656835920694,40.0241003105589));
#43512=CARTESIAN_POINT('Ctrl Pts',(20.1681250332468,10.3674692989962,40.0218091325499));
#43513=CARTESIAN_POINT('Ctrl Pts',(20.1766820185255,10.3680248893364,40.0210413397855));
#43514=CARTESIAN_POINT('Ctrl Pts',(20.1916468570121,10.3690002738514,40.019597758199));
#43515=CARTESIAN_POINT('Ctrl Pts',(20.1980570312033,10.3694192826215,40.0189469721179));
#43516=CARTESIAN_POINT('Ctrl Pts',(20.2104795092473,10.3702336780429,40.0176228861435));
#43517=CARTESIAN_POINT('Ctrl Pts',(20.2164921498367,10.3706289411123,40.0169533914352));
#43518=CARTESIAN_POINT('Ctrl Pts',(20.2308335874043,10.3715743653407,40.0152881693736));
#43519=CARTESIAN_POINT('Ctrl Pts',(20.2391591782037,10.3721253352737,40.0142663870391));
#43520=CARTESIAN_POINT('Ctrl Pts',(20.2690754749539,10.3741129451991,40.0103966114978));
#43521=CARTESIAN_POINT('Ctrl Pts',(20.2906235779385,10.3755592610023,40.0072374510516));
#43522=CARTESIAN_POINT('Ctrl Pts',(20.4622960855105,10.3872039789299,39.9790918425619));
#43523=CARTESIAN_POINT('Ctrl Pts',(20.6090099300316,10.3979675922106,39.936788775574));
#43524=CARTESIAN_POINT('Ctrl Pts',(20.8246847233666,10.4146684795706,39.8458945662411));
#43525=CARTESIAN_POINT('Ctrl Pts',(20.8980724662136,10.4205102164572,39.8093040253629));
#43526=CARTESIAN_POINT('Ctrl Pts',(20.9998505664068,10.4286660521415,39.750188244022));
#43527=CARTESIAN_POINT('Ctrl Pts',(21.0302824692156,10.4311114556584,39.7313616493725));
#43528=CARTESIAN_POINT('Ctrl Pts',(21.0663707241151,10.4340040028155,39.7076227873082));
#43529=CARTESIAN_POINT('Ctrl Pts',(21.0725426584164,10.4344984246822,39.703511708031));
#43530=CARTESIAN_POINT('Ctrl Pts',(21.0821228150311,10.4352652592268,39.6970503768493));
#43531=CARTESIAN_POINT('Ctrl Pts',(21.0855473555649,10.4355392501401,39.6947246259562));
#43532=CARTESIAN_POINT('Ctrl Pts',(21.0919029331634,10.4360474784253,39.6903783243166));
#43533=CARTESIAN_POINT('Ctrl Pts',(21.0948358362845,10.4362818981583,39.6883607026794));
#43534=CARTESIAN_POINT('Ctrl Pts',(21.101494845346,10.4368138993051,39.6837525867704));
#43535=CARTESIAN_POINT('Ctrl Pts',(21.1052174003785,10.4371111363833,39.6811570603093));
#43536=CARTESIAN_POINT('Ctrl Pts',(21.116564805273,10.4380168090292,39.6731855043083));
#43537=CARTESIAN_POINT('Ctrl Pts',(21.1241599842667,10.4386224633106,39.6677671809273));
#43538=CARTESIAN_POINT('Ctrl Pts',(21.1970705839275,10.4444344089309,39.6149512053395));
#43539=CARTESIAN_POINT('Ctrl Pts',(21.2593993963351,10.4493879628641,39.5635476591145));
#43540=CARTESIAN_POINT('Ctrl Pts',(21.4381357006637,10.4641674328672,39.3962397964793));
#43541=CARTESIAN_POINT('Ctrl Pts',(21.543134905801,10.4737374464768,39.269275794489));
#43542=CARTESIAN_POINT('Ctrl Pts',(21.6518517561269,10.4864392719816,39.0972369782981));
#43543=CARTESIAN_POINT('Ctrl Pts',(21.6718783960239,10.4889307615572,39.0632850573302));
#43544=CARTESIAN_POINT('Ctrl Pts',(21.696296696039,10.4921857042504,39.0188297237604));
#43545=CARTESIAN_POINT('Ctrl Pts',(21.7016557432144,10.4929147139332,39.0088664725818));
#43546=CARTESIAN_POINT('Ctrl Pts',(21.7101871469799,10.4940996386523,38.9926653592908));
#43547=CARTESIAN_POINT('Ctrl Pts',(21.7134137897006,10.4945536424513,38.9864562620348));
#43548=CARTESIAN_POINT('Ctrl Pts',(21.7195285857133,10.4954254216499,38.9745313093857));
#43549=CARTESIAN_POINT('Ctrl Pts',(21.722422202895,10.4958429992367,38.9688183478161));
#43550=CARTESIAN_POINT('Ctrl Pts',(21.7289503409683,10.4967967200319,38.955768841088));
#43551=CARTESIAN_POINT('Ctrl Pts',(21.7325666898277,10.4973334844451,38.9484233923756));
#43552=CARTESIAN_POINT('Ctrl Pts',(21.7419892288439,10.4987547225221,38.9289730523874));
#43553=CARTESIAN_POINT('Ctrl Pts',(21.7477159212063,10.4996419070503,38.9168303608091));
#43554=CARTESIAN_POINT('Ctrl Pts',(21.7899933635443,10.506373343065,38.8247063222588));
#43555=CARTESIAN_POINT('Ctrl Pts',(21.8211584396975,10.5123991818598,38.742381064723));
#43556=CARTESIAN_POINT('Ctrl Pts',(21.857138561599,10.5211145771021,38.6233600890604));
#43557=CARTESIAN_POINT('Ctrl Pts',(21.8666890615977,10.523688419848,38.5882020001733));
#43558=CARTESIAN_POINT('Ctrl Pts',(21.8949450428071,10.5322368138504,38.4711808205938));
#43559=CARTESIAN_POINT('Ctrl Pts',(21.9093025709464,10.5382611489536,38.3883670934481));
#43560=CARTESIAN_POINT('Ctrl Pts',(21.9250212246722,10.5487312788639,38.2412000422267));
#43561=CARTESIAN_POINT('Ctrl Pts',(21.9286482703333,10.5532048026547,38.1772122271859));
#43562=CARTESIAN_POINT('Ctrl Pts',(21.9291731189973,10.5584067857043,38.1002560000262));
#43563=CARTESIAN_POINT('Ctrl Pts',(21.9291316961775,10.5592728299215,38.0873544691316));
#43564=CARTESIAN_POINT('Ctrl Pts',(21.9288923212058,10.5604767802341,38.069279497368));
#43565=CARTESIAN_POINT('Ctrl Pts',(21.9288029730921,10.5608203494869,38.0641053121799));
#43566=CARTESIAN_POINT('Ctrl Pts',(21.9286150419257,10.5614044792397,38.0552795388353));
#43567=CARTESIAN_POINT('Ctrl Pts',(21.9285269063632,10.5616456118431,38.0516277778662));
#43568=CARTESIAN_POINT('Ctrl Pts',(21.9283375052746,10.5621081078961,38.044607017854));
#43569=CARTESIAN_POINT('Ctrl Pts',(21.9282377828284,10.5623295586608,38.0412380222649));
#43570=CARTESIAN_POINT('Ctrl Pts',(21.9279482679635,10.5629188882786,38.0322533845217));
#43571=CARTESIAN_POINT('Ctrl Pts',(21.9277427681328,10.5632859024816,38.0266382272589));
#43572=CARTESIAN_POINT('Ctrl Pts',(21.9269122234895,10.5646063711641,38.0063677069782));
#43573=CARTESIAN_POINT('Ctrl Pts',(21.9261445469413,10.565552290228,37.9917182427414));
#43574=CARTESIAN_POINT('Ctrl Pts',(21.9177483415487,10.5739795171772,37.8602160388294));
#43575=CARTESIAN_POINT('Ctrl Pts',(21.899660666174,10.5809660497249,37.7442581646185));
#43576=CARTESIAN_POINT('Ctrl Pts',(21.8341767007462,10.5970418487259,37.4831959467704));
#43577=CARTESIAN_POINT('Ctrl Pts',(21.7798999241105,10.6061154329658,37.3406583943935));
#43578=CARTESIAN_POINT('Ctrl Pts',(21.7023705840695,10.6167956764077,37.1924146604005));
#43579=CARTESIAN_POINT('Ctrl Pts',(21.6951174756711,10.6177780720611,37.1789389400326));
#43580=CARTESIAN_POINT('Ctrl Pts',(21.6838992128174,10.6192733693845,37.1586776706207));
#43581=CARTESIAN_POINT('Ctrl Pts',(21.6800515434783,10.6197821118376,37.1518274972547));
#43582=CARTESIAN_POINT('Ctrl Pts',(21.6730167971142,10.6207049771654,37.1394804926256));
#43583=CARTESIAN_POINT('Ctrl Pts',(21.6698441889629,10.6211185785751,37.1339755124999));
#43584=CARTESIAN_POINT('Ctrl Pts',(21.6629808945733,10.6220078390341,37.1222014403659));
#43585=CARTESIAN_POINT('Ctrl Pts',(21.6592818360192,10.6224837949027,37.1159373672581));
#43586=CARTESIAN_POINT('Ctrl Pts',(21.6492587401756,10.6237647179186,37.0991812147398));
#43587=CARTESIAN_POINT('Ctrl Pts',(21.6428701285082,10.6245720152212,37.0887283440504));
#43588=CARTESIAN_POINT('Ctrl Pts',(21.6122953015223,10.6283937742077,37.0397570848757));
#43589=CARTESIAN_POINT('Ctrl Pts',(21.5868531354346,10.6314539741804,37.0020438452081));
#43590=CARTESIAN_POINT('Ctrl Pts',(21.4427924566792,10.6481838413501,36.8039799040044));
#43591=CARTESIAN_POINT('Ctrl Pts',(21.3012133724693,10.6627652521498,36.6618985636947));
#43592=CARTESIAN_POINT('Ctrl Pts',(21.1080101421072,10.6794219046218,36.5202944995813));
#43593=CARTESIAN_POINT('Ctrl Pts',(21.0748764638824,10.6821753743147,36.4975652643608));
#43594=CARTESIAN_POINT('Ctrl Pts',(21.034605438134,10.6853801058381,36.4717516087254));
#43595=CARTESIAN_POINT('Ctrl Pts',(21.0281316559267,10.6858910343871,36.4676561210282));
#43596=CARTESIAN_POINT('Ctrl Pts',(21.0180770680163,10.6866778124796,36.4613788666111));
#43597=CARTESIAN_POINT('Ctrl Pts',(21.0145133467516,10.686955372716,36.459170086419));
#43598=CARTESIAN_POINT('Ctrl Pts',(21.0079147765544,10.687466857538,36.4551100349873));
#43599=CARTESIAN_POINT('Ctrl Pts',(21.0048820339142,10.6877009855418,36.4532555474239));
#43600=CARTESIAN_POINT('Ctrl Pts',(20.9980266130018,10.6882280905272,36.449089526444));
#43601=CARTESIAN_POINT('Ctrl Pts',(20.994201030031,10.6885207491733,36.4467828863591));
#43602=CARTESIAN_POINT('Ctrl Pts',(20.9829106389744,10.6893802077857,36.4400286944265));
#43603=CARTESIAN_POINT('Ctrl Pts',(20.9754236323362,10.6899446790255,36.4356181916699));
#43604=CARTESIAN_POINT('Ctrl Pts',(20.9202627753361,10.6940654617186,36.4036236801353));
#43605=CARTESIAN_POINT('Ctrl Pts',(20.8714518598468,10.6975049623196,36.3780391638108));
#43606=CARTESIAN_POINT('Ctrl Pts',(20.708105074409,10.7085702856281,36.3011483558419));
#43607=CARTESIAN_POINT('Ctrl Pts',(20.5896565834821,10.715921898939,36.2589164613412));
#43608=CARTESIAN_POINT('Ctrl Pts',(20.3811804371502,10.7288782260234,36.2067905676883));
#43609=CARTESIAN_POINT('Ctrl Pts',(20.2930268834515,10.7343582265289,36.1911593004242));
#43610=CARTESIAN_POINT('Ctrl Pts',(20.1837518312159,10.7413339392909,36.1795320540584));
#43611=CARTESIAN_POINT('Ctrl Pts',(20.1633571586141,10.7426432289965,36.1776898651474));
#43612=CARTESIAN_POINT('Ctrl Pts',(20.1341286410681,10.7445317543835,36.1755182278936));
#43613=CARTESIAN_POINT('Ctrl Pts',(20.1253153848545,10.745102771396,36.1749242525069));
#43614=CARTESIAN_POINT('Ctrl Pts',(20.110026972918,10.7460961705874,36.1739993105376));
#43615=CARTESIAN_POINT('Ctrl Pts',(20.1035536010687,10.746517678233,36.1736404176326));
#43616=CARTESIAN_POINT('Ctrl Pts',(20.0910986259198,10.7473304263732,36.1730128572742));
#43617=CARTESIAN_POINT('Ctrl Pts',(20.0851173305992,10.7477215126921,36.1727393931927));
#43618=CARTESIAN_POINT('Ctrl Pts',(20.0709952597496,10.7486467621112,36.1721596031678));
#43619=CARTESIAN_POINT('Ctrl Pts',(20.0628536765095,10.7491816559649,36.17187699187));
#43620=CARTESIAN_POINT('Ctrl Pts',(20.034396681097,10.7510565473495,36.1710696189872));
#43621=CARTESIAN_POINT('Ctrl Pts',(20.0140755594527,10.7524048520605,36.170814324209));
#43622=CARTESIAN_POINT('Ctrl Pts',(19.8244742170813,10.7650773821779,36.171428123064));
#43623=CARTESIAN_POINT('Ctrl Pts',(19.6560335694318,10.7771214248263,36.1942555700715));
#43624=CARTESIAN_POINT('Ctrl Pts',(19.4596217751291,10.7916335279829,36.2477811096073));
#43625=CARTESIAN_POINT('Ctrl Pts',(19.4267191744352,10.7940772742089,36.2576993133833));
#43626=CARTESIAN_POINT('Ctrl Pts',(19.3941039816494,10.7965035432258,36.2684889921579));
#43627=CARTESIAN_POINT('Origin',(20.,-1.3495818343519,38.1));
#43628=CARTESIAN_POINT('',(19.394104009052,11.7619801941422,36.2684889830926));
#43629=CARTESIAN_POINT('',(19.3941040036879,11.589834535998,36.2684889848672));
#43630=CARTESIAN_POINT('',(19.3941040087494,-1.3495818343519,36.2684889831927));
#43631=CARTESIAN_POINT('',(18.0708700189552,11.126372316702,38.0997295667639));
#43632=CARTESIAN_POINT('Ctrl Pts',(19.3941040090521,11.7619801941421,36.2684889830926));
#43633=CARTESIAN_POINT('Ctrl Pts',(19.4044891081785,11.7612816111124,36.265053410023));
#43634=CARTESIAN_POINT('Ctrl Pts',(19.4149032568815,11.7605802509376,36.2617062224656));
#43635=CARTESIAN_POINT('Ctrl Pts',(19.4333417291731,11.7593367408316,36.2559525142545));
#43636=CARTESIAN_POINT('Ctrl Pts',(19.4413541858722,11.7587957973654,36.2535093890524));
#43637=CARTESIAN_POINT('Ctrl Pts',(19.4551775088053,11.7578614464176,36.2493926471621));
#43638=CARTESIAN_POINT('Ctrl Pts',(19.4609808468757,11.7574688531459,36.2476940121907));
#43639=CARTESIAN_POINT('Ctrl Pts',(19.4729858020327,11.756655992765,36.2442413604791));
#43640=CARTESIAN_POINT('Ctrl Pts',(19.479188407167,11.7562356107018,36.2424910831708));
#43641=CARTESIAN_POINT('Ctrl Pts',(19.4936899410176,11.7552517762315,36.2384773232609));
#43642=CARTESIAN_POINT('Ctrl Pts',(19.5019954174636,11.7546875477548,36.2362382170528));
#43643=CARTESIAN_POINT('Ctrl Pts',(19.5288566781731,11.7528601414259,36.229188951451));
#43644=CARTESIAN_POINT('Ctrl Pts',(19.5474687807113,11.7515899306252,36.2245999200712));
#43645=CARTESIAN_POINT('Ctrl Pts',(19.6429945344472,11.7450481072071,36.202551706652));
#43646=CARTESIAN_POINT('Ctrl Pts',(19.7208487991724,11.739637640203,36.1895459509694));
#43647=CARTESIAN_POINT('Ctrl Pts',(19.9051343753092,11.7266644358477,36.1702661899108));
#43648=CARTESIAN_POINT('Ctrl Pts',(20.0117272473897,11.7190265464471,36.1679720693119));
#43649=CARTESIAN_POINT('Ctrl Pts',(20.2034270806906,11.7053700045545,36.1797154639987));
#43650=CARTESIAN_POINT('Ctrl Pts',(20.2884659233915,11.6993454636034,36.1906371933352));
#43651=CARTESIAN_POINT('Ctrl Pts',(20.38169698589,11.6929589644814,36.2089850068213));
#43652=CARTESIAN_POINT('Ctrl Pts',(20.3908744169038,11.6923327222023,36.2108606477118));
#43653=CARTESIAN_POINT('Ctrl Pts',(20.4044846305104,11.6914079739603,36.2137456690271));
#43654=CARTESIAN_POINT('Ctrl Pts',(20.4089279258414,11.6911067046575,36.2147039569472));
#43655=CARTESIAN_POINT('Ctrl Pts',(20.4168456537537,11.6905710346533,36.2164408862365));
#43656=CARTESIAN_POINT('Ctrl Pts',(20.4203213485379,11.690336296182,36.2172134484282));
#43657=CARTESIAN_POINT('Ctrl Pts',(20.4278283700572,11.6898301833444,36.2189039004153));
#43658=CARTESIAN_POINT('Ctrl Pts',(20.431858882062,11.6895590011233,36.2198251259853));
#43659=CARTESIAN_POINT('Ctrl Pts',(20.4430870462426,11.688804996969,36.2224294781767));
#43660=CARTESIAN_POINT('Ctrl Pts',(20.4502781276192,11.6883237617114,36.2241410481966));
#43661=CARTESIAN_POINT('Ctrl Pts',(20.491830317535,11.6855517581262,36.2342837170584));
#43662=CARTESIAN_POINT('Ctrl Pts',(20.5259666613401,11.6833090048776,36.2436180985407));
#43663=CARTESIAN_POINT('Ctrl Pts',(20.6367183710823,11.6760883336552,36.2772032930524));
#43664=CARTESIAN_POINT('Ctrl Pts',(20.7120822538879,11.6712612540214,36.3053024932868));
#43665=CARTESIAN_POINT('Ctrl Pts',(20.9264804106436,11.6572239287648,36.4008799376506));
#43666=CARTESIAN_POINT('Ctrl Pts',(21.0594091813543,11.6480767351947,36.4804257125253));
#43667=CARTESIAN_POINT('Ctrl Pts',(21.1985418401572,11.6369230974557,36.5882102153351));
#43668=CARTESIAN_POINT('Ctrl Pts',(21.2154250937131,11.6355411459726,36.6017501285546));
#43669=CARTESIAN_POINT('Ctrl Pts',(21.2385142355628,11.6336093312208,36.6209141197064));
#43670=CARTESIAN_POINT('Ctrl Pts',(21.2449170838421,11.6330690445826,36.6262992149943));
#43671=CARTESIAN_POINT('Ctrl Pts',(21.2558848672494,11.6321355242298,36.6356461189588));
#43672=CARTESIAN_POINT('Ctrl Pts',(21.2604666215982,11.6317431013556,36.6395880775738));
#43673=CARTESIAN_POINT('Ctrl Pts',(21.2698966061139,11.630930307761,36.6477786936579));
#43674=CARTESIAN_POINT('Ctrl Pts',(21.2747422104012,11.6305098208214,36.6520302461213));
#43675=CARTESIAN_POINT('Ctrl Pts',(21.2860110471288,11.6295252436052,36.6620179748811));
#43676=CARTESIAN_POINT('Ctrl Pts',(21.2924173188268,11.6289603737401,36.6677729970963));
#43677=CARTESIAN_POINT('Ctrl Pts',(21.3129981639976,11.627128781812,36.6865121571082));
#43678=CARTESIAN_POINT('Ctrl Pts',(21.3270168934776,11.6258549817018,36.6996649758481));
#43679=CARTESIAN_POINT('Ctrl Pts',(21.3978402073543,11.619281409724,36.7681322880924));
#43680=CARTESIAN_POINT('Ctrl Pts',(21.4513851287496,11.6138412600597,36.8266944002168));
#43681=CARTESIAN_POINT('Ctrl Pts',(21.5688754656985,11.600740761414,36.9722620377601));
#43682=CARTESIAN_POINT('Ctrl Pts',(21.6294271448523,11.5930019546244,37.0616707265058));
#43683=CARTESIAN_POINT('Ctrl Pts',(21.7232099611914,11.579385560088,37.228729786257));
#43684=CARTESIAN_POINT('Ctrl Pts',(21.7594303467048,11.5734955139161,37.30440419551));
#43685=CARTESIAN_POINT('Ctrl Pts',(21.7940981209714,11.5672333016133,37.3908864627234));
#43686=CARTESIAN_POINT('Ctrl Pts',(21.7975159053477,11.5666078437841,37.3995953633059));
#43687=CARTESIAN_POINT('Ctrl Pts',(21.8024991682618,11.5656840256995,37.4125700435162));
#43688=CARTESIAN_POINT('Ctrl Pts',(21.8041130871613,11.5653829100184,37.4168168865981));
#43689=CARTESIAN_POINT('Ctrl Pts',(21.8069650112877,11.5648474068196,37.4244019829029));
#43690=CARTESIAN_POINT('Ctrl Pts',(21.8082087890132,11.5646126823845,37.4277379909748));
#43691=CARTESIAN_POINT('Ctrl Pts',(21.810877506984,11.5641064792307,37.4349569050847));
#43692=CARTESIAN_POINT('Ctrl Pts',(21.8122991947508,11.5638351932976,37.4388409473546));
#43693=CARTESIAN_POINT('Ctrl Pts',(21.8162293395495,11.5630806074456,37.449686006512));
#43694=CARTESIAN_POINT('Ctrl Pts',(21.8187102895848,11.5625988981783,37.4566570192788));
#43695=CARTESIAN_POINT('Ctrl Pts',(21.8328619682382,11.5598185851996,37.4971567951531));
#43696=CARTESIAN_POINT('Ctrl Pts',(21.8436463480084,11.5575683338466,37.5309908132421));
#43697=CARTESIAN_POINT('Ctrl Pts',(21.8759023823103,11.550311031841,37.6427629675267));
#43698=CARTESIAN_POINT('Ctrl Pts',(21.8934125656299,11.5454565748662,37.7217586844452));
#43699=CARTESIAN_POINT('Ctrl Pts',(21.9296881269651,11.5314324146581,37.9534749478192));
#43700=CARTESIAN_POINT('Ctrl Pts',(21.9352265552165,11.5223223328693,38.107601150019));
#43701=CARTESIAN_POINT('Ctrl Pts',(21.9206143802755,11.5112094319007,38.282354584335));
#43702=CARTESIAN_POINT('Ctrl Pts',(21.9184433106685,11.5098247271884,38.3039313502964));
#43703=CARTESIAN_POINT('Ctrl Pts',(21.9149304248526,11.5078896704848,38.3337822450996));
#43704=CARTESIAN_POINT('Ctrl Pts',(21.9138976713883,11.5073489378651,38.3420916561724));
#43705=CARTESIAN_POINT('Ctrl Pts',(21.9120261209,11.5064148535698,38.3563888137574));
#43706=CARTESIAN_POINT('Ctrl Pts',(21.9112132041025,11.5060223150222,38.3623798732914));
#43707=CARTESIAN_POINT('Ctrl Pts',(21.9094755146625,11.5052094762245,38.3747496283011));
#43708=CARTESIAN_POINT('Ctrl Pts',(21.9085469115264,11.5047890606146,38.3811277008114));
#43709=CARTESIAN_POINT('Ctrl Pts',(21.9063039393352,11.5038049882842,38.3960099590994));
#43710=CARTESIAN_POINT('Ctrl Pts',(21.9049646050337,11.5032405543671,38.4045101879026));
#43711=CARTESIAN_POINT('Ctrl Pts',(21.9004555137718,11.5014118080604,38.4319329832436));
#43712=CARTESIAN_POINT('Ctrl Pts',(21.8970604060537,11.5001404483009,38.4508168126058));
#43713=CARTESIAN_POINT('Ctrl Pts',(21.8782463902904,11.4935884710089,38.5471850493148));
#43714=CARTESIAN_POINT('Ctrl Pts',(21.8583617419863,11.4881685128589,38.6237105414434));
#43715=CARTESIAN_POINT('Ctrl Pts',(21.8006607427853,11.4751520921861,38.800423663352));
#43716=CARTESIAN_POINT('Ctrl Pts',(21.7590865108009,11.467479292573,38.8991147880653));
#43717=CARTESIAN_POINT('Ctrl Pts',(21.6701682482757,11.4538356887566,39.0691785123149));
#43718=CARTESIAN_POINT('Ctrl Pts',(21.6258388761496,11.4478568294055,39.1418351589144));
#43719=CARTESIAN_POINT('Ctrl Pts',(21.5714609862753,11.4415124952514,39.218990882663));
#43720=CARTESIAN_POINT('Ctrl Pts',(21.5660112163951,11.4408864935662,39.226605124111));
#43721=CARTESIAN_POINT('Ctrl Pts',(21.5578341665533,11.4399620305949,39.237855843497));
#43722=CARTESIAN_POINT('Ctrl Pts',(21.5551492258448,11.4396608083972,39.2415227100084));
#43723=CARTESIAN_POINT('Ctrl Pts',(21.5503377478702,11.4391251895512,39.2480453393494));
#43724=CARTESIAN_POINT('Ctrl Pts',(21.5482162445073,11.4388904553942,39.2509047287409));
#43725=CARTESIAN_POINT('Ctrl Pts',(21.5436138237458,11.4383843149102,39.2570721746336));
#43726=CARTESIAN_POINT('Ctrl Pts',(21.5411301890773,11.4381131009247,39.2603781259911));
#43727=CARTESIAN_POINT('Ctrl Pts',(21.5341757510771,11.4373589186249,39.2695734235797));
#43728=CARTESIAN_POINT('Ctrl Pts',(21.5296816305831,11.4368775382034,39.2754451674588));
#43729=CARTESIAN_POINT('Ctrl Pts',(21.5034662142887,11.4341029933899,39.3092916452899));
#43730=CARTESIAN_POINT('Ctrl Pts',(21.4810099799045,11.4318579470929,39.3366918632568));
#43731=CARTESIAN_POINT('Ctrl Pts',(21.405092404967,11.4246260889572,39.4242873599754));
#43732=CARTESIAN_POINT('Ctrl Pts',(21.3486145402051,11.419790650427,39.4817607124033));
#43733=CARTESIAN_POINT('Ctrl Pts',(21.1739862551003,11.4057576538502,39.638527125597));
#43734=CARTESIAN_POINT('Ctrl Pts',(21.0473504373242,11.3966220873006,39.7273783367911));
#43735=CARTESIAN_POINT('Ctrl Pts',(20.8924091828192,11.3854810264254,39.8104436489183));
#43736=CARTESIAN_POINT('Ctrl Pts',(20.8731508924725,11.3840980144002,39.8203543485665));
#43737=CARTESIAN_POINT('Ctrl Pts',(20.8462255066924,11.3821649506419,39.8336421170417));
#43738=CARTESIAN_POINT('Ctrl Pts',(20.8386966625309,11.3816244919909,39.8372968954115));
#43739=CARTESIAN_POINT('Ctrl Pts',(20.825689315217,11.3806907541416,39.8435068832587));
#43740=CARTESIAN_POINT('Ctrl Pts',(20.8202221005183,11.3802982866656,39.8460855653937));
#43741=CARTESIAN_POINT('Ctrl Pts',(20.8089000169826,11.3794854757088,39.8513608623392));
#43742=CARTESIAN_POINT('Ctrl Pts',(20.8030435785427,11.3790650163406,39.8540539093432));
#43743=CARTESIAN_POINT('Ctrl Pts',(20.7893340927644,11.3780806341408,39.8602750819948));
#43744=CARTESIAN_POINT('Ctrl Pts',(20.7814707561896,11.3775159326444,39.8637800677702));
#43745=CARTESIAN_POINT('Ctrl Pts',(20.7559879087411,11.3756854400817,39.8749348729003));
#43746=CARTESIAN_POINT('Ctrl Pts',(20.7382779897368,11.3744125828281,39.8823740028251));
#43747=CARTESIAN_POINT('Ctrl Pts',(20.6470127824749,11.3678473587451,39.9191168018251));
#43748=CARTESIAN_POINT('Ctrl Pts',(20.571824014896,11.362415015562,39.9441328264967));
#43749=CARTESIAN_POINT('Ctrl Pts',(20.3914487583912,11.3493457414456,39.9920520667622));
#43750=CARTESIAN_POINT('Ctrl Pts',(20.2854579677333,11.3416311068129,40.0109171279271));
#43751=CARTESIAN_POINT('Ctrl Pts',(20.0945721445837,11.3280042424927,40.0286513738939));
#43752=CARTESIAN_POINT('Ctrl Pts',(20.0102555688925,11.3220812178345,40.0309423476456));
#43753=CARTESIAN_POINT('Ctrl Pts',(19.9166987983089,11.3157884901401,40.0273533783619));
#43754=CARTESIAN_POINT('Ctrl Pts',(19.9073498451879,11.3151628194661,40.0269265924695));
#43755=CARTESIAN_POINT('Ctrl Pts',(19.8934667745314,11.3142387489903,40.0261915465926));
#43756=CARTESIAN_POINT('Ctrl Pts',(19.8889302145428,11.3139375916165,40.0259352808703));
#43757=CARTESIAN_POINT('Ctrl Pts',(19.8808405792688,11.3134020431568,40.0254496268523));
#43758=CARTESIAN_POINT('Ctrl Pts',(19.8772872023722,11.313167314922,40.0252264290502));
#43759=CARTESIAN_POINT('Ctrl Pts',(19.8696076763202,11.3126611363241,40.0247227077444));
#43760=CARTESIAN_POINT('Ctrl Pts',(19.865481814334,11.3123898785727,40.0244387541049));
#43761=CARTESIAN_POINT('Ctrl Pts',(19.8539788540989,11.3116354507978,40.023609913492));
#43762=CARTESIAN_POINT('Ctrl Pts',(19.8466038318823,11.3111538703452,40.0230358536065));
#43763=CARTESIAN_POINT('Ctrl Pts',(19.8038869549981,11.3083758187503,40.0194635318891));
#43764=CARTESIAN_POINT('Ctrl Pts',(19.7686272527186,11.3061276080525,40.0155332454391));
#43765=CARTESIAN_POINT('Ctrl Pts',(19.653571628061,11.2988802897344,39.9994845890002));
#43766=CARTESIAN_POINT('Ctrl Pts',(19.5744211197147,11.2940332963429,39.983331918372));
#43767=CARTESIAN_POINT('Ctrl Pts',(19.3479530451862,11.2800051697463,39.9221030454742));
#43768=CARTESIAN_POINT('Ctrl Pts',(19.2047549580786,11.2708845864594,39.8643139753325));
#43769=CARTESIAN_POINT('Ctrl Pts',(19.0509629410205,11.259760336108,39.7796847292297));
#43770=CARTESIAN_POINT('Ctrl Pts',(19.0321559719663,11.2583765918905,39.768918813538));
#43771=CARTESIAN_POINT('Ctrl Pts',(19.0057022560993,11.2563947990807,39.7531780382109));
#43772=CARTESIAN_POINT('Ctrl Pts',(18.9979028270842,11.2558060482059,39.7484619743615));
#43773=CARTESIAN_POINT('Ctrl Pts',(18.984659954302,11.2547986241385,39.740325721691));
#43774=CARTESIAN_POINT('Ctrl Pts',(18.9791996004789,11.254380963533,39.7369332375866));
#43775=CARTESIAN_POINT('Ctrl Pts',(18.9682747956089,11.2535406955188,39.7300698041833));
#43776=CARTESIAN_POINT('Ctrl Pts',(18.9628106577409,11.2531180794708,39.7265985154545));
#43777=CARTESIAN_POINT('Ctrl Pts',(18.9518390687641,11.2522647029719,39.7195506605933));
#43778=CARTESIAN_POINT('Ctrl Pts',(18.9463322036395,11.2518339187012,39.7159733454214));
#43779=CARTESIAN_POINT('Ctrl Pts',(18.9262605435618,11.2502546803487,39.7027883754893));
#43780=CARTESIAN_POINT('Ctrl Pts',(18.9118083780358,11.2490999526442,39.6930115997608));
#43781=CARTESIAN_POINT('Ctrl Pts',(18.8787194124754,11.2464142797585,39.6699667833101));
#43782=CARTESIAN_POINT('Ctrl Pts',(18.8601823536816,11.2448782670727,39.6565607969657));
#43783=CARTESIAN_POINT('Ctrl Pts',(18.7970673038197,11.239537298614,39.6091840232765));
#43784=CARTESIAN_POINT('Ctrl Pts',(18.7537372053046,11.2356736062469,39.5736049495915));
#43785=CARTESIAN_POINT('Ctrl Pts',(18.6489189000324,11.2258275129363,39.4796037696543));
#43786=CARTESIAN_POINT('Ctrl Pts',(18.5896192353827,11.2197814417717,39.4189204315053));
#43787=CARTESIAN_POINT('Ctrl Pts',(18.4628524749788,11.205873370371,39.2708373986103));
#43788=CARTESIAN_POINT('Ctrl Pts',(18.3984930156784,11.1980319791849,39.1811401381752));
#43789=CARTESIAN_POINT('Ctrl Pts',(18.3374625237523,11.1900129232928,39.0785680120811));
#43790=CARTESIAN_POINT('Ctrl Pts',(18.3328414929143,11.1894015883336,39.07067437102));
#43791=CARTESIAN_POINT('Ctrl Pts',(18.3260300727759,11.1884945362618,39.0588469662555));
#43792=CARTESIAN_POINT('Ctrl Pts',(18.3237971101384,11.1881962044461,39.0549380581947));
#43793=CARTESIAN_POINT('Ctrl Pts',(18.3198242493175,11.1876637064792,39.0479265038123));
#43794=CARTESIAN_POINT('Ctrl Pts',(18.3180792372086,11.1874292188806,39.04482684032));
#43795=CARTESIAN_POINT('Ctrl Pts',(18.3143090469007,11.1869212992067,39.0380863093922));
#43796=CARTESIAN_POINT('Ctrl Pts',(18.3122870907346,11.1866480718237,39.0344437114882));
#43797=CARTESIAN_POINT('Ctrl Pts',(18.3066401411706,11.1858825719376,39.0241924901261));
#43798=CARTESIAN_POINT('Ctrl Pts',(18.3030420068112,11.1853919655264,39.0175690405687));
#43799=CARTESIAN_POINT('Ctrl Pts',(18.2815949770577,11.1824492952118,38.977531646426));
#43800=CARTESIAN_POINT('Ctrl Pts',(18.2646932560577,11.1800524252294,38.94361637071));
#43801=CARTESIAN_POINT('Ctrl Pts',(18.1784772327418,11.1672607197251,38.7570404151906));
#43802=CARTESIAN_POINT('Ctrl Pts',(18.1282856364326,11.1575868259096,38.5963302243795));
#43803=CARTESIAN_POINT('Ctrl Pts',(18.0915188350189,11.1445451990656,38.3853170457206));
#43804=CARTESIAN_POINT('Ctrl Pts',(18.0851948544881,11.1416810364982,38.3392216197336));
#43805=CARTESIAN_POINT('Ctrl Pts',(18.0785841656132,11.1375438959706,38.2734570878014));
#43806=CARTESIAN_POINT('Ctrl Pts',(18.0769221894167,11.1363099360548,38.2539411024129));
#43807=CARTESIAN_POINT('Ctrl Pts',(18.0741336388994,11.1337702160291,38.2140135981025));
#43808=CARTESIAN_POINT('Ctrl Pts',(18.0730337813545,11.132463837611,38.1936027932038));
#43809=CARTESIAN_POINT('Ctrl Pts',(18.0719215865466,11.1305754392644,38.1643044276047));
#43810=CARTESIAN_POINT('Ctrl Pts',(18.0716459911718,11.1300015740114,38.1554277922072));
#43811=CARTESIAN_POINT('Ctrl Pts',(18.0712768607941,11.1290097742771,38.1401346046638));
#43812=CARTESIAN_POINT('Ctrl Pts',(18.0711540311399,11.1285927547571,38.1337188516865));
#43813=CARTESIAN_POINT('Ctrl Pts',(18.0709862947616,11.1278206857492,38.1218682568075));
#43814=CARTESIAN_POINT('Ctrl Pts',(18.0709323413288,11.1274659214192,38.1164335908947));
#43815=CARTESIAN_POINT('Ctrl Pts',(18.0708799375339,11.1268647404811,38.1072424114113));
#43816=CARTESIAN_POINT('Ctrl Pts',(18.0708694923661,11.1266186994183,38.1034859791869));
#43817=CARTESIAN_POINT('Ctrl Pts',(18.0708700189552,11.126372316702,38.0997295667639));
#43818=CARTESIAN_POINT('Ctrl Pts',(18.0708700189004,11.126372342366,38.099729958043));
#43819=CARTESIAN_POINT('Ctrl Pts',(18.0708709872349,11.1259186174904,38.0928123546099));
#43820=CARTESIAN_POINT('Ctrl Pts',(18.0709091639535,11.1254637368608,38.0858948654552));
#43821=CARTESIAN_POINT('Ctrl Pts',(18.0711428693587,11.1240498725853,38.0644498650811));
#43822=CARTESIAN_POINT('Ctrl Pts',(18.0714653045813,11.1230869765028,38.0499245414285));
#43823=CARTESIAN_POINT('Ctrl Pts',(18.0746986210286,11.1166533098097,37.9534163132403));
#43824=CARTESIAN_POINT('Ctrl Pts',(18.0826718787771,11.1110271372982,37.8716979530662));
#43825=CARTESIAN_POINT('Ctrl Pts',(18.1164219929695,11.0962795412273,37.6638884925326));
#43826=CARTESIAN_POINT('Ctrl Pts',(18.1496497491305,11.0870037676159,37.5394111811541));
#43827=CARTESIAN_POINT('Ctrl Pts',(18.2155494381882,11.0738309847884,37.3646981679544));
#43828=CARTESIAN_POINT('Ctrl Pts',(18.238555699285,11.0697780377839,37.3111730665822));
#43829=CARTESIAN_POINT('Ctrl Pts',(18.2693069981766,11.0650156706717,37.2477117991244));
#43830=CARTESIAN_POINT('Ctrl Pts',(18.2747691295907,11.0641916014966,37.2367086778925));
#43831=CARTESIAN_POINT('Ctrl Pts',(18.2826356033553,11.0630358269944,37.2212350531694));
#43832=CARTESIAN_POINT('Ctrl Pts',(18.2849529157069,11.062699034814,37.2167209938264));
#43833=CARTESIAN_POINT('Ctrl Pts',(18.2889605280384,11.0621229081025,37.2089895117613));
#43834=CARTESIAN_POINT('Ctrl Pts',(18.2906421501433,11.0618830393679,37.2057676438564));
#43835=CARTESIAN_POINT('Ctrl Pts',(18.2939124520734,11.0614201964878,37.1995449127445));
#43836=CARTESIAN_POINT('Ctrl Pts',(18.2954999519789,11.0611971482145,37.1965434863292));
#43837=CARTESIAN_POINT('Ctrl Pts',(18.2997957715752,11.060597895667,37.1884731673233));
#43838=CARTESIAN_POINT('Ctrl Pts',(18.3025188583325,11.0602226101327,37.1834121096186));
#43839=CARTESIAN_POINT('Ctrl Pts',(18.312674706629,11.0588394723014,37.1647372082706));
#43840=CARTESIAN_POINT('Ctrl Pts',(18.3202491977173,11.0578401215727,37.151200540538));
#43841=CARTESIAN_POINT('Ctrl Pts',(18.3999604669722,11.0476327056034,37.0126926868956));
#43842=CARTESIAN_POINT('Ctrl Pts',(18.4857501115488,11.0391669846012,36.896079869725));
#43843=CARTESIAN_POINT('Ctrl Pts',(18.65994591166,11.023811867071,36.7077399526684));
#43844=CARTESIAN_POINT('Ctrl Pts',(18.7431664487442,11.0170228411159,36.6321792125026));
#43845=CARTESIAN_POINT('Ctrl Pts',(18.8507850777767,11.0084631781482,36.5503624077049));
#43846=CARTESIAN_POINT('Ctrl Pts',(18.8693422943006,11.0069950429047,36.5367710706089));
#43847=CARTESIAN_POINT('Ctrl Pts',(18.8955221226699,11.0049323855551,36.5183069721611));
#43848=CARTESIAN_POINT('Ctrl Pts',(18.9029431750116,11.0043486335185,36.5131507525847));
#43849=CARTESIAN_POINT('Ctrl Pts',(18.915739945366,11.0033434817161,36.5043921024277));
#43850=CARTESIAN_POINT('Ctrl Pts',(18.9210981130249,11.0029230473476,36.5007641995449));
#43851=CARTESIAN_POINT('Ctrl Pts',(18.9318453578966,11.0020805670416,36.493566059421));
#43852=CARTESIAN_POINT('Ctrl Pts',(18.9372343295317,11.0016585285829,36.489995815887));
#43853=CARTESIAN_POINT('Ctrl Pts',(18.9502646693496,11.0006389694786,36.4814570228568));
#43854=CARTESIAN_POINT('Ctrl Pts',(18.9579234461513,11.0000404600824,36.476515449909));
#43855=CARTESIAN_POINT('Ctrl Pts',(18.9839090849794,10.9980120932452,36.4600087095519));
#43856=CARTESIAN_POINT('Ctrl Pts',(19.0023951585604,10.9965729802426,36.4486984842456));
#43857=CARTESIAN_POINT('Ctrl Pts',(19.139116232397,10.985953347471,36.3681829708129));
#43858=CARTESIAN_POINT('Ctrl Pts',(19.2641741872061,10.976326845162,36.3114720486756));
#43859=CARTESIAN_POINT('Ctrl Pts',(19.394104009089,10.9665681892825,36.2684889830804));
#43860=CARTESIAN_POINT('Ctrl Pts',(19.3941039816494,10.7965035432258,36.2684889921579));
#43861=CARTESIAN_POINT('Ctrl Pts',(19.3599116928284,10.7990471336171,36.2798004020081));
#43862=CARTESIAN_POINT('Ctrl Pts',(19.3260352778518,10.8015715106911,36.2920696020883));
#43863=CARTESIAN_POINT('Ctrl Pts',(19.2620765811673,10.8063228479862,36.3172823953138));
#43864=CARTESIAN_POINT('Ctrl Pts',(19.2319460337816,10.8085547174039,36.3300546763576));
#43865=CARTESIAN_POINT('Ctrl Pts',(19.1955772863557,10.8112284913409,36.3465751184865));
#43866=CARTESIAN_POINT('Ctrl Pts',(19.1890183817105,10.8117098744599,36.3495990355919));
#43867=CARTESIAN_POINT('Ctrl Pts',(19.1787653143114,10.8124609259612,36.3543961114865));
#43868=CARTESIAN_POINT('Ctrl Pts',(19.1750596392986,10.8127320711585,36.3561442873237));
#43869=CARTESIAN_POINT('Ctrl Pts',(19.1681396046576,10.8132378100208,36.3594358520478));
#43870=CARTESIAN_POINT('Ctrl Pts',(19.1649239886415,10.813472569004,36.3609763296577));
#43871=CARTESIAN_POINT('Ctrl Pts',(19.1575692678434,10.8140089580062,36.364524796596));
#43872=CARTESIAN_POINT('Ctrl Pts',(19.1534330664639,10.8143102209137,36.3665386799133));
#43873=CARTESIAN_POINT('Ctrl Pts',(19.1426065060084,10.8150978447772,36.3718580385094));
#43874=CARTESIAN_POINT('Ctrl Pts',(19.1359279745571,10.8155827622142,36.3751876096739));
#43875=CARTESIAN_POINT('Ctrl Pts',(19.0903420554511,10.8188873733811,36.3982456237854));
#43876=CARTESIAN_POINT('Ctrl Pts',(19.0520908374519,10.8216337703324,36.4192518243906));
#43877=CARTESIAN_POINT('Ctrl Pts',(18.8972017639679,10.8327800232323,36.5112832481035));
#43878=CARTESIAN_POINT('Ctrl Pts',(18.7875498857725,10.840756397621,36.5932964814711));
#43879=CARTESIAN_POINT('Ctrl Pts',(18.6211573705008,10.8544391580279,36.7477710458493));
#43880=CARTESIAN_POINT('Ctrl Pts',(18.5592650701366,10.8599805149514,36.8139167925076));
#43881=CARTESIAN_POINT('Ctrl Pts',(18.489261821023,10.8670301788138,36.9001511868764));
#43882=CARTESIAN_POINT('Ctrl Pts',(18.4765344795101,10.8683473724555,36.9163531879437));
#43883=CARTESIAN_POINT('Ctrl Pts',(18.4587116599003,10.870245297248,36.9398055252864));
#43884=CARTESIAN_POINT('Ctrl Pts',(18.4534025584471,10.8708176949897,36.9468923224708));
#43885=CARTESIAN_POINT('Ctrl Pts',(18.444288890421,10.8718127181908,36.9592337737255));
#43886=CARTESIAN_POINT('Ctrl Pts',(18.4404616605289,10.8722344610605,36.9644715743379));
#43887=CARTESIAN_POINT('Ctrl Pts',(18.4331558029089,10.8730471098984,36.9745766974896));
#43888=CARTESIAN_POINT('Ctrl Pts',(18.4296732504468,10.8734378590631,36.9794411010226));
#43889=CARTESIAN_POINT('Ctrl Pts',(18.4215135114813,10.8743614556455,36.9909513063783));
#43890=CARTESIAN_POINT('Ctrl Pts',(18.416855610414,10.8748950274869,36.9976105780742));
#43891=CARTESIAN_POINT('Ctrl Pts',(18.4007260589849,10.8767652214336,37.0209836121035));
#43892=CARTESIAN_POINT('Ctrl Pts',(18.389476227185,10.8781101097891,37.0378481144686));
#43893=CARTESIAN_POINT('Ctrl Pts',(18.2864409875565,10.8908208539611,37.1977084127085));
#43894=CARTESIAN_POINT('Ctrl Pts',(18.213677883871,10.9029127476218,37.3520403874864));
#43895=CARTESIAN_POINT('Ctrl Pts',(18.1408071899472,10.9200085100449,37.5805359071926));
#43896=CARTESIAN_POINT('Ctrl Pts',(18.123185067349,10.9249735967894,37.6483276302469));
#43897=CARTESIAN_POINT('Ctrl Pts',(18.1028112370222,10.9320638973313,37.7488868729032));
#43898=CARTESIAN_POINT('Ctrl Pts',(18.0971475691218,10.9342878673296,37.7810038130815));
#43899=CARTESIAN_POINT('Ctrl Pts',(18.0912280363286,10.9369535071018,37.820385625047));
#43900=CARTESIAN_POINT('Ctrl Pts',(18.090195650858,10.9374343794746,37.8275262213884));
#43901=CARTESIAN_POINT('Ctrl Pts',(18.0886400295997,10.9381848122368,37.8387292697301));
#43902=CARTESIAN_POINT('Ctrl Pts',(18.0880896435333,10.9384558455259,37.8427877908128));
#43903=CARTESIAN_POINT('Ctrl Pts',(18.0870842461246,10.9389614886362,37.8503831117824));
#43904=CARTESIAN_POINT('Ctrl Pts',(18.0866261206356,10.9391962630999,37.8539193824085));
#43905=CARTESIAN_POINT('Ctrl Pts',(18.0855990819622,10.9397328343895,37.8620233860938));
#43906=CARTESIAN_POINT('Ctrl Pts',(18.0850367102923,10.9400342631664,37.8665918940887));
#43907=CARTESIAN_POINT('Ctrl Pts',(18.0836044799661,10.9408226066535,37.8785805309168));
#43908=CARTESIAN_POINT('Ctrl Pts',(18.0827613532863,10.9413080735657,37.8860038635187));
#43909=CARTESIAN_POINT('Ctrl Pts',(18.0772713260349,10.9446246177656,37.9369802348705));
#43910=CARTESIAN_POINT('Ctrl Pts',(18.0740653448849,10.9473817967564,37.9806794801089));
#43911=CARTESIAN_POINT('Ctrl Pts',(18.0713816451734,10.9516208186538,38.0491571450946));
#43912=CARTESIAN_POINT('Ctrl Pts',(18.0708884270925,10.9531345312603,38.0738777395733));
#43913=CARTESIAN_POINT('Ctrl Pts',(18.0708086691379,10.9598246133687,38.1839165646558));
#43914=CARTESIAN_POINT('Ctrl Pts',(18.0764063827742,10.9648818282327,38.2691444193352));
#43915=CARTESIAN_POINT('Ctrl Pts',(18.0919149180857,10.9719379610865,38.3860354226241));
#43916=CARTESIAN_POINT('Ctrl Pts',(18.0970199238408,10.9738937876136,38.4182321512069));
#43917=CARTESIAN_POINT('Ctrl Pts',(18.1197604123069,10.981459504979,38.5413898537029));
#43918=CARTESIAN_POINT('Ctrl Pts',(18.1431215745388,10.9871594415207,38.6311544189538));
#43919=CARTESIAN_POINT('Ctrl Pts',(18.1771769418904,10.9939387332478,38.7316974012605));
#43920=CARTESIAN_POINT('Ctrl Pts',(18.1816507373773,10.9948067610656,38.7444621417286));
#43921=CARTESIAN_POINT('Ctrl Pts',(18.1890575470281,10.996209189312,38.7649041357443));
#43922=CARTESIAN_POINT('Ctrl Pts',(18.1919060863509,10.9967408087142,38.7726116812072));
#43923=CARTESIAN_POINT('Ctrl Pts',(18.1970635808618,10.9976899284244,38.7862972320725));
#43924=CARTESIAN_POINT('Ctrl Pts',(18.1993532590413,10.9981067843807,38.7922824097363));
#43925=CARTESIAN_POINT('Ctrl Pts',(18.2042001618036,10.9989799627064,38.8047653923189));
#43926=CARTESIAN_POINT('Ctrl Pts',(18.2067629266385,10.9994364648422,38.8112609321807));
#43927=CARTESIAN_POINT('Ctrl Pts',(18.2135453386114,11.0006313360473,38.8281818402969));
#43928=CARTESIAN_POINT('Ctrl Pts',(18.2178209416765,11.0013715693115,38.8385843518228));
#43929=CARTESIAN_POINT('Ctrl Pts',(18.2372307904447,11.0046758581754,38.8846583725112));
#43930=CARTESIAN_POINT('Ctrl Pts',(18.2533458893538,11.0072727381979,38.9199043233803));
#43931=CARTESIAN_POINT('Ctrl Pts',(18.299904155933,11.0144101218393,39.0141219156325));
#43932=CARTESIAN_POINT('Ctrl Pts',(18.3323441975341,11.0190139728566,39.072042860555));
#43933=CARTESIAN_POINT('Ctrl Pts',(18.4302313154363,11.0319456277407,39.2274458135195));
#43934=CARTESIAN_POINT('Ctrl Pts',(18.5016846873692,11.0404031915967,39.3208019009502));
#43935=CARTESIAN_POINT('Ctrl Pts',(18.5910050510469,11.0496996635165,39.4177580707008));
#43936=CARTESIAN_POINT('Ctrl Pts',(18.6009566592841,11.0507195119575,39.4283188042161));
#43937=CARTESIAN_POINT('Ctrl Pts',(18.6447201610558,11.0551327647021,39.4737235406742));
#43938=CARTESIAN_POINT('Ctrl Pts',(18.6797247387762,11.0584806333226,39.5073997129096));
#43939=CARTESIAN_POINT('Ctrl Pts',(18.7217047583309,11.0622556370353,39.5448401158269));
#43940=CARTESIAN_POINT('Ctrl Pts',(18.7274741424071,11.0627694157682,39.549924008961));
#43941=CARTESIAN_POINT('Ctrl Pts',(18.7367570844875,11.0635878667725,39.5580059061044));
#43942=CARTESIAN_POINT('Ctrl Pts',(18.7402512052919,11.063894091051,39.5610259618359));
#43943=CARTESIAN_POINT('Ctrl Pts',(18.7464702786413,11.0644358179942,39.5663623646954));
#43944=CARTESIAN_POINT('Ctrl Pts',(18.7491908657074,11.0646716833239,39.5686837158875));
#43945=CARTESIAN_POINT('Ctrl Pts',(18.7549974618703,11.0651727058998,39.573610378352));
#43946=CARTESIAN_POINT('Ctrl Pts',(18.7580851967673,11.0654377101211,39.5762135649659));
#43947=CARTESIAN_POINT('Ctrl Pts',(18.7665134006095,11.0661572723944,39.5832739978637));
#43948=CARTESIAN_POINT('Ctrl Pts',(18.7718699030438,11.0666104712647,39.5877121402246));
#43949=CARTESIAN_POINT('Ctrl Pts',(18.7996774226552,11.0689427160613,39.6104995863804));
#43950=CARTESIAN_POINT('Ctrl Pts',(18.8225174276069,11.0707898234213,39.6283711268983));
#43951=CARTESIAN_POINT('Ctrl Pts',(18.9736937418759,11.0826415838328,39.7412599776763));
#43952=CARTESIAN_POINT('Ctrl Pts',(19.1130142084943,11.0918940290622,39.8205543686528));
#43953=CARTESIAN_POINT('Ctrl Pts',(19.3463140040522,11.1071517443397,39.9173782876406));
#43954=CARTESIAN_POINT('Ctrl Pts',(19.4345474521585,11.1128653962314,39.9467347430041));
#43955=CARTESIAN_POINT('Ctrl Pts',(19.5376584830146,11.1196599018256,39.9729564816677));
#43956=CARTESIAN_POINT('Ctrl Pts',(19.5508070994759,11.1205282867505,39.9761533476015));
#43957=CARTESIAN_POINT('Ctrl Pts',(19.5719940909266,11.1219311810019,39.9810691233432));
#43958=CARTESIAN_POINT('Ctrl Pts',(19.5800118711664,11.1224629062973,39.9828754800037));
#43959=CARTESIAN_POINT('Ctrl Pts',(19.5943014841957,11.1234121471048,39.9859990295698));
#43960=CARTESIAN_POINT('Ctrl Pts',(19.6005688362644,11.1238290176804,39.9873363158301));
#43961=CARTESIAN_POINT('Ctrl Pts',(19.6136781788222,11.1247021571285,39.9900652783141));
#43962=CARTESIAN_POINT('Ctrl Pts',(19.6205212827763,11.125158605422,39.9914510849688));
#43963=CARTESIAN_POINT('Ctrl Pts',(19.638403194324,11.1263531809751,39.9949714292462));
#43964=CARTESIAN_POINT('Ctrl Pts',(19.6494532769682,11.1270931707262,39.9970466397704));
#43965=CARTESIAN_POINT('Ctrl Pts',(19.6986293492169,11.1303948033599,40.0058376030066));
#43966=CARTESIAN_POINT('Ctrl Pts',(19.736931932925,11.1329892056909,40.0115009979894));
#43967=CARTESIAN_POINT('Ctrl Pts',(19.841184505067,11.140117768177,40.0237230516145));
#43968=CARTESIAN_POINT('Ctrl Pts',(19.907339601263,11.1447150814766,40.0280418147694));
#43969=CARTESIAN_POINT('Ctrl Pts',(20.0598071285967,11.1554507258419,40.0301300869685));
#43970=CARTESIAN_POINT('Ctrl Pts',(20.146013525069,11.1616261459808,40.025527963186));
#43971=CARTESIAN_POINT('Ctrl Pts',(20.3238671928586,11.1743842365249,40.0040186331108));
#43972=CARTESIAN_POINT('Ctrl Pts',(20.4152018114396,11.1809448982904,39.9862101381461));
#43973=CARTESIAN_POINT('Ctrl Pts',(20.5139520413686,11.1878219477999,39.9594310143172));
#43974=CARTESIAN_POINT('Ctrl Pts',(20.5229799169806,11.1884485669499,39.9569120638768));
#43975=CARTESIAN_POINT('Ctrl Pts',(20.5363594818685,11.1893737615224,39.9530735909714));
#43976=CARTESIAN_POINT('Ctrl Pts',(20.5407252768277,11.189675104094,39.9518043642341));
#43977=CARTESIAN_POINT('Ctrl Pts',(20.5485020966611,11.190210853103,39.9495136346206));
#43978=CARTESIAN_POINT('Ctrl Pts',(20.5519148110153,11.1904455977197,39.9484981138193));
#43979=CARTESIAN_POINT('Ctrl Pts',(20.5592834200984,11.1909516656761,39.9462832121868));
#43980=CARTESIAN_POINT('Ctrl Pts',(20.5632382687285,11.1912227971804,39.9450805665424));
#43981=CARTESIAN_POINT('Ctrl Pts',(20.5742509064289,11.1919765190596,39.9416929816526));
#43982=CARTESIAN_POINT('Ctrl Pts',(20.5813001478432,11.192457524681,39.9394801669547));
#43983=CARTESIAN_POINT('Ctrl Pts',(20.6219755840167,11.1952255295468,39.9264546392231));
#43984=CARTESIAN_POINT('Ctrl Pts',(20.6553149360056,11.1974646755207,39.9147597340614));
#43985=CARTESIAN_POINT('Ctrl Pts',(20.7631601280733,11.2046677806116,39.8735692398989));
#43986=CARTESIAN_POINT('Ctrl Pts',(20.8361565848331,11.2094817392772,39.8403463852523));
#43987=CARTESIAN_POINT('Ctrl Pts',(21.0434242734331,11.223525467744,39.7299514181623));
#43988=CARTESIAN_POINT('Ctrl Pts',(21.1707074125025,11.232690505048,39.6410755166232));
#43989=CARTESIAN_POINT('Ctrl Pts',(21.3021225149627,11.2438637108733,39.5235473003117));
#43990=CARTESIAN_POINT('Ctrl Pts',(21.3179935892802,11.245244302311,39.508865784622));
#43991=CARTESIAN_POINT('Ctrl Pts',(21.3396568095881,11.2471745140905,39.4881398082503));
#43992=CARTESIAN_POINT('Ctrl Pts',(21.3456617970365,11.2477145788709,39.482319362202));
#43993=CARTESIAN_POINT('Ctrl Pts',(21.3559406019377,11.2486478180218,39.4722259878023));
#43994=CARTESIAN_POINT('Ctrl Pts',(21.3602325698061,11.2490401826862,39.4679716489181));
#43995=CARTESIAN_POINT('Ctrl Pts',(21.3690617264055,11.2498529518913,39.4591372662695));
#43996=CARTESIAN_POINT('Ctrl Pts',(21.3735960821235,11.2502734730759,39.4545545100724));
#43997=CARTESIAN_POINT('Ctrl Pts',(21.3841357955715,11.2512582978363,39.4437949519513));
#43998=CARTESIAN_POINT('Ctrl Pts',(21.3901228794296,11.2518233821822,39.4376005194008));
#43999=CARTESIAN_POINT('Ctrl Pts',(21.4093467604036,11.2536563803627,39.4174423937141));
#44000=CARTESIAN_POINT('Ctrl Pts',(21.4224158544404,11.2549313874469,39.403321082275));
#44001=CARTESIAN_POINT('Ctrl Pts',(21.4883425497027,11.2615156652357,39.329913662011));
#44002=CARTESIAN_POINT('Ctrl Pts',(21.5377068651489,11.2669658296068,39.2676068853146));
#44003=CARTESIAN_POINT('Ctrl Pts',(21.6449092802338,11.2801040036711,39.1136662776948));
#44004=CARTESIAN_POINT('Ctrl Pts',(21.6991523084523,11.2878713152156,39.0198503426908));
#44005=CARTESIAN_POINT('Ctrl Pts',(21.7807163039062,11.3014743742508,38.8466746403488));
#44006=CARTESIAN_POINT('Ctrl Pts',(21.8112817039661,11.3073246293017,38.7691304706126));
#44007=CARTESIAN_POINT('Ctrl Pts',(21.8396022811142,11.3135499887683,38.6809418629148));
#44008=CARTESIAN_POINT('Ctrl Pts',(21.8423967566412,11.3141751729334,38.6720176575357));
#44009=CARTESIAN_POINT('Ctrl Pts',(21.8464520993388,11.3150986659946,38.6587287662054));
#44010=CARTESIAN_POINT('Ctrl Pts',(21.8477625699267,11.315399727561,38.6543795410763));
#44011=CARTESIAN_POINT('Ctrl Pts',(21.8500727631516,11.3159351714369,38.646613211717));
#44012=CARTESIAN_POINT('Ctrl Pts',(21.8510783970509,11.3161698903665,38.6431979389408));
#44013=CARTESIAN_POINT('Ctrl Pts',(21.8532320217961,11.3166761234742,38.6358084931247));
#44014=CARTESIAN_POINT('Ctrl Pts',(21.8543766844103,11.3169474446457,38.6318334147317));
#44015=CARTESIAN_POINT('Ctrl Pts',(21.8575338320387,11.3177022303112,38.6207354456465));
#44016=CARTESIAN_POINT('Ctrl Pts',(21.8595181494617,11.3181841027809,38.6136045148415));
#44017=CARTESIAN_POINT('Ctrl Pts',(21.8707928830716,11.3209672994778,38.5721651308519));
#44018=CARTESIAN_POINT('Ctrl Pts',(21.8791754197273,11.3232201539496,38.5376140448056));
#44019=CARTESIAN_POINT('Ctrl Pts',(21.9035123567488,11.3304902122526,38.4236405726242));
#44020=CARTESIAN_POINT('Ctrl Pts',(21.9154221619336,11.3353542084999,38.3434392082175));
#44021=CARTESIAN_POINT('Ctrl Pts',(21.9351995619217,11.3493738448671,38.1098046220398));
#44022=CARTESIAN_POINT('Ctrl Pts',(21.9298511034609,11.3584710349114,37.9559099938192));
#44023=CARTESIAN_POINT('Ctrl Pts',(21.903003268927,11.3695697724975,37.7828375909111));
#44024=CARTESIAN_POINT('Ctrl Pts',(21.8993154298238,11.3709554096055,37.7614527020763));
#44025=CARTESIAN_POINT('Ctrl Pts',(21.8937053396126,11.3728915629396,37.7319065387209));
#44026=CARTESIAN_POINT('Ctrl Pts',(21.8920893597929,11.3734324452901,37.723688213774));
#44027=CARTESIAN_POINT('Ctrl Pts',(21.8892147116964,11.3743667182407,37.7095555209315));
#44028=CARTESIAN_POINT('Ctrl Pts',(21.8879816504018,11.3747592949414,37.7036360201898));
#44029=CARTESIAN_POINT('Ctrl Pts',(21.8853768347011,11.3755721469248,37.6914191808932));
#44030=CARTESIAN_POINT('Ctrl Pts',(21.8840013123848,11.3759925372756,37.6851227316235));
#44031=CARTESIAN_POINT('Ctrl Pts',(21.8807161018317,11.3769764361389,37.6704380012747));
#44032=CARTESIAN_POINT('Ctrl Pts',(21.8787818147337,11.377540721035,37.6620554201458));
#44033=CARTESIAN_POINT('Ctrl Pts',(21.8723555920662,11.3793685004335,37.6350325505946));
#44034=CARTESIAN_POINT('Ctrl Pts',(21.8676419222311,11.3806390319143,37.6164466962242));
#44035=CARTESIAN_POINT('Ctrl Pts',(21.8421163091833,11.3871836995057,37.5217471785182));
#44036=CARTESIAN_POINT('Ctrl Pts',(21.8169281826751,11.3925968262206,37.4469012821207));
#44037=CARTESIAN_POINT('Ctrl Pts',(21.7471137408864,11.4055823897504,37.2750791087723));
#44038=CARTESIAN_POINT('Ctrl Pts',(21.6988838838886,11.4132303232867,37.1798414076816));
#44039=CARTESIAN_POINT('Ctrl Pts',(21.5982618390742,11.4268832344703,37.0163008268001));
#44040=CARTESIAN_POINT('Ctrl Pts',(21.5486896573047,11.4328947132075,36.9465665284007));
#44041=CARTESIAN_POINT('Ctrl Pts',(21.4887286844768,11.4392691597864,36.8730863196949));
#44042=CARTESIAN_POINT('Ctrl Pts',(21.4827544218702,11.4398953350182,36.8658729368436));
#44043=CARTESIAN_POINT('Ctrl Pts',(21.4738031219805,11.440820003263,36.8552238863034));
#44044=CARTESIAN_POINT('Ctrl Pts',(21.4708662039674,11.4411212589423,36.851754901205));
#44045=CARTESIAN_POINT('Ctrl Pts',(21.4656068219443,11.441656913563,36.8455870387391));
#44046=CARTESIAN_POINT('Ctrl Pts',(21.4632891263502,11.4418916502018,36.8428841869837));
#44047=CARTESIAN_POINT('Ctrl Pts',(21.4582638696937,11.4423977690667,36.8370565580966));
#44048=CARTESIAN_POINT('Ctrl Pts',(21.45555374836,11.4426689590957,36.833934070623));
#44049=CARTESIAN_POINT('Ctrl Pts',(21.4479701350849,11.4434230091762,36.8252530872529));
#44050=CARTESIAN_POINT('Ctrl Pts',(21.4430746366408,11.4439042822326,36.8197137815917));
#44051=CARTESIAN_POINT('Ctrl Pts',(21.4145592801289,11.4466769622597,36.7878197327932));
#44052=CARTESIAN_POINT('Ctrl Pts',(21.3902478784872,11.4489203266873,36.7620888555165));
#44053=CARTESIAN_POINT('Ctrl Pts',(21.3084467601857,11.4561439833719,36.6801508956201));
#44054=CARTESIAN_POINT('Ctrl Pts',(21.2481478521524,11.4609732944377,36.6268627006417));
#44055=CARTESIAN_POINT('Ctrl Pts',(21.0629033424365,11.4750093570021,36.4827203767234));
#44056=CARTESIAN_POINT('Ctrl Pts',(20.930196871483,11.484153341171,36.4029188517528));
#44057=CARTESIAN_POINT('Ctrl Pts',(20.7696565560982,11.4953035757415,36.3309211628988));
#44058=CARTESIAN_POINT('Ctrl Pts',(20.7497579451865,11.4966858913651,36.3223965262477));
#44059=CARTESIAN_POINT('Ctrl Pts',(20.7219751478198,11.4986181341304,36.311043752855));
#44060=CARTESIAN_POINT('Ctrl Pts',(20.7142091682948,11.4991584789886,36.307929178692));
#44061=CARTESIAN_POINT('Ctrl Pts',(20.7007987249799,11.5000920722507,36.3026518872159));
#44062=CARTESIAN_POINT('Ctrl Pts',(20.6951638609284,11.5004845095124,36.3004649776839));
#44063=CARTESIAN_POINT('Ctrl Pts',(20.6834984613273,11.5012973068433,36.2960005642646));
#44064=CARTESIAN_POINT('Ctrl Pts',(20.6774666089673,11.5017177830159,36.2937267363941));
#44065=CARTESIAN_POINT('Ctrl Pts',(20.6633511235763,11.5027022896786,36.2884862713249));
#44066=CARTESIAN_POINT('Ctrl Pts',(20.6552588505572,11.5032670994319,36.2855434595881));
#44067=CARTESIAN_POINT('Ctrl Pts',(20.6290432859745,11.505098303962,36.2762082313613));
#44068=CARTESIAN_POINT('Ctrl Pts',(20.6108445736694,11.506371772622,36.2700325870075));
#44069=CARTESIAN_POINT('Ctrl Pts',(20.5171405020204,11.5129424204164,36.2397880590791));
#44070=CARTESIAN_POINT('Ctrl Pts',(20.4403054803013,11.5183798367697,36.2201194327732));
#44071=CARTESIAN_POINT('Ctrl Pts',(20.2567175885002,11.531469603815,36.1849973082169));
#44072=CARTESIAN_POINT('Ctrl Pts',(20.1494436223446,11.5392001587137,36.173655483205));
#44073=CARTESIAN_POINT('Ctrl Pts',(19.9578619823083,11.552820216672,36.1695040233845));
#44074=CARTESIAN_POINT('Ctrl Pts',(19.8738904718882,11.5587216026732,36.1731657563484));
#44075=CARTESIAN_POINT('Ctrl Pts',(19.7811148404891,11.5649943093235,36.1833050885303));
#44076=CARTESIAN_POINT('Ctrl Pts',(19.7718212357972,11.5656198405102,36.1843892470191));
#44077=CARTESIAN_POINT('Ctrl Pts',(19.7580269053695,11.5665437450826,36.1861002586328));
#44078=CARTESIAN_POINT('Ctrl Pts',(19.7535200832844,11.5668448746368,36.1866754456614));
#44079=CARTESIAN_POINT('Ctrl Pts',(19.7454852185212,11.5673803923078,36.1877297631371));
#44080=CARTESIAN_POINT('Ctrl Pts',(19.7419564392349,11.5676151174222,36.1882027423781));
#44081=CARTESIAN_POINT('Ctrl Pts',(19.7343312590901,11.5681213104353,36.1892462790511));
#44082=CARTESIAN_POINT('Ctrl Pts',(19.7302353866208,11.5683925856111,36.1898202398257));
#44083=CARTESIAN_POINT('Ctrl Pts',(19.7188178772814,11.5691471132607,36.1914576486214));
#44084=CARTESIAN_POINT('Ctrl Pts',(19.7115003684001,11.569628775475,36.1925500635598));
#44085=CARTESIAN_POINT('Ctrl Pts',(19.6691190976066,11.5724082772486,36.1991265399423));
#44086=CARTESIAN_POINT('Ctrl Pts',(19.6342031353967,11.5746577973772,36.2055356632801));
#44087=CARTESIAN_POINT('Ctrl Pts',(19.5300497104521,11.5813000772639,36.2276412771628));
#44088=CARTESIAN_POINT('Ctrl Pts',(19.4614862629894,11.5855827213597,36.2461977505825));
#44089=CARTESIAN_POINT('Ctrl Pts',(19.3941040036879,11.589834535998,36.2684889848672));
#44090=CARTESIAN_POINT('Origin',(20.,-1.3495818343519,38.1));
#44091=CARTESIAN_POINT('',(19.394104060634,12.5529621656639,36.2684889660284));
#44092=CARTESIAN_POINT('',(19.3941040087481,12.3811612414289,36.2684889831931));
#44093=CARTESIAN_POINT('',(19.3941040087494,-1.3495818343519,36.2684889831927));
#44094=CARTESIAN_POINT('Ctrl Pts',(19.394104060634,12.5529621656639,36.2684889660284));
#44095=CARTESIAN_POINT('Ctrl Pts',(19.424631338161,12.551017496247,36.2583900077636));
#44096=CARTESIAN_POINT('Ctrl Pts',(19.4554190886317,12.5490873835358,36.2490516417566));
#44097=CARTESIAN_POINT('Ctrl Pts',(19.5665534787306,12.5421885724538,36.2183585513128));
#44098=CARTESIAN_POINT('Ctrl Pts',(19.6480132246812,12.5372541669735,36.2014333502371));
#44099=CARTESIAN_POINT('Ctrl Pts',(19.8084588065227,12.5274358374843,36.1787806489044));
#44100=CARTESIAN_POINT('Ctrl Pts',(19.8872045077698,12.5225712982824,36.1725543251561));
#44101=CARTESIAN_POINT('Ctrl Pts',(19.9852778237007,12.5163363490775,36.1708308646105));
#44102=CARTESIAN_POINT('Ctrl Pts',(20.0044547571054,12.515109068506,36.1707798444788));
#44103=CARTESIAN_POINT('Ctrl Pts',(20.0322314693566,12.5133183574325,36.1711200899231));
#44104=CARTESIAN_POINT('Ctrl Pts',(20.0408332899999,12.5127620016514,36.1712830136058));
#44105=CARTESIAN_POINT('Ctrl Pts',(20.0558765706518,12.511785728515,36.1716686216731));
#44106=CARTESIAN_POINT('Ctrl Pts',(20.0623185870952,12.5113666009464,36.1718660607175));
#44107=CARTESIAN_POINT('Ctrl Pts',(20.0748020570529,12.5105523099961,36.1723112883656));
#44108=CARTESIAN_POINT('Ctrl Pts',(20.0808435802147,12.5101572717702,36.1725552067973));
#44109=CARTESIAN_POINT('Ctrl Pts',(20.0952505265848,12.5092129238402,36.1732047232552));
#44110=CARTESIAN_POINT('Ctrl Pts',(20.1036145949129,12.5086628095685,36.1736364015874));
#44111=CARTESIAN_POINT('Ctrl Pts',(20.1336354991816,12.5066814388033,36.175381894291));
#44112=CARTESIAN_POINT('Ctrl Pts',(20.1552719492921,12.5052405855515,36.177006537645));
#44113=CARTESIAN_POINT('Ctrl Pts',(20.3297576347557,12.4935125285578,36.1930722345579));
#44114=CARTESIAN_POINT('Ctrl Pts',(20.4803839460583,12.4826488744393,36.2253462457159));
#44115=CARTESIAN_POINT('Ctrl Pts',(20.702145777582,12.4659208925764,36.3013648582102));
#44116=CARTESIAN_POINT('Ctrl Pts',(20.7770073281302,12.4601495456332,36.3324145462756));
#44117=CARTESIAN_POINT('Ctrl Pts',(20.8816024639393,12.4520781759104,36.3837300966564));
#44118=CARTESIAN_POINT('Ctrl Pts',(20.9130687655454,12.4496495599521,36.4002614586026));
#44119=CARTESIAN_POINT('Ctrl Pts',(20.9505170415081,12.4467741367281,36.421275875092));
#44120=CARTESIAN_POINT('Ctrl Pts',(20.9569506217065,12.4462806879936,36.4249349726863));
#44121=CARTESIAN_POINT('Ctrl Pts',(20.9669468588086,12.445515030065,36.430696720405));
#44122=CARTESIAN_POINT('Ctrl Pts',(20.9705239955341,12.4452412503049,36.4327739079785));
#44123=CARTESIAN_POINT('Ctrl Pts',(20.9771675520344,12.4447332094362,36.4366603450079));
#44124=CARTESIAN_POINT('Ctrl Pts',(20.9802356154347,12.4444987672265,36.4384665603212));
#44125=CARTESIAN_POINT('Ctrl Pts',(20.9872068410248,12.4439664534437,36.442596656203));
#44126=CARTESIAN_POINT('Ctrl Pts',(20.9911068007277,12.443668927838,36.4449258319974));
#44127=CARTESIAN_POINT('Ctrl Pts',(21.0030106518199,12.4427615028905,36.4520923418715));
#44128=CARTESIAN_POINT('Ctrl Pts',(21.0109877718324,12.4421544005366,36.456974208624));
#44129=CARTESIAN_POINT('Ctrl Pts',(21.0877462134587,12.436319082453,36.5047198235209));
#44130=CARTESIAN_POINT('Ctrl Pts',(21.1538068961394,12.4313457027217,36.5518256552691));
#44131=CARTESIAN_POINT('Ctrl Pts',(21.3438935628083,12.416561067179,36.7063174952605));
#44132=CARTESIAN_POINT('Ctrl Pts',(21.4573750412662,12.4070019722847,36.825457705512));
#44133=CARTESIAN_POINT('Ctrl Pts',(21.577691585422,12.394320804484,36.9891560058173));
#44134=CARTESIAN_POINT('Ctrl Pts',(21.5999784543272,12.3918377277858,37.0215039523279));
#44135=CARTESIAN_POINT('Ctrl Pts',(21.6273852690981,12.3885923077777,37.0640041391241));
#44136=CARTESIAN_POINT('Ctrl Pts',(21.6334254258537,12.3878641548137,37.0735538946565));
#44137=CARTESIAN_POINT('Ctrl Pts',(21.6430680354153,12.3866802813498,37.0890999500792));
#44138=CARTESIAN_POINT('Ctrl Pts',(21.6467224401222,12.3862264657556,37.0950638413322));
#44139=CARTESIAN_POINT('Ctrl Pts',(21.6536608945825,12.3853548164983,37.1065266863398));
#44140=CARTESIAN_POINT('Ctrl Pts',(21.6569501559026,12.3849371793809,37.112022389714));
#44141=CARTESIAN_POINT('Ctrl Pts',(21.6643847076799,12.3839830010491,37.1245856089187));
#44142=CARTESIAN_POINT('Ctrl Pts',(21.6685124395976,12.3834458365236,37.1316633204786));
#44143=CARTESIAN_POINT('Ctrl Pts',(21.6792944984959,12.3820228462614,37.1504246584588));
#44144=CARTESIAN_POINT('Ctrl Pts',(21.6858718835424,12.3811342989299,37.1621517613509));
#44145=CARTESIAN_POINT('Ctrl Pts',(21.7352662021658,12.3743007321268,37.2524179093656));
#44146=CARTESIAN_POINT('Ctrl Pts',(21.772690111719,12.3681675404258,37.3337691212933));
#44147=CARTESIAN_POINT('Ctrl Pts',(21.8616425961561,12.3505340907464,37.5689035611052));
#44148=CARTESIAN_POINT('Ctrl Pts',(21.8996427433279,12.3387365851242,37.7269976866177));
#44149=CARTESIAN_POINT('Ctrl Pts',(21.9207579090756,12.3254897360622,37.9179526754323));
#44150=CARTESIAN_POINT('Ctrl Pts',(21.9233694676922,12.3234360176934,37.9480055451786));
#44151=CARTESIAN_POINT('Ctrl Pts',(21.9257203854433,12.3209464510019,37.9851385084746));
#44152=CARTESIAN_POINT('Ctrl Pts',(21.9261269214358,12.3204771289205,37.9921702664075));
#44153=CARTESIAN_POINT('Ctrl Pts',(21.9267069659523,12.3197406974457,38.0032565727329));
#44154=CARTESIAN_POINT('Ctrl Pts',(21.9269062038707,12.3194722025434,38.0073096250532));
#44155=CARTESIAN_POINT('Ctrl Pts',(21.9272567947968,12.3189686828517,38.0149319910307));
#44156=CARTESIAN_POINT('Ctrl Pts',(21.9274110203678,12.3187335088595,38.0185010548979));
#44157=CARTESIAN_POINT('Ctrl Pts',(21.9277406042984,12.3181976723973,38.0266531950203));
#44158=CARTESIAN_POINT('Ctrl Pts',(21.9279095338035,12.3178973692364,38.0312364791351));
#44159=CARTESIAN_POINT('Ctrl Pts',(21.9283143127749,12.3171030412837,38.0433967101393));
#44160=CARTESIAN_POINT('Ctrl Pts',(21.9285218529068,12.3166105385146,38.0509746114753));
#44161=CARTESIAN_POINT('Ctrl Pts',(21.9296729381394,12.3131456484107,38.1045398260795));
#44162=CARTESIAN_POINT('Ctrl Pts',(21.9290162370414,12.3102548198355,38.1505509409755));
#44163=CARTESIAN_POINT('Ctrl Pts',(21.9252342300737,12.3055870741923,38.2260634270872));
#44164=CARTESIAN_POINT('Ctrl Pts',(21.9230731362518,12.3037811699448,38.2555913479382));
#44165=CARTESIAN_POINT('Ctrl Pts',(21.9042523260376,12.2919000832757,38.4508824543671));
#44166=CARTESIAN_POINT('Ctrl Pts',(21.866861624304,12.2822124796613,38.6139298674188));
#44167=CARTESIAN_POINT('Ctrl Pts',(21.7941029216956,12.2691751064047,38.8103334752139));
#44168=CARTESIAN_POINT('Ctrl Pts',(21.7778826180906,12.2664709839502,38.8500079340842));
#44169=CARTESIAN_POINT('Ctrl Pts',(21.7555947259018,12.2629759307675,38.8997281957132));
#44170=CARTESIAN_POINT('Ctrl Pts',(21.7507377820153,12.2622261684407,38.9103056445679));
#44171=CARTESIAN_POINT('Ctrl Pts',(21.7427774143578,12.2610157491995,38.9272360123358));
#44172=CARTESIAN_POINT('Ctrl Pts',(21.7397342130453,12.2605571593158,38.9336170594816));
#44173=CARTESIAN_POINT('Ctrl Pts',(21.7338754899577,12.2596820209802,38.9457299344488));
#44174=CARTESIAN_POINT('Ctrl Pts',(21.7310664413949,12.2592657004296,38.9514648028758));
#44175=CARTESIAN_POINT('Ctrl Pts',(21.7245923831517,12.2583135462291,38.964517583625));
#44176=CARTESIAN_POINT('Ctrl Pts',(21.7209091937215,12.257777087019,38.9718262922799));
#44177=CARTESIAN_POINT('Ctrl Pts',(21.7112011893108,12.2563764488287,38.9907890659834));
#44178=CARTESIAN_POINT('Ctrl Pts',(21.7051038835884,12.2555097527991,39.002405342494));
#44179=CARTESIAN_POINT('Ctrl Pts',(21.6618192074786,12.2494448471855,39.0828639892144));
#44180=CARTESIAN_POINT('Ctrl Pts',(21.6205969476849,12.2441041267393,39.1494414574469));
#44181=CARTESIAN_POINT('Ctrl Pts',(21.4799957146038,12.2271105442328,39.3484043153222));
#44182=CARTESIAN_POINT('Ctrl Pts',(21.367576077139,12.2150640152101,39.4706310059811));
#44183=CARTESIAN_POINT('Ctrl Pts',(21.212104380237,12.200971364667,39.6012545720403));
#44184=CARTESIAN_POINT('Ctrl Pts',(21.1825489529847,12.1983925303452,39.6246444685866));
#44185=CARTESIAN_POINT('Ctrl Pts',(21.1462890874629,12.1953642966231,39.6516509038929));
#44186=CARTESIAN_POINT('Ctrl Pts',(21.140226776087,12.1948624165314,39.6561112117293));
#44187=CARTESIAN_POINT('Ctrl Pts',(21.1307702960272,12.1940865650379,39.6629838228121));
#44188=CARTESIAN_POINT('Ctrl Pts',(21.1273942414321,12.1938109561178,39.6654207478978));
#44189=CARTESIAN_POINT('Ctrl Pts',(21.1211191375286,12.1933012681254,39.6699194537262));
#44190=CARTESIAN_POINT('Ctrl Pts',(21.1182222997528,12.1930669971097,39.6719841285469));
#44191=CARTESIAN_POINT('Ctrl Pts',(21.1116439439237,12.1925372908182,39.6766453607336));
#44192=CARTESIAN_POINT('Ctrl Pts',(21.1079590384875,12.1922421877734,39.6792370378244));
#44193=CARTESIAN_POINT('Ctrl Pts',(21.0967517777663,12.1913494385396,39.6870608224347));
#44194=CARTESIAN_POINT('Ctrl Pts',(21.0892010597726,12.1907544591513,39.6922523592626));
#44195=CARTESIAN_POINT('Ctrl Pts',(20.990916712871,12.1830895996628,39.7588019625556));
#44196=CARTESIAN_POINT('Ctrl Pts',(20.8951394698338,12.1764895350745,39.812388002061));
#44197=CARTESIAN_POINT('Ctrl Pts',(20.7191759435041,12.1649334108905,39.8920137364516));
#44198=CARTESIAN_POINT('Ctrl Pts',(20.6408764782058,12.1599715022992,39.9214840577016));
#44199=CARTESIAN_POINT('Ctrl Pts',(20.4860365610512,12.1501621750001,39.9685383608472));
#44200=CARTESIAN_POINT('Ctrl Pts',(20.4098507259706,12.1453368952395,39.9867133857815));
#44201=CARTESIAN_POINT('Ctrl Pts',(20.3139728939988,12.1391491484393,40.0035041472148));
#44202=CARTESIAN_POINT('Ctrl Pts',(20.2951209627249,12.1379272745513,40.0065179234554));
#44203=CARTESIAN_POINT('Ctrl Pts',(20.2677285412972,12.1361430311735,40.0104810223676));
#44204=CARTESIAN_POINT('Ctrl Pts',(20.2592211495001,12.1355876639642,40.0116539175246));
#44205=CARTESIAN_POINT('Ctrl Pts',(20.244318346252,12.1346125371526,40.0136072245455));
#44206=CARTESIAN_POINT('Ctrl Pts',(20.2379262823542,12.1341935616724,40.0144124807987));
#44207=CARTESIAN_POINT('Ctrl Pts',(20.2255232667001,12.133379132015,40.0159119044806));
#44208=CARTESIAN_POINT('Ctrl Pts',(20.2195128395581,12.1329838009568,40.0166098406884));
#44209=CARTESIAN_POINT('Ctrl Pts',(20.2051589223262,12.1320380549513,40.0182082258476));
#44210=CARTESIAN_POINT('Ctrl Pts',(20.1968127013243,12.1314868299798,40.0190825250524));
#44211=CARTESIAN_POINT('Ctrl Pts',(20.1667635619287,12.1294973588631,40.0220322039629));
#44212=CARTESIAN_POINT('Ctrl Pts',(20.1450322157591,12.1280494132623,40.0237940298105));
#44213=CARTESIAN_POINT('Ctrl Pts',(19.9718174261623,12.1164308465449,40.0348855735713));
#44214=CARTESIAN_POINT('Ctrl Pts',(19.8197714495793,12.1056984985874,40.0266749919094));
#44215=CARTESIAN_POINT('Ctrl Pts',(19.5892858667585,12.0890059960846,39.9866944539443));
#44216=CARTESIAN_POINT('Ctrl Pts',(19.5092553432328,12.083142117305,39.9674778246224));
#44217=CARTESIAN_POINT('Ctrl Pts',(19.3964378589307,12.0749597469714,39.9326321262008));
#44218=CARTESIAN_POINT('Ctrl Pts',(19.3624834579184,12.0725090947382,39.9210987975881));
#44219=CARTESIAN_POINT('Ctrl Pts',(19.3219111637762,12.0696111949304,39.9060435057152));
#44220=CARTESIAN_POINT('Ctrl Pts',(19.3149694069985,12.0691164692555,39.9034219432513));
#44221=CARTESIAN_POINT('Ctrl Pts',(19.3041777697033,12.0683492667924,39.8992751665651));
#44222=CARTESIAN_POINT('Ctrl Pts',(19.3003174740358,12.0680752093743,39.8977775348618));
#44223=CARTESIAN_POINT('Ctrl Pts',(19.2931473423426,12.067566920968,39.89496923359));
#44224=CARTESIAN_POINT('Ctrl Pts',(19.2898363431304,12.0673325072271,39.8936618438148));
#44225=CARTESIAN_POINT('Ctrl Pts',(19.2823139189638,12.0668006005164,39.8906674250551));
#44226=CARTESIAN_POINT('Ctrl Pts',(19.2781048208173,12.0665034513812,39.8889747033924));
#44227=CARTESIAN_POINT('Ctrl Pts',(19.2652647225308,12.0655983157268,39.8837582622424));
#44228=CARTESIAN_POINT('Ctrl Pts',(19.2566531029044,12.0649931056814,39.8801867500672));
#44229=CARTESIAN_POINT('Ctrl Pts',(19.1744167535828,12.0592282961597,39.8453799145038));
#44230=CARTESIAN_POINT('Ctrl Pts',(19.1027656157187,12.0543168698859,39.809652764802));
#44231=CARTESIAN_POINT('Ctrl Pts',(18.8911396409166,12.0395505057245,39.687148659267));
#44232=CARTESIAN_POINT('Ctrl Pts',(18.7598851654615,12.0299589513158,39.5868513144517));
#44233=CARTESIAN_POINT('Ctrl Pts',(18.6147535238725,12.0172169038948,39.4432082857444));
#44234=CARTESIAN_POINT('Ctrl Pts',(18.5874272912644,12.0147093882261,39.4144406765749));
#44235=CARTESIAN_POINT('Ctrl Pts',(18.5534568132957,12.0114363070004,39.376394896038));
#44236=CARTESIAN_POINT('Ctrl Pts',(18.5459798219425,12.0107056696838,39.3678708272194));
#44237=CARTESIAN_POINT('Ctrl Pts',(18.5340070934943,12.0095187452775,39.3539762353205));
#44238=CARTESIAN_POINT('Ctrl Pts',(18.5294646242508,12.0090643814645,39.3486461897602));
#44239=CARTESIAN_POINT('Ctrl Pts',(18.5208250585105,12.0081923477016,39.3383961566038));
#44240=CARTESIAN_POINT('Ctrl Pts',(18.5167232286311,12.0077748779611,39.3334802657873));
#44241=CARTESIAN_POINT('Ctrl Pts',(18.5074390774839,12.0068220087002,39.3222402789538));
#44242=CARTESIAN_POINT('Ctrl Pts',(18.5022723654489,12.006285991922,39.3159035061034));
#44243=CARTESIAN_POINT('Ctrl Pts',(18.4887526199817,12.0048680334814,39.2991051368935));
#44244=CARTESIAN_POINT('Ctrl Pts',(18.4804680514826,12.0039834010131,39.2885892541526));
#44245=CARTESIAN_POINT('Ctrl Pts',(18.4190115001122,11.9972999632436,39.2088876454116));
#44246=CARTESIAN_POINT('Ctrl Pts',(18.3704866374972,11.9913224552735,39.1362619048918));
#44247=CARTESIAN_POINT('Ctrl Pts',(18.3082514153552,11.9825650176364,39.0278761574961));
#44248=CARTESIAN_POINT('Ctrl Pts',(18.2904205048242,11.9798977569822,38.9945977826753));
#44249=CARTESIAN_POINT('Ctrl Pts',(18.2357998863346,11.9712044731663,38.8850529727456));
#44250=CARTESIAN_POINT('Ctrl Pts',(18.2030506959797,11.9651292595463,38.806882888797));
#44251=CARTESIAN_POINT('Ctrl Pts',(18.155094989453,11.9546934980988,38.667299070028));
#44252=CARTESIAN_POINT('Ctrl Pts',(18.1375699479435,11.9503006437687,38.6068122693153));
#44253=CARTESIAN_POINT('Ctrl Pts',(18.1200789722994,11.9451826545723,38.5331315641721));
#44254=CARTESIAN_POINT('Ctrl Pts',(18.1172495789451,11.9443244667038,38.5206624487318));
#44255=CARTESIAN_POINT('Ctrl Pts',(18.1134533078516,11.9431295122151,38.5031261866552));
#44256=CARTESIAN_POINT('Ctrl Pts',(18.1123825367493,11.9427871925066,38.4980822251391));
#44257=CARTESIAN_POINT('Ctrl Pts',(18.1105884941989,11.9422045424815,38.4894612123815));
#44258=CARTESIAN_POINT('Ctrl Pts',(18.1098551299822,11.9419636470719,38.4858863115054));
#44259=CARTESIAN_POINT('Ctrl Pts',(18.108463089275,11.941501104647,38.4790014006423));
#44260=CARTESIAN_POINT('Ctrl Pts',(18.1078029519872,11.9412793727008,38.4756917330097));
#44261=CARTESIAN_POINT('Ctrl Pts',(18.1060625213008,11.9406882894039,38.4668449399428));
#44262=CARTESIAN_POINT('Ctrl Pts',(18.1049978152948,11.9403198121827,38.4613047261026));
#44263=CARTESIAN_POINT('Ctrl Pts',(18.1012253161049,11.9389884210131,38.44119897386));
#44264=CARTESIAN_POINT('Ctrl Pts',(18.0986609428953,11.9380332064153,38.4266065861845));
#44265=CARTESIAN_POINT('Ctrl Pts',(18.0794575725492,11.9304408543882,38.3094276702888));
#44266=CARTESIAN_POINT('Ctrl Pts',(18.0709629304851,11.9241914034759,38.205664609979));
#44267=CARTESIAN_POINT('Ctrl Pts',(18.0707334764535,11.9087151054445,37.9468805119815));
#44268=CARTESIAN_POINT('Ctrl Pts',(18.0892346249004,11.8995431730862,37.7926169603208));
#44269=CARTESIAN_POINT('Ctrl Pts',(18.1310982777059,11.8883624079805,37.6212349761986));
#44270=CARTESIAN_POINT('Ctrl Pts',(18.136578699205,11.8869823470234,37.6003295168955));
#44271=CARTESIAN_POINT('Ctrl Pts',(18.1446649327772,11.8850527593879,37.5714697164514));
#44272=CARTESIAN_POINT('Ctrl Pts',(18.1469731684293,11.8845127800516,37.5634331074577));
#44273=CARTESIAN_POINT('Ctrl Pts',(18.1510394411321,11.8835796482179,37.5496147483513));
#44274=CARTESIAN_POINT('Ctrl Pts',(18.152772546919,11.8831873049853,37.5438257389201));
#44275=CARTESIAN_POINT('Ctrl Pts',(18.1564108489232,11.8823745421807,37.531877509525));
#44276=CARTESIAN_POINT('Ctrl Pts',(18.1583197770217,11.8819540057961,37.5257195138662));
#44277=CARTESIAN_POINT('Ctrl Pts',(18.1628519291694,11.8809690792889,37.5113542985195));
#44278=CARTESIAN_POINT('Ctrl Pts',(18.1654993248703,11.880403907923,37.5031549071008));
#44279=CARTESIAN_POINT('Ctrl Pts',(18.174238092862,11.8785703462414,37.4766971147556));
#44280=CARTESIAN_POINT('Ctrl Pts',(18.1805476571886,11.877294856603,37.4585125448242));
#44281=CARTESIAN_POINT('Ctrl Pts',(18.2143033974603,11.8707063114775,37.365733218681));
#44282=CARTESIAN_POINT('Ctrl Pts',(18.2460652388906,11.8652521565718,37.2928011453625));
#44283=CARTESIAN_POINT('Ctrl Pts',(18.3315283322058,11.8520997518482,37.1255879821471));
#44284=CARTESIAN_POINT('Ctrl Pts',(18.3888615229535,11.8443219046793,37.0334604316663));
#44285=CARTESIAN_POINT('Ctrl Pts',(18.5032681451682,11.8307241373128,36.8800683813324));
#44286=CARTESIAN_POINT('Ctrl Pts',(18.5571726610135,11.8248889240047,36.816764996132));
#44287=CARTESIAN_POINT('Ctrl Pts',(18.6215046106875,11.8186775026742,36.7504147181015));
#44288=CARTESIAN_POINT('Ctrl Pts',(18.6280617511577,11.8180524245044,36.7437494989938));
#44289=CARTESIAN_POINT('Ctrl Pts',(18.63787602175,11.8171290566407,36.7339174788928));
#44290=CARTESIAN_POINT('Ctrl Pts',(18.6410961763068,11.8168280153476,36.730714206019));
#44291=CARTESIAN_POINT('Ctrl Pts',(18.6468605696159,11.8162925928854,36.7250203950593));
#44292=CARTESIAN_POINT('Ctrl Pts',(18.6494004113494,11.8160578752119,36.7225255051657));
#44293=CARTESIAN_POINT('Ctrl Pts',(18.6549063698593,11.8155516281636,36.7171468639056));
#44294=CARTESIAN_POINT('Ctrl Pts',(18.6578748532003,11.8152802918852,36.7142656239474));
#44295=CARTESIAN_POINT('Ctrl Pts',(18.6661811527464,11.8145254236098,36.7062551741298));
#44296=CARTESIAN_POINT('Ctrl Pts',(18.6715393290097,11.8140434841966,36.701147038862));
#44297=CARTESIAN_POINT('Ctrl Pts',(18.7028063959762,11.8112591248584,36.6716807484468));
#44298=CARTESIAN_POINT('Ctrl Pts',(18.7293573469193,11.8090052219865,36.6480100663089));
#44299=CARTESIAN_POINT('Ctrl Pts',(18.8185245643896,11.801730028319,36.5728362179607));
#44300=CARTESIAN_POINT('Ctrl Pts',(18.8837366080479,11.7968621923528,36.5245408099081));
#44301=CARTESIAN_POINT('Ctrl Pts',(19.0805520101866,11.7828443763861,36.3971553927843));
#44302=CARTESIAN_POINT('Ctrl Pts',(19.2187658255787,11.7737523780295,36.329482769854));
#44303=CARTESIAN_POINT('Ctrl Pts',(19.3736905474639,11.7633525661543,36.2753370339213));
#44304=CARTESIAN_POINT('Ctrl Pts',(19.3838832094158,11.7626677251025,36.2718702030071));
#44305=CARTESIAN_POINT('Ctrl Pts',(19.3941040090521,11.7619801941421,36.2684889830926));
#44306=CARTESIAN_POINT('',(18.070870558151,11.7455906108586,38.0995325677651));
#44307=CARTESIAN_POINT('Ctrl Pts',(19.3941040036879,11.589834535998,36.2684889848672));
#44308=CARTESIAN_POINT('Ctrl Pts',(19.3847992552261,11.5904216648079,36.2715671590049));
#44309=CARTESIAN_POINT('Ctrl Pts',(19.3755170286381,11.591008177693,36.2747165499176));
#44310=CARTESIAN_POINT('Ctrl Pts',(19.2210205634771,11.600789172277,36.3284528217096));
#44311=CARTESIAN_POINT('Ctrl Pts',(19.0823620386687,11.6099032911439,36.3961447601399));
#44312=CARTESIAN_POINT('Ctrl Pts',(18.9350060058248,11.6210204272785,36.4913358843555));
#44313=CARTESIAN_POINT('Ctrl Pts',(18.9169980559991,11.6224046295,36.5034038789726));
#44314=CARTESIAN_POINT('Ctrl Pts',(18.8923230790278,11.6243390550331,36.5205493116066));
#44315=CARTESIAN_POINT('Ctrl Pts',(18.8854795765921,11.624879666536,36.5253708815999));
#44316=CARTESIAN_POINT('Ctrl Pts',(18.8737484620666,11.625813596965,36.5337507931408));
#44317=CARTESIAN_POINT('Ctrl Pts',(18.8688457559863,11.6262061033816,36.5372878769412));
#44318=CARTESIAN_POINT('Ctrl Pts',(18.8589297763901,11.6270044827186,36.5445129267101));
#44319=CARTESIAN_POINT('Ctrl Pts',(18.8539175653154,11.6274104036865,36.5482022226558));
#44320=CARTESIAN_POINT('Ctrl Pts',(18.8422591153987,11.6283601725191,36.5568708522089));
#44321=CARTESIAN_POINT('Ctrl Pts',(18.8356270435076,11.6289047434328,36.5618689466772));
#44322=CARTESIAN_POINT('Ctrl Pts',(18.8217370010024,11.6300544300048,36.572478143461));
#44323=CARTESIAN_POINT('Ctrl Pts',(18.8144863884877,11.6306598997217,36.5780984956274));
#44324=CARTESIAN_POINT('Ctrl Pts',(18.7952251635713,11.6322827884831,36.5932501049463));
#44325=CARTESIAN_POINT('Ctrl Pts',(18.7832878346289,11.6333038008267,36.6028730392944));
#44326=CARTESIAN_POINT('Ctrl Pts',(18.6883532289436,11.6415483802967,36.6812871987918));
#44327=CARTESIAN_POINT('Ctrl Pts',(18.6111536768575,11.6490443489946,36.756771672466));
#44328=CARTESIAN_POINT('Ctrl Pts',(18.455126308962,11.6659612014356,36.9372380237683));
#44329=CARTESIAN_POINT('Ctrl Pts',(18.379865355166,11.6754146641219,37.044625346559));
#44330=CARTESIAN_POINT('Ctrl Pts',(18.3010323377094,11.6865679109604,37.1856703429942));
#44331=CARTESIAN_POINT('Ctrl Pts',(18.2866602305069,11.6886659176534,37.2128940670595));
#44332=CARTESIAN_POINT('Ctrl Pts',(18.2696696300476,11.6912195433938,37.2470325912097));
#44333=CARTESIAN_POINT('Ctrl Pts',(18.2664320088598,11.6917096828299,37.2536321048101));
#44334=CARTESIAN_POINT('Ctrl Pts',(18.2614170613492,11.6924743119621,37.2640040020269));
#44335=CARTESIAN_POINT('Ctrl Pts',(18.2596141512818,11.692750328012,37.2677638306387));
#44336=CARTESIAN_POINT('Ctrl Pts',(18.2562959571921,11.6932603869921,37.2747416049217));
#44337=CARTESIAN_POINT('Ctrl Pts',(18.2547773944911,11.6934946242704,37.277957869008));
#44338=CARTESIAN_POINT('Ctrl Pts',(18.2513589976422,11.6940237706861,37.2852500852844));
#44339=CARTESIAN_POINT('Ctrl Pts',(18.2494645183888,11.6943183505608,37.2893284837318));
#44340=CARTESIAN_POINT('Ctrl Pts',(18.2437701394599,11.6952079500471,37.3017002743868));
#44341=CARTESIAN_POINT('Ctrl Pts',(18.2400147212215,11.6958003303856,37.3100141764609));
#44342=CARTESIAN_POINT('Ctrl Pts',(18.1930086331833,11.7032925200229,37.4160773300174));
#44343=CARTESIAN_POINT('Ctrl Pts',(18.157888858645,11.7097447425299,37.5172465445072));
#44344=CARTESIAN_POINT('Ctrl Pts',(18.0912163094748,11.7258131373009,37.7772502200088));
#44345=CARTESIAN_POINT('Ctrl Pts',(18.0709092920218,11.7353493249005,37.9380723583049));
#44346=CARTESIAN_POINT('Ctrl Pts',(18.0708700569582,11.7455896548511,38.099531214715));
#44347=CARTESIAN_POINT('Ctrl Pts',(18.0708700566166,11.7455897441458,38.0995326226208));
#44348=CARTESIAN_POINT('Ctrl Pts',(18.0708667520166,11.7464548413653,38.11317256992));
#44349=CARTESIAN_POINT('Ctrl Pts',(18.0710081096649,11.7473241274613,38.1268119579521));
#44350=CARTESIAN_POINT('Ctrl Pts',(18.0715353871247,11.7489349523901,38.1519541277993));
#44351=CARTESIAN_POINT('Ctrl Pts',(18.0718796265132,11.7496751891478,38.1634571554648));
#44352=CARTESIAN_POINT('Ctrl Pts',(18.0725689054531,11.7508212029005,38.181183564671));
#44353=CARTESIAN_POINT('Ctrl Pts',(18.0728412238664,11.7512247262145,38.1874096417373));
#44354=CARTESIAN_POINT('Ctrl Pts',(18.0734409464895,11.7520266431385,38.1997510611974));
#44355=CARTESIAN_POINT('Ctrl Pts',(18.0737673119516,11.7524249999186,38.2058663824237));
#44356=CARTESIAN_POINT('Ctrl Pts',(18.074525013846,11.753276039888,38.2188976466794));
#44357=CARTESIAN_POINT('Ctrl Pts',(18.0749645050548,11.7537289712671,38.2258130112067));
#44358=CARTESIAN_POINT('Ctrl Pts',(18.0761983387331,11.7549042164061,38.243703924058));
#44359=CARTESIAN_POINT('Ctrl Pts',(18.0770493435745,11.7556282825458,38.2546751892176));
#44360=CARTESIAN_POINT('Ctrl Pts',(18.0808285555749,11.7585362761984,38.2985277515414));
#44361=CARTESIAN_POINT('Ctrl Pts',(18.0845065341355,11.7607433321031,38.3313371052114));
#44362=CARTESIAN_POINT('Ctrl Pts',(18.1139570869446,11.7752962467233,38.544488538909));
#44363=CARTESIAN_POINT('Ctrl Pts',(18.1643236778433,11.7884429296676,38.7204796349323));
#44364=CARTESIAN_POINT('Ctrl Pts',(18.2648771594039,11.8058883528737,38.9456042813956));
#44365=CARTESIAN_POINT('Ctrl Pts',(18.2941027201047,11.810392163972,39.0031135480106));
#44366=CARTESIAN_POINT('Ctrl Pts',(18.3325911986786,11.8156256440845,39.0702875809741));
#44367=CARTESIAN_POINT('Ctrl Pts',(18.3391392588077,11.8164946155136,39.081453881314));
#44368=CARTESIAN_POINT('Ctrl Pts',(18.3484654887304,11.8177019154218,39.0969970740262));
#44369=CARTESIAN_POINT('Ctrl Pts',(18.3511494779868,11.8180459483263,39.1014296605992));
#44370=CARTESIAN_POINT('Ctrl Pts',(18.3557565683414,11.8186306278153,39.1089694973281));
#44371=CARTESIAN_POINT('Ctrl Pts',(18.3576706862402,11.818871849106,39.1120821780398));
#44372=CARTESIAN_POINT('Ctrl Pts',(18.3613664922593,11.8193343304889,39.1180540915133));
#44373=CARTESIAN_POINT('Ctrl Pts',(18.3631468318724,11.8195556787752,39.1209141062608));
#44374=CARTESIAN_POINT('Ctrl Pts',(18.3679121115936,11.8201443673867,39.1285247489712));
#44375=CARTESIAN_POINT('Ctrl Pts',(18.3709103280634,11.8205108465204,39.1332670891138));
#44376=CARTESIAN_POINT('Ctrl Pts',(18.3817933735479,11.8218273590555,39.1503158985907));
#44377=CARTESIAN_POINT('Ctrl Pts',(18.3897975464905,11.8227699158798,39.1625461225048));
#44378=CARTESIAN_POINT('Ctrl Pts',(18.4645086322899,11.831347574072,39.2739198416129));
#44379=CARTESIAN_POINT('Ctrl Pts',(18.5401634634514,11.8384669156742,39.3667703310375));
#44380=CARTESIAN_POINT('Ctrl Pts',(18.7172904129973,11.8535609628362,39.5470457904174));
#44381=CARTESIAN_POINT('Ctrl Pts',(18.8202228041047,11.8615148637864,39.6321246202758));
#44382=CARTESIAN_POINT('Ctrl Pts',(18.9460385741022,11.8710507719706,39.7158682700098));
#44383=CARTESIAN_POINT('Ctrl Pts',(18.9611234552733,11.8721907190265,39.7256077155327));
#44384=CARTESIAN_POINT('Ctrl Pts',(18.9850143982375,11.873992186421,39.7405643783623));
#44385=CARTESIAN_POINT('Ctrl Pts',(18.9937300119363,11.8746485652307,39.7459246507666));
#44386=CARTESIAN_POINT('Ctrl Pts',(19.0085317430884,11.8757621527334,39.7548664943664));
#44387=CARTESIAN_POINT('Ctrl Pts',(19.0145956982148,11.876218045587,39.7584844824404));
#44388=CARTESIAN_POINT('Ctrl Pts',(19.0265289638169,11.8771146481267,39.7655157750273));
#44389=CARTESIAN_POINT('Ctrl Pts',(19.0323967051017,11.8775552609616,39.7689315494957));
#44390=CARTESIAN_POINT('Ctrl Pts',(19.0436803203662,11.8784021224858,39.7754205450068));
#44391=CARTESIAN_POINT('Ctrl Pts',(19.049093291539,11.8788081890486,39.7784986632611));
#44392=CARTESIAN_POINT('Ctrl Pts',(19.0616646422348,11.8797508713398,39.7855671086773));
#44393=CARTESIAN_POINT('Ctrl Pts',(19.0688336944745,11.8802881657033,39.7895381112748));
#44394=CARTESIAN_POINT('Ctrl Pts',(19.0878366704714,11.8817117281409,39.7999063448686));
#44395=CARTESIAN_POINT('Ctrl Pts',(19.0997124108739,11.8826007213315,39.806225589545));
#44396=CARTESIAN_POINT('Ctrl Pts',(19.1910371336369,11.8894333605902,39.8536018421503));
#44397=CARTESIAN_POINT('Ctrl Pts',(19.2731767869918,11.8955650772468,39.889207690285));
#44398=CARTESIAN_POINT('Ctrl Pts',(19.5101773075653,11.913195221869,39.9729234790555));
#44399=CARTESIAN_POINT('Ctrl Pts',(19.6690481392435,11.9249908537421,40.0074161018928));
#44400=CARTESIAN_POINT('Ctrl Pts',(19.8604279017471,11.93823842866,40.0243112014333));
#44401=CARTESIAN_POINT('Ctrl Pts',(19.8905608729884,11.9402942175166,40.026259924992));
#44402=CARTESIAN_POINT('Ctrl Pts',(19.9277686787684,11.9427859336734,40.027790142086));
#44403=CARTESIAN_POINT('Ctrl Pts',(19.9348098762534,11.9432554018865,40.0280410906511));
#44404=CARTESIAN_POINT('Ctrl Pts',(19.9459089407901,11.9439920101512,40.0283757892356));
#44405=CARTESIAN_POINT('Ctrl Pts',(19.9499658806472,11.9442605368059,40.0284853162138));
#44406=CARTESIAN_POINT('Ctrl Pts',(19.9575945057654,11.9447640816737,40.02866718035));
#44407=CARTESIAN_POINT('Ctrl Pts',(19.9611660047791,11.9449992492878,40.0287423984462));
#44408=CARTESIAN_POINT('Ctrl Pts',(19.9693225404395,11.9455350275714,40.0288915152025));
#44409=CARTESIAN_POINT('Ctrl Pts',(19.9739076425209,11.9458352792141,40.0289589870954));
#44410=CARTESIAN_POINT('Ctrl Pts',(19.9860703682847,11.9466293819463,40.0290945922662));
#44411=CARTESIAN_POINT('Ctrl Pts',(19.9936483195658,11.9471217123832,40.0291344279974));
#44412=CARTESIAN_POINT('Ctrl Pts',(20.0471633339938,11.950582577631,40.0291004054082));
#44413=CARTESIAN_POINT('Ctrl Pts',(20.0930888457495,11.9534697678043,40.0274304139056));
#44414=CARTESIAN_POINT('Ctrl Pts',(20.1684737796634,11.9581361489141,40.0219878828372));
#44415=CARTESIAN_POINT('Ctrl Pts',(20.1979806192835,11.9599441722833,40.0191729046023));
#44416=CARTESIAN_POINT('Ctrl Pts',(20.392773193643,11.9718232889834,39.9960489127812));
#44417=CARTESIAN_POINT('Ctrl Pts',(20.5548892799386,11.9815068646078,39.9550932515951));
#44418=CARTESIAN_POINT('Ctrl Pts',(20.7496614401286,11.9945443683278,39.8780309266109));
#44419=CARTESIAN_POINT('Ctrl Pts',(20.7890470022918,11.9972537473934,39.8609061990242));
#44420=CARTESIAN_POINT('Ctrl Pts',(20.8383463656397,12.000754721376,39.8374848428605));
#44421=CARTESIAN_POINT('Ctrl Pts',(20.848820764612,12.0015049735651,39.8323918459337));
#44422=CARTESIAN_POINT('Ctrl Pts',(20.8655793436303,12.0027159939214,39.8240548018818));
#44423=CARTESIAN_POINT('Ctrl Pts',(20.8718930304937,12.0031746913167,39.8208704486929));
#44424=CARTESIAN_POINT('Ctrl Pts',(20.883874503638,12.0040499101917,39.8147446438005));
#44425=CARTESIAN_POINT('Ctrl Pts',(20.8895454832324,12.0044662030703,39.8118096165303));
#44426=CARTESIAN_POINT('Ctrl Pts',(20.9024487022078,12.0054181190964,39.8050500955126));
#44427=CARTESIAN_POINT('Ctrl Pts',(20.9096713551937,12.0059543666727,39.8012076623364));
#44428=CARTESIAN_POINT('Ctrl Pts',(20.9284027540773,12.0073540943327,39.7910892113087));
#44429=CARTESIAN_POINT('Ctrl Pts',(20.9398722015289,12.0082200861068,39.7847417086385));
#44430=CARTESIAN_POINT('Ctrl Pts',(21.019743907696,12.0143146010229,39.7394690979064));
#44431=CARTESIAN_POINT('Ctrl Pts',(21.0857637819588,12.0196873930672,39.6965120296976));
#44432=CARTESIAN_POINT('Ctrl Pts',(21.2815144847728,12.0366887182697,39.5513749254521));
#44433=CARTESIAN_POINT('Ctrl Pts',(21.4008895230141,12.0487053537516,39.4365142261852));
#44434=CARTESIAN_POINT('Ctrl Pts',(21.5277583354589,12.0627673644305,39.2785219812654));
#44435=CARTESIAN_POINT('Ctrl Pts',(21.5504656490871,12.0653436603892,39.2484843598443));
#44436=CARTESIAN_POINT('Ctrl Pts',(21.576640749079,12.068369318758,39.2116668192777));
#44437=CARTESIAN_POINT('Ctrl Pts',(21.5809646172689,12.0688710605764,39.205508956213));
#44438=CARTESIAN_POINT('Ctrl Pts',(21.5876248467642,12.0696467445179,39.1959047563196));
#44439=CARTESIAN_POINT('Ctrl Pts',(21.5899862075072,12.0699223230541,39.1924759721553));
#44440=CARTESIAN_POINT('Ctrl Pts',(21.5943447108031,12.0704319826447,39.1861031972554));
#44441=CARTESIAN_POINT('Ctrl Pts',(21.59634479308,12.0706662554669,39.1831613517417));
#44442=CARTESIAN_POINT('Ctrl Pts',(21.6008596500037,12.0711960010508,39.1764809509586));
#44443=CARTESIAN_POINT('Ctrl Pts',(21.6033694674206,12.0714911413672,39.172739114952));
#44444=CARTESIAN_POINT('Ctrl Pts',(21.6109452600013,12.0723841178648,39.16135853469));
#44445=CARTESIAN_POINT('Ctrl Pts',(21.6159700153187,12.0729792852458,39.1536923115998));
#44446=CARTESIAN_POINT('Ctrl Pts',(21.6802773058293,12.0806380882972,39.0540372240027));
#44447=CARTESIAN_POINT('Ctrl Pts',(21.7316921262177,12.087232756108,38.9571864849764));
#44448=CARTESIAN_POINT('Ctrl Pts',(21.8073272938944,12.0987734127171,38.7797555959279));
#44449=CARTESIAN_POINT('Ctrl Pts',(21.8350240704192,12.1037254674551,38.7009873949841));
#44450=CARTESIAN_POINT('Ctrl Pts',(21.8787163698481,12.113536726854,38.5451132135908));
#44451=CARTESIAN_POINT('Ctrl Pts',(21.8952644423721,12.118374732858,38.4683361554826));
#44452=CARTESIAN_POINT('Ctrl Pts',(21.9099723956715,12.1245777788818,38.3718704217822));
#44453=CARTESIAN_POINT('Ctrl Pts',(21.9125728642164,12.1258014064445,38.3529289936295));
#44454=CARTESIAN_POINT('Ctrl Pts',(21.9159334081861,12.1275877469895,38.3254230916756));
#44455=CARTESIAN_POINT('Ctrl Pts',(21.9169184856031,12.1281434342293,38.3168868610455));
#44456=CARTESIAN_POINT('Ctrl Pts',(21.9185423681137,12.129118931081,38.3019387430238));
#44457=CARTESIAN_POINT('Ctrl Pts',(21.9192061444247,12.1295379547332,38.2955296594074));
#44458=CARTESIAN_POINT('Ctrl Pts',(21.9204308306483,12.1303523364546,38.2830971784982));
#44459=CARTESIAN_POINT('Ctrl Pts',(21.9209955413117,12.1307475707419,38.2770742243838));
#44460=CARTESIAN_POINT('Ctrl Pts',(21.9222755029665,12.1316928576013,38.2626953595162));
#44461=CARTESIAN_POINT('Ctrl Pts',(21.9229646078136,12.132243718411,38.2543373015887));
#44462=CARTESIAN_POINT('Ctrl Pts',(21.9252462923784,12.1342305308373,38.2242702163021));
#44463=CARTESIAN_POINT('Ctrl Pts',(21.926525863421,12.1356761481378,38.2025397724955));
#44464=CARTESIAN_POINT('Ctrl Pts',(21.933818565484,12.147331889191,38.0285616240693));
#44465=CARTESIAN_POINT('Ctrl Pts',(21.9221410062127,12.1581086987237,37.8761387541007));
#44466=CARTESIAN_POINT('Ctrl Pts',(21.8768431373976,12.1748131355117,37.6464673768813));
#44467=CARTESIAN_POINT('Ctrl Pts',(21.8559287623335,12.1806455460191,37.5673067433111));
#44468=CARTESIAN_POINT('Ctrl Pts',(21.8187435340262,12.1887902004488,37.4558012035432));
#44469=CARTESIAN_POINT('Ctrl Pts',(21.8064948763291,12.1912333889468,37.4222118367068));
#44470=CARTESIAN_POINT('Ctrl Pts',(21.7905864737342,12.1941236772767,37.382088028064));
#44471=CARTESIAN_POINT('Ctrl Pts',(21.7878142554608,12.1946179710928,37.3752119539274));
#44472=CARTESIAN_POINT('Ctrl Pts',(21.783432578722,12.1953846507579,37.3645219739979));
#44473=CARTESIAN_POINT('Ctrl Pts',(21.7818504053442,12.1956586138327,37.3606970692921));
#44474=CARTESIAN_POINT('Ctrl Pts',(21.7788845763381,12.1961668172798,37.3535920054577));
#44475=CARTESIAN_POINT('Ctrl Pts',(21.7775041648888,12.1964012398475,37.3503106147376));
#44476=CARTESIAN_POINT('Ctrl Pts',(21.774343164509,12.1969332817196,37.3428543797382));
#44477=CARTESIAN_POINT('Ctrl Pts',(21.7725569238967,12.1972305564748,37.3386819926555));
#44478=CARTESIAN_POINT('Ctrl Pts',(21.767052833198,12.1981364581636,37.3259496559369));
#44479=CARTESIAN_POINT('Ctrl Pts',(21.7632875121547,12.1987423017599,37.3174101914648));
#44480=CARTESIAN_POINT('Ctrl Pts',(21.726235959192,12.2045749421816,37.2350052037527));
#44481=CARTESIAN_POINT('Ctrl Pts',(21.6883849867663,12.2095469840815,37.1632683371349));
#44482=CARTESIAN_POINT('Ctrl Pts',(21.5606599440557,12.2243323900068,36.9542461766252));
#44483=CARTESIAN_POINT('Ctrl Pts',(21.4577192458435,12.2338930907415,36.8258472871048));
#44484=CARTESIAN_POINT('Ctrl Pts',(21.3115113143279,12.2465773107174,36.6847174203685));
#44485=CARTESIAN_POINT('Ctrl Pts',(21.282412877523,12.2490616396196,36.6582983734788));
#44486=CARTESIAN_POINT('Ctrl Pts',(21.2439340760874,12.2523084760693,36.6254497983625));
#44487=CARTESIAN_POINT('Ctrl Pts',(21.2352744164194,12.2530367556515,36.6181878020119));
#44488=CARTESIAN_POINT('Ctrl Pts',(21.2211525660466,12.254220783788,36.6065550239984));
#44489=CARTESIAN_POINT('Ctrl Pts',(21.2157294472782,12.2546746264976,36.6021370574069));
#44490=CARTESIAN_POINT('Ctrl Pts',(21.2052949967704,12.2555462931071,36.5937305858084));
#44491=CARTESIAN_POINT('Ctrl Pts',(21.2002875857202,12.2559639202724,36.5897373449361));
#44492=CARTESIAN_POINT('Ctrl Pts',(21.1888298787898,12.2569180275994,36.5806931864642));
#44493=CARTESIAN_POINT('Ctrl Pts',(21.1823671412532,12.257455130753,36.5756583013783));
#44494=CARTESIAN_POINT('Ctrl Pts',(21.1652159149453,12.2588778544036,36.5624710960687));
#44495=CARTESIAN_POINT('Ctrl Pts',(21.1544741012035,12.2597661948697,36.5543891844834));
#44496=CARTESIAN_POINT('Ctrl Pts',(21.0717093789921,12.2665914126742,36.493462931605));
#44497=CARTESIAN_POINT('Ctrl Pts',(20.9961892849935,12.2727159278967,36.4455740968745));
#44498=CARTESIAN_POINT('Ctrl Pts',(20.775446145391,12.2903171298382,36.3262031637697));
#44499=CARTESIAN_POINT('Ctrl Pts',(20.6241695646565,12.302089960567,36.267493262113));
#44500=CARTESIAN_POINT('Ctrl Pts',(20.4377021427713,12.3153467701843,36.2209329114971));
#44501=CARTESIAN_POINT('Ctrl Pts',(20.4078815416648,12.3174281133537,36.2142351164447));
#44502=CARTESIAN_POINT('Ctrl Pts',(20.3709772532854,12.3199463507237,36.2068628020227));
#44503=CARTESIAN_POINT('Ctrl Pts',(20.3640343891044,12.3204176196015,36.2055154948656));
#44504=CARTESIAN_POINT('Ctrl Pts',(20.353090116737,12.3211564118,36.2034540752868));
#44505=CARTESIAN_POINT('Ctrl Pts',(20.3490936789788,12.3214253352063,36.2027143917852));
#44506=CARTESIAN_POINT('Ctrl Pts',(20.3415812732448,12.3219292060278,36.2013484931997));
#44507=CARTESIAN_POINT('Ctrl Pts',(20.3380659445226,12.3221643052714,36.2007194183288));
#44508=CARTESIAN_POINT('Ctrl Pts',(20.3300421087723,12.3226993985278,36.1993065204055));
#44509=CARTESIAN_POINT('Ctrl Pts',(20.3255325495797,12.3229990369049,36.1985289754604));
#44510=CARTESIAN_POINT('Ctrl Pts',(20.3135798019636,12.3237904428302,36.1965118332401));
#44511=CARTESIAN_POINT('Ctrl Pts',(20.3061319442596,12.3242807061441,36.195299831885));
#44512=CARTESIAN_POINT('Ctrl Pts',(20.2539218335032,12.3276986372308,36.1871177560539));
#44513=CARTESIAN_POINT('Ctrl Pts',(20.208929297298,12.3305472098203,36.1816819669351));
#44514=CARTESIAN_POINT('Ctrl Pts',(20.0269101550315,12.3418320492146,36.1661725411715));
#44515=CARTESIAN_POINT('Ctrl Pts',(19.8891744838841,12.3498530059803,36.1691617887092));
#44516=CARTESIAN_POINT('Ctrl Pts',(19.6884441257685,12.3620623308559,36.1950849140065));
#44517=CARTESIAN_POINT('Ctrl Pts',(19.6244388164892,12.3660306662166,36.2066639799372));
#44518=CARTESIAN_POINT('Ctrl Pts',(19.5239358809418,12.3724784752898,36.2301429249375));
#44519=CARTESIAN_POINT('Ctrl Pts',(19.4869968082867,12.3748955523179,36.2399381895636));
#44520=CARTESIAN_POINT('Ctrl Pts',(19.4396464623003,12.3780661859068,36.2540119895151));
#44521=CARTESIAN_POINT('Ctrl Pts',(19.4289462750206,12.3787875034616,36.2572939852841));
#44522=CARTESIAN_POINT('Ctrl Pts',(19.4116291418237,12.3799629835065,36.2627708684501));
#44523=CARTESIAN_POINT('Ctrl Pts',(19.4049943666356,12.3804152912751,36.2649088734563));
#44524=CARTESIAN_POINT('Ctrl Pts',(19.3969483833219,12.3809662089533,36.2675498512499));
#44525=CARTESIAN_POINT('Ctrl Pts',(19.3955259198999,12.381063698177,36.2680185900266));
#44526=CARTESIAN_POINT('Ctrl Pts',(19.3941040087481,12.3811612414289,36.2684889831931));
#44527=CARTESIAN_POINT('Origin',(20.,-1.3495818343519,38.1));
#44528=CARTESIAN_POINT('',(19.3941040122263,13.3471516131145,36.2684889820425));
#44529=CARTESIAN_POINT('',(19.3941040017606,13.1771182491666,36.2684889855047));
#44530=CARTESIAN_POINT('',(19.3941040087494,-1.3495818343519,36.2684889831927));
#44531=CARTESIAN_POINT('',(18.070870312024,12.710826110243,38.0989027900441));
#44532=CARTESIAN_POINT('Ctrl Pts',(19.3941040122264,13.3471516131145,36.2684889820425));
#44533=CARTESIAN_POINT('Ctrl Pts',(19.4104866366325,13.3459230207428,36.2630693223737));
#44534=CARTESIAN_POINT('Ctrl Pts',(19.4269473258092,13.3446960253705,36.2578677037214));
#44535=CARTESIAN_POINT('Ctrl Pts',(19.4546956134867,13.3426420104863,36.2495074043374));
#44536=CARTESIAN_POINT('Ctrl Pts',(19.46594005021,13.3418135851885,36.2462309483532));
#44537=CARTESIAN_POINT('Ctrl Pts',(19.4922436281491,13.3398857010468,36.2388256864404));
#44538=CARTESIAN_POINT('Ctrl Pts',(19.5073246304984,13.3387879650191,36.2347768609654));
#44539=CARTESIAN_POINT('Ctrl Pts',(19.5693839592259,13.3343057046446,36.2189208860509));
#44540=CARTESIAN_POINT('Ctrl Pts',(19.6167541759491,13.3309658843936,36.2087008831235));
#44541=CARTESIAN_POINT('Ctrl Pts',(19.6720309607961,13.3271988364703,36.1989376852914));
#44542=CARTESIAN_POINT('Ctrl Pts',(19.6796068318972,13.3266853660904,36.1976462374905));
#44543=CARTESIAN_POINT('Ctrl Pts',(19.6917462656369,13.3258673104694,36.195651421404));
#44544=CARTESIAN_POINT('Ctrl Pts',(19.6963048919101,13.3255611755419,36.194919120885));
#44545=CARTESIAN_POINT('Ctrl Pts',(19.7043990621246,13.3250195487343,36.1936486600551));
#44546=CARTESIAN_POINT('Ctrl Pts',(19.7079335239297,13.3247836946747,36.1931039566469));
#44547=CARTESIAN_POINT('Ctrl Pts',(19.7154635278836,13.3242826312277,36.1919649191741));
#44548=CARTESIAN_POINT('Ctrl Pts',(19.7194594222162,13.3240175751984,36.1913733055976));
#44549=CARTESIAN_POINT('Ctrl Pts',(19.7303449656706,13.3232977276198,36.1897965668133));
#44550=CARTESIAN_POINT('Ctrl Pts',(19.7372382175781,13.3228442970681,36.1888361548501));
#44551=CARTESIAN_POINT('Ctrl Pts',(19.7729223355767,13.3205087975777,36.1840611323613));
#44552=CARTESIAN_POINT('Ctrl Pts',(19.801793241533,13.3186587734508,36.1808594861779));
#44553=CARTESIAN_POINT('Ctrl Pts',(19.9899276761389,13.3067958172471,36.1642875926935));
#44554=CARTESIAN_POINT('Ctrl Pts',(20.1502705285004,13.2975358824369,36.1700997341512));
#44555=CARTESIAN_POINT('Ctrl Pts',(20.3995782342778,13.2822797140152,36.2104307659568));
#44556=CARTESIAN_POINT('Ctrl Pts',(20.4898846891814,13.2765770051853,36.2318072271933));
#44557=CARTESIAN_POINT('Ctrl Pts',(20.5912028442351,13.2697946368871,36.2636436248688));
#44558=CARTESIAN_POINT('Ctrl Pts',(20.6040645742524,13.2689265351607,36.2678342010854));
#44559=CARTESIAN_POINT('Ctrl Pts',(20.6246669120749,13.26752400971,36.2747873185555));
#44560=CARTESIAN_POINT('Ctrl Pts',(20.6324359413459,13.2669923676292,36.2774647163344));
#44561=CARTESIAN_POINT('Ctrl Pts',(20.6462326667885,13.2660432210262,36.282318244735));
#44562=CARTESIAN_POINT('Ctrl Pts',(20.6522671081762,13.2656263609765,36.2844749406881));
#44563=CARTESIAN_POINT('Ctrl Pts',(20.6648542174755,13.2647531879786,36.2890444001578));
#44564=CARTESIAN_POINT('Ctrl Pts',(20.6714047442395,13.2642966953321,36.2914627506309));
#44565=CARTESIAN_POINT('Ctrl Pts',(20.6884708075529,13.2631018799049,36.2978687669469));
#44566=CARTESIAN_POINT('Ctrl Pts',(20.6989647350276,13.2623616932598,36.3019128708161));
#44567=CARTESIAN_POINT('Ctrl Pts',(20.7454497181009,13.2590579260164,36.3202954705671));
#44568=CARTESIAN_POINT('Ctrl Pts',(20.7810371849496,13.2564615338074,36.3356236103787));
#44569=CARTESIAN_POINT('Ctrl Pts',(20.8762398377979,13.2493258909702,36.3800738017463));
#44570=CARTESIAN_POINT('Ctrl Pts',(20.9348494356302,13.2447233313987,36.4112142358477));
#44571=CARTESIAN_POINT('Ctrl Pts',(21.0915521980205,13.2318601121271,36.5051335256935));
#44572=CARTESIAN_POINT('Ctrl Pts',(21.1857467305076,13.2234729694017,36.573864933976));
#44573=CARTESIAN_POINT('Ctrl Pts',(21.2848959874715,13.2141622415327,36.6609626791333));
#44574=CARTESIAN_POINT('Ctrl Pts',(21.2964955796549,13.2130650678889,36.6714044166166));
#44575=CARTESIAN_POINT('Ctrl Pts',(21.3435735045677,13.2085832189015,36.7148288044768));
#44576=CARTESIAN_POINT('Ctrl Pts',(21.3779335204569,13.2052432554018,36.7490043967403));
#44577=CARTESIAN_POINT('Ctrl Pts',(21.4162141110084,13.2014760658311,36.790061372385));
#44578=CARTESIAN_POINT('Ctrl Pts',(21.4214213368371,13.200962589925,36.7957136034056));
#44579=CARTESIAN_POINT('Ctrl Pts',(21.4297027205722,13.20014452721,36.8048112089124));
#44580=CARTESIAN_POINT('Ctrl Pts',(21.4327984623419,13.1998383906732,36.8082366930513));
#44581=CARTESIAN_POINT('Ctrl Pts',(21.438270173611,13.1992967620524,36.8143350928391));
#44582=CARTESIAN_POINT('Ctrl Pts',(21.4406510429733,13.1990609077802,36.8170035389755));
#44583=CARTESIAN_POINT('Ctrl Pts',(21.4457053862687,13.1985598450376,36.8227001880427));
#44584=CARTESIAN_POINT('Ctrl Pts',(21.4483767698581,13.1982947899194,36.8257301671977));
#44585=CARTESIAN_POINT('Ctrl Pts',(21.4556247822914,13.1975749473947,36.8340033625685));
#44586=CARTESIAN_POINT('Ctrl Pts',(21.4601826415725,13.1971215209537,36.8392630529444));
#44587=CARTESIAN_POINT('Ctrl Pts',(21.4836118063188,13.1947860794523,36.8665974015581));
#44588=CARTESIAN_POINT('Ctrl Pts',(21.5020125127447,13.1929361073085,36.8890728370711));
#44589=CARTESIAN_POINT('Ctrl Pts',(21.6183205435363,13.1810733513055,37.0378692237385));
#44590=CARTESIAN_POINT('Ctrl Pts',(21.7007243985576,13.1718135505467,37.1755369235098));
#44591=CARTESIAN_POINT('Ctrl Pts',(21.802600615668,13.1565573547744,37.406626873208));
#44592=CARTESIAN_POINT('Ctrl Pts',(21.8338269770233,13.1508544504002,37.4940210563692));
#44593=CARTESIAN_POINT('Ctrl Pts',(21.8622724628248,13.144071865199,37.5963465319282));
#44594=CARTESIAN_POINT('Ctrl Pts',(21.8657582438401,13.1432037583718,37.6094169771574));
#44595=CARTESIAN_POINT('Ctrl Pts',(21.8711401114591,13.1418012262648,37.6304845399501));
#44596=CARTESIAN_POINT('Ctrl Pts',(21.873123094322,13.1412695826714,37.6384591523824));
#44597=CARTESIAN_POINT('Ctrl Pts',(21.8765616818611,13.1403204343388,37.6526747522642));
#44598=CARTESIAN_POINT('Ctrl Pts',(21.878037261573,13.1399035740804,37.6589108190113));
#44599=CARTESIAN_POINT('Ctrl Pts',(21.8810556999298,13.139030401638,37.6719570480719));
#44600=CARTESIAN_POINT('Ctrl Pts',(21.8825927065103,13.1385739097609,37.6787684553881));
#44601=CARTESIAN_POINT('Ctrl Pts',(21.8865085594151,13.1373790985584,37.6965715824627));
#44602=CARTESIAN_POINT('Ctrl Pts',(21.8888282998934,13.1366389153929,37.7075758961327));
#44603=CARTESIAN_POINT('Ctrl Pts',(21.8987110557985,13.1333351861143,37.7565763829884));
#44604=CARTESIAN_POINT('Ctrl Pts',(21.9052242331493,13.1307388293194,37.7947726915976));
#44605=CARTESIAN_POINT('Ctrl Pts',(21.9197584446584,13.1236033125858,37.8988291196341));
#44606=CARTESIAN_POINT('Ctrl Pts',(21.925539047832,13.1190008464822,37.9649443521454));
#44607=CARTESIAN_POINT('Ctrl Pts',(21.9320502179657,13.1061423907135,38.1474533354929));
#44608=CARTESIAN_POINT('Ctrl Pts',(21.9256770709189,13.0977601445207,38.2638168473678));
#44609=CARTESIAN_POINT('Ctrl Pts',(21.9065937978554,13.0884471474128,38.3944302193596));
#44610=CARTESIAN_POINT('Ctrl Pts',(21.9041343466194,13.0873433232281,38.4099378549386));
#44611=CARTESIAN_POINT('Ctrl Pts',(21.8933188571675,13.0828566601612,38.4731358037159));
#44612=CARTESIAN_POINT('Ctrl Pts',(21.8833574585024,13.0795184403877,38.520537999419));
#44613=CARTESIAN_POINT('Ctrl Pts',(21.8697596235999,13.0757529751212,38.5749742635082));
#44614=CARTESIAN_POINT('Ctrl Pts',(21.8678528600873,13.0752395665345,38.5824181784729));
#44615=CARTESIAN_POINT('Ctrl Pts',(21.8647293369496,13.0744215902376,38.5943160638661));
#44616=CARTESIAN_POINT('Ctrl Pts',(21.863541002051,13.0741154733053,38.5987773108806));
#44617=CARTESIAN_POINT('Ctrl Pts',(21.8614037783182,13.0735738667729,38.6066866088654));
#44618=CARTESIAN_POINT('Ctrl Pts',(21.8604613041627,13.0733380150907,38.6101363367485));
#44619=CARTESIAN_POINT('Ctrl Pts',(21.8584337870053,13.072836943765,38.6174772789418));
#44620=CARTESIAN_POINT('Ctrl Pts',(21.8573461149006,13.0725718775461,38.6213677062395));
#44621=CARTESIAN_POINT('Ctrl Pts',(21.8543510806332,13.0718519734385,38.6319521344957));
#44622=CARTESIAN_POINT('Ctrl Pts',(21.8524196748341,13.0713984969087,38.6386393557295));
#44623=CARTESIAN_POINT('Ctrl Pts',(21.8422399281184,13.0690623487005,38.6731828681232));
#44624=CARTESIAN_POINT('Ctrl Pts',(21.8333987925271,13.0672117430411,38.7008624147925));
#44625=CARTESIAN_POINT('Ctrl Pts',(21.771872335493,13.055346545361,38.8794622835719));
#44626=CARTESIAN_POINT('Ctrl Pts',(21.7012229380199,13.0460851093458,39.0235506671442));
#44627=CARTESIAN_POINT('Ctrl Pts',(21.5628153516968,13.0308292464975,39.2347845284807));
#44628=CARTESIAN_POINT('Ctrl Pts',(21.5065230114638,13.0251287268431,39.3085167596184));
#44629=CARTESIAN_POINT('Ctrl Pts',(21.4361966824007,13.0183487868164,39.3880468176911));
#44630=CARTESIAN_POINT('Ctrl Pts',(21.4271303824469,13.0174807422252,39.3980848861556));
#44631=CARTESIAN_POINT('Ctrl Pts',(21.4123878709626,13.0160782913333,39.4140664294999));
#44632=CARTESIAN_POINT('Ctrl Pts',(21.4067778263824,13.0155466661956,39.4200705371096));
#44633=CARTESIAN_POINT('Ctrl Pts',(21.3967247845257,13.0145975389675,39.4306928642066));
#44634=CARTESIAN_POINT('Ctrl Pts',(21.3922967857882,13.0141806812558,39.4353251593499));
#44635=CARTESIAN_POINT('Ctrl Pts',(21.3829956941587,13.0133075020316,39.4449588197553));
#44636=CARTESIAN_POINT('Ctrl Pts',(21.3781183699987,13.0128510007657,39.4499559522515));
#44637=CARTESIAN_POINT('Ctrl Pts',(21.3653148824627,13.011656138009,39.4629322502915));
#44638=CARTESIAN_POINT('Ctrl Pts',(21.3573459742881,13.010915912381,39.4708686823296));
#44639=CARTESIAN_POINT('Ctrl Pts',(21.3216155433143,13.0076117197749,39.5058365125635));
#44640=CARTESIAN_POINT('Ctrl Pts',(21.293114415621,13.005014930777,39.5320959069014));
#44641=CARTESIAN_POINT('Ctrl Pts',(21.2137188031712,12.9978778749748,39.6009433611213));
#44642=CARTESIAN_POINT('Ctrl Pts',(21.1613899964115,12.9932742680904,39.641789877225));
#44643=CARTESIAN_POINT('Ctrl Pts',(20.9967247244561,12.97911704074,39.7571771174533));
#44644=CARTESIAN_POINT('Ctrl Pts',(20.8785927519293,12.9693661124324,39.8227214746303));
#44645=CARTESIAN_POINT('Ctrl Pts',(20.7123522386906,12.9567470631984,39.8933778168564));
#44646=CARTESIAN_POINT('Ctrl Pts',(20.6694745084918,12.9535868605786,39.9098216409358));
#44647=CARTESIAN_POINT('Ctrl Pts',(20.6188808313852,12.949998050936,39.9271799240489));
#44648=CARTESIAN_POINT('Ctrl Pts',(20.6116999432382,12.9494919221188,39.9295964424867));
#44649=CARTESIAN_POINT('Ctrl Pts',(20.6001506873117,12.9486832967249,39.9334074104137));
#44650=CARTESIAN_POINT('Ctrl Pts',(20.5957913486339,12.9483793051997,39.9348286704784));
#44651=CARTESIAN_POINT('Ctrl Pts',(20.5880267023203,12.9478400857853,39.9373295608548));
#44652=CARTESIAN_POINT('Ctrl Pts',(20.5846234186874,12.9476045073072,39.9384152895781));
#44653=CARTESIAN_POINT('Ctrl Pts',(20.5773469980773,12.9471024705249,39.9407143921046));
#44654=CARTESIAN_POINT('Ctrl Pts',(20.573473048543,12.9468361736054,39.9419249965286));
#44655=CARTESIAN_POINT('Ctrl Pts',(20.5628626993358,12.9461094360908,39.945203998203));
#44656=CARTESIAN_POINT('Ctrl Pts',(20.5561186589963,12.9456504007926,39.9472477511557));
#44657=CARTESIAN_POINT('Ctrl Pts',(20.5204076043933,12.9432342022211,39.9578565383805));
#44658=CARTESIAN_POINT('Ctrl Pts',(20.4912517458491,12.9413117792703,39.965777843303));
#44659=CARTESIAN_POINT('Ctrl Pts',(20.3047241725903,12.9292599988344,40.0117790572774));
#44660=CARTESIAN_POINT('Ctrl Pts',(20.1432575342885,12.91988983781,40.03060757333));
#44661=CARTESIAN_POINT('Ctrl Pts',(19.8918904887004,12.9046833221753,40.0281736255631));
#44662=CARTESIAN_POINT('Ctrl Pts',(19.8026391473951,12.8991723910193,40.0210899929774));
#44663=CARTESIAN_POINT('Ctrl Pts',(19.7009114083019,12.8926025723142,40.0058513434477));
#44664=CARTESIAN_POINT('Ctrl Pts',(19.687636081004,12.8917396596755,40.0037205930605));
#44665=CARTESIAN_POINT('Ctrl Pts',(19.6663086228007,12.8903439070732,40.0000683545536));
#44666=CARTESIAN_POINT('Ctrl Pts',(19.6582418672984,12.8898138052589,39.9986339990952));
#44667=CARTESIAN_POINT('Ctrl Pts',(19.643885928606,12.8888664179622,39.9959869058434));
#44668=CARTESIAN_POINT('Ctrl Pts',(19.6375931495088,12.8884497684525,39.9947941450312));
#44669=CARTESIAN_POINT('Ctrl Pts',(19.6244408518261,12.887576019657,39.992233285598));
#44670=CARTESIAN_POINT('Ctrl Pts',(19.617582612476,12.8871187356132,39.9908591752054));
#44671=CARTESIAN_POINT('Ctrl Pts',(19.5996645967671,12.8859195752531,39.9871676687298));
#44672=CARTESIAN_POINT('Ctrl Pts',(19.5886175725973,12.8851758099725,39.9847903687745));
#44673=CARTESIAN_POINT('Ctrl Pts',(19.5392666116037,12.8818327482801,39.9737155941892));
#44674=CARTESIAN_POINT('Ctrl Pts',(19.5012151413987,12.8791996711569,39.9639470665539));
#44675=CARTESIAN_POINT('Ctrl Pts',(19.3060465410578,12.8653946924124,39.9074395605454));
#44676=CARTESIAN_POINT('Ctrl Pts',(19.1550739613653,12.8536174360061,39.8419791046248));
#44677=CARTESIAN_POINT('Ctrl Pts',(18.9445484973521,12.8362234263025,39.7168288036242));
#44678=CARTESIAN_POINT('Ctrl Pts',(18.8775416623102,12.8305335302837,39.6710518013999));
#44679=CARTESIAN_POINT('Ctrl Pts',(18.8062448970758,12.8244567138134,39.6154466299317));
#44680=CARTESIAN_POINT('Ctrl Pts',(18.7989240432594,12.823832495801,39.6096510486458));
#44681=CARTESIAN_POINT('Ctrl Pts',(18.7881067434159,12.8229101480593,39.6009589929291));
#44682=CARTESIAN_POINT('Ctrl Pts',(18.7845781112529,12.8226092753919,39.598103066284));
#44683=CARTESIAN_POINT('Ctrl Pts',(18.7783002468361,12.8220740358612,39.5929852456389));
#44684=CARTESIAN_POINT('Ctrl Pts',(18.7755471708376,12.821839333429,39.5907281779216));
#44685=CARTESIAN_POINT('Ctrl Pts',(18.7727872050046,12.8216040671038,39.5884526572878));
#44686=CARTESIAN_POINT('Ctrl Pts',(18.7727741229622,12.8216029519586,39.5884418711916));
#44687=CARTESIAN_POINT('Ctrl Pts',(18.7727481362398,12.8216007367877,39.5884204446584));
#44688=CARTESIAN_POINT('Ctrl Pts',(18.7727352311704,12.8215996367288,39.588409803908));
#44689=CARTESIAN_POINT('Ctrl Pts',(18.772709594357,12.8215974513866,39.588388664761));
#44690=CARTESIAN_POINT('Ctrl Pts',(18.7726968627564,12.8215963661155,39.5883781664901));
#44691=CARTESIAN_POINT('Ctrl Pts',(18.7726715698982,12.8215942100944,39.5883573098651));
#44692=CARTESIAN_POINT('Ctrl Pts',(18.7726590086188,12.8215931393426,39.5883469515004));
#44693=CARTESIAN_POINT('Ctrl Pts',(18.7726340532885,12.8215910120948,39.5883263721413));
#44694=CARTESIAN_POINT('Ctrl Pts',(18.7726216591897,12.8215899555946,39.5883161511144));
#44695=CARTESIAN_POINT('Ctrl Pts',(18.772597035398,12.8215878566093,39.5882958441243));
#44696=CARTESIAN_POINT('Ctrl Pts',(18.7725848055628,12.821586814112,39.5882857580505));
#44697=CARTESIAN_POINT('Ctrl Pts',(18.7725605068196,12.821584742836,39.5882657181181));
#44698=CARTESIAN_POINT('Ctrl Pts',(18.7725484380574,12.8215837140697,39.5882557643864));
#44699=CARTESIAN_POINT('Ctrl Pts',(18.7725244592334,12.8215816700656,39.5882359873212));
#44700=CARTESIAN_POINT('Ctrl Pts',(18.7725125489533,12.8215806548093,39.5882261638143));
#44701=CARTESIAN_POINT('Ctrl Pts',(18.7693324349942,12.8213095755693,39.5856031662366));
#44702=CARTESIAN_POINT('Ctrl Pts',(18.7661725477835,12.8210402445904,39.5829798521973));
#44703=CARTESIAN_POINT('Ctrl Pts',(18.7574928997894,12.8203004298393,39.5757271295888));
#44704=CARTESIAN_POINT('Ctrl Pts',(18.7519905862658,12.8198314252761,39.5710768036695));
#44705=CARTESIAN_POINT('Ctrl Pts',(18.7396084035956,12.8187756285039,39.5604924241627));
#44706=CARTESIAN_POINT('Ctrl Pts',(18.7327440929185,12.8181900663589,39.5545403296896));
#44707=CARTESIAN_POINT('Ctrl Pts',(18.711354852398,12.8163636818709,39.5357272038118));
#44708=CARTESIAN_POINT('Ctrl Pts',(18.6969812629984,12.815133759565,39.522695031856));
#44709=CARTESIAN_POINT('Ctrl Pts',(18.6400319629903,12.8102384024566,39.4694732855197));
#44710=CARTESIAN_POINT('Ctrl Pts',(18.5990962053157,12.8066678079791,39.4275691225681));
#44711=CARTESIAN_POINT('Ctrl Pts',(18.4948705759095,12.7972261004701,39.3106785738321));
#44712=CARTESIAN_POINT('Ctrl Pts',(18.4352887521709,12.7914362519711,39.2326236449761));
#44713=CARTESIAN_POINT('Ctrl Pts',(18.3298943415409,12.7797563213007,39.0702639614246));
#44714=CARTESIAN_POINT('Ctrl Pts',(18.2839178012904,12.7738882745998,38.986410340952));
#44715=CARTESIAN_POINT('Ctrl Pts',(18.2387086279348,12.7669223864517,38.8871340580069));
#44716=CARTESIAN_POINT('Ctrl Pts',(18.2332062565997,12.7660501222301,38.8747045731856));
#44717=CARTESIAN_POINT('Ctrl Pts',(18.2245813657808,12.7646421657658,38.8546516249525));
#44718=CARTESIAN_POINT('Ctrl Pts',(18.2213754613741,12.7641092902842,38.8470643539315));
#44719=CARTESIAN_POINT('Ctrl Pts',(18.2157608452973,12.7631587319812,38.8335354781735));
#44720=CARTESIAN_POINT('Ctrl Pts',(18.2133329636354,12.7627417004449,38.8276019230526));
#44721=CARTESIAN_POINT('Ctrl Pts',(18.2083260997637,12.7618689743556,38.8151893596229));
#44722=CARTESIAN_POINT('Ctrl Pts',(18.2057525852766,12.7614131041079,38.8087082598088));
#44723=CARTESIAN_POINT('Ctrl Pts',(18.1991359997421,12.7602217067549,38.7917780987395));
#44724=CARTESIAN_POINT('Ctrl Pts',(18.1951487653516,12.7594843354415,38.7813076376802));
#44725=CARTESIAN_POINT('Ctrl Pts',(18.1779266227264,12.7562111336676,38.7348700279562));
#44726=CARTESIAN_POINT('Ctrl Pts',(18.1656748292056,12.7536432349123,38.6985500464781));
#44727=CARTESIAN_POINT('Ctrl Pts',(18.1354956329723,12.7466087250239,38.5994289321728));
#44728=CARTESIAN_POINT('Ctrl Pts',(18.1196630484594,12.742081010321,38.5360473017325));
#44729=CARTESIAN_POINT('Ctrl Pts',(18.0829226756844,12.728673977758,38.3490888010809));
#44730=CARTESIAN_POINT('Ctrl Pts',(18.0707990830953,12.7196304759924,38.2241384755919));
#44731=CARTESIAN_POINT('Ctrl Pts',(18.070870312024,12.710826110243,38.0989027900441));
#44732=CARTESIAN_POINT('Ctrl Pts',(18.0708703135747,12.7108259188098,38.0989000670461));
#44733=CARTESIAN_POINT('Ctrl Pts',(18.0709026179318,12.7068427740739,38.0422427098023));
#44734=CARTESIAN_POINT('Ctrl Pts',(18.0734309147293,12.7029187220878,37.9856069657395));
#44735=CARTESIAN_POINT('Ctrl Pts',(18.0789883844697,12.6987069164986,37.9230990867487));
#44736=CARTESIAN_POINT('Ctrl Pts',(18.0795557556661,12.6983000684806,37.9170424451146));
#44737=CARTESIAN_POINT('Ctrl Pts',(18.0805522371805,12.6976223674496,37.9069208747982));
#44738=CARTESIAN_POINT('Ctrl Pts',(18.0809656300099,12.6973506938101,37.9028544945266));
#44739=CARTESIAN_POINT('Ctrl Pts',(18.081742345095,12.6968570081796,37.8954482648573));
#44740=CARTESIAN_POINT('Ctrl Pts',(18.0821014724423,12.6966347689286,37.8921080055112));
#44741=CARTESIAN_POINT('Ctrl Pts',(18.0828591844516,12.6961780051474,37.8852295939745));
#44742=CARTESIAN_POINT('Ctrl Pts',(18.0832588334862,12.6959435519465,37.8816916518885));
#44743=CARTESIAN_POINT('Ctrl Pts',(18.0841909141036,12.695411083327,37.8736402033923));
#44744=CARTESIAN_POINT('Ctrl Pts',(18.0847295007692,12.6951134146856,37.8691274660265));
#44745=CARTESIAN_POINT('Ctrl Pts',(18.0861719981272,12.6943413367468,37.8573935335564));
#44746=CARTESIAN_POINT('Ctrl Pts',(18.0871008420414,12.6938682799795,37.8501753938117));
#44747=CARTESIAN_POINT('Ctrl Pts',(18.0933979240791,12.690809789562,37.8033356180808));
#44748=CARTESIAN_POINT('Ctrl Pts',(18.0999564567127,12.6882858144034,37.7638805295169));
#44749=CARTESIAN_POINT('Ctrl Pts',(18.1132876790424,12.6840327512664,37.6966726168074));
#44750=CARTESIAN_POINT('Ctrl Pts',(18.1194583621691,12.6822837523729,37.6688160082693));
#44751=CARTESIAN_POINT('Ctrl Pts',(18.1531427171125,12.6736727124743,37.5312762650907));
#44752=CARTESIAN_POINT('Ctrl Pts',(18.1896453070339,12.6670232320669,37.4240220826873));
#44753=CARTESIAN_POINT('Ctrl Pts',(18.2620148362235,12.6562241379459,37.2601719599779));
#44754=CARTESIAN_POINT('Ctrl Pts',(18.2917780902862,12.652195654333,37.2011783404125));
#44755=CARTESIAN_POINT('Ctrl Pts',(18.3436498845137,12.6456597181386,37.1102835110783));
#44756=CARTESIAN_POINT('Ctrl Pts',(18.363796244046,12.6432169203731,37.077321468207));
#44757=CARTESIAN_POINT('Ctrl Pts',(18.391061212038,12.6400171262155,37.0355824384427));
#44758=CARTESIAN_POINT('Ctrl Pts',(18.3972870732006,12.6392931221061,37.02623092131));
#44759=CARTESIAN_POINT('Ctrl Pts',(18.4075129713709,12.6381143429789,37.0111582565043));
#44760=CARTESIAN_POINT('Ctrl Pts',(18.4114630664718,12.6376614423418,37.0054034133859));
#44761=CARTESIAN_POINT('Ctrl Pts',(18.4190998393028,12.6367904247175,36.9944058995908));
#44762=CARTESIAN_POINT('Ctrl Pts',(18.4227815884265,12.6363724981213,36.9891599064275));
#44763=CARTESIAN_POINT('Ctrl Pts',(18.4312465609693,12.635416087076,36.9772253924588));
#44764=CARTESIAN_POINT('Ctrl Pts',(18.4360465188126,12.6348769690029,36.9705489488405));
#44765=CARTESIAN_POINT('Ctrl Pts',(18.4488660345377,12.6334454009973,36.9529562106468));
#44766=CARTESIAN_POINT('Ctrl Pts',(18.4569580172595,12.6325501765981,36.9420935024053));
#44767=CARTESIAN_POINT('Ctrl Pts',(18.5217824141114,12.6254428547722,36.8569593308747));
#44768=CARTESIAN_POINT('Ctrl Pts',(18.5837210048834,12.6190246081369,36.7868258367444));
#44769=CARTESIAN_POINT('Ctrl Pts',(18.7642969505792,12.6012676443994,36.6100517931978));
#44770=CARTESIAN_POINT('Ctrl Pts',(18.8914568175212,12.5896737559539,36.5131674388335));
#44771=CARTESIAN_POINT('Ctrl Pts',(19.0456515281141,12.5773851187491,36.4233576357675));
#44772=CARTESIAN_POINT('Ctrl Pts',(19.062373416056,12.5760745473963,36.41394926697));
#44773=CARTESIAN_POINT('Ctrl Pts',(19.087153945382,12.574167527684,36.4004895183066));
#44774=CARTESIAN_POINT('Ctrl Pts',(19.0951045652452,12.5735609118318,36.3962429585337));
#44775=CARTESIAN_POINT('Ctrl Pts',(19.1094789486094,12.5724739580307,36.3886943658217));
#44776=CARTESIAN_POINT('Ctrl Pts',(19.1158919938871,12.5719924936274,36.3853724153249));
#44777=CARTESIAN_POINT('Ctrl Pts',(19.125955120808,12.5712425913719,36.3802311970385));
#44778=CARTESIAN_POINT('Ctrl Pts',(19.1295924895831,12.5709726720597,36.3783873975091));
#44779=CARTESIAN_POINT('Ctrl Pts',(19.136413973045,12.5704686313622,36.3749566999036));
#44780=CARTESIAN_POINT('Ctrl Pts',(19.1395966020977,12.5702343486909,36.373367089859));
#44781=CARTESIAN_POINT('Ctrl Pts',(19.1468219535318,12.5697044507354,36.3697832223703));
#44782=CARTESIAN_POINT('Ctrl Pts',(19.1508672721363,12.5694091686982,36.3677943285923));
#44783=CARTESIAN_POINT('Ctrl Pts',(19.1631690343525,12.5685153396171,36.3617995782881));
#44784=CARTESIAN_POINT('Ctrl Pts',(19.1714472709191,12.5679194688469,36.3578383673378));
#44785=CARTESIAN_POINT('Ctrl Pts',(19.2494530179171,12.5623542043217,36.321193697273));
#44786=CARTESIAN_POINT('Ctrl Pts',(19.3210323635695,12.5576170286597,36.2926623636835));
#44787=CARTESIAN_POINT('Ctrl Pts',(19.394104060634,12.5529621656639,36.2684889660284));
#44788=CARTESIAN_POINT('Ctrl Pts',(19.3941040087481,12.3811612414289,36.2684889831931));
#44789=CARTESIAN_POINT('Ctrl Pts',(19.3894385614427,12.3814812915961,36.2700323950502));
#44790=CARTESIAN_POINT('Ctrl Pts',(19.3847790597086,12.3818019234793,36.2715936175433));
#44791=CARTESIAN_POINT('Ctrl Pts',(19.3723204967097,12.3826619093985,36.2758210252751));
#44792=CARTESIAN_POINT('Ctrl Pts',(19.3645325459949,12.383202315171,36.2785193929037));
#44793=CARTESIAN_POINT('Ctrl Pts',(19.3439298925368,12.3846395490855,36.285806008883));
#44794=CARTESIAN_POINT('Ctrl Pts',(19.3311462371627,12.3855391868955,36.2904800495199));
#44795=CARTESIAN_POINT('Ctrl Pts',(19.2282827106638,12.3928431038524,36.3293285953864));
#44796=CARTESIAN_POINT('Ctrl Pts',(19.1408430686202,12.3994670186418,36.3700667720709));
#44797=CARTESIAN_POINT('Ctrl Pts',(18.9730597772507,12.4129994089861,36.4641037847634));
#44798=CARTESIAN_POINT('Ctrl Pts',(18.8929217054918,12.4198877654547,36.5172369712706));
#44799=CARTESIAN_POINT('Ctrl Pts',(18.7555623280958,12.432249848792,36.6238625797878));
#44800=CARTESIAN_POINT('Ctrl Pts',(18.696988212218,12.437731368485,36.6753001297696));
#44801=CARTESIAN_POINT('Ctrl Pts',(18.6315663969375,12.4439710121969,36.7401710214812));
#44802=CARTESIAN_POINT('Ctrl Pts',(18.6215646358858,12.4449283571687,36.7503106456924));
#44803=CARTESIAN_POINT('Ctrl Pts',(18.607938726817,12.4462361940956,36.7644338515393));
#44804=CARTESIAN_POINT('Ctrl Pts',(18.6042178965868,12.4465937022498,36.7683229195028));
#44805=CARTESIAN_POINT('Ctrl Pts',(18.5979712220241,12.4471944603881,36.7749069827943));
#44806=CARTESIAN_POINT('Ctrl Pts',(18.5954367736909,12.4474383613948,36.7775937301403));
#44807=CARTESIAN_POINT('Ctrl Pts',(18.5906335855341,12.4479008638559,36.782714935962));
#44808=CARTESIAN_POINT('Ctrl Pts',(18.5883634114059,12.4481195778438,36.785148003643));
#44809=CARTESIAN_POINT('Ctrl Pts',(18.5824309088651,12.4486914764439,36.7915392599731));
#44810=CARTESIAN_POINT('Ctrl Pts',(18.5787788288706,12.4490438891074,36.79550698707));
#44811=CARTESIAN_POINT('Ctrl Pts',(18.5661812898456,12.4502609404076,36.8093090242261));
#44812=CARTESIAN_POINT('Ctrl Pts',(18.5573206360105,12.4511194965842,36.8192207196997));
#44813=CARTESIAN_POINT('Ctrl Pts',(18.4543801621525,12.4611351320356,36.9367957871383));
#44814=CARTESIAN_POINT('Ctrl Pts',(18.3724329171708,12.4695404467044,37.0545225461056));
#44815=CARTESIAN_POINT('Ctrl Pts',(18.2625909057656,12.4833197714927,37.257038087801));
#44816=CARTESIAN_POINT('Ctrl Pts',(18.2262052961051,12.4885794995811,37.3365698201978));
#44817=CARTESIAN_POINT('Ctrl Pts',(18.1845178086963,12.4959028971725,37.4469270980462));
#44818=CARTESIAN_POINT('Ctrl Pts',(18.1743830716012,12.4978217088382,37.4758185512877));
#44819=CARTESIAN_POINT('Ctrl Pts',(18.1581780124565,12.501151626343,37.5257918954755));
#44820=CARTESIAN_POINT('Ctrl Pts',(18.1517717770796,12.5025519740575,37.546759044586));
#44821=CARTESIAN_POINT('Ctrl Pts',(18.1432203360055,12.5045485009324,37.5765554117449));
#44822=CARTESIAN_POINT('Ctrl Pts',(18.1407778731173,12.5051350914937,37.5852981096874));
#44823=CARTESIAN_POINT('Ctrl Pts',(18.1366853734852,12.5061469017297,37.600356362579));
#44824=CARTESIAN_POINT('Ctrl Pts',(18.1350055058335,12.5065711551665,37.6066637082198));
#44825=CARTESIAN_POINT('Ctrl Pts',(18.1318592437799,12.5073831769145,37.6187226350318));
#44826=CARTESIAN_POINT('Ctrl Pts',(18.1303873184461,12.5077707623048,37.6244727066352));
#44827=CARTESIAN_POINT('Ctrl Pts',(18.1266458038984,12.5087762977336,37.6393748551344));
#44828=CARTESIAN_POINT('Ctrl Pts',(18.124416759365,12.5093955362011,37.6485368561473));
#44829=CARTESIAN_POINT('Ctrl Pts',(18.117113007349,12.5114949990487,37.6795453107317));
#44830=CARTESIAN_POINT('Ctrl Pts',(18.1123522957543,12.5129851355133,37.7014631187228));
#44831=CARTESIAN_POINT('Ctrl Pts',(18.0831797851786,12.5229959686526,37.8480474258763));
#44832=CARTESIAN_POINT('Ctrl Pts',(18.0707556558024,12.5318961291499,37.9747587684464));
#44833=CARTESIAN_POINT('Ctrl Pts',(18.0709900032668,12.550305627564,38.2332319793663));
#44834=CARTESIAN_POINT('Ctrl Pts',(18.0845508458415,12.5597741731661,38.3643680613534));
#44835=CARTESIAN_POINT('Ctrl Pts',(18.1142285855124,12.569639921465,38.5069502337397));
#44836=CARTESIAN_POINT('Ctrl Pts',(18.1172608135519,12.570590326765,38.5207558732588));
#44837=CARTESIAN_POINT('Ctrl Pts',(18.1216908215274,12.5719015529136,38.5399179443012));
#44838=CARTESIAN_POINT('Ctrl Pts',(18.1229602388603,12.5722691784662,38.5453031603507));
#44839=CARTESIAN_POINT('Ctrl Pts',(18.1250363658388,12.5728575645545,38.5539440231882));
#44840=CARTESIAN_POINT('Ctrl Pts',(18.1258284162553,12.573079145883,38.5572031066483));
#44841=CARTESIAN_POINT('Ctrl Pts',(18.1275042302377,12.5735419566209,38.5640211156387));
#44842=CARTESIAN_POINT('Ctrl Pts',(18.1283896463398,12.5737830849446,38.5675796059643));
#44843=CARTESIAN_POINT('Ctrl Pts',(18.1305671077183,12.5743679600476,38.5762255444833));
#44844=CARTESIAN_POINT('Ctrl Pts',(18.1318697928919,12.5747111020066,38.5813103352729));
#44845=CARTESIAN_POINT('Ctrl Pts',(18.1365637488479,12.5759241380805,38.599326149744));
#44846=CARTESIAN_POINT('Ctrl Pts',(18.1400687526548,12.5767877894335,38.6122275325809));
#44847=CARTESIAN_POINT('Ctrl Pts',(18.1623996749785,12.5820474968774,38.6911712786608));
#44848=CARTESIAN_POINT('Ctrl Pts',(18.184608914253,12.586273971855,38.7562131937333));
#44849=CARTESIAN_POINT('Ctrl Pts',(18.2620999292085,12.5988456686863,38.9488548275447));
#44850=CARTESIAN_POINT('Ctrl Pts',(18.3277326192903,12.606971159464,39.0717891010379));
#44851=CARTESIAN_POINT('Ctrl Pts',(18.443083646501,12.6195121011069,39.241002972756));
#44852=CARTESIAN_POINT('Ctrl Pts',(18.4829203654776,12.6236152388869,39.2934589538701));
#44853=CARTESIAN_POINT('Ctrl Pts',(18.5334425004029,12.6286263575041,39.3533590594835));
#44854=CARTESIAN_POINT('Ctrl Pts',(18.5416211679351,12.629431981433,39.3628661852549));
#44855=CARTESIAN_POINT('Ctrl Pts',(18.5551737834233,12.6307582906004,39.3783129127683));
#44856=CARTESIAN_POINT('Ctrl Pts',(18.5604931421139,12.6312767292056,39.3843000825241));
#44857=CARTESIAN_POINT('Ctrl Pts',(18.5701078089014,12.6322100947065,39.3949870324086));
#44858=CARTESIAN_POINT('Ctrl Pts',(18.5743894170783,12.6326244458917,39.3996990253569));
#44859=CARTESIAN_POINT('Ctrl Pts',(18.5835435983463,12.6335076509805,39.4096737213795));
#44860=CARTESIAN_POINT('Ctrl Pts',(18.5884223401308,12.6339767619553,39.414930607326));
#44861=CARTESIAN_POINT('Ctrl Pts',(18.6016123275189,12.6352408565748,39.4289849303291));
#44862=CARTESIAN_POINT('Ctrl Pts',(18.6099771246929,12.6360381197919,39.4377314463036));
#44863=CARTESIAN_POINT('Ctrl Pts',(18.6521413790621,12.6400357613395,39.4809973457759));
#44864=CARTESIAN_POINT('Ctrl Pts',(18.6871442238691,12.6432883316831,39.5143145122849));
#44865=CARTESIAN_POINT('Ctrl Pts',(18.7931847713054,12.6529641124202,39.6079172417125));
#44866=CARTESIAN_POINT('Ctrl Pts',(18.8673755819212,12.6595221357419,39.6644090409455));
#44867=CARTESIAN_POINT('Ctrl Pts',(19.0575521339271,12.6756921820771,39.7885767865864));
#44868=CARTESIAN_POINT('Ctrl Pts',(19.1770930177662,12.6853512204797,39.849951212422));
#44869=CARTESIAN_POINT('Ctrl Pts',(19.315133925163,12.695380620995,39.9035238691594));
#44870=CARTESIAN_POINT('Ctrl Pts',(19.3282853061669,12.6963251378596,39.9084632385829));
#44871=CARTESIAN_POINT('Ctrl Pts',(19.3466771286605,12.6976296220969,39.9151424843372));
#44872=CARTESIAN_POINT('Ctrl Pts',(19.3518724675394,12.6979963046104,39.917004049577));
#44873=CARTESIAN_POINT('Ctrl Pts',(19.3602354577664,12.6985835725821,39.919960196882));
#44874=CARTESIAN_POINT('Ctrl Pts',(19.3633980489312,12.6988049731445,39.9210688466003));
#44875=CARTESIAN_POINT('Ctrl Pts',(19.3700295089851,12.6992677607782,39.9233741256175));
#44876=CARTESIAN_POINT('Ctrl Pts',(19.3734989222998,12.6995090453215,39.9245691057));
#44877=CARTESIAN_POINT('Ctrl Pts',(19.3819513049755,12.7000948944786,39.9274534333073));
#44878=CARTESIAN_POINT('Ctrl Pts',(19.3869378651887,12.7004388494064,39.92913232457));
#44879=CARTESIAN_POINT('Ctrl Pts',(19.4046946583734,12.7016579197617,39.935029967261));
#44880=CARTESIAN_POINT('Ctrl Pts',(19.4175024266653,12.7025267098489,39.9391356752712));
#44881=CARTESIAN_POINT('Ctrl Pts',(19.5857165784426,12.713812890742,39.9911254707784));
#44882=CARTESIAN_POINT('Ctrl Pts',(19.7465542659121,12.7232610610126,40.0193147913548));
#44883=CARTESIAN_POINT('Ctrl Pts',(20.0173762349158,12.7395474937246,40.0320980399145));
#44884=CARTESIAN_POINT('Ctrl Pts',(20.1259323487551,12.7461684534555,40.0280666368807));
#44885=CARTESIAN_POINT('Ctrl Pts',(20.2472870897022,12.7539728685391,40.0132649373908));
#44886=CARTESIAN_POINT('Ctrl Pts',(20.2609894771528,12.7548596849453,40.0114439835572));
#44887=CARTESIAN_POINT('Ctrl Pts',(20.2828903948863,12.7562866140849,40.0082936201062));
#44888=CARTESIAN_POINT('Ctrl Pts',(20.2911021291783,12.7568237856814,40.0070582222107));
#44889=CARTESIAN_POINT('Ctrl Pts',(20.3056488766126,12.7577792794614,40.004773622166));
#44890=CARTESIAN_POINT('Ctrl Pts',(20.3119871479582,12.758196926578,40.003745730218));
#44891=CARTESIAN_POINT('Ctrl Pts',(20.3251669424736,12.7590681875109,40.0015407457398));
#44892=CARTESIAN_POINT('Ctrl Pts',(20.3320074694585,12.759521963393,40.0003583310249));
#44893=CARTESIAN_POINT('Ctrl Pts',(20.3497310993728,12.7607018543041,39.9971961089283));
#44894=CARTESIAN_POINT('Ctrl Pts',(20.3606036985184,12.7614297479509,39.9951595926481));
#44895=CARTESIAN_POINT('Ctrl Pts',(20.4077197198617,12.7646022452176,39.9859142952311));
#44896=CARTESIAN_POINT('Ctrl Pts',(20.4437672277241,12.7670765329702,39.9777588845758));
#44897=CARTESIAN_POINT('Ctrl Pts',(20.5395577538856,12.7737832951403,39.9531749205135));
#44898=CARTESIAN_POINT('Ctrl Pts',(20.5987770524872,12.7780700377408,39.93489634623));
#44899=CARTESIAN_POINT('Ctrl Pts',(20.7833496792119,12.7918543893037,39.8680389985579));
#44900=CARTESIAN_POINT('Ctrl Pts',(20.9045535782705,12.8015733017003,39.8092040961798));
#44901=CARTESIAN_POINT('Ctrl Pts',(21.0631221448746,12.8146714398749,39.7106071693668));
#44902=CARTESIAN_POINT('Ctrl Pts',(21.1064481018816,12.8182901088628,39.6811571253871));
#44903=CARTESIAN_POINT('Ctrl Pts',(21.1554266306209,12.8223823792018,39.6448642739442));
#44904=CARTESIAN_POINT('Ctrl Pts',(21.1622932821645,12.8229561268215,39.6397047303394));
#44905=CARTESIAN_POINT('Ctrl Pts',(21.1726614715716,12.8238221971327,39.6318052722251));
#44906=CARTESIAN_POINT('Ctrl Pts',(21.1761882635435,12.8241167508104,39.6290989139398));
#44907=CARTESIAN_POINT('Ctrl Pts',(21.182517419016,12.8246452269678,39.6242072492631));
#44908=CARTESIAN_POINT('Ctrl Pts',(21.1853231118073,12.8248794498153,39.6220263815832));
#44909=CARTESIAN_POINT('Ctrl Pts',(21.1914396551959,12.8253899574658,39.6172448152299));
#44910=CARTESIAN_POINT('Ctrl Pts',(21.1947480157991,12.8256660204348,39.6146410336762));
#44911=CARTESIAN_POINT('Ctrl Pts',(21.2041151416654,12.8264475542174,39.6072190302928));
#44912=CARTESIAN_POINT('Ctrl Pts',(21.2101535524101,12.8269512452004,39.6023750744001));
#44913=CARTESIAN_POINT('Ctrl Pts',(21.2485852930034,12.8301574626768,39.5711634456018));
#44914=CARTESIAN_POINT('Ctrl Pts',(21.2801469785742,12.8327926657436,39.5437837223654));
#44915=CARTESIAN_POINT('Ctrl Pts',(21.3859893354915,12.8417379764338,39.4457633541241));
#44916=CARTESIAN_POINT('Ctrl Pts',(21.4555188571318,12.847814938025,39.370241575832));
#44917=CARTESIAN_POINT('Ctrl Pts',(21.6022832578745,12.8620374247799,39.1828640958038));
#44918=CARTESIAN_POINT('Ctrl Pts',(21.6743581448781,12.8701994281383,39.0676899569763));
#44919=CARTESIAN_POINT('Ctrl Pts',(21.7397841383618,12.8797255810793,38.933595757464));
#44920=CARTESIAN_POINT('Ctrl Pts',(21.7456675998606,12.8806057547467,38.9212035984987));
#44921=CARTESIAN_POINT('Ctrl Pts',(21.7548867655927,12.8820240255675,38.9012386953374));
#44922=CARTESIAN_POINT('Ctrl Pts',(21.7583068480036,12.8825592386653,38.8937052549385));
#44923=CARTESIAN_POINT('Ctrl Pts',(21.7642931343387,12.8835124784087,38.8802906280256));
#44924=CARTESIAN_POINT('Ctrl Pts',(21.7668786698948,12.8839298408367,38.8744181637039));
#44925=CARTESIAN_POINT('Ctrl Pts',(21.7722060169351,12.8848017505141,38.8621527257608));
#44926=CARTESIAN_POINT('Ctrl Pts',(21.7749426392276,12.8852564659792,38.8557576127109));
#44927=CARTESIAN_POINT('Ctrl Pts',(21.7819661760717,12.8864415223991,38.839095989857));
#44928=CARTESIAN_POINT('Ctrl Pts',(21.7861989219825,12.8871736713122,38.8288070644789));
#44929=CARTESIAN_POINT('Ctrl Pts',(21.8043322603752,12.8903909790854,38.7836216998618));
#44930=CARTESIAN_POINT('Ctrl Pts',(21.8173001062669,12.8929068707238,38.7483621861104));
#44931=CARTESIAN_POINT('Ctrl Pts',(21.8493745770503,12.8997584565884,38.6526107214742));
#44932=CARTESIAN_POINT('Ctrl Pts',(21.8665395683111,12.9041513811197,38.5915217137517));
#44933=CARTESIAN_POINT('Ctrl Pts',(21.9096358826708,12.9177498686682,38.402903985855));
#44934=CARTESIAN_POINT('Ctrl Pts',(21.925708350767,12.927149540771,38.2735078487818));
#44935=CARTESIAN_POINT('Ctrl Pts',(21.9298642738757,12.9400979826412,38.0891762989428));
#44936=CARTESIAN_POINT('Ctrl Pts',(21.9287944882263,12.9438564142326,38.0348362869205));
#44937=CARTESIAN_POINT('Ctrl Pts',(21.9248958727853,12.9480858454839,37.9719630035297));
#44938=CARTESIAN_POINT('Ctrl Pts',(21.9243015311271,12.9486645697535,37.9633207486838));
#44939=CARTESIAN_POINT('Ctrl Pts',(21.9233129197937,12.9495366382826,37.9502339393603));
#44940=CARTESIAN_POINT('Ctrl Pts',(21.9229614217371,12.9498322591349,37.9457864082832));
#44941=CARTESIAN_POINT('Ctrl Pts',(21.9223021584115,12.9503618640069,37.937797648107));
#44942=CARTESIAN_POINT('Ctrl Pts',(21.9220000335551,12.9505961543609,37.9342560322098));
#44943=CARTESIAN_POINT('Ctrl Pts',(21.9213197985246,12.9511058981754,37.9265341375067));
#44944=CARTESIAN_POINT('Ctrl Pts',(21.9209378350196,12.9513811347682,37.9223542613179));
#44945=CARTESIAN_POINT('Ctrl Pts',(21.9198182318219,12.9521579846264,37.9105283160174));
#44946=CARTESIAN_POINT('Ctrl Pts',(21.9190485515986,12.9526578516448,37.9028852524798));
#44947=CARTESIAN_POINT('Ctrl Pts',(21.9139261232015,12.9557837028355,37.8548957020745));
#44948=CARTESIAN_POINT('Ctrl Pts',(21.9083465067761,12.9583461971388,37.8146870280596));
#44949=CARTESIAN_POINT('Ctrl Pts',(21.8665713713731,12.9737242171507,37.5705097206401));
#44950=CARTESIAN_POINT('Ctrl Pts',(21.7989877623501,12.9855081415591,37.3732891954765));
#44951=CARTESIAN_POINT('Ctrl Pts',(21.6831026738316,13.0008510152839,37.1564951841658));
#44952=CARTESIAN_POINT('Ctrl Pts',(21.6638661860848,13.0032934489121,37.1229713716697));
#44953=CARTESIAN_POINT('Ctrl Pts',(21.6375138706213,13.0065219768893,37.0800844765128));
#44954=CARTESIAN_POINT('Ctrl Pts',(21.6313003609931,13.0072753454439,37.070175513025));
#44955=CARTESIAN_POINT('Ctrl Pts',(21.6211804342089,13.0084901952066,37.0543582290642));
#44956=CARTESIAN_POINT('Ctrl Pts',(21.6173308484455,13.0089495818076,37.0484137515919));
#44957=CARTESIAN_POINT('Ctrl Pts',(21.6099495448155,13.0098253297987,37.0371520500439));
#44958=CARTESIAN_POINT('Ctrl Pts',(21.6064239906753,13.0102414581594,37.031830883182));
#44959=CARTESIAN_POINT('Ctrl Pts',(21.5983307158113,13.0111918987519,37.019746285706));
#44960=CARTESIAN_POINT('Ctrl Pts',(21.5937463776876,13.0117268283385,37.0129941837723));
#44961=CARTESIAN_POINT('Ctrl Pts',(21.579580719837,13.0133694814656,36.9924123659104));
#44962=CARTESIAN_POINT('Ctrl Pts',(21.5698614195101,13.0144823951787,36.978679033073));
#44963=CARTESIAN_POINT('Ctrl Pts',(21.5471102082805,13.0170563267166,36.9474073028732));
#44964=CARTESIAN_POINT('Ctrl Pts',(21.5339576680707,13.0185218493343,36.9299599455592));
#44965=CARTESIAN_POINT('Ctrl Pts',(21.4882474111427,13.0235416538979,36.8714192583834));
#44966=CARTESIAN_POINT('Ctrl Pts',(21.4543144208415,13.0271471592378,36.831433982806));
#44967=CARTESIAN_POINT('Ctrl Pts',(21.3202457637964,13.0409466648584,36.6859104386596));
#44968=CARTESIAN_POINT('Ctrl Pts',(21.2099237570059,13.0514763907563,36.5904382149351));
#44969=CARTESIAN_POINT('Ctrl Pts',(21.0752167925078,13.0629507230472,36.4981980845933));
#44970=CARTESIAN_POINT('Ctrl Pts',(21.0603644449194,13.0641981109907,36.4883276372919));
#44971=CARTESIAN_POINT('Ctrl Pts',(21.0124534846761,13.0681611002534,36.4574364310749));
#44972=CARTESIAN_POINT('Ctrl Pts',(20.9788881743543,13.0708465518793,36.4372145087747));
#44973=CARTESIAN_POINT('Ctrl Pts',(20.9384209019949,13.0739583972686,36.4144849181742));
#44974=CARTESIAN_POINT('Ctrl Pts',(20.9320941546162,13.0744413489899,36.4109779837634));
#44975=CARTESIAN_POINT('Ctrl Pts',(20.9217721718468,13.0752233190207,36.4053321406502));
#44976=CARTESIAN_POINT('Ctrl Pts',(20.9177889335841,13.075523647175,36.4031716160037));
#44977=CARTESIAN_POINT('Ctrl Pts',(20.9106633770325,13.0760582962267,36.3993391168336));
#44978=CARTESIAN_POINT('Ctrl Pts',(20.907524018441,13.0762929496728,36.3976617896364));
#44979=CARTESIAN_POINT('Ctrl Pts',(20.9007192750668,13.076799620928,36.3940502587445));
#44980=CARTESIAN_POINT('Ctrl Pts',(20.8970523027785,13.0770714426467,36.3921191789105));
#44981=CARTESIAN_POINT('Ctrl Pts',(20.8867874006271,13.0778290378445,36.386755716232));
#44982=CARTESIAN_POINT('Ctrl Pts',(20.8801757150774,13.078313200024,36.3833496032255));
#44983=CARTESIAN_POINT('Ctrl Pts',(20.8413226403807,13.0811370611157,36.3636173216586));
#44984=CARTESIAN_POINT('Ctrl Pts',(20.8086448915068,13.0834266195273,36.348160270803));
#44985=CARTESIAN_POINT('Ctrl Pts',(20.6992023602477,13.0908783770015,36.300108000189));
#44986=CARTESIAN_POINT('Ctrl Pts',(20.6207553576899,13.0958784896369,36.2715689059064));
#44987=CARTESIAN_POINT('Ctrl Pts',(20.3965826012643,13.1098365678575,36.2061135275885));
#44988=CARTESIAN_POINT('Ctrl Pts',(20.2480627250366,13.1187514936008,36.1810048645534));
#44989=CARTESIAN_POINT('Ctrl Pts',(20.0762789190967,13.1296494133157,36.1722543560187));
#44990=CARTESIAN_POINT('Ctrl Pts',(20.0544003542533,13.1310470346824,36.1715129554781));
#44991=CARTESIAN_POINT('Ctrl Pts',(20.0241100082486,13.1329972752595,36.1710023531467));
#44992=CARTESIAN_POINT('Ctrl Pts',(20.0157046954574,13.1335400731801,36.1709156127982));
#44993=CARTESIAN_POINT('Ctrl Pts',(20.001244769397,13.1344767697442,36.1708609008153));
#44994=CARTESIAN_POINT('Ctrl Pts',(19.995190330847,13.1348698446403,36.1708664952495));
#44995=CARTESIAN_POINT('Ctrl Pts',(19.9826955951752,13.1356828985425,36.1709368606554));
#44996=CARTESIAN_POINT('Ctrl Pts',(19.9762554030158,13.136102988948,36.171005383513));
#44997=CARTESIAN_POINT('Ctrl Pts',(19.9612417095771,13.1370847497069,36.171240325024));
#44998=CARTESIAN_POINT('Ctrl Pts',(19.9526687885613,13.1376471863161,36.1714316601912));
#44999=CARTESIAN_POINT('Ctrl Pts',(19.9250852006237,13.1394629379899,36.1722313150435));
#45000=CARTESIAN_POINT('Ctrl Pts',(19.9060826501282,13.1407231612337,36.1730636187345));
#45001=CARTESIAN_POINT('Ctrl Pts',(19.8095132781625,13.1471770872879,36.1787251254538));
#45002=CARTESIAN_POINT('Ctrl Pts',(19.7322862382402,13.152505474303,36.1879568699085));
#45003=CARTESIAN_POINT('Ctrl Pts',(19.5731407572556,13.1638224954935,36.2168120686515));
#45004=CARTESIAN_POINT('Ctrl Pts',(19.491519858161,13.1698182844823,36.2371924624697));
#45005=CARTESIAN_POINT('Ctrl Pts',(19.4056874079929,13.1762486944391,36.2646874199425));
#45006=CARTESIAN_POINT('Ctrl Pts',(19.3998909291043,13.1766835529467,36.2665745683422));
#45007=CARTESIAN_POINT('Ctrl Pts',(19.3941040017606,13.1771182491666,36.2684889855047));
#45008=CARTESIAN_POINT('Origin',(20.,-1.3495818343519,38.1));
#45009=CARTESIAN_POINT('',(19.3941040087558,14.1433118141013,36.2684889831906));
#45010=CARTESIAN_POINT('',(19.3941039465104,13.9716756753762,36.2684890037825));
#45011=CARTESIAN_POINT('',(19.3941040087494,-1.3495818343519,36.2684889831927));
#45012=CARTESIAN_POINT('Ctrl Pts',(19.3941040087558,14.1433118141013,36.2684889831906));
#45013=CARTESIAN_POINT('Ctrl Pts',(19.3976160935084,14.1430688068057,36.2673271239099));
#45014=CARTESIAN_POINT('Ctrl Pts',(19.4011315012555,14.1428254683569,36.2661753730009));
#45015=CARTESIAN_POINT('Ctrl Pts',(19.4244732636406,14.1412090431187,36.2586022016742));
#45016=CARTESIAN_POINT('Ctrl Pts',(19.4443985677122,14.1398258608876,36.2524925259179));
#45017=CARTESIAN_POINT('Ctrl Pts',(19.6252695505569,14.1272354607431,36.2002227601991));
#45018=CARTESIAN_POINT('Ctrl Pts',(19.7914583679699,14.1153272214476,36.1748860704946));
#45019=CARTESIAN_POINT('Ctrl Pts',(20.0299828443551,14.0983175489016,36.1697888308123));
#45020=CARTESIAN_POINT('Ctrl Pts',(20.1012163382998,14.0932624730263,36.1722109059716));
#45021=CARTESIAN_POINT('Ctrl Pts',(20.2045896030247,14.0860881045754,36.181472969214));
#45022=CARTESIAN_POINT('Ctrl Pts',(20.2369458372837,14.083866151986,36.1851997880184));
#45023=CARTESIAN_POINT('Ctrl Pts',(20.2765252366262,14.0811893805295,36.190777341895));
#45024=CARTESIAN_POINT('Ctrl Pts',(20.2838501740516,14.0806957358182,36.1918526137187));
#45025=CARTESIAN_POINT('Ctrl Pts',(20.2952841830029,14.0799280868499,36.1935983794985));
#45026=CARTESIAN_POINT('Ctrl Pts',(20.2993974853126,14.0796525212811,36.1942400376794));
#45027=CARTESIAN_POINT('Ctrl Pts',(20.3070218471814,14.079142872763,36.1954547005856));
#45028=CARTESIAN_POINT('Ctrl Pts',(20.3105333690153,14.0789085981258,36.1960240969901));
#45029=CARTESIAN_POINT('Ctrl Pts',(20.3184891109961,14.0783788320141,36.1973367230223));
#45030=CARTESIAN_POINT('Ctrl Pts',(20.3229323063404,14.0780836730877,36.1980858100528));
#45031=CARTESIAN_POINT('Ctrl Pts',(20.3364071948248,14.0771905868003,36.2004061500026));
#45032=CARTESIAN_POINT('Ctrl Pts',(20.3454305106529,14.076595329195,36.2020262472717));
#45033=CARTESIAN_POINT('Ctrl Pts',(20.4619723023775,14.0689392873396,36.2238094857254));
#45034=CARTESIAN_POINT('Ctrl Pts',(20.5676157177188,14.0623470837316,36.2530216340581));
#45035=CARTESIAN_POINT('Ctrl Pts',(20.7485112528232,14.0508043559172,36.3200439956306));
#45036=CARTESIAN_POINT('Ctrl Pts',(20.8248305511398,14.0458478009006,36.3541000587445));
#45037=CARTESIAN_POINT('Ctrl Pts',(20.9681151109353,14.0360335254723,36.4295361639827));
#45038=CARTESIAN_POINT('Ctrl Pts',(21.035227516728,14.0311972764296,36.4702766661915));
#45039=CARTESIAN_POINT('Ctrl Pts',(21.1153741593196,14.0249963414926,36.5258817016223));
#45040=CARTESIAN_POINT('Ctrl Pts',(21.130916007199,14.0237729547481,36.5370102765727));
#45041=CARTESIAN_POINT('Ctrl Pts',(21.1532003677679,14.0219869013892,36.5534731508901));
#45042=CARTESIAN_POINT('Ctrl Pts',(21.1600769619241,14.021431257288,36.5586246979634));
#45043=CARTESIAN_POINT('Ctrl Pts',(21.1720496595552,14.0204558095169,36.5677194550205));
#45044=CARTESIAN_POINT('Ctrl Pts',(21.1771608858139,14.0200367915553,36.5716426071693));
#45045=CARTESIAN_POINT('Ctrl Pts',(21.1870327449106,14.0192224012284,36.5792987087563));
#45046=CARTESIAN_POINT('Ctrl Pts',(21.1917956665112,14.0188271525539,36.5830285953364));
#45047=CARTESIAN_POINT('Ctrl Pts',(21.2031198990285,14.0178817996629,36.5919829540234));
#45048=CARTESIAN_POINT('Ctrl Pts',(21.2096647926734,14.0173308869573,36.5972278988443));
#45049=CARTESIAN_POINT('Ctrl Pts',(21.2330758015869,14.0153437010099,36.6162410399895));
#45050=CARTESIAN_POINT('Ctrl Pts',(21.2497422252132,14.01389775736,36.6302514198873));
#45051=CARTESIAN_POINT('Ctrl Pts',(21.3811355477787,14.0022403833949,36.7445561670811));
#45052=CARTESIAN_POINT('Ctrl Pts',(21.4838267992947,13.991462126117,36.8578230281235));
#45053=CARTESIAN_POINT('Ctrl Pts',(21.619498044531,13.9747577900388,37.0485938896644));
#45054=CARTESIAN_POINT('Ctrl Pts',(21.662606269588,13.9689268555469,37.1181798581264));
#45055=CARTESIAN_POINT('Ctrl Pts',(21.7180230246129,13.9607839693108,37.2218105774161));
#45056=CARTESIAN_POINT('Ctrl Pts',(21.7339981539065,13.9583411301057,37.2537904646497));
#45057=CARTESIAN_POINT('Ctrl Pts',(21.7522039706805,13.9554511970229,37.2929196073081));
#45058=CARTESIAN_POINT('Ctrl Pts',(21.7552925920212,13.9549569224629,37.2996591751505));
#45059=CARTESIAN_POINT('Ctrl Pts',(21.7600450457539,13.9541902656215,37.3101891833869));
#45060=CARTESIAN_POINT('Ctrl Pts',(21.761735618768,13.9539163062687,37.3139673674167));
#45061=CARTESIAN_POINT('Ctrl Pts',(21.7648575868329,13.9534081053938,37.3210051806488));
#45062=CARTESIAN_POINT('Ctrl Pts',(21.7662921059007,13.9531736817022,37.3242633002542));
#45063=CARTESIAN_POINT('Ctrl Pts',(21.7695350504108,13.9526416316915,37.3316843994367));
#45064=CARTESIAN_POINT('Ctrl Pts',(21.77133780582,13.9523443499583,37.3358497952535));
#45065=CARTESIAN_POINT('Ctrl Pts',(21.7768025517078,13.951438408351,37.3485997390255));
#45066=CARTESIAN_POINT('Ctrl Pts',(21.7804170278818,13.950832532164,37.3572046881782));
#45067=CARTESIAN_POINT('Ctrl Pts',(21.8148224506742,13.9449964094858,37.4408075151127));
#45068=CARTESIAN_POINT('Ctrl Pts',(21.8409234212904,13.9400212580426,37.5176601423191));
#45069=CARTESIAN_POINT('Ctrl Pts',(21.9049342675449,13.9252348430738,37.7541292447737));
#45070=CARTESIAN_POINT('Ctrl Pts',(21.9274222354392,13.9156757004248,37.9171232414008));
#45071=CARTESIAN_POINT('Ctrl Pts',(21.929423274001,13.9029944418731,38.120273014458));
#45072=CARTESIAN_POINT('Ctrl Pts',(21.9286106211337,13.9005113279489,38.1595474469649));
#45073=CARTESIAN_POINT('Ctrl Pts',(21.9260214645185,13.8972658657942,38.2100525210719));
#45074=CARTESIAN_POINT('Ctrl Pts',(21.9253438161285,13.8965377090272,38.2213318591557));
#45075=CARTESIAN_POINT('Ctrl Pts',(21.9240863394978,13.8953538308932,38.2395823709361));
#45076=CARTESIAN_POINT('Ctrl Pts',(21.9235676096224,13.8949000144599,38.2465575968564));
#45077=CARTESIAN_POINT('Ctrl Pts',(21.9225012326045,13.8940283646176,38.2599143202236));
#45078=CARTESIAN_POINT('Ctrl Pts',(21.9219597142393,13.8936107277599,38.2662962247473));
#45079=CARTESIAN_POINT('Ctrl Pts',(21.9206530422187,13.8926565514477,38.2808357831492));
#45080=CARTESIAN_POINT('Ctrl Pts',(21.9198676820002,13.8921193886916,38.2889914526473));
#45081=CARTESIAN_POINT('Ctrl Pts',(21.9176563734879,13.8906964061911,38.3105169179353));
#45082=CARTESIAN_POINT('Ctrl Pts',(21.9161425817499,13.8898078648995,38.3238770431184));
#45083=CARTESIAN_POINT('Ctrl Pts',(21.9034900731792,13.8829745426769,38.4259894071141));
#45084=CARTESIAN_POINT('Ctrl Pts',(21.8863320196529,13.8768416051837,38.5138730038096));
#45085=CARTESIAN_POINT('Ctrl Pts',(21.8211460277485,13.8592091140062,38.7566586608354));
#45086=CARTESIAN_POINT('Ctrl Pts',(21.7596220350663,13.8474123461747,38.9071557708579));
#45087=CARTESIAN_POINT('Ctrl Pts',(21.665192058352,13.8341652053685,39.0744682109062));
#45088=CARTESIAN_POINT('Ctrl Pts',(21.6497468646515,13.832110666802,39.1003941313301));
#45089=CARTESIAN_POINT('Ctrl Pts',(21.6299525628263,13.8296202482447,39.1319141535314));
#45090=CARTESIAN_POINT('Ctrl Pts',(21.62617361565,13.8291508679072,39.1378591199517));
#45091=CARTESIAN_POINT('Ctrl Pts',(21.6201664356084,13.8284143657695,39.1471961353276));
#45092=CARTESIAN_POINT('Ctrl Pts',(21.6179599648291,13.828145858025,39.1506020073663));
#45093=CARTESIAN_POINT('Ctrl Pts',(21.6137909162434,13.8276423278268,39.1569929979081));
#45094=CARTESIAN_POINT('Ctrl Pts',(21.6118308168242,13.827407156092,39.1599795928037));
#45095=CARTESIAN_POINT('Ctrl Pts',(21.6073354661182,13.8268713419989,39.1667878363475));
#45096=CARTESIAN_POINT('Ctrl Pts',(21.6047948776525,13.8265710588392,39.1706058986159));
#45097=CARTESIAN_POINT('Ctrl Pts',(21.5980193327871,13.8257768188965,39.1807100524044));
#45098=CARTESIAN_POINT('Ctrl Pts',(21.59376085241,13.8252843835983,39.1869803840118));
#45099=CARTESIAN_POINT('Ctrl Pts',(21.5635419317525,13.8218358216206,39.2309163575541));
#45100=CARTESIAN_POINT('Ctrl Pts',(21.5362835463843,13.8189603373178,39.2676766743053));
#45101=CARTESIAN_POINT('Ctrl Pts',(21.4892080064309,13.8143005540875,39.3266559071788));
#45102=CARTESIAN_POINT('Ctrl Pts',(21.4701400281522,13.8124878749912,39.3494453277702));
#45103=CARTESIAN_POINT('Ctrl Pts',(21.3409390494567,13.8006189396445,39.4968072400247));
#45104=CARTESIAN_POINT('Ctrl Pts',(21.2156288217498,13.7909500406133,39.607128204402));
#45105=CARTESIAN_POINT('Ctrl Pts',(21.0418509349754,13.7779119308769,39.7241797440317));
#45106=CARTESIAN_POINT('Ctrl Pts',(21.0051785159135,13.775183260718,39.7471274742549));
#45107=CARTESIAN_POINT('Ctrl Pts',(20.9576682450241,13.7716605572902,39.7746791927508));
#45108=CARTESIAN_POINT('Ctrl Pts',(20.9475157037163,13.7709085097926,39.7804442411589));
#45109=CARTESIAN_POINT('Ctrl Pts',(20.9311256542882,13.7696952825597,39.7895554635599));
#45110=CARTESIAN_POINT('Ctrl Pts',(20.9249208641306,13.7692361873095,39.7929601417061));
#45111=CARTESIAN_POINT('Ctrl Pts',(20.9130837988498,13.7683606622248,39.7993708514347));
#45112=CARTESIAN_POINT('Ctrl Pts',(20.9074550506823,13.7679444635435,39.8023832247121));
#45113=CARTESIAN_POINT('Ctrl Pts',(20.8945893904619,13.7669933972063,39.8091866849455));
#45114=CARTESIAN_POINT('Ctrl Pts',(20.8873431790587,13.7664579092037,39.8129598304228));
#45115=CARTESIAN_POINT('Ctrl Pts',(20.8684419560345,13.7650614596873,39.8226496946919));
#45116=CARTESIAN_POINT('Ctrl Pts',(20.8567505475633,13.7641980057753,39.8284941095206));
#45117=CARTESIAN_POINT('Ctrl Pts',(20.7760919478953,13.7582422830106,39.8677951336482));
#45118=CARTESIAN_POINT('Ctrl Pts',(20.7052521195398,13.7530134473972,39.8972298401828));
#45119=CARTESIAN_POINT('Ctrl Pts',(20.475157394538,13.7360379959209,39.9771351487719));
#45120=CARTESIAN_POINT('Ctrl Pts',(20.311035843168,13.7238766857764,40.0111933586574));
#45121=CARTESIAN_POINT('Ctrl Pts',(20.1068790790113,13.7096664930776,40.0265382302504));
#45122=CARTESIAN_POINT('Ctrl Pts',(20.0690899643947,13.7070780253914,40.0282633986948));
#45123=CARTESIAN_POINT('Ctrl Pts',(20.0237388025867,13.7040400240934,40.0289986482153));
#45124=CARTESIAN_POINT('Ctrl Pts',(20.0162051534916,13.7035376244872,40.0290766478204));
#45125=CARTESIAN_POINT('Ctrl Pts',(20.0045058264873,13.7027611452615,40.0291292347054));
#45126=CARTESIAN_POINT('Ctrl Pts',(20.0003404646575,13.7024854239596,40.0291344669476));
#45127=CARTESIAN_POINT('Ctrl Pts',(19.9926178768566,13.7019756335411,40.0291191551665));
#45128=CARTESIAN_POINT('Ctrl Pts',(19.9890607546178,13.7017413718175,40.0291022637049));
#45129=CARTESIAN_POINT('Ctrl Pts',(19.9810010089807,13.7012118201667,40.0290416972593));
#45130=CARTESIAN_POINT('Ctrl Pts',(19.9764984878256,13.7009168616498,40.0289920972794));
#45131=CARTESIAN_POINT('Ctrl Pts',(19.9628453795154,13.7000249838259,40.0287938834603));
#45132=CARTESIAN_POINT('Ctrl Pts',(19.9536954758066,13.6994307236876,40.0285959166591));
#45133=CARTESIAN_POINT('Ctrl Pts',(19.8346460323971,13.6917396764961,40.0251724227426));
#45134=CARTESIAN_POINT('Ctrl Pts',(19.7251981713305,13.6851163589902,40.0126218327514));
#45135=CARTESIAN_POINT('Ctrl Pts',(19.5347554325774,13.6734915660326,39.9740864936778));
#45136=CARTESIAN_POINT('Ctrl Pts',(19.4532950810222,13.668485206967,39.9519627307868));
#45137=CARTESIAN_POINT('Ctrl Pts',(19.300434521341,13.6586837507401,39.8994793924129));
#45138=CARTESIAN_POINT('Ctrl Pts',(19.2289057456295,13.6539150639549,39.8700083417161));
#45139=CARTESIAN_POINT('Ctrl Pts',(19.1422715753804,13.6477953524673,39.8280637265226));
#45140=CARTESIAN_POINT('Ctrl Pts',(19.125323753237,13.6465813110532,39.8195475323259));
#45141=CARTESIAN_POINT('Ctrl Pts',(19.1009088277112,13.6448064414409,39.8068248258356));
#45142=CARTESIAN_POINT('Ctrl Pts',(19.0933394854519,13.6442525112324,39.8028160880288));
#45143=CARTESIAN_POINT('Ctrl Pts',(19.0801270563051,13.6432790486247,39.795705689688));
#45144=CARTESIAN_POINT('Ctrl Pts',(19.0744722944561,13.6428602921241,39.7926259135379));
#45145=CARTESIAN_POINT('Ctrl Pts',(19.0635281858917,13.6420456522766,39.7865941387933));
#45146=CARTESIAN_POINT('Ctrl Pts',(19.0582371093959,13.641649889068,39.7836454211349));
#45147=CARTESIAN_POINT('Ctrl Pts',(19.0456275562015,13.6407020836127,39.7765400778502));
#45148=CARTESIAN_POINT('Ctrl Pts',(19.0383222721577,13.6401492232894,39.7723604091534));
#45149=CARTESIAN_POINT('Ctrl Pts',(19.0120565621523,13.6381476851336,39.7571036533601));
#45150=CARTESIAN_POINT('Ctrl Pts',(18.9932588554332,13.6366891534786,39.7457511825473));
#45151=CARTESIAN_POINT('Ctrl Pts',(18.8480624751101,13.6252131409166,39.6546444792358));
#45152=CARTESIAN_POINT('Ctrl Pts',(18.7311489735664,13.6146529975257,39.5607805287003));
#45153=CARTESIAN_POINT('Ctrl Pts',(18.5673877571369,13.5980086351894,39.394679974854));
#45154=CARTESIAN_POINT('Ctrl Pts',(18.5124682596127,13.5920240549374,39.3311884934657));
#45155=CARTESIAN_POINT('Ctrl Pts',(18.4399708836711,13.5836973552639,39.2354145052578));
#45156=CARTESIAN_POINT('Ctrl Pts',(18.4189070358755,13.5812183819914,39.2058943882269));
#45157=CARTESIAN_POINT('Ctrl Pts',(18.394534960865,13.5782916260778,39.1696167442398));
#45158=CARTESIAN_POINT('Ctrl Pts',(18.3904194147332,13.5777952799965,39.1634135204228));
#45159=CARTESIAN_POINT('Ctrl Pts',(18.3840678490589,13.577026117915,39.1537186664927));
#45160=CARTESIAN_POINT('Ctrl Pts',(18.3818070586116,13.5767517084751,39.150243471679));
#45161=CARTESIAN_POINT('Ctrl Pts',(18.3776262019851,13.5762431049307,39.1437712797646));
#45162=CARTESIAN_POINT('Ctrl Pts',(18.3757032442635,13.5760087259825,39.1407762845968));
#45163=CARTESIAN_POINT('Ctrl Pts',(18.3713519839047,13.5754773294615,39.1339577899366));
#45164=CARTESIAN_POINT('Ctrl Pts',(18.3689288550081,13.5751806530446,39.1301310560846));
#45165=CARTESIAN_POINT('Ctrl Pts',(18.3615793107461,13.5742783874152,39.1184333177141));
#45166=CARTESIAN_POINT('Ctrl Pts',(18.356696137072,13.5736755490665,39.1105351058001));
#45167=CARTESIAN_POINT('Ctrl Pts',(18.3120974267784,13.5681353738897,39.03722138046));
#45168=CARTESIAN_POINT('Ctrl Pts',(18.2762451042946,13.5634250517028,38.9695234816367));
#45169=CARTESIAN_POINT('Ctrl Pts',(18.1977738219659,13.5519773257749,38.7972999057954));
#45170=CARTESIAN_POINT('Ctrl Pts',(18.1601192794525,13.545346309984,38.6908351663647));
#45171=CARTESIAN_POINT('Ctrl Pts',(18.1170861024548,13.5349163872611,38.5239498236574));
#45172=CARTESIAN_POINT('Ctrl Pts',(18.1048832695978,13.5312631084513,38.4655542460667));
#45173=CARTESIAN_POINT('Ctrl Pts',(18.0916107487005,13.5260380016165,38.3831298721843));
#45174=CARTESIAN_POINT('Ctrl Pts',(18.0882544864497,13.5245325476312,38.3595015896524));
#45175=CARTESIAN_POINT('Ctrl Pts',(18.0831320914044,13.5218656593165,38.3179116240109));
#45176=CARTESIAN_POINT('Ctrl Pts',(18.0811780451344,13.5207100359022,38.2999758116383));
#45177=CARTESIAN_POINT('Ctrl Pts',(18.0786838709592,13.5190052402117,38.2736587327016));
#45178=CARTESIAN_POINT('Ctrl Pts',(18.0779464133546,13.5184622123355,38.2652967923427));
#45179=CARTESIAN_POINT('Ctrl Pts',(18.0767418359538,13.5175012877753,38.2505381179601));
#45180=CARTESIAN_POINT('Ctrl Pts',(18.0762519940819,13.5170841049667,38.244143326596));
#45181=CARTESIAN_POINT('Ctrl Pts',(18.0753577620025,13.5162675150875,38.2316516154254));
#45182=CARTESIAN_POINT('Ctrl Pts',(18.0749504322072,13.5158682047112,38.2255549769141));
#45183=CARTESIAN_POINT('Ctrl Pts',(18.0739305071454,13.5147893497022,38.2091155940957));
#45184=CARTESIAN_POINT('Ctrl Pts',(18.0733722663082,13.5141081239309,38.1987697973994));
#45185=CARTESIAN_POINT('Ctrl Pts',(18.0716010841214,13.5115575378631,38.1601671838289));
#45186=CARTESIAN_POINT('Ctrl Pts',(18.0709263040178,13.5096716246729,38.1318904507338));
#45187=CARTESIAN_POINT('Ctrl Pts',(18.0708705914026,13.5076665792831,38.1021211705687));
#45188=CARTESIAN_POINT('Ctrl Pts',(18.0708695284367,13.5075662293439,38.1006320175785));
#45189=CARTESIAN_POINT('Ctrl Pts',(18.0708907846761,13.5043414775085,38.0528025588322));
#45190=CARTESIAN_POINT('Ctrl Pts',(18.0725810774865,13.5011680464547,38.006481683527));
#45191=CARTESIAN_POINT('Ctrl Pts',(18.0829799114519,13.4912057006306,37.8632915999895));
#45192=CARTESIAN_POINT('Ctrl Pts',(18.0973439892374,13.4842805306195,37.766992648821));
#45193=CARTESIAN_POINT('Ctrl Pts',(18.1286691419385,13.474201116631,37.6292528833835));
#45194=CARTESIAN_POINT('Ctrl Pts',(18.1399031679281,13.4710607735314,37.5866560953272));
#45195=CARTESIAN_POINT('Ctrl Pts',(18.1724034023549,13.4630787192221,37.4785745757789));
#45196=CARTESIAN_POINT('Ctrl Pts',(18.1957363603164,13.4582783704154,37.4137684033061));
#45197=CARTESIAN_POINT('Ctrl Pts',(18.2260593482032,13.4530352735776,37.3418696283535));
#45198=CARTESIAN_POINT('Ctrl Pts',(18.2296929501473,13.4524206844592,37.3334231584612));
#45199=CARTESIAN_POINT('Ctrl Pts',(18.2351992186039,13.4515097658556,37.3208715700381));
#45200=CARTESIAN_POINT('Ctrl Pts',(18.2370260550778,13.451210789539,37.3167466700077));
#45201=CARTESIAN_POINT('Ctrl Pts',(18.2403194752569,13.4506775988557,37.3093802016011));
#45202=CARTESIAN_POINT('Ctrl Pts',(18.2417805669996,13.4504430594559,37.3061362579796));
#45203=CARTESIAN_POINT('Ctrl Pts',(18.2449691179403,13.4499355509745,37.2991089606773));
#45204=CARTESIAN_POINT('Ctrl Pts',(18.2466998357794,13.4496627837764,37.2953271541788));
#45205=CARTESIAN_POINT('Ctrl Pts',(18.2515877793142,13.4488998752378,37.284737108301));
#45206=CARTESIAN_POINT('Ctrl Pts',(18.2547725644857,13.4484113819329,37.277941559953));
#45207=CARTESIAN_POINT('Ctrl Pts',(18.2740222383722,13.4455084106901,37.2374835977458));
#45208=CARTESIAN_POINT('Ctrl Pts',(18.2910222341674,13.4431474095355,37.2042716832809));
#45209=CARTESIAN_POINT('Ctrl Pts',(18.3865858704374,13.4307822465975,37.0302137604338));
#45210=CARTESIAN_POINT('Ctrl Pts',(18.4816193707039,13.421451897999,36.8991343559337));
#45211=CARTESIAN_POINT('Ctrl Pts',(18.6482753897287,13.4066556838582,36.7211621307233));
#45212=CARTESIAN_POINT('Ctrl Pts',(18.7084850091553,13.4015534488396,36.6646116362718));
#45213=CARTESIAN_POINT('Ctrl Pts',(18.782341260351,13.3954357956097,36.6036627366104));
#45214=CARTESIAN_POINT('Ctrl Pts',(18.7926439950767,13.3945854980515,36.5953374214171));
#45215=CARTESIAN_POINT('Ctrl Pts',(18.8094797635608,13.3932005389319,36.5820172159));
#45216=CARTESIAN_POINT('Ctrl Pts',(18.8159605503241,13.3926684769468,36.5769567490174));
#45217=CARTESIAN_POINT('Ctrl Pts',(18.8275353788711,13.3917199827977,36.5680371712818));
#45218=CARTESIAN_POINT('Ctrl Pts',(18.8326166490525,13.3913042026741,36.5641616274272));
#45219=CARTESIAN_POINT('Ctrl Pts',(18.8433432649051,13.3904276956455,36.5560642996642));
#45220=CARTESIAN_POINT('Ctrl Pts',(18.8489926716681,13.3899667610494,36.5518480767304));
#45221=CARTESIAN_POINT('Ctrl Pts',(18.863957070886,13.3887475688915,36.5408071431221));
#45222=CARTESIAN_POINT('Ctrl Pts',(18.873310338234,13.3879873049897,36.5340350265729));
#45223=CARTESIAN_POINT('Ctrl Pts',(18.9168440532029,13.3844563776115,36.5031069057664));
#45224=CARTESIAN_POINT('Ctrl Pts',(18.95174183085,13.3816470890907,36.4799849659832));
#45225=CARTESIAN_POINT('Ctrl Pts',(19.1151742340503,13.3685749248996,36.3791934439524));
#45226=CARTESIAN_POINT('Ctrl Pts',(19.2516913052596,13.3578316580854,36.3156016048513));
#45227=CARTESIAN_POINT('Ctrl Pts',(19.3941040122264,13.3471516131145,36.2684889820425));
#45228=CARTESIAN_POINT('',(18.0708702075028,13.336361172809,38.0991052376092));
#45229=CARTESIAN_POINT('Ctrl Pts',(19.3941040017606,13.1771182491666,36.2684889855047));
#45230=CARTESIAN_POINT('Ctrl Pts',(19.295739838268,13.1845070632129,36.3010295777036));
#45231=CARTESIAN_POINT('Ctrl Pts',(19.2001359782007,13.1918587964505,36.3414484626243));
#45232=CARTESIAN_POINT('Ctrl Pts',(19.1000991907493,13.1994385856499,36.3935987976581));
#45233=CARTESIAN_POINT('Ctrl Pts',(19.0920034783272,13.2000510867163,36.3978928192897));
#45234=CARTESIAN_POINT('Ctrl Pts',(19.0799737026927,13.2009595240691,36.4043837506301));
#45235=CARTESIAN_POINT('Ctrl Pts',(19.0760163839233,13.201258086554,36.4065369413214));
#45236=CARTESIAN_POINT('Ctrl Pts',(19.0691686469783,13.2017741891633,36.4102939678087));
#45237=CARTESIAN_POINT('Ctrl Pts',(19.0662747790067,13.2019921284975,36.4118913852251));
#45238=CARTESIAN_POINT('Ctrl Pts',(19.0633726770854,13.2022105165394,36.413503093668));
#45239=CARTESIAN_POINT('Ctrl Pts',(19.0633603915884,13.2022114410407,36.4135099167051));
#45240=CARTESIAN_POINT('Ctrl Pts',(19.0633360823957,13.2022132703363,36.4135234177293));
#45241=CARTESIAN_POINT('Ctrl Pts',(19.0633240588882,13.2022141751166,36.4135300956046));
#45242=CARTESIAN_POINT('Ctrl Pts',(19.0633002687762,13.2022159653394,36.4135433090036));
#45243=CARTESIAN_POINT('Ctrl Pts',(19.0632885019325,13.2022168507999,36.4135498446532));
#45244=CARTESIAN_POINT('Ctrl Pts',(19.0632662162387,13.2022185278036,36.4135622230853));
#45245=CARTESIAN_POINT('Ctrl Pts',(19.0632556979489,13.2022193193052,36.4135680655243));
#45246=CARTESIAN_POINT('Ctrl Pts',(19.0632347137632,13.2022208983612,36.4135797215566));
#45247=CARTESIAN_POINT('Ctrl Pts',(19.0632242476582,13.2022216859315,36.4135855352649));
#45248=CARTESIAN_POINT('Ctrl Pts',(19.0632033681448,13.2022232571023,36.4135971336639));
#45249=CARTESIAN_POINT('Ctrl Pts',(19.0631929541759,13.202224040745,36.4136029186647));
#45250=CARTESIAN_POINT('Ctrl Pts',(19.0631721779797,13.2022256041326,36.4136144601755));
#45251=CARTESIAN_POINT('Ctrl Pts',(19.0631618156603,13.2022263838844,36.4136202167354));
#45252=CARTESIAN_POINT('Ctrl Pts',(19.0631411424176,13.2022279395163,36.4136317015526));
#45253=CARTESIAN_POINT('Ctrl Pts',(19.0631308313712,13.2022287154056,36.413637429877));
#45254=CARTESIAN_POINT('Ctrl Pts',(19.0631102607706,13.2022302633054,36.4136488581661));
#45255=CARTESIAN_POINT('Ctrl Pts',(19.063100000887,13.2022310353406,36.4136545583126));
#45256=CARTESIAN_POINT('Ctrl Pts',(19.0630795320652,13.2022325755732,36.413665930546));
#45257=CARTESIAN_POINT('Ctrl Pts',(19.063069323209,13.2022333437646,36.4136716025861));
#45258=CARTESIAN_POINT('Ctrl Pts',(19.0630489543621,13.2022348764661,36.4136829197588));
#45259=CARTESIAN_POINT('Ctrl Pts',(19.0630387954007,13.2022356408988,36.4136885643183));
#45260=CARTESIAN_POINT('Ctrl Pts',(19.0630185283358,13.2022371659333,36.4136998254191));
#45261=CARTESIAN_POINT('Ctrl Pts',(19.063008419748,13.2022379265714,36.4137054422282));
#45262=CARTESIAN_POINT('Ctrl Pts',(19.0629882517581,13.2022394441427,36.4137166487541));
#45263=CARTESIAN_POINT('Ctrl Pts',(19.0629781927242,13.202240201048,36.413722238265));
#45264=CARTESIAN_POINT('Ctrl Pts',(19.0629581244126,13.2022417111108,36.4137333898737));
#45265=CARTESIAN_POINT('Ctrl Pts',(19.0629481148217,13.2022424642917,36.4137389521444));
#45266=CARTESIAN_POINT('Ctrl Pts',(19.06292814557,13.2022439668926,36.4137500491727));
#45267=CARTESIAN_POINT('Ctrl Pts',(19.0629181855005,13.2022447163433,36.4137555841562));
#45268=CARTESIAN_POINT('Ctrl Pts',(19.0628983132665,13.2022462116361,36.4137666277322));
#45269=CARTESIAN_POINT('Ctrl Pts',(19.0628884017446,13.2022469574299,36.4137721359663));
#45270=CARTESIAN_POINT('Ctrl Pts',(19.0628686276627,13.2022484453295,36.4137831254526));
#45271=CARTESIAN_POINT('Ctrl Pts',(19.062858764783,13.2022491874593,36.4137886068813));
#45272=CARTESIAN_POINT('Ctrl Pts',(19.0592991190886,13.2025170313741,36.4157669689827));
#45273=CARTESIAN_POINT('Ctrl Pts',(19.0557555344542,13.2027834157959,36.4177510766372));
#45274=CARTESIAN_POINT('Ctrl Pts',(19.0459716788548,13.2035182838886,36.4232698627054));
#45275=CARTESIAN_POINT('Ctrl Pts',(19.0397447335202,13.2039852904599,36.4268282162327));
#45276=CARTESIAN_POINT('Ctrl Pts',(19.025819094879,13.2050284376012,36.4348892948614));
#45277=CARTESIAN_POINT('Ctrl Pts',(19.0181314375016,13.2056034476988,36.4394108788538));
#45278=CARTESIAN_POINT('Ctrl Pts',(18.9942489272227,13.2073879755422,36.4536814895117));
#45279=CARTESIAN_POINT('Ctrl Pts',(18.9781653257,13.2085871581053,36.4636156273978));
#45280=CARTESIAN_POINT('Ctrl Pts',(18.9148369702489,13.2133092053696,36.5040286632081));
#45281=CARTESIAN_POINT('Ctrl Pts',(18.8687851716678,13.2167441774213,36.5363321005163));
#45282=CARTESIAN_POINT('Ctrl Pts',(18.7777021688406,13.223680186999,36.6063562868535));
#45283=CARTESIAN_POINT('Ctrl Pts',(18.7328511649458,13.2271742182929,36.6442123598367));
#45284=CARTESIAN_POINT('Ctrl Pts',(18.596959891002,13.2382351795582,36.7699555364346));
#45285=CARTESIAN_POINT('Ctrl Pts',(18.5128104311542,13.2458354397861,36.8647666324445));
#45286=CARTESIAN_POINT('Ctrl Pts',(18.4253787922848,13.2552633350704,36.9852742463396));
#45287=CARTESIAN_POINT('Ctrl Pts',(18.412527513997,13.2566946027963,37.0036531145008));
#45288=CARTESIAN_POINT('Ctrl Pts',(18.3947323252872,13.258744823538,37.0300714264242));
#45289=CARTESIAN_POINT('Ctrl Pts',(18.3895221857977,13.2593538163374,37.0379300094492));
#45290=CARTESIAN_POINT('Ctrl Pts',(18.3811265251355,13.2603496703628,37.0507972271508));
#45291=CARTESIAN_POINT('Ctrl Pts',(18.3779060990942,13.2607352324195,37.0557829911789));
#45292=CARTESIAN_POINT('Ctrl Pts',(18.3711925172954,13.2615466017112,37.0662827528582));
#45293=CARTESIAN_POINT('Ctrl Pts',(18.3677042418526,13.2619725819766,37.0717997671009));
#45294=CARTESIAN_POINT('Ctrl Pts',(18.3594317258841,13.2629934777316,37.0850316740258));
#45295=CARTESIAN_POINT('Ctrl Pts',(18.3546738461803,13.2635893459159,37.0927627848549));
#45296=CARTESIAN_POINT('Ctrl Pts',(18.3386112457111,13.2656312718369,37.1192805219571));
#45297=CARTESIAN_POINT('Ctrl Pts',(18.3275726692109,13.2670868692993,37.1382255754771));
#45298=CARTESIAN_POINT('Ctrl Pts',(18.3018981769354,13.2706028747853,37.1840686296835));
#45299=CARTESIAN_POINT('Ctrl Pts',(18.2875754893299,13.2726737486651,37.211134321155));
#45300=CARTESIAN_POINT('Ctrl Pts',(18.234879484166,13.2807351863236,37.3167191823275));
#45301=CARTESIAN_POINT('Ctrl Pts',(18.2012177998712,13.2868703672801,37.397462659485));
#45302=CARTESIAN_POINT('Ctrl Pts',(18.1374569480367,13.3009769688883,37.585397226114));
#45303=CARTESIAN_POINT('Ctrl Pts',(18.1109190123339,13.3089738170708,37.693481761211));
#45304=CARTESIAN_POINT('Ctrl Pts',(18.0897939048198,13.3185267566863,37.8291794622294));
#45305=CARTESIAN_POINT('Ctrl Pts',(18.0862867601388,13.3203353082226,37.8551880976322));
#45306=CARTESIAN_POINT('Ctrl Pts',(18.0818866307341,13.3229758969158,37.8937440804848));
#45307=CARTESIAN_POINT('Ctrl Pts',(18.0805840081068,13.3238254920839,37.9062406881092));
#45308=CARTESIAN_POINT('Ctrl Pts',(18.0785886463918,13.3252514121523,37.927384269676));
#45309=CARTESIAN_POINT('Ctrl Pts',(18.0778319879714,13.3258308641969,37.9360246341787));
#45310=CARTESIAN_POINT('Ctrl Pts',(18.0767742064885,13.326703809504,37.9491191588825));
#45311=CARTESIAN_POINT('Ctrl Pts',(18.0764302402003,13.3269995860633,37.9535696027994));
#45312=CARTESIAN_POINT('Ctrl Pts',(18.0758552968145,13.3275157226276,37.9613604351347));
#45313=CARTESIAN_POINT('Ctrl Pts',(18.0756175671818,13.3277364529654,37.9647002564846));
#45314=CARTESIAN_POINT('Ctrl Pts',(18.0751590355586,13.3281773751392,37.9713878915008));
#45315=CARTESIAN_POINT('Ctrl Pts',(18.0749382724596,13.3283975648136,37.9747356458153));
#45316=CARTESIAN_POINT('Ctrl Pts',(18.0744692701854,13.3288835600262,37.9821420379353));
#45317=CARTESIAN_POINT('Ctrl Pts',(18.0742251264333,13.3291491406976,37.9862009325409));
#45318=CARTESIAN_POINT('Ctrl Pts',(18.0736507023885,13.3298069821556,37.9962824930422));
#45319=CARTESIAN_POINT('Ctrl Pts',(18.0733358282452,13.3301984245531,38.0023060430788));
#45320=CARTESIAN_POINT('Ctrl Pts',(18.0716108636269,13.332545666938,38.0385661124733));
#45321=CARTESIAN_POINT('Ctrl Pts',(18.0708842484705,13.3344667389137,38.0688325647746));
#45322=CARTESIAN_POINT('Ctrl Pts',(18.0708702075028,13.336361172809,38.0991052376092));
#45323=CARTESIAN_POINT('Ctrl Pts',(18.0708702086382,13.3363610198239,38.0991027929391));
#45324=CARTESIAN_POINT('Ctrl Pts',(18.0708489954218,13.3392153506683,38.1447143910078));
#45325=CARTESIAN_POINT('Ctrl Pts',(18.072445425963,13.3420078590196,38.1903161632809));
#45326=CARTESIAN_POINT('Ctrl Pts',(18.0874536075436,13.3549139772547,38.4029540689302));
#45327=CARTESIAN_POINT('Ctrl Pts',(18.1209706118427,13.3646569627379,38.5678291612205));
#45328=CARTESIAN_POINT('Ctrl Pts',(18.1889039431484,13.3776934586107,38.7657419056431));
#45329=CARTESIAN_POINT('Ctrl Pts',(18.2037154102981,13.3803262450693,38.8047286589164));
#45330=CARTESIAN_POINT('Ctrl Pts',(18.2242205707633,13.3837408668965,38.8538454629391));
#45331=CARTESIAN_POINT('Ctrl Pts',(18.2287588969273,13.3844838607765,38.8644478456376));
#45332=CARTESIAN_POINT('Ctrl Pts',(18.2362226172729,13.385685962907,38.881461162125));
#45333=CARTESIAN_POINT('Ctrl Pts',(18.2390885957778,13.3861430554713,38.8878979807245));
#45334=CARTESIAN_POINT('Ctrl Pts',(18.2446213721524,13.387017065147,38.9001432865034));
#45335=CARTESIAN_POINT('Ctrl Pts',(18.2472819041317,13.3874337640563,38.9059545153501));
#45336=CARTESIAN_POINT('Ctrl Pts',(18.2534337497153,13.3883892269867,38.9192170659335));
#45337=CARTESIAN_POINT('Ctrl Pts',(18.2569439403197,13.3889286324031,38.9266594444078));
#45338=CARTESIAN_POINT('Ctrl Pts',(18.2662375189434,13.3903420032177,38.9460414986288));
#45339=CARTESIAN_POINT('Ctrl Pts',(18.272096565465,13.3912185613104,38.9579442080747));
#45340=CARTESIAN_POINT('Ctrl Pts',(18.3155898683635,13.3976234681318,39.0440483131015));
#45341=CARTESIAN_POINT('Ctrl Pts',(18.3578614607377,13.4033136954771,39.1157963937834));
#45342=CARTESIAN_POINT('Ctrl Pts',(18.4729610116639,13.4176301007636,39.2851025333739));
#45343=CARTESIAN_POINT('Ctrl Pts',(18.5506409955429,13.4263810307947,39.3789335177755));
#45344=CARTESIAN_POINT('Ctrl Pts',(18.6726409319254,13.4385976535679,39.5008041971015));
#45345=CARTESIAN_POINT('Ctrl Pts',(18.7100724914958,13.4421716545388,39.5353474354571));
#45346=CARTESIAN_POINT('Ctrl Pts',(18.7623182600264,13.4468883800316,39.5798650344584));
#45347=CARTESIAN_POINT('Ctrl Pts',(18.775965414295,13.4480967986252,39.5911726903452));
#45348=CARTESIAN_POINT('Ctrl Pts',(18.7964000097191,13.4498692698242,39.6076346276636));
#45349=CARTESIAN_POINT('Ctrl Pts',(18.8030685016884,13.450441984569,39.6129342688132));
#45350=CARTESIAN_POINT('Ctrl Pts',(18.8151483506504,13.4514688978372,39.6224046099851));
#45351=CARTESIAN_POINT('Ctrl Pts',(18.8205471340836,13.4519241049869,39.6265910284029));
#45352=CARTESIAN_POINT('Ctrl Pts',(18.8291613906758,13.4526443508002,39.6331978681199));
#45353=CARTESIAN_POINT('Ctrl Pts',(18.8323623317358,13.4529106623808,39.6356370105848));
#45354=CARTESIAN_POINT('Ctrl Pts',(18.838319976088,13.4534038405728,39.6401473850961));
#45355=CARTESIAN_POINT('Ctrl Pts',(18.8410745720454,13.4536308836003,39.6422212222934));
#45356=CARTESIAN_POINT('Ctrl Pts',(18.8474557856805,13.4541545910222,39.6469986592832));
#45357=CARTESIAN_POINT('Ctrl Pts',(18.8510863582522,13.4544508828239,39.6496968937895));
#45358=CARTESIAN_POINT('Ctrl Pts',(18.8621743921037,13.455350819529,39.6578771155848));
#45359=CARTESIAN_POINT('Ctrl Pts',(18.8696619783147,13.4559517342549,39.6633183253148));
#45360=CARTESIAN_POINT('Ctrl Pts',(18.9375845730285,13.4613446940022,39.7119343717222));
#45361=CARTESIAN_POINT('Ctrl Pts',(19.0004346202833,13.4659230425509,39.7516448768358));
#45362=CARTESIAN_POINT('Ctrl Pts',(19.2112031354325,13.4805128720727,39.8683636805306));
#45363=CARTESIAN_POINT('Ctrl Pts',(19.3668180631527,13.4902031167279,39.9298612089557));
#45364=CARTESIAN_POINT('Ctrl Pts',(19.5699004235054,13.5032403955912,39.981060470662));
#45365=CARTESIAN_POINT('Ctrl Pts',(19.6117328526723,13.5059410613468,39.9901381772669));
#45366=CARTESIAN_POINT('Ctrl Pts',(19.6652754877856,13.5094322185521,39.9999045793668));
#45367=CARTESIAN_POINT('Ctrl Pts',(19.6767392135258,13.5101816559981,40.0018886308294));
#45368=CARTESIAN_POINT('Ctrl Pts',(19.6951955133683,13.5113916752244,40.00491121706));
#45369=CARTESIAN_POINT('Ctrl Pts',(19.7021771910167,13.5118501924461,40.0060152392362));
#45370=CARTESIAN_POINT('Ctrl Pts',(19.7154778499266,13.5127252739528,40.0080436278508));
#45371=CARTESIAN_POINT('Ctrl Pts',(19.7217956748935,13.5131416107981,40.0089750369025));
#45372=CARTESIAN_POINT('Ctrl Pts',(19.7362226364188,13.5140939171807,40.0110288005477));
#45373=CARTESIAN_POINT('Ctrl Pts',(19.7443344823529,13.5146305130166,40.0121309352835));
#45374=CARTESIAN_POINT('Ctrl Pts',(19.7654705373687,13.5160317433022,40.0148657345928));
#45375=CARTESIAN_POINT('Ctrl Pts',(19.7785046524799,13.5168988983045,40.0164171380416));
#45376=CARTESIAN_POINT('Ctrl Pts',(19.8695725422199,13.5229798873746,40.0263151719155));
#45377=CARTESIAN_POINT('Ctrl Pts',(19.9480260652365,13.5283371203793,40.0300252040865));
#45378=CARTESIAN_POINT('Ctrl Pts',(20.1916405720254,13.5453334103625,40.0266810675328));
#45379=CARTESIAN_POINT('Ctrl Pts',(20.3558082288573,13.5573630659639,40.0032129851045));
#45380=CARTESIAN_POINT('Ctrl Pts',(20.5512640292596,13.5714384224051,39.9490724026588));
#45381=CARTESIAN_POINT('Ctrl Pts',(20.5872576533532,13.5740158248595,39.937958022169));
#45382=CARTESIAN_POINT('Ctrl Pts',(20.6300274432953,13.5770426054451,39.9233662832219));
#45383=CARTESIAN_POINT('Ctrl Pts',(20.6371352066219,13.5775444071354,39.9208948116692));
#45384=CARTESIAN_POINT('Ctrl Pts',(20.6481528311048,13.5783201634238,39.9169914138822));
#45385=CARTESIAN_POINT('Ctrl Pts',(20.6520727283757,13.5785957549147,39.9155883477024));
#45386=CARTESIAN_POINT('Ctrl Pts',(20.6593334889027,13.5791054263012,39.9129629235679));
#45387=CARTESIAN_POINT('Ctrl Pts',(20.6626754850138,13.5793396980409,39.9117440254431));
#45388=CARTESIAN_POINT('Ctrl Pts',(20.6702424481523,13.5798694257478,39.9089604515167));
#45389=CARTESIAN_POINT('Ctrl Pts',(20.6744653094934,13.5801645493644,39.9073902184543));
#45390=CARTESIAN_POINT('Ctrl Pts',(20.6872613774784,13.5810574251361,39.9025810231823));
#45391=CARTESIAN_POINT('Ctrl Pts',(20.6958171925645,13.5816525093738,39.8992956924009));
#45392=CARTESIAN_POINT('Ctrl Pts',(20.8062320829659,13.5893113493639,39.8559923184681));
#45393=CARTESIAN_POINT('Ctrl Pts',(20.9045465706814,13.5959061146401,39.8074314442493));
#45394=CARTESIAN_POINT('Ctrl Pts',(21.0695968470069,13.6074468153303,39.7076262187894));
#45395=CARTESIAN_POINT('Ctrl Pts',(21.13809549857,13.6123988190635,39.6598838678357));
#45396=CARTESIAN_POINT('Ctrl Pts',(21.2646270248928,13.6222100886688,39.5589104273561));
#45397=CARTESIAN_POINT('Ctrl Pts',(21.3229159928581,13.6270481607459,39.5062689222233));
#45398=CARTESIAN_POINT('Ctrl Pts',(21.3912150425075,13.6332512862093,39.4365735256565));
#45399=CARTESIAN_POINT('Ctrl Pts',(21.4043924341608,13.6344749228778,39.4227206557487));
#45400=CARTESIAN_POINT('Ctrl Pts',(21.4231906273248,13.6362612743164,39.4023612531121));
#45401=CARTESIAN_POINT('Ctrl Pts',(21.4289775331301,13.6368169632218,39.396009105369));
#45402=CARTESIAN_POINT('Ctrl Pts',(21.4390291247481,13.6377924620046,39.3848265456323));
#45403=CARTESIAN_POINT('Ctrl Pts',(21.4433124383181,13.6382114859127,39.3800129991352));
#45404=CARTESIAN_POINT('Ctrl Pts',(21.451570231621,13.6390258673992,39.3706388214836));
#45405=CARTESIAN_POINT('Ctrl Pts',(21.4555475370432,13.6394211011919,39.3660807707246));
#45406=CARTESIAN_POINT('Ctrl Pts',(21.4649873765201,13.6403663856911,39.3551593028287));
#45407=CARTESIAN_POINT('Ctrl Pts',(21.4704299461195,13.6409172446259,39.3487788669928));
#45408=CARTESIAN_POINT('Ctrl Pts',(21.4898487450387,13.6429040433563,39.3257108476849));
#45409=CARTESIAN_POINT('Ctrl Pts',(21.5035834658426,13.6443496486619,39.3088230064279));
#45410=CARTESIAN_POINT('Ctrl Pts',(21.6111534198342,13.6560055780185,39.1718877107781));
#45411=CARTESIAN_POINT('Ctrl Pts',(21.6907333274036,13.6667826130711,39.0413615887572));
#45412=CARTESIAN_POINT('Ctrl Pts',(21.788160134289,13.6834871105829,38.8285018758172));
#45413=CARTESIAN_POINT('Ctrl Pts',(21.8174367900994,13.6893193618148,38.7520405177836));
#45414=CARTESIAN_POINT('Ctrl Pts',(21.8524067692817,13.6974638252642,38.6398233547797));
#45415=CARTESIAN_POINT('Ctrl Pts',(21.862091218629,13.6999069759091,38.6054075457684));
#45416=CARTESIAN_POINT('Ctrl Pts',(21.8726234378143,13.7027972256356,38.563550406144));
#45417=CARTESIAN_POINT('Ctrl Pts',(21.8743910659366,13.7032915172621,38.5563503645383));
#45418=CARTESIAN_POINT('Ctrl Pts',(21.8770808566796,13.7040581942789,38.5451147571212));
#45419=CARTESIAN_POINT('Ctrl Pts',(21.8780315888109,13.7043321568776,38.5410862067083));
#45420=CARTESIAN_POINT('Ctrl Pts',(21.8797758875643,13.7048403599001,38.5335871801471));
#45421=CARTESIAN_POINT('Ctrl Pts',(21.880572806567,13.7050747825164,38.5301175999407));
#45422=CARTESIAN_POINT('Ctrl Pts',(21.8823638931859,13.7056068250852,38.5222195275474));
#45423=CARTESIAN_POINT('Ctrl Pts',(21.8833520383913,13.705904100485,38.5177897274217));
#45424=CARTESIAN_POINT('Ctrl Pts',(21.8863242244484,13.7068100060923,38.5042407347854));
#45425=CARTESIAN_POINT('Ctrl Pts',(21.888257770244,13.7074158529275,38.4951104313992));
#45426=CARTESIAN_POINT('Ctrl Pts',(21.9063357556511,13.7132488512,38.4065802709513));
#45427=CARTESIAN_POINT('Ctrl Pts',(21.9175312420245,13.7182212127513,38.3262408002213));
#45428=CARTESIAN_POINT('Ctrl Pts',(21.9359972793637,13.7330067223166,38.0819784549729));
#45429=CARTESIAN_POINT('Ctrl Pts',(21.9274729233002,13.7425672628078,37.9176332779694));
#45430=CARTESIAN_POINT('Ctrl Pts',(21.8912738612039,13.7552511786532,37.7176784970078));
#45431=CARTESIAN_POINT('Ctrl Pts',(21.8830947958538,13.7577353830588,37.679238547234));
#45432=CARTESIAN_POINT('Ctrl Pts',(21.8710597075914,13.7609820785598,37.6301001714052));
#45433=CARTESIAN_POINT('Ctrl Pts',(21.8682748482875,13.7617103454296,37.6191472567324));
#45434=CARTESIAN_POINT('Ctrl Pts',(21.8636108002008,13.7628943579551,37.6014558488316));
#45435=CARTESIAN_POINT('Ctrl Pts',(21.8617908863542,13.76334819786,37.5947018913116));
#45436=CARTESIAN_POINT('Ctrl Pts',(21.8582343150544,13.7642198625127,37.5817830494051));
#45437=CARTESIAN_POINT('Ctrl Pts',(21.8565036059079,13.7646374905447,37.5756166124614));
#45438=CARTESIAN_POINT('Ctrl Pts',(21.8524891414737,13.7655916046178,37.5615822657654));
#45439=CARTESIAN_POINT('Ctrl Pts',(21.8501859207831,13.766128713682,37.553720098425));
#45440=CARTESIAN_POINT('Ctrl Pts',(21.8439713708303,13.7675514632587,37.532996604485));
#45441=CARTESIAN_POINT('Ctrl Pts',(21.8399756227077,13.7684398238992,37.5201612643735));
#45442=CARTESIAN_POINT('Ctrl Pts',(21.8084002587606,13.7752658657872,37.4223474303605));
#45443=CARTESIAN_POINT('Ctrl Pts',(21.7750855501925,13.7813912376485,37.3393479085504));
#45444=CARTESIAN_POINT('Ctrl Pts',(21.6656600888732,13.7989955722757,37.1134613562713));
#45445=CARTESIAN_POINT('Ctrl Pts',(21.5771689092334,13.8107707837113,36.9774061675487));
#45446=CARTESIAN_POINT('Ctrl Pts',(21.4530375835079,13.8240266108867,36.8306869132449));
#45447=CARTESIAN_POINT('Ctrl Pts',(21.4327743999678,13.8261052686655,36.8078577058324));
#45448=CARTESIAN_POINT('Ctrl Pts',(21.4071596873433,13.8286207206734,36.7803431704839));
#45449=CARTESIAN_POINT('Ctrl Pts',(21.4023141947713,13.8290918015148,36.7751953214397));
#45450=CARTESIAN_POINT('Ctrl Pts',(21.3946389813676,13.8298303656721,36.7671304708519));
#45451=CARTESIAN_POINT('Ctrl Pts',(21.3918282151018,13.8300992476635,36.7641956391424));
#45452=CARTESIAN_POINT('Ctrl Pts',(21.3865298172039,13.8306030843481,36.7586982526915));
#45453=CARTESIAN_POINT('Ctrl Pts',(21.3840443719918,13.8308381906166,36.7561337537022));
#45454=CARTESIAN_POINT('Ctrl Pts',(21.3783572600727,13.8313733548836,36.7502982664452));
#45455=CARTESIAN_POINT('Ctrl Pts',(21.3751510667925,13.8316730568944,36.7470317629303));
#45456=CARTESIAN_POINT('Ctrl Pts',(21.3666261457944,13.8324647425108,36.7384080929788));
#45457=CARTESIAN_POINT('Ctrl Pts',(21.3612874824639,13.832955220183,36.7330706169493));
#45458=CARTESIAN_POINT('Ctrl Pts',(21.3236529755767,13.8363770307189,36.6958836416411));
#45459=CARTESIAN_POINT('Ctrl Pts',(21.2902710545293,13.8392290685353,36.665147635996));
#45460=CARTESIAN_POINT('Ctrl Pts',(21.1516409444714,13.8505101085888,36.546260668394));
#45461=CARTESIAN_POINT('Ctrl Pts',(21.0382032601898,13.8585249811965,36.4682762356855));
#45462=CARTESIAN_POINT('Ctrl Pts',(20.860228107468,13.8707293613139,36.3720589809401));
#45463=CARTESIAN_POINT('Ctrl Pts',(20.8014920038589,13.8746994998026,36.3440438306523));
#45464=CARTESIAN_POINT('Ctrl Pts',(20.7061706074671,13.8811499531319,36.3043590128268));
#45465=CARTESIAN_POINT('Ctrl Pts',(20.6704577325247,13.8835678042471,36.2907212495012));
#45466=CARTESIAN_POINT('Ctrl Pts',(20.6237942155584,13.8867393156911,36.2744730549034));
#45467=CARTESIAN_POINT('Ctrl Pts',(20.6131915946963,13.8874607144765,36.2708843912302));
#45468=CARTESIAN_POINT('Ctrl Pts',(20.5959362441997,13.8886362942413,36.265210871696));
#45469=CARTESIAN_POINT('Ctrl Pts',(20.5893022856478,13.8890886199057,36.2630694170678));
#45470=CARTESIAN_POINT('Ctrl Pts',(20.5765446078646,13.8899592456646,36.2590274356056));
#45471=CARTESIAN_POINT('Ctrl Pts',(20.57042272428,13.8903773592552,36.2571213871565));
#45472=CARTESIAN_POINT('Ctrl Pts',(20.5564103793656,13.8913351990854,36.2528351533583));
#45473=CARTESIAN_POINT('Ctrl Pts',(20.5485139822354,13.8918755655511,36.2504749559208));
#45474=CARTESIAN_POINT('Ctrl Pts',(20.5275388463699,13.8933126264856,36.2443517213357));
#45475=CARTESIAN_POINT('Ctrl Pts',(20.5144351882301,13.8942121295448,36.2406764161148));
#45476=CARTESIAN_POINT('Ctrl Pts',(20.408346861704,13.9015098692605,36.2121281368261));
#45477=CARTESIAN_POINT('Ctrl Pts',(20.3136730499356,13.9081273104651,36.1941113959828));
#45478=CARTESIAN_POINT('Ctrl Pts',(20.1226197140805,13.9216554501872,36.1723760006934));
#45479=CARTESIAN_POINT('Ctrl Pts',(20.0265014590896,13.9285464540461,36.1686621087005));
#45480=CARTESIAN_POINT('Ctrl Pts',(19.8711016849172,13.9396015732736,36.174263250096));
#45481=CARTESIAN_POINT('Ctrl Pts',(19.8118169313951,13.943796212096,36.1791499368758));
#45482=CARTESIAN_POINT('Ctrl Pts',(19.7236330946968,13.9499230948671,36.1905415198447));
#45483=CARTESIAN_POINT('Ctrl Pts',(19.6945057189264,13.9519280547887,36.1949845586013));
#45484=CARTESIAN_POINT('Ctrl Pts',(19.6586043647402,13.9543669138082,36.2013055922326));
#45485=CARTESIAN_POINT('Ctrl Pts',(19.6517255744913,13.9548327238142,36.2025553072365));
#45486=CARTESIAN_POINT('Ctrl Pts',(19.640876391822,13.9555648940217,36.2045873367379));
#45487=CARTESIAN_POINT('Ctrl Pts',(19.6369014904076,13.9558326135998,36.2053447798912));
#45488=CARTESIAN_POINT('Ctrl Pts',(19.6294195347463,13.9563355029707,36.2067949254307));
#45489=CARTESIAN_POINT('Ctrl Pts',(19.6259120641732,13.9565708172079,36.2074848607976));
#45490=CARTESIAN_POINT('Ctrl Pts',(19.6178902793492,13.9571080224161,36.2090859547423));
#45491=CARTESIAN_POINT('Ctrl Pts',(19.6133772980862,13.9574095473211,36.210003531057));
#45492=CARTESIAN_POINT('Ctrl Pts',(19.6013814759793,13.9582092585773,36.2124872785569));
#45493=CARTESIAN_POINT('Ctrl Pts',(19.5939044932465,13.9587058898582,36.2140818031038));
#45494=CARTESIAN_POINT('Ctrl Pts',(19.5400681055324,13.962269880212,36.2258978522188));
#45495=CARTESIAN_POINT('Ctrl Pts',(19.4940861494538,13.9652503128363,36.2377840522972));
#45496=CARTESIAN_POINT('Ctrl Pts',(19.4303355821949,13.969352282064,36.256799603463));
#45497=CARTESIAN_POINT('Ctrl Pts',(19.4121731230477,13.9705174109781,36.2625114023504));
#45498=CARTESIAN_POINT('Ctrl Pts',(19.3941039465104,13.9716756753762,36.2684890037825));
#45499=CARTESIAN_POINT('Origin',(20.,-1.3495818343519,38.1));
#45500=CARTESIAN_POINT('',(19.3941040816519,14.9348319053408,36.2684889590753));
#45501=CARTESIAN_POINT('',(19.3941039945165,14.7625557686229,36.2684889879012));
#45502=CARTESIAN_POINT('',(19.3941040087494,-1.3495818343519,36.2684889831927));
#45503=CARTESIAN_POINT('',(18.0708708463018,14.2998795404039,38.1017114188227));
#45504=CARTESIAN_POINT('Ctrl Pts',(19.3941040816519,14.9348319053408,36.2684889590753));
#45505=CARTESIAN_POINT('Ctrl Pts',(19.4247862302146,14.9328999468963,36.2583387671491));
#45506=CARTESIAN_POINT('Ctrl Pts',(19.4557306857153,14.9309715206932,36.2489571730916));
#45507=CARTESIAN_POINT('Ctrl Pts',(19.6120641793806,14.9212744810258,36.2058234950179));
#45508=CARTESIAN_POINT('Ctrl Pts',(19.7403665114976,14.9134320283775,36.1840191843203));
#45509=CARTESIAN_POINT('Ctrl Pts',(19.8836306306663,14.9042650559825,36.1743336816182));
#45510=CARTESIAN_POINT('Ctrl Pts',(19.897394118544,14.9033805905104,36.1735512939181));
#45511=CARTESIAN_POINT('Ctrl Pts',(19.9194490484728,14.9019567243745,36.172534596882));
#45512=CARTESIAN_POINT('Ctrl Pts',(19.9277358358974,14.9014202445816,36.1722061253688));
#45513=CARTESIAN_POINT('Ctrl Pts',(19.9424403209514,14.9004655467306,36.1717182130495));
#45514=CARTESIAN_POINT('Ctrl Pts',(19.9488572204114,14.9000479999005,36.1715373529738));
#45515=CARTESIAN_POINT('Ctrl Pts',(19.9622199291313,14.8991765102028,36.1712274671801));
#45516=CARTESIAN_POINT('Ctrl Pts',(19.9691657609965,14.8987224031027,36.171103925894));
#45517=CARTESIAN_POINT('Ctrl Pts',(19.9871953287831,14.897540694577,36.1708806528431));
#45518=CARTESIAN_POINT('Ctrl Pts',(19.9982794010565,14.8968113042384,36.1708389268761));
#45519=CARTESIAN_POINT('Ctrl Pts',(20.0465289848394,14.8936231329239,36.171073108807));
#45520=CARTESIAN_POINT('Ctrl Pts',(20.0836796137598,14.8911343032896,36.1723274923241));
#45521=CARTESIAN_POINT('Ctrl Pts',(20.1831060922766,14.8843770745986,36.1785640923564));
#45522=CARTESIAN_POINT('Ctrl Pts',(20.2452108772903,14.880053385642,36.1854989974155));
#45523=CARTESIAN_POINT('Ctrl Pts',(20.4426830809356,14.8660038154632,36.217315832157));
#45524=CARTESIAN_POINT('Ctrl Pts',(20.5757616948277,14.8560450273797,36.2536620669921));
#45525=CARTESIAN_POINT('Ctrl Pts',(20.7218537719816,14.8450634560484,36.3109097158509));
#45526=CARTESIAN_POINT('Ctrl Pts',(20.7397616984407,14.8437171756498,36.3182397492967));
#45527=CARTESIAN_POINT('Ctrl Pts',(20.7861779411219,14.8402323024529,36.3380592175638));
#45528=CARTESIAN_POINT('Ctrl Pts',(20.814501148073,14.8381103958795,36.3509719193962));
#45529=CARTESIAN_POINT('Ctrl Pts',(20.8491387344421,14.8355318017446,36.3677874253341));
#45530=CARTESIAN_POINT('Ctrl Pts',(20.855757680072,14.8350398095165,36.3710477764029));
#45531=CARTESIAN_POINT('Ctrl Pts',(20.8660933994628,14.8342729190881,36.3762128266292));
#45532=CARTESIAN_POINT('Ctrl Pts',(20.8698228843148,14.8339964801779,36.3780917137045));
#45533=CARTESIAN_POINT('Ctrl Pts',(20.8767170161116,14.8334860324997,36.3815930408509));
#45534=CARTESIAN_POINT('Ctrl Pts',(20.87988325262,14.8332518268973,36.3832121081187));
#45535=CARTESIAN_POINT('Ctrl Pts',(20.8870358297812,14.8327232481282,36.3868945913395));
#45536=CARTESIAN_POINT('Ctrl Pts',(20.8910194489728,14.8324292011929,36.3889631660726));
#45537=CARTESIAN_POINT('Ctrl Pts',(20.9030405365733,14.8315428090705,36.3952587254979));
#45538=CARTESIAN_POINT('Ctrl Pts',(20.9110555537767,14.8309530752577,36.3995286507979));
#45539=CARTESIAN_POINT('Ctrl Pts',(21.0070918910693,14.8238984916717,36.4515650457887));
#45540=CARTESIAN_POINT('Ctrl Pts',(21.0913085345902,14.8178264372581,36.5060666434814));
#45541=CARTESIAN_POINT('Ctrl Pts',(21.3053016691491,14.8016812306791,36.6695030167515));
#45542=CARTESIAN_POINT('Ctrl Pts',(21.4255903173114,14.7917354971492,36.7893434100483));
#45543=CARTESIAN_POINT('Ctrl Pts',(21.5411240658571,14.779715441941,36.9394428385481));
#45544=CARTESIAN_POINT('Ctrl Pts',(21.5532749576368,14.7784153144304,36.9557565086986));
#45545=CARTESIAN_POINT('Ctrl Pts',(21.5699294722998,14.7765803530981,36.9788709142835));
#45546=CARTESIAN_POINT('Ctrl Pts',(21.574651670708,14.7760538710277,36.9855130833277));
#45547=CARTESIAN_POINT('Ctrl Pts',(21.5827704530443,14.7751377477546,36.9970874419509));
#45548=CARTESIAN_POINT('Ctrl Pts',(21.5861864458013,14.7747488474186,37.0020059310054));
#45549=CARTESIAN_POINT('Ctrl Pts',(21.5932526317669,14.7739371281863,37.0122819140797));
#45550=CARTESIAN_POINT('Ctrl Pts',(21.5968988255033,14.7735141655081,37.0176420543741));
#45551=CARTESIAN_POINT('Ctrl Pts',(21.6054473550095,14.7725126870356,37.0303461712138));
#45552=CARTESIAN_POINT('Ctrl Pts',(21.6103263894723,14.7719333114294,37.0377055784089));
#45553=CARTESIAN_POINT('Ctrl Pts',(21.6263412496798,14.7700053077335,37.0622258457392));
#45554=CARTESIAN_POINT('Ctrl Pts',(21.637254306052,14.7686485210301,37.0795298443927));
#45555=CARTESIAN_POINT('Ctrl Pts',(21.6943019797833,14.7613170612082,37.1732572748959));
#45556=CARTESIAN_POINT('Ctrl Pts',(21.7353588374863,14.7551629062869,37.2526294021031));
#45557=CARTESIAN_POINT('Ctrl Pts',(21.8225714392239,14.7396916739259,37.4543840959422));
#45558=CARTESIAN_POINT('Ctrl Pts',(21.8620720898699,14.7302530221989,37.5791619877419));
#45559=CARTESIAN_POINT('Ctrl Pts',(21.8989537850175,14.7175687758162,37.7563932903388));
#45560=CARTESIAN_POINT('Ctrl Pts',(21.9072958969132,14.7140837352363,37.8062068453744));
#45561=CARTESIAN_POINT('Ctrl Pts',(21.9146555585686,14.7101733922558,37.863997989214));
#45562=CARTESIAN_POINT('Ctrl Pts',(21.9155900440249,14.7096544847598,37.8717071064323));
#45563=CARTESIAN_POINT('Ctrl Pts',(21.9170085726011,14.7088294527818,37.8840318916333));
#45564=CARTESIAN_POINT('Ctrl Pts',(21.917522543215,14.7085217375214,37.8886439292698));
#45565=CARTESIAN_POINT('Ctrl Pts',(21.9184034497825,14.7079783260974,37.8968164097645));
#45566=CARTESIAN_POINT('Ctrl Pts',(21.9187771251771,14.7077422592171,37.9003760730656));
#45567=CARTESIAN_POINT('Ctrl Pts',(21.9195500481131,14.7072418690173,37.9079417372841));
#45568=CARTESIAN_POINT('Ctrl Pts',(21.9199466633966,14.7069776933006,37.911947948867));
#45569=CARTESIAN_POINT('Ctrl Pts',(21.920988827981,14.7062627265642,37.9228219483343));
#45570=CARTESIAN_POINT('Ctrl Pts',(21.921610094989,14.7058132655294,37.9296920859859));
#45571=CARTESIAN_POINT('Ctrl Pts',(21.9245876520355,14.7035329752186,37.9647118953069));
#45572=CARTESIAN_POINT('Ctrl Pts',(21.92636244644,14.7017324132734,37.9929092408048));
#45573=CARTESIAN_POINT('Ctrl Pts',(21.92979395014,14.6964551657695,38.0767799507119));
#45574=CARTESIAN_POINT('Ctrl Pts',(21.9296602259244,14.6930512297805,38.1324996970163));
#45575=CARTESIAN_POINT('Ctrl Pts',(21.921528783017,14.6823031074037,38.3102886959911));
#45576=CARTESIAN_POINT('Ctrl Pts',(21.9043416800587,14.6751212411879,38.4316285920931));
#45577=CARTESIAN_POINT('Ctrl Pts',(21.8579861900769,14.6630375971956,38.6246315107449));
#45578=CARTESIAN_POINT('Ctrl Pts',(21.8358139212696,14.6583115960219,38.6976086160165));
#45579=CARTESIAN_POINT('Ctrl Pts',(21.8048578236406,14.6526079183648,38.78132316183));
#45580=CARTESIAN_POINT('Ctrl Pts',(21.8002055461629,14.6517696567692,38.7935221643994));
#45581=CARTESIAN_POINT('Ctrl Pts',(21.7924430507267,14.6504004804363,38.8132721348784));
#45582=CARTESIAN_POINT('Ctrl Pts',(21.7894080293417,14.6498720679008,38.8208523632807));
#45583=CARTESIAN_POINT('Ctrl Pts',(21.7839146420267,14.6489276636536,38.8343240821607));
#45584=CARTESIAN_POINT('Ctrl Pts',(21.781474968644,14.6485123034955,38.8402231029507));
#45585=CARTESIAN_POINT('Ctrl Pts',(21.7762678284143,14.6476341829824,38.8526388808497));
#45586=CARTESIAN_POINT('Ctrl Pts',(21.773493680488,14.647171202346,38.8591527160272));
#45587=CARTESIAN_POINT('Ctrl Pts',(21.7660456247167,14.6459407841036,38.876377470418));
#45588=CARTESIAN_POINT('Ctrl Pts',(21.761310197324,14.6451712731735,38.8870613087939));
#45589=CARTESIAN_POINT('Ctrl Pts',(21.738542399015,14.6415299264438,38.9371942849403));
#45590=CARTESIAN_POINT('Ctrl Pts',(21.7192812124342,14.6386164542797,38.9760682310339));
#45591=CARTESIAN_POINT('Ctrl Pts',(21.6199659301158,14.624333139912,39.1606000503536));
#45592=CARTESIAN_POINT('Ctrl Pts',(21.5226309567835,14.6123567140228,39.2961352243444));
#45593=CARTESIAN_POINT('Ctrl Pts',(21.3888352432497,14.5984740266838,39.4392406559418));
#45594=CARTESIAN_POINT('Ctrl Pts',(21.3680018272237,14.5963753064603,39.4605146057124));
#45595=CARTESIAN_POINT('Ctrl Pts',(21.3139938495377,14.5911067623355,39.5131691628338));
#45596=CARTESIAN_POINT('Ctrl Pts',(21.2801797847202,14.5879641487012,39.5438723663814));
#45597=CARTESIAN_POINT('Ctrl Pts',(21.2395234397472,14.5843925091466,39.5782359439074));
#45598=CARTESIAN_POINT('Ctrl Pts',(21.2337130268103,14.5838868033292,39.5830886809741));
#45599=CARTESIAN_POINT('Ctrl Pts',(21.2243390897565,14.5830787216351,39.5908243881961));
#45600=CARTESIAN_POINT('Ctrl Pts',(21.2207936664035,14.5827748539383,39.5937290210376));
#45601=CARTESIAN_POINT('Ctrl Pts',(21.2144666982101,14.5822357731247,39.5988748964508));
#45602=CARTESIAN_POINT('Ctrl Pts',(21.2116892443056,14.5820002100893,39.6011210784958));
#45603=CARTESIAN_POINT('Ctrl Pts',(21.2057417339669,14.5814981148765,39.6059036854004));
#45604=CARTESIAN_POINT('Ctrl Pts',(21.202569910501,14.5812317445556,39.6084378176918));
#45605=CARTESIAN_POINT('Ctrl Pts',(21.1938667916878,14.5805045990922,39.6153462870569));
#45606=CARTESIAN_POINT('Ctrl Pts',(21.1883194056939,14.5800452318888,39.6197003914577));
#45607=CARTESIAN_POINT('Ctrl Pts',(21.1588290636444,14.577624149487,39.642586938216));
#45608=CARTESIAN_POINT('Ctrl Pts',(21.1344746340417,14.5756973414608,39.6605854073017));
#45609=CARTESIAN_POINT('Ctrl Pts',(20.9773153735092,14.563645680831,39.771105017111));
#45610=CARTESIAN_POINT('Ctrl Pts',(20.8337228065082,14.5542786840768,39.8471851382568));
#45611=CARTESIAN_POINT('Ctrl Pts',(20.5986659097545,14.5390768219629,39.9360654868534));
#45612=CARTESIAN_POINT('Ctrl Pts',(20.512944586633,14.5335671611212,39.9618329857692));
#45613=CARTESIAN_POINT('Ctrl Pts',(20.4126396995163,14.5269987481531,39.9845295945417));
#45614=CARTESIAN_POINT('Ctrl Pts',(20.3994962190366,14.5261358700942,39.9873595499071));
#45615=CARTESIAN_POINT('Ctrl Pts',(20.3782973146781,14.5247401626346,39.9916925823877));
#45616=CARTESIAN_POINT('Ctrl Pts',(20.3702598682514,14.5242100710944,39.993282153064));
#45617=CARTESIAN_POINT('Ctrl Pts',(20.3559217253216,14.5232626955192,39.9960230231005));
#45618=CARTESIAN_POINT('Ctrl Pts',(20.3496249242537,14.5228460474002,39.9971942413408));
#45619=CARTESIAN_POINT('Ctrl Pts',(20.3364394807328,14.5219722946969,39.9995788896028));
#45620=CARTESIAN_POINT('Ctrl Pts',(20.3295498493853,14.5215150053206,40.0007862522197));
#45621=CARTESIAN_POINT('Ctrl Pts',(20.3115127794415,14.5203158156879,40.0038461180996));
#45622=CARTESIAN_POINT('Ctrl Pts',(20.3003554931003,14.5195720262978,40.0056381665317));
#45623=CARTESIAN_POINT('Ctrl Pts',(20.2509700869346,14.5162705064993,40.0131258165526));
#45624=CARTESIAN_POINT('Ctrl Pts',(20.212593907927,14.5136801665685,40.0177694964867));
#45625=CARTESIAN_POINT('Ctrl Pts',(20.1080143770553,14.5065485483287,40.0272466049029));
#45626=CARTESIAN_POINT('Ctrl Pts',(20.0416638302314,14.5019437042671,40.0298210146939));
#45627=CARTESIAN_POINT('Ctrl Pts',(19.8280666551264,14.4869030104798,40.0270879694292));
#45628=CARTESIAN_POINT('Ctrl Pts',(19.6815220422533,14.4762138563043,40.0083499655989));
#45629=CARTESIAN_POINT('Ctrl Pts',(19.504999816808,14.4636230088017,39.9648620483704));
#45630=CARTESIAN_POINT('Ctrl Pts',(19.4716868822015,14.4612623700115,39.955699666514));
#45631=CARTESIAN_POINT('Ctrl Pts',(19.4319781748459,14.4584813264809,39.9436220286079));
#45632=CARTESIAN_POINT('Ctrl Pts',(19.4253316428006,14.4580169493766,39.9415610934912));
#45633=CARTESIAN_POINT('Ctrl Pts',(19.4144553897955,14.4572590554553,39.938124002261));
#45634=CARTESIAN_POINT('Ctrl Pts',(19.410219088809,14.4569643559199,39.9367691243071));
#45635=CARTESIAN_POINT('Ctrl Pts',(19.4026063985318,14.4564357252254,39.934305337392));
#45636=CARTESIAN_POINT('Ctrl Pts',(19.3992283725346,14.4562014928851,39.9332017450712));
#45637=CARTESIAN_POINT('Ctrl Pts',(19.3918567246019,14.4556910891093,39.9307708822247));
#45638=CARTESIAN_POINT('Ctrl Pts',(19.3878643995931,14.4554151388284,39.9294398798986));
#45639=CARTESIAN_POINT('Ctrl Pts',(19.3765485806149,14.4546342465418,39.9256261066141));
#45640=CARTESIAN_POINT('Ctrl Pts',(19.3692355115153,14.4541310797432,39.9231123164689));
#45641=CARTESIAN_POINT('Ctrl Pts',(19.3230943259983,14.4509647161153,39.9069408949773));
#45642=CARTESIAN_POINT('Ctrl Pts',(19.2846932902263,14.4483668321885,39.8920863769269));
#45643=CARTESIAN_POINT('Ctrl Pts',(19.1488116232062,14.4392097191443,39.8344590422087));
#45644=CARTESIAN_POINT('Ctrl Pts',(19.0544282360465,14.4329084162657,39.7848642589556));
#45645=CARTESIAN_POINT('Ctrl Pts',(18.8674306180326,14.4196605771262,39.6659165388674));
#45646=CARTESIAN_POINT('Ctrl Pts',(18.7759920320964,14.412723800333,39.5955293663914));
#45647=CARTESIAN_POINT('Ctrl Pts',(18.6719170038453,14.4037892782618,39.4994427201339));
#45648=CARTESIAN_POINT('Ctrl Pts',(18.6528254044976,14.4021029686193,39.4810738114305));
#45649=CARTESIAN_POINT('Ctrl Pts',(18.6269918736274,14.3997509550951,39.4551727174637));
#45650=CARTESIAN_POINT('Ctrl Pts',(18.619921237454,14.3990996853729,39.4479714433529));
#45651=CARTESIAN_POINT('Ctrl Pts',(18.6086969853665,14.3980535109125,39.4363589277012));
#45652=CARTESIAN_POINT('Ctrl Pts',(18.6045070161338,14.3976601815787,39.4319829551337));
#45653=CARTESIAN_POINT('Ctrl Pts',(18.5959069765196,14.3968470188198,39.4229160183698));
#45654=CARTESIAN_POINT('Ctrl Pts',(18.5914996431544,14.3964270758429,39.4182225735173));
#45655=CARTESIAN_POINT('Ctrl Pts',(18.582820414027,14.3955936485318,39.408886694315));
#45656=CARTESIAN_POINT('Ctrl Pts',(18.5785476311178,14.3951802094035,39.4042451912353));
#45657=CARTESIAN_POINT('Ctrl Pts',(18.5647397035229,14.3938338075739,39.3890972585624));
#45658=CARTESIAN_POINT('Ctrl Pts',(18.5552978637193,14.3928969651113,39.3785067774203));
#45659=CARTESIAN_POINT('Ctrl Pts',(18.4906990553966,14.3863725773239,39.3044198836624));
#45660=CARTESIAN_POINT('Ctrl Pts',(18.439636956027,14.3806199794427,39.237488567998));
#45661=CARTESIAN_POINT('Ctrl Pts',(18.3562149296603,14.3700746907748,39.1119085980691));
#45662=CARTESIAN_POINT('Ctrl Pts',(18.3222267444621,14.3653383569757,39.0544969018628));
#45663=CARTESIAN_POINT('Ctrl Pts',(18.2357481980994,14.3520505016559,38.889475389284));
#45664=CARTESIAN_POINT('Ctrl Pts',(18.1901888144504,14.3434730023865,38.778560681935));
#45665=CARTESIAN_POINT('Ctrl Pts',(18.1509233321687,14.3343709194131,38.6501559779213));
#45666=CARTESIAN_POINT('Ctrl Pts',(18.1468085956264,14.3333877552602,38.6361322354116));
#45667=CARTESIAN_POINT('Ctrl Pts',(18.1413352222397,14.3320390628001,38.616661664716));
#45668=CARTESIAN_POINT('Ctrl Pts',(18.1398405145446,14.3316662218134,38.6112540684305));
#45669=CARTESIAN_POINT('Ctrl Pts',(18.1374860604111,14.3310716438687,38.6025890274246));
#45670=CARTESIAN_POINT('Ctrl Pts',(18.1366112335004,14.33084905443,38.5993357697672));
#45671=CARTESIAN_POINT('Ctrl Pts',(18.1348052495487,14.3303860587598,38.5925489342785));
#45672=CARTESIAN_POINT('Ctrl Pts',(18.1338756065242,14.3301457457831,38.5890149876141));
#45673=CARTESIAN_POINT('Ctrl Pts',(18.1316519191684,14.3295660311852,38.5804631712082));
#45674=CARTESIAN_POINT('Ctrl Pts',(18.1303680286128,14.3292272086903,38.5754426391592));
#45675=CARTESIAN_POINT('Ctrl Pts',(18.1276754703403,14.3285076133287,38.5647340628571));
#45676=CARTESIAN_POINT('Ctrl Pts',(18.1262724533015,14.3281271521443,38.5590446344207));
#45677=CARTESIAN_POINT('Ctrl Pts',(18.1224390156797,14.3270718043661,38.5431890802928));
#45678=CARTESIAN_POINT('Ctrl Pts',(18.12006522082,14.3263998744108,38.5330092929739));
#45679=CARTESIAN_POINT('Ctrl Pts',(18.0867292803845,14.3166796244212,38.3846076511583));
#45680=CARTESIAN_POINT('Ctrl Pts',(18.0709965071608,14.3083550520962,38.2433903014528));
#45681=CARTESIAN_POINT('Ctrl Pts',(18.070870759842,14.299879738933,38.1017122113181));
#45682=CARTESIAN_POINT('Ctrl Pts',(18.0708707591309,14.2998796909909,38.1017114098911));
#45683=CARTESIAN_POINT('Ctrl Pts',(18.0707878522312,14.2942891859856,38.0082573955159));
#45684=CARTESIAN_POINT('Ctrl Pts',(18.0774957121742,14.2886562223612,37.9149266385927));
#45685=CARTESIAN_POINT('Ctrl Pts',(18.0959050454575,14.2806751915482,37.7883016683291));
#45686=CARTESIAN_POINT('Ctrl Pts',(18.1017851561007,14.2784985604903,37.7542925728336));
#45687=CARTESIAN_POINT('Ctrl Pts',(18.1106084993665,14.2756328702757,37.7103215921296));
#45688=CARTESIAN_POINT('Ctrl Pts',(18.1127245697726,14.2749695858103,37.7001988644041));
#45689=CARTESIAN_POINT('Ctrl Pts',(18.1164318309083,14.2738462128772,37.6831498987801));
#45690=CARTESIAN_POINT('Ctrl Pts',(18.1179801059569,14.2733874786639,37.6762144755653));
#45691=CARTESIAN_POINT('Ctrl Pts',(18.1211162326129,14.272478298117,37.6625225538848));
#45692=CARTESIAN_POINT('Ctrl Pts',(18.1227022986039,14.272027914496,37.6557657538437));
#45693=CARTESIAN_POINT('Ctrl Pts',(18.1258259926136,14.2711585653936,37.6427740335848));
#45694=CARTESIAN_POINT('Ctrl Pts',(18.1273583615969,14.2707397730916,37.6365379338302));
#45695=CARTESIAN_POINT('Ctrl Pts',(18.1309444898016,14.2697768913639,37.6222520826934));
#45696=CARTESIAN_POINT('Ctrl Pts',(18.1330191570007,14.2692321384901,37.6142077594996));
#45697=CARTESIAN_POINT('Ctrl Pts',(18.1386870477191,14.2677757338819,37.5928037452177));
#45698=CARTESIAN_POINT('Ctrl Pts',(18.1423720784214,14.2668611518366,37.5794690832454));
#45699=CARTESIAN_POINT('Ctrl Pts',(18.1766362955734,14.2586335718002,37.4604805375846));
#45700=CARTESIAN_POINT('Ctrl Pts',(18.2160503423616,14.2510306864612,37.3576009145721));
#45701=CARTESIAN_POINT('Ctrl Pts',(18.2955300035121,14.2381418447551,37.1936062870507));
#45702=CARTESIAN_POINT('Ctrl Pts',(18.3306854640465,14.2329690411936,37.1303835792582));
#45703=CARTESIAN_POINT('Ctrl Pts',(18.4143809391876,14.2218102555178,36.9979688626955));
#45704=CARTESIAN_POINT('Ctrl Pts',(18.4640924114812,14.21584385365,36.9296789884445));
#45705=CARTESIAN_POINT('Ctrl Pts',(18.5286630372816,14.2089912893424,36.8522094638793));
#45706=CARTESIAN_POINT('Ctrl Pts',(18.5393673610844,14.2078817389792,36.839696061038));
#45707=CARTESIAN_POINT('Ctrl Pts',(18.5531202473567,14.2064908289844,36.8240294994696));
#45708=CARTESIAN_POINT('Ctrl Pts',(18.556020703883,14.2061993959142,36.8207480583815));
#45709=CARTESIAN_POINT('Ctrl Pts',(18.5616824335083,14.2056342577341,36.8143864319971));
#45710=CARTESIAN_POINT('Ctrl Pts',(18.5644424865603,14.2053604675247,36.8113051972182));
#45711=CARTESIAN_POINT('Ctrl Pts',(18.5695964641611,14.2048524173568,36.8055885672839));
#45712=CARTESIAN_POINT('Ctrl Pts',(18.5719877504815,14.204617976235,36.802950946174));
#45713=CARTESIAN_POINT('Ctrl Pts',(18.5774465648602,14.204085677847,36.7969631957744));
#45714=CARTESIAN_POINT('Ctrl Pts',(18.580518626907,14.2037881664674,36.7936172760333));
#45715=CARTESIAN_POINT('Ctrl Pts',(18.5899510050457,14.2028808280875,36.7834166079093));
#45716=CARTESIAN_POINT('Ctrl Pts',(18.5963494829116,14.2022737972977,36.776597101819));
#45717=CARTESIAN_POINT('Ctrl Pts',(18.6601697575652,14.1962989662403,36.7095609610465));
#45718=CARTESIAN_POINT('Ctrl Pts',(18.7213889777377,14.1912000113379,36.6530641389772));
#45719=CARTESIAN_POINT('Ctrl Pts',(18.8594388694836,14.1804889145527,36.5412909930582));
#45720=CARTESIAN_POINT('Ctrl Pts',(18.937065336087,14.1749110020345,36.4873550260979));
#45721=CARTESIAN_POINT('Ctrl Pts',(19.0762875667289,14.1651671985223,36.4050572635616));
#45722=CARTESIAN_POINT('Ctrl Pts',(19.1359954373219,14.1610635279119,36.3738567528303));
#45723=CARTESIAN_POINT('Ctrl Pts',(19.2207523208231,14.1552446400369,36.3350677012214));
#45724=CARTESIAN_POINT('Ctrl Pts',(19.2445097757659,14.1536145492692,36.3247683557207));
#45725=CARTESIAN_POINT('Ctrl Pts',(19.2861234294359,14.1507560788408,36.3077146081867));
#45726=CARTESIAN_POINT('Ctrl Pts',(19.3038862197052,14.1495349620833,36.3007411950635));
#45727=CARTESIAN_POINT('Ctrl Pts',(19.3297689470991,14.1477529355454,36.2910206514505));
#45728=CARTESIAN_POINT('Ctrl Pts',(19.3378087207323,14.1471990261802,36.2880621827648));
#45729=CARTESIAN_POINT('Ctrl Pts',(19.3519522795343,14.1462238215299,36.2829643539803));
#45730=CARTESIAN_POINT('Ctrl Pts',(19.3580476587169,14.1458032937396,36.2808019413121));
#45731=CARTESIAN_POINT('Ctrl Pts',(19.3698278172143,14.1449900364659,36.2766893583239));
#45732=CARTESIAN_POINT('Ctrl Pts',(19.3755110700828,14.1445974497822,36.2747350189503));
#45733=CARTESIAN_POINT('Ctrl Pts',(19.3854984955816,14.1439070924976,36.2713526795806));
#45734=CARTESIAN_POINT('Ctrl Pts',(19.3897987554653,14.1436097021173,36.2699132365454));
#45735=CARTESIAN_POINT('Ctrl Pts',(19.3941040087558,14.1433118141013,36.2684889831906));
#45736=CARTESIAN_POINT('Ctrl Pts',(19.3941039465104,13.9716756753762,36.2684890037825));
#45737=CARTESIAN_POINT('Ctrl Pts',(19.2849119469309,13.9786750649394,36.3046116379105));
#45738=CARTESIAN_POINT('Ctrl Pts',(19.179127144956,13.9854371548148,36.3504403871307));
#45739=CARTESIAN_POINT('Ctrl Pts',(18.9998767884834,13.9977430294354,36.4479678007505));
#45740=CARTESIAN_POINT('Ctrl Pts',(18.9247759297133,14.0031957124574,36.4958344384174));
#45741=CARTESIAN_POINT('Ctrl Pts',(18.8368294460731,14.0101385072896,36.5608463898901));
#45742=CARTESIAN_POINT('Ctrl Pts',(18.8206024090689,14.0114442625977,36.5732449951234));
#45743=CARTESIAN_POINT('Ctrl Pts',(18.7976504505213,14.0133285833006,36.5913661899096));
#45744=CARTESIAN_POINT('Ctrl Pts',(18.7907628623517,14.0138989810789,36.5968812579279));
#45745=CARTESIAN_POINT('Ctrl Pts',(18.7788818245945,14.0148916525,36.6065292200839));
#45746=CARTESIAN_POINT('Ctrl Pts',(18.7738708813281,14.0153130552183,36.6106404223933));
#45747=CARTESIAN_POINT('Ctrl Pts',(18.7642692623827,14.0161258502759,36.6185993184577));
#45748=CARTESIAN_POINT('Ctrl Pts',(18.7596755950149,14.0165170896234,36.6224432991564));
#45749=CARTESIAN_POINT('Ctrl Pts',(18.7488698310427,14.0174430878813,36.6315714625633));
#45750=CARTESIAN_POINT('Ctrl Pts',(18.7426732333181,14.0179785804158,36.6368737349178));
#45751=CARTESIAN_POINT('Ctrl Pts',(18.721113582958,14.0198575942255,36.6555598873457));
#45752=CARTESIAN_POINT('Ctrl Pts',(18.7059295514659,14.0212094708056,36.6691473426178));
#45753=CARTESIAN_POINT('Ctrl Pts',(18.5669725708207,14.0338541316554,36.7975144060723));
#45754=CARTESIAN_POINT('Ctrl Pts',(18.4585744779452,14.0458620437653,36.9278140733033));
#45755=CARTESIAN_POINT('Ctrl Pts',(18.3634323532194,14.0585718979818,37.0785891304716));
#45756=CARTESIAN_POINT('Ctrl Pts',(18.3583941275299,14.0592525663647,37.0867063664525));
#45757=CARTESIAN_POINT('Ctrl Pts',(18.3060161409061,14.0664081486044,37.1725101315125));
#45758=CARTESIAN_POINT('Ctrl Pts',(18.2641616587065,14.0728230564806,37.2534256089593));
#45759=CARTESIAN_POINT('Ctrl Pts',(18.2246119917548,14.079539603185,37.3452676240532));
#45760=CARTESIAN_POINT('Ctrl Pts',(18.2211105494007,14.0801409671818,37.3535578593079));
#45761=CARTESIAN_POINT('Ctrl Pts',(18.215956038518,14.0810361589589,37.3660042914641));
#45762=CARTESIAN_POINT('Ctrl Pts',(18.2142592629757,14.0813325041069,37.3701420838388));
#45763=CARTESIAN_POINT('Ctrl Pts',(18.2112394801778,14.0818628783071,37.3775797632312));
#45764=CARTESIAN_POINT('Ctrl Pts',(18.2099111980462,14.0820972177378,37.3808774252267));
#45765=CARTESIAN_POINT('Ctrl Pts',(18.2070377429455,14.0826064579249,37.3880685095928));
#45766=CARTESIAN_POINT('Ctrl Pts',(18.2054961356777,14.0828811451278,37.391963289079));
#45767=CARTESIAN_POINT('Ctrl Pts',(18.2012537814394,14.0836412809253,37.4027842066803));
#45768=CARTESIAN_POINT('Ctrl Pts',(18.1985803299087,14.0841251377074,37.4097210724496));
#45769=CARTESIAN_POINT('Ctrl Pts',(18.184671742712,14.0866691850657,37.4464411810257));
#45770=CARTESIAN_POINT('Ctrl Pts',(18.1741342000889,14.0886910511325,37.4764856250123));
#45771=CARTESIAN_POINT('Ctrl Pts',(18.1025222395381,14.1032654569102,37.6980808331471));
#45772=CARTESIAN_POINT('Ctrl Pts',(18.0709770307598,14.1147043860589,37.8978838092169));
#45773=CARTESIAN_POINT('Ctrl Pts',(18.0708429566733,14.1303155216926,38.1504268368755));
#45774=CARTESIAN_POINT('Ctrl Pts',(18.072873971112,14.1335455015647,38.2018543337162));
#45775=CARTESIAN_POINT('Ctrl Pts',(18.077970987111,14.1376569892982,38.2658613695612));
#45776=CARTESIAN_POINT('Ctrl Pts',(18.0791106073354,14.1384781995256,38.278576170833));
#45777=CARTESIAN_POINT('Ctrl Pts',(18.0811093846322,14.1397812248853,38.2986354069124));
#45778=CARTESIAN_POINT('Ctrl Pts',(18.0818847343445,14.1402604246902,38.3059879699693));
#45779=CARTESIAN_POINT('Ctrl Pts',(18.083403997203,14.1411533406297,38.3196419324309));
#45780=CARTESIAN_POINT('Ctrl Pts',(18.0841367736193,14.1415667032452,38.3259444901209));
#45781=CARTESIAN_POINT('Ctrl Pts',(18.0858282114475,14.1424841983547,38.3398922429677));
#45782=CARTESIAN_POINT('Ctrl Pts',(18.0868016064441,14.1429887855927,38.3475355092181));
#45783=CARTESIAN_POINT('Ctrl Pts',(18.0897481392812,14.144451804665,38.3696158497815));
#45784=CARTESIAN_POINT('Ctrl Pts',(18.0918390585632,14.1454139053866,38.3840364055957));
#45785=CARTESIAN_POINT('Ctrl Pts',(18.1096941016752,14.1530757191918,38.4980660666897));
#45786=CARTESIAN_POINT('Ctrl Pts',(18.1330810844507,14.160016752213,38.5963071742129));
#45787=CARTESIAN_POINT('Ctrl Pts',(18.1918465668368,14.1735033709713,38.7784770602139));
#45788=CARTESIAN_POINT('Ctrl Pts',(18.2256981268137,14.179998813167,38.8626281187381));
#45789=CARTESIAN_POINT('Ctrl Pts',(18.3032684230973,14.1926079821378,39.0220416301474));
#45790=CARTESIAN_POINT('Ctrl Pts',(18.3464191710355,14.1987106665962,39.0973630188985));
#45791=CARTESIAN_POINT('Ctrl Pts',(18.3996924673201,14.2051691639591,39.1773329050062));
#45792=CARTESIAN_POINT('Ctrl Pts',(18.4049451997717,14.2057957453093,39.1850947333449));
#45793=CARTESIAN_POINT('Ctrl Pts',(18.4128298534666,14.2067208950661,39.1965647050211));
#45794=CARTESIAN_POINT('Ctrl Pts',(18.4154185587463,14.2070222302401,39.2003021782356));
#45795=CARTESIAN_POINT('Ctrl Pts',(18.4200581850617,14.2075579712121,39.2069503584316));
#45796=CARTESIAN_POINT('Ctrl Pts',(18.4221039696758,14.2077927151483,39.2098645650853));
#45797=CARTESIAN_POINT('Ctrl Pts',(18.426542281998,14.2082987874333,39.2161498348777));
#45798=CARTESIAN_POINT('Ctrl Pts',(18.4289375744055,14.2085699239158,39.2195188698347));
#45799=CARTESIAN_POINT('Ctrl Pts',(18.4356443203041,14.2093236737108,39.2288881498322));
#45800=CARTESIAN_POINT('Ctrl Pts',(18.4399795001487,14.2098047020793,39.2348714428392));
#45801=CARTESIAN_POINT('Ctrl Pts',(18.465240640136,14.2125731041899,39.269317875493));
#45802=CARTESIAN_POINT('Ctrl Pts',(18.4869124628092,14.2148126085949,39.297228914235));
#45803=CARTESIAN_POINT('Ctrl Pts',(18.5602094546646,14.2220174581278,39.3864556243148));
#45804=CARTESIAN_POINT('Ctrl Pts',(18.6148923358614,14.2268327196856,39.4451556761213));
#45805=CARTESIAN_POINT('Ctrl Pts',(18.7853430230445,14.2408758103055,39.6066765519526));
#45806=CARTESIAN_POINT('Ctrl Pts',(18.9099853077166,14.2500390747562,39.6991646343082));
#45807=CARTESIAN_POINT('Ctrl Pts',(19.0631082948539,14.2612103368516,39.7864886559279));
#45808=CARTESIAN_POINT('Ctrl Pts',(19.0820685138739,14.2625910643644,39.7968829602451));
#45809=CARTESIAN_POINT('Ctrl Pts',(19.1085988977558,14.2645214364564,39.8108525872945));
#45810=CARTESIAN_POINT('Ctrl Pts',(19.1160241157818,14.2650615233667,39.8147008873421));
#45811=CARTESIAN_POINT('Ctrl Pts',(19.1288575211868,14.2659947904957,39.8212466006609));
#45812=CARTESIAN_POINT('Ctrl Pts',(19.1342538362738,14.2663871608946,39.8239671276723));
#45813=CARTESIAN_POINT('Ctrl Pts',(19.1454330171029,14.2671999323132,39.829537334185));
#45814=CARTESIAN_POINT('Ctrl Pts',(19.1512175557214,14.267620449934,39.8323834677098));
#45815=CARTESIAN_POINT('Ctrl Pts',(19.1647647741944,14.2686052495256,39.8389648890694));
#45816=CARTESIAN_POINT('Ctrl Pts',(19.172538374529,14.2691703121474,39.8426772570269));
#45817=CARTESIAN_POINT('Ctrl Pts',(19.1977521749771,14.2710031683828,39.8545116441086));
#45818=CARTESIAN_POINT('Ctrl Pts',(19.2152886236255,14.2722780537122,39.8624246629341));
#45819=CARTESIAN_POINT('Ctrl Pts',(19.3058049725359,14.2788612522324,39.9016498477938));
#45820=CARTESIAN_POINT('Ctrl Pts',(19.3805405727024,14.2843104070488,39.9286924317987));
#45821=CARTESIAN_POINT('Ctrl Pts',(19.5604893664041,14.2974449078329,39.9815069222736));
#45822=CARTESIAN_POINT('Ctrl Pts',(19.6666304157314,14.3052094770627,40.0031815398957));
#45823=CARTESIAN_POINT('Ctrl Pts',(19.8567509171756,14.3188138762382,40.0256069441313));
#45824=CARTESIAN_POINT('Ctrl Pts',(19.9400391728748,14.3246680119929,40.0299975469649));
#45825=CARTESIAN_POINT('Ctrl Pts',(20.0327102416572,14.3308969669913,40.0288753325193));
#45826=CARTESIAN_POINT('Ctrl Pts',(20.0420603879069,14.3315221784472,40.0286941024248));
#45827=CARTESIAN_POINT('Ctrl Pts',(20.0559498356314,14.3324457038719,40.0283238332691));
#45828=CARTESIAN_POINT('Ctrl Pts',(20.0604902125199,14.3327467707857,40.028186745442));
#45829=CARTESIAN_POINT('Ctrl Pts',(20.0685883392662,14.3332822204649,40.0279136059334));
#45830=CARTESIAN_POINT('Ctrl Pts',(20.0721462277512,14.3335169398803,40.0277837417011));
#45831=CARTESIAN_POINT('Ctrl Pts',(20.0798371326405,14.3340231698315,40.027481698928));
#45832=CARTESIAN_POINT('Ctrl Pts',(20.0839699517125,14.3342944873828,40.027306077263));
#45833=CARTESIAN_POINT('Ctrl Pts',(20.0954959053672,14.3350492527391,40.0267791440044));
#45834=CARTESIAN_POINT('Ctrl Pts',(20.1028877282419,14.335531108659,40.0263985717944));
#45835=CARTESIAN_POINT('Ctrl Pts',(20.1457587995633,14.3383140142852,40.0239438639971));
#45836=CARTESIAN_POINT('Ctrl Pts',(20.1811801236259,14.3405666060866,40.0209320056448));
#45837=CARTESIAN_POINT('Ctrl Pts',(20.2969657317302,14.3478353769175,40.0078551131425));
#45838=CARTESIAN_POINT('Ctrl Pts',(20.3767858369393,14.3526984103629,39.9937091658136));
#45839=CARTESIAN_POINT('Ctrl Pts',(20.6046334064205,14.3667185025429,39.9383468707799));
#45840=CARTESIAN_POINT('Ctrl Pts',(20.7489038395766,14.3758169935013,39.8844432042381));
#45841=CARTESIAN_POINT('Ctrl Pts',(20.9045364980838,14.3869171605174,39.8040619396936));
#45842=CARTESIAN_POINT('Ctrl Pts',(20.9236452280323,14.3883027039898,39.7937806242355));
#45843=CARTESIAN_POINT('Ctrl Pts',(20.9498835484393,14.3902387471173,39.7790872371453));
#45844=CARTESIAN_POINT('Ctrl Pts',(20.9571643883838,14.3907796143533,39.7749474724691));
#45845=CARTESIAN_POINT('Ctrl Pts',(20.9696546580332,14.3917138681886,39.7677376776728));
#45846=CARTESIAN_POINT('Ctrl Pts',(20.9748770783563,14.3921064409661,39.7646903009539));
#45847=CARTESIAN_POINT('Ctrl Pts',(20.9856363184326,14.3929192914005,39.7583440966246));
#45848=CARTESIAN_POINT('Ctrl Pts',(20.9911710989411,14.3933396841547,39.7550419770992));
#45849=CARTESIAN_POINT('Ctrl Pts',(21.0040551082252,14.3943236000621,39.7472674069181));
#45850=CARTESIAN_POINT('Ctrl Pts',(21.0113911258097,14.3948878996797,39.7427734344215));
#45851=CARTESIAN_POINT('Ctrl Pts',(21.0349803188844,14.3967157750897,39.7281050269173));
#45852=CARTESIAN_POINT('Ctrl Pts',(21.0511115059862,14.3979863888938,39.717737554811));
#45853=CARTESIAN_POINT('Ctrl Pts',(21.1328290246359,14.4045317839027,39.6634796864818));
#45854=CARTESIAN_POINT('Ctrl Pts',(21.1958240152582,14.4099455905328,39.6158404885852));
#45855=CARTESIAN_POINT('Ctrl Pts',(21.3366507447113,14.422934280803,39.4950888733766));
#45856=CARTESIAN_POINT('Ctrl Pts',(21.411687329708,14.4305847476165,39.419107442892));
#45857=CARTESIAN_POINT('Ctrl Pts',(21.5348377060535,14.4442367306801,39.2717978999963));
#45858=CARTESIAN_POINT('Ctrl Pts',(21.5852127261009,14.4502449039189,39.2026972998371));
#45859=CARTESIAN_POINT('Ctrl Pts',(21.63584897827,14.4566163001405,39.1225597246511));
#45860=CARTESIAN_POINT('Ctrl Pts',(21.640794139209,14.4572424583278,39.1146057715237));
#45861=CARTESIAN_POINT('Ctrl Pts',(21.6480529394401,14.4581671063632,39.1027386119726));
#45862=CARTESIAN_POINT('Ctrl Pts',(21.6504109004741,14.4584683587056,39.0988528799499));
#45863=CARTESIAN_POINT('Ctrl Pts',(21.6545914694076,14.4590040097025,39.0919084147454));
#45864=CARTESIAN_POINT('Ctrl Pts',(21.6564193589304,14.4592387460354,39.0888529425354));
#45865=CARTESIAN_POINT('Ctrl Pts',(21.6603515949405,14.459744866858,39.082238378688));
#45866=CARTESIAN_POINT('Ctrl Pts',(21.6624529575637,14.4600160591368,39.0786775853519));
#45867=CARTESIAN_POINT('Ctrl Pts',(21.6682795415641,14.4607701218344,39.0687314267732));
#45868=CARTESIAN_POINT('Ctrl Pts',(21.6719795808526,14.461251405172,39.0623312795175));
#45869=CARTESIAN_POINT('Ctrl Pts',(21.6931803477115,14.4640242651393,39.0251678264176));
#45870=CARTESIAN_POINT('Ctrl Pts',(21.7098699129593,14.4662677919328,38.9939465651123));
#45871=CARTESIAN_POINT('Ctrl Pts',(21.7616274728153,14.4734922405503,38.8903636615829));
#45872=CARTESIAN_POINT('Ctrl Pts',(21.7930350695368,14.4783221433256,38.8162635483253));
#45873=CARTESIAN_POINT('Ctrl Pts',(21.87095410656,14.492358105124,38.5948576064915));
#45874=CARTESIAN_POINT('Ctrl Pts',(21.9045255013967,14.5015014702645,38.4436999878402));
#45875=CARTESIAN_POINT('Ctrl Pts',(21.9218681088986,14.5126509071936,38.2686240364368));
#45876=CARTESIAN_POINT('Ctrl Pts',(21.9236390787485,14.5140331464573,38.2470500881662));
#45877=CARTESIAN_POINT('Ctrl Pts',(21.9255907247164,14.5159652992896,38.2171022028006));
#45878=CARTESIAN_POINT('Ctrl Pts',(21.9260805047094,14.516505631759,38.2087494863649));
#45879=CARTESIAN_POINT('Ctrl Pts',(21.9268304787907,14.5174392093566,38.194357812878));
#45880=CARTESIAN_POINT('Ctrl Pts',(21.927116658865,14.5178316434063,38.1883202841593));
#45881=CARTESIAN_POINT('Ctrl Pts',(21.9276494046836,14.5186444394878,38.175841174625));
#45882=CARTESIAN_POINT('Ctrl Pts',(21.9278920657791,14.5190649176471,38.1693995112679));
#45883=CARTESIAN_POINT('Ctrl Pts',(21.9283834510545,14.5200494383605,38.1543504477407));
#45884=CARTESIAN_POINT('Ctrl Pts',(21.9286068373525,14.5206142602441,38.145742412877));
#45885=CARTESIAN_POINT('Ctrl Pts',(21.9291425154037,14.5224455439847,38.1179182901047));
#45886=CARTESIAN_POINT('Ctrl Pts',(21.9292252779906,14.5237190805797,38.0986994518787));
#45887=CARTESIAN_POINT('Ctrl Pts',(21.9281779893899,14.5302903299362,38.0002319835502));
#45888=CARTESIAN_POINT('Ctrl Pts',(21.9224522138208,14.5357283088537,37.9211184758602));
#45889=CARTESIAN_POINT('Ctrl Pts',(21.8975070706028,14.5488203043225,37.7358418939755));
#45890=CARTESIAN_POINT('Ctrl Pts',(21.8742202824952,14.5565525783041,37.6304897175076));
#45891=CARTESIAN_POINT('Ctrl Pts',(21.8173686545484,14.5701718826056,37.4475001091928));
#45892=CARTESIAN_POINT('Ctrl Pts',(21.7872644691981,14.5760709150314,37.3690594171895));
#45893=CARTESIAN_POINT('Ctrl Pts',(21.7482280493922,14.5823414435496,37.2843231155787));
#45894=CARTESIAN_POINT('Ctrl Pts',(21.744251464342,14.5829669593776,37.2758538174195));
#45895=CARTESIAN_POINT('Ctrl Pts',(21.738252512324,14.5838908457376,37.2633152316894));
#45896=CARTESIAN_POINT('Ctrl Pts',(21.7362772053697,14.5841919722831,37.2592237721688));
#45897=CARTESIAN_POINT('Ctrl Pts',(21.7327282001407,14.5847274866882,37.2519385534095));
#45898=CARTESIAN_POINT('Ctrl Pts',(21.7311601013199,14.5849622115285,37.2487421441923));
#45899=CARTESIAN_POINT('Ctrl Pts',(21.7277512648392,14.585468406314,37.2418419556257));
#45900=CARTESIAN_POINT('Ctrl Pts',(21.7259074671023,14.5857396835238,37.2381397572271));
#45901=CARTESIAN_POINT('Ctrl Pts',(21.7207322006901,14.5864942225824,37.2278314447371));
#45902=CARTESIAN_POINT('Ctrl Pts',(21.7173745699723,14.586975894094,37.2212384362011));
#45903=CARTESIAN_POINT('Ctrl Pts',(21.6976906043734,14.5897555591137,37.1831309449869));
#45904=CARTESIAN_POINT('Ctrl Pts',(21.6805337756067,14.5920052265549,37.1520501765005));
#45905=CARTESIAN_POINT('Ctrl Pts',(21.6215479739906,14.5992596758385,37.0518341829809));
#45906=CARTESIAN_POINT('Ctrl Pts',(21.5762314243651,14.6041120008986,36.9848470547321));
#45907=CARTESIAN_POINT('Ctrl Pts',(21.4328718209787,14.6181369482902,36.799208226113));
#45908=CARTESIAN_POINT('Ctrl Pts',(21.3247028410053,14.6272496872541,36.689206954274));
#45909=CARTESIAN_POINT('Ctrl Pts',(21.1876939987385,14.6383656561559,36.5796724922583));
#45910=CARTESIAN_POINT('Ctrl Pts',(21.1705305053323,14.6397503221424,36.5664188833777));
#45911=CARTESIAN_POINT('Ctrl Pts',(21.1464351286698,14.6416853323904,36.5484526549187));
#45912=CARTESIAN_POINT('Ctrl Pts',(21.1396900432251,14.6422260578762,36.543491320283));
#45913=CARTESIAN_POINT('Ctrl Pts',(21.1280194086006,14.6431601324464,36.535023538784));
#45914=CARTESIAN_POINT('Ctrl Pts',(21.12310924136,14.6435526684364,36.5314960181971));
#45915=CARTESIAN_POINT('Ctrl Pts',(21.1129304456644,14.644365504378,36.5242557560328));
#45916=CARTESIAN_POINT('Ctrl Pts',(21.1076596365849,14.6447859196996,36.5205462250903));
#45917=CARTESIAN_POINT('Ctrl Pts',(21.0953085661789,14.6457699955869,36.5119459231924));
#45918=CARTESIAN_POINT('Ctrl Pts',(21.0882140184412,14.6463344333748,36.5070760055687));
#45919=CARTESIAN_POINT('Ctrl Pts',(21.0651965169169,14.6481632100783,36.4915016130267));
#45920=CARTESIAN_POINT('Ctrl Pts',(21.0491467967063,14.6494345967078,36.4809874507779));
#45921=CARTESIAN_POINT('Ctrl Pts',(20.9662173885793,14.6559868226076,36.4284113999003));
#45922=CARTESIAN_POINT('Ctrl Pts',(20.8969644355208,14.6614070145264,36.3902525287703));
#45923=CARTESIAN_POINT('Ctrl Pts',(20.7505318002892,14.6727516258303,36.3209163305776));
#45924=CARTESIAN_POINT('Ctrl Pts',(20.6732765741397,14.6786763520575,36.2902669214684));
#45925=CARTESIAN_POINT('Ctrl Pts',(20.4904244559541,14.6923888466525,36.2310574632859));
#45926=CARTESIAN_POINT('Ctrl Pts',(20.3838754813475,14.7001553189174,36.2062978663796));
#45927=CARTESIAN_POINT('Ctrl Pts',(20.2667117797668,14.7081092172196,36.1893740372918));
#45928=CARTESIAN_POINT('Ctrl Pts',(20.2576212725021,14.7087225039489,36.1881270881732));
#45929=CARTESIAN_POINT('Ctrl Pts',(20.2440521357221,14.7096318748217,36.1863643427277));
#45930=CARTESIAN_POINT('Ctrl Pts',(20.2395801971605,14.7099305929198,36.1857993302979));
#45931=CARTESIAN_POINT('Ctrl Pts',(20.2315752822523,14.7104635052454,36.1848164314224));
#45932=CARTESIAN_POINT('Ctrl Pts',(20.2280431049758,14.7106980230727,36.1843926405278));
#45933=CARTESIAN_POINT('Ctrl Pts',(20.2203761786501,14.7112056932662,36.1834942689287));
#45934=CARTESIAN_POINT('Ctrl Pts',(20.2162410696391,14.7114786426324,36.1830232974927));
#45935=CARTESIAN_POINT('Ctrl Pts',(20.2046323551703,14.7122425787989,36.1817391545809));
#45936=CARTESIAN_POINT('Ctrl Pts',(20.1971553724795,14.7127319104081,36.1809562705672));
#45937=CARTESIAN_POINT('Ctrl Pts',(20.1523264217291,14.7156505593776,36.1765271864679));
#45938=CARTESIAN_POINT('Ctrl Pts',(20.1148762269242,14.718025725202,36.1739275956097));
#45939=CARTESIAN_POINT('Ctrl Pts',(19.9137778933238,14.730555823681,36.1658556994479));
#45940=CARTESIAN_POINT('Ctrl Pts',(19.7500020003764,14.7400188738409,36.1801406301291));
#45941=CARTESIAN_POINT('Ctrl Pts',(19.5237833685961,14.7540856011064,36.2293449190564));
#45942=CARTESIAN_POINT('Ctrl Pts',(19.4583997580746,14.7582666790052,36.2472188202353));
#45943=CARTESIAN_POINT('Ctrl Pts',(19.3941039945165,14.7625557686229,36.2684889879012));
#45944=CARTESIAN_POINT('Origin',(20.,-1.3495818343519,38.1));
#45945=CARTESIAN_POINT('',(19.3941040321498,15.7277949589794,36.2684889754515));
#45946=CARTESIAN_POINT('',(19.394103641706,15.5577020380306,36.2684891046172));
#45947=CARTESIAN_POINT('',(19.3941040087494,-1.3495818343519,36.2684889831927));
#45948=CARTESIAN_POINT('Ctrl Pts',(19.3941040321498,15.7277949589794,36.2684889754514));
#45949=CARTESIAN_POINT('Ctrl Pts',(19.4085375566523,15.7267271732423,36.2637141124117));
#45950=CARTESIAN_POINT('Ctrl Pts',(19.4230334395446,15.7256632891615,36.2591079108319));
#45951=CARTESIAN_POINT('Ctrl Pts',(19.4769071148735,15.7217442201161,36.2426885248953));
#45952=CARTESIAN_POINT('Ctrl Pts',(19.5166018821413,15.7189248518383,36.2319638844828));
#45953=CARTESIAN_POINT('Ctrl Pts',(19.5641139309572,15.7156538202491,36.220743416885));
#45954=CARTESIAN_POINT('Ctrl Pts',(19.5716262984956,15.7151396686082,36.2190167605359));
#45955=CARTESIAN_POINT('Ctrl Pts',(19.5832506867176,15.7143490010339,36.2164182439874));
#45956=CARTESIAN_POINT('Ctrl Pts',(19.5873554402317,15.7140707480158,36.2155147414123));
#45957=CARTESIAN_POINT('Ctrl Pts',(19.5949366572934,15.7135586149015,36.2138719881819));
#45958=CARTESIAN_POINT('Ctrl Pts',(19.5984121868959,15.7133245273396,36.2131289346317));
#45959=CARTESIAN_POINT('Ctrl Pts',(19.6062481792904,15.7127983000245,36.2114762642137));
#45960=CARTESIAN_POINT('Ctrl Pts',(19.610609740669,15.7125064738596,36.2105721437792));
#45961=CARTESIAN_POINT('Ctrl Pts',(19.6234301560033,15.7116517284729,36.2079608421738));
#45962=CARTESIAN_POINT('Ctrl Pts',(19.6318975161582,15.711091099965,36.2062952737316));
#45963=CARTESIAN_POINT('Ctrl Pts',(19.6928596581227,15.7070808757036,36.1947280832066));
#45964=CARTESIAN_POINT('Ctrl Pts',(19.7457398939406,15.7037410856224,36.1869528922951));
#45965=CARTESIAN_POINT('Ctrl Pts',(19.820884861692,15.6991044086728,36.1790757779161));
#45966=CARTESIAN_POINT('Ctrl Pts',(19.8429285271434,15.6977574653253,36.1771477692367));
#45967=CARTESIAN_POINT('Ctrl Pts',(20.0322938340505,15.6862645985766,36.1638635680227));
#45968=CARTESIAN_POINT('Ctrl Pts',(20.2003943389596,15.6765125810087,36.1739911840351));
#45969=CARTESIAN_POINT('Ctrl Pts',(20.4058318820859,15.6634760378526,36.2135837454306));
#45970=CARTESIAN_POINT('Ctrl Pts',(20.446326998144,15.660854688351,36.2227526493166));
#45971=CARTESIAN_POINT('Ctrl Pts',(20.4976360195265,15.6574529713628,36.2361240501768));
#45972=CARTESIAN_POINT('Ctrl Pts',(20.508752934047,15.6567110789579,36.2391277295259));
#45973=CARTESIAN_POINT('Ctrl Pts',(20.526623831838,15.6555103292636,36.2441283746714));
#45974=CARTESIAN_POINT('Ctrl Pts',(20.5333950480607,15.655053479349,36.2460631427992));
#45975=CARTESIAN_POINT('Ctrl Pts',(20.5462920352944,15.6541796481183,36.2498247568621));
#45976=CARTESIAN_POINT('Ctrl Pts',(20.5524196285936,15.6537628834141,36.2516450637265));
#45977=CARTESIAN_POINT('Ctrl Pts',(20.5664213173985,15.6528068645446,36.2558803506851));
#45978=CARTESIAN_POINT('Ctrl Pts',(20.5742891776747,15.6522669663381,36.2583153563502));
#45979=CARTESIAN_POINT('Ctrl Pts',(20.5948127006934,15.6508514653293,36.2648114364196));
#45980=CARTESIAN_POINT('Ctrl Pts',(20.6074422338898,15.6499732570847,36.2689529961436));
#45981=CARTESIAN_POINT('Ctrl Pts',(20.6991024338432,15.6435461946761,36.3000634787849));
#45982=CARTESIAN_POINT('Ctrl Pts',(20.776339935786,15.6378342394285,36.3320043698093));
#45983=CARTESIAN_POINT('Ctrl Pts',(20.995129069237,15.6207818377479,36.4395889702883));
#45984=CARTESIAN_POINT('Ctrl Pts',(21.1296075189399,15.6091150971267,36.5279858919304));
#45985=CARTESIAN_POINT('Ctrl Pts',(21.2799112377696,15.5954125008689,36.6561322185206));
#45986=CARTESIAN_POINT('Ctrl Pts',(21.3075229557033,15.5928667775108,36.6810880525385));
#45987=CARTESIAN_POINT('Ctrl Pts',(21.3398134502562,15.589872144931,36.7120163127197));
#45988=CARTESIAN_POINT('Ctrl Pts',(21.3451991387624,15.5893720694162,36.7172353492887));
#45989=CARTESIAN_POINT('Ctrl Pts',(21.353523299206,15.5885983987347,36.7253965943152));
#45990=CARTESIAN_POINT('Ctrl Pts',(21.3564828520732,15.5883231804795,36.7283170492948));
#45991=CARTESIAN_POINT('Ctrl Pts',(21.361957397213,15.5878138474623,36.733754317844));
#45992=CARTESIAN_POINT('Ctrl Pts',(21.3644748470554,15.5875795430648,36.736268498594));
#45993=CARTESIAN_POINT('Ctrl Pts',(21.3701696631782,15.5870492943094,36.7419874756169));
#45994=CARTESIAN_POINT('Ctrl Pts',(21.3733427429397,15.5867536850555,36.7451964593665));
#45995=CARTESIAN_POINT('Ctrl Pts',(21.3829518518804,15.5858578800712,36.7549827457934));
#45996=CARTESIAN_POINT('Ctrl Pts',(21.3893522212693,15.5852603779916,36.7615951090444));
#45997=CARTESIAN_POINT('Ctrl Pts',(21.4433928454948,15.5802056598205,36.8182310836686));
#45998=CARTESIAN_POINT('Ctrl Pts',(21.4883676390894,15.5759329086197,36.8707406531145));
#45999=CARTESIAN_POINT('Ctrl Pts',(21.5913455854817,15.5656608209672,37.0049325294973));
#46000=CARTESIAN_POINT('Ctrl Pts',(21.6459924361639,15.5597560391722,37.0889294141743));
#46001=CARTESIAN_POINT('Ctrl Pts',(21.7460259395296,15.5471979069135,37.2724676154762));
#46002=CARTESIAN_POINT('Ctrl Pts',(21.7899663028703,15.5405429194917,37.3723791449959));
#46003=CARTESIAN_POINT('Ctrl Pts',(21.8300135742332,15.5326404848229,37.4894178065164));
#46004=CARTESIAN_POINT('Ctrl Pts',(21.8346302860397,15.5316927883579,37.5034331630212));
#46005=CARTESIAN_POINT('Ctrl Pts',(21.8414238557428,15.5302397598384,37.5248820080998));
#46006=CARTESIAN_POINT('Ctrl Pts',(21.8437175513971,15.5297382337177,37.5322781412575));
#46007=CARTESIAN_POINT('Ctrl Pts',(21.8478100531924,15.5288230041019,37.5457610204101));
#46008=CARTESIAN_POINT('Ctrl Pts',(21.849623477474,15.5284097815853,37.551843244001));
#46009=CARTESIAN_POINT('Ctrl Pts',(21.8534753441479,15.5275151571575,37.5649991614076));
#46010=CARTESIAN_POINT('Ctrl Pts',(21.8555033709289,15.527033425708,37.5720757756974));
#46011=CARTESIAN_POINT('Ctrl Pts',(21.8608998997988,15.5257218073417,37.5913217531051));
#46012=CARTESIAN_POINT('Ctrl Pts',(21.8641894575628,15.5248893960787,37.6035126895597));
#46013=CARTESIAN_POINT('Ctrl Pts',(21.8798138466165,15.5207670131837,37.6637613799391));
#46014=CARTESIAN_POINT('Ctrl Pts',(21.8904101869077,15.5174221638474,37.7122464722687));
#46015=CARTESIAN_POINT('Ctrl Pts',(21.9038960606682,15.5121626743248,37.7878146213803));
#46016=CARTESIAN_POINT('Ctrl Pts',(21.9081015256913,15.5102866751858,37.8146434179864));
#46017=CARTESIAN_POINT('Ctrl Pts',(21.9285826523755,15.4996480655928,37.9661417142186));
#46018=CARTESIAN_POINT('Ctrl Pts',(21.9332049105341,15.4906061002666,38.092073840477));
#46019=CARTESIAN_POINT('Ctrl Pts',(21.921130115353,15.4765410159168,38.2898764992507));
#46020=CARTESIAN_POINT('Ctrl Pts',(21.9126419041394,15.4714549368797,38.3619106998993));
#46021=CARTESIAN_POINT('Ctrl Pts',(21.8977454429915,15.4656198606342,38.4468335251208));
#46022=CARTESIAN_POINT('Ctrl Pts',(21.8952275216262,15.4646968966408,38.4603386299913));
#46023=CARTESIAN_POINT('Ctrl Pts',(21.8915372997211,15.4634280397048,38.4790215748941));
#46024=CARTESIAN_POINT('Ctrl Pts',(21.8904876468279,15.4630756560278,38.4842228120673));
#46025=CARTESIAN_POINT('Ctrl Pts',(21.8886740509162,15.4624810332889,38.4930221559424));
#46026=CARTESIAN_POINT('Ctrl Pts',(21.8879212579673,15.4622381723908,38.4966225033613));
#46027=CARTESIAN_POINT('Ctrl Pts',(21.8864647909285,15.4617757740526,38.5034901727427));
#46028=CARTESIAN_POINT('Ctrl Pts',(21.8857629194071,15.4615561330702,38.5067578384331));
#46029=CARTESIAN_POINT('Ctrl Pts',(21.8838898304956,15.4609782428977,38.5153692213372));
#46030=CARTESIAN_POINT('Ctrl Pts',(21.8827043582617,15.4606207972262,38.5207098580398));
#46031=CARTESIAN_POINT('Ctrl Pts',(21.8784577368085,15.459368729564,38.5394637299755));
#46032=CARTESIAN_POINT('Ctrl Pts',(21.8752757469053,15.4584806637124,38.5528495755311));
#46033=CARTESIAN_POINT('Ctrl Pts',(21.8383263780269,15.4486885458102,38.7012135719824));
#46034=CARTESIAN_POINT('Ctrl Pts',(21.7901888193471,15.4404921868739,38.8322142356736));
#46035=CARTESIAN_POINT('Ctrl Pts',(21.6699312892944,15.4243070583666,39.0747706104339));
#46036=CARTESIAN_POINT('Ctrl Pts',(21.5996043498948,15.4163659961291,39.1863273948278));
#46037=CARTESIAN_POINT('Ctrl Pts',(21.5091734073059,15.4070033805869,39.3017345654883));
#46038=CARTESIAN_POINT('Ctrl Pts',(21.4997257631104,15.4060343583162,39.3135044103313));
#46039=CARTESIAN_POINT('Ctrl Pts',(21.4851790074799,15.4045553396243,39.331197353137));
#46040=CARTESIAN_POINT('Ctrl Pts',(21.4801802516527,15.4040493645198,39.3372025001138));
#46041=CARTESIAN_POINT('Ctrl Pts',(21.4710525854525,15.4031294463274,39.3480333252024));
#46042=CARTESIAN_POINT('Ctrl Pts',(21.4669360437069,15.4027160091941,39.3528693196211));
#46043=CARTESIAN_POINT('Ctrl Pts',(21.4580320360931,15.4018247835741,39.3632254468956));
#46044=CARTESIAN_POINT('Ctrl Pts',(21.4532369494356,15.4013466860645,39.3687388676496));
#46045=CARTESIAN_POINT('Ctrl Pts',(21.4402270020213,15.4000543996305,39.3835272679631));
#46046=CARTESIAN_POINT('Ctrl Pts',(21.4319540321716,15.3992378094522,39.3927504409573));
#46047=CARTESIAN_POINT('Ctrl Pts',(21.391864800589,15.3953046473618,39.4365871794421));
#46048=CARTESIAN_POINT('Ctrl Pts',(21.3588815409081,15.3921390434092,39.4701070110743));
#46049=CARTESIAN_POINT('Ctrl Pts',(21.3016145165002,15.3867517567224,39.5242020555569));
#46050=CARTESIAN_POINT('Ctrl Pts',(21.2779854429527,15.3845577169161,39.545442796018));
#46051=CARTESIAN_POINT('Ctrl Pts',(21.1260539856926,15.3706342996767,39.6753791296951));
#46052=CARTESIAN_POINT('Ctrl Pts',(20.9845409896285,15.3583824167357,39.7674795249549));
#46053=CARTESIAN_POINT('Ctrl Pts',(20.7986849251493,15.3440795812625,39.8564404798812));
#46054=CARTESIAN_POINT('Ctrl Pts',(20.7639995693595,15.3414836328523,39.8718030078));
#46055=CARTESIAN_POINT('Ctrl Pts',(20.7219002254329,15.3384380492012,39.8889828031167));
#46056=CARTESIAN_POINT('Ctrl Pts',(20.7149025360734,15.337935247864,39.8917906612813));
#46057=CARTESIAN_POINT('Ctrl Pts',(20.7040124808177,15.3371582832542,39.8960863966644));
#46058=CARTESIAN_POINT('Ctrl Pts',(20.7001315491789,15.336882475076,39.897602773721));
#46059=CARTESIAN_POINT('Ctrl Pts',(20.692928360163,15.3363726053825,39.9003903736069));
#46060=CARTESIAN_POINT('Ctrl Pts',(20.6896075276151,15.3361383507479,39.9016649710479));
#46061=CARTESIAN_POINT('Ctrl Pts',(20.6820765480582,15.335608918214,39.9045316285624));
#46062=CARTESIAN_POINT('Ctrl Pts',(20.6778643510864,15.3353140710924,39.9061181407743));
#46063=CARTESIAN_POINT('Ctrl Pts',(20.6650790809015,15.3344228645973,39.9108826490856));
#46064=CARTESIAN_POINT('Ctrl Pts',(20.6564887798748,15.3338291585201,39.9140145100043));
#46065=CARTESIAN_POINT('Ctrl Pts',(20.543948400933,15.3261133696095,39.9541404467903));
#46066=CARTESIAN_POINT('Ctrl Pts',(20.4370157988463,15.3194681944235,39.9822171622928));
#46067=CARTESIAN_POINT('Ctrl Pts',(20.2444412014136,15.3077770373346,40.0154699672662));
#46068=CARTESIAN_POINT('Ctrl Pts',(20.1597634307075,15.3027271058219,40.0243834965628));
#46069=CARTESIAN_POINT('Ctrl Pts',(19.9984614643572,15.2929326424395,40.030640553098));
#46070=CARTESIAN_POINT('Ctrl Pts',(19.9220459436619,15.2882187775183,40.0290662181722));
#46071=CARTESIAN_POINT('Ctrl Pts',(19.8271448834909,15.2821649643941,40.0214626798917));
#46072=CARTESIAN_POINT('Ctrl Pts',(19.8083828873996,15.2809585543214,40.0196824121958));
#46073=CARTESIAN_POINT('Ctrl Pts',(19.7811581236177,15.2791928226067,40.0166960578686));
#46074=CARTESIAN_POINT('Ctrl Pts',(19.7726721456242,15.2786402980827,40.0157081165657));
#46075=CARTESIAN_POINT('Ctrl Pts',(19.7578057289366,15.2776684609402,40.0138771929179));
#46076=CARTESIAN_POINT('Ctrl Pts',(19.7514223791438,15.2772499161873,40.0130585822829));
#46077=CARTESIAN_POINT('Ctrl Pts',(19.7390327888985,15.2764350607119,40.011406665313));
#46078=CARTESIAN_POINT('Ctrl Pts',(19.7330261392349,15.2760388671883,40.0105769499638));
#46079=CARTESIAN_POINT('Ctrl Pts',(19.7186676047639,15.2750890153492,40.008524531897));
#46080=CARTESIAN_POINT('Ctrl Pts',(19.7103196947321,15.2745345309396,40.0072753137343));
#46081=CARTESIAN_POINT('Ctrl Pts',(19.680128032732,15.2725208225955,40.0025545145015));
#46082=CARTESIAN_POINT('Ctrl Pts',(19.6583368888801,15.2710515874259,39.9987622299225));
#46083=CARTESIAN_POINT('Ctrl Pts',(19.493958766669,15.2598441958226,39.9672345119551));
#46084=CARTESIAN_POINT('Ctrl Pts',(19.3548743813257,15.2495966812474,39.9238530192994));
#46085=CARTESIAN_POINT('Ctrl Pts',(19.1424040560139,15.2330297591623,39.8302133311163));
#46086=CARTESIAN_POINT('Ctrl Pts',(19.0652655584608,15.2268142796279,39.7897876339777));
#46087=CARTESIAN_POINT('Ctrl Pts',(18.9595704378302,15.2182129055477,39.7249364832432));
#46088=CARTESIAN_POINT('Ctrl Pts',(18.9285864535048,15.2156810605605,39.7046761983854));
#46089=CARTESIAN_POINT('Ctrl Pts',(18.8920556801133,15.2127005252348,39.6792586905437));
#46090=CARTESIAN_POINT('Ctrl Pts',(18.8859339162135,15.2122012149464,39.6749461556205));
#46091=CARTESIAN_POINT('Ctrl Pts',(18.8764542161156,15.2114284691882,39.6681851598062));
#46092=CARTESIAN_POINT('Ctrl Pts',(18.873078901255,15.2111534167321,39.6657613681315));
#46093=CARTESIAN_POINT('Ctrl Pts',(18.8668279200554,15.2106442338538,39.661241895053));
#46094=CARTESIAN_POINT('Ctrl Pts',(18.8639502453261,15.2104099147768,39.6591491823679));
#46095=CARTESIAN_POINT('Ctrl Pts',(18.8574332007428,15.2098794334755,39.6543822122633));
#46096=CARTESIAN_POINT('Ctrl Pts',(18.8537974278094,15.209583607584,39.6517031343314));
#46097=CARTESIAN_POINT('Ctrl Pts',(18.8427684654447,15.2086864931242,39.6435163506903));
#46098=CARTESIAN_POINT('Ctrl Pts',(18.8354051862607,15.2080879097539,39.6379682953233));
#46099=CARTESIAN_POINT('Ctrl Pts',(18.7720914277111,15.2029413207942,39.5895474399158));
#46100=CARTESIAN_POINT('Ctrl Pts',(18.7184828857319,15.1985854926288,39.5436853390429));
#46101=CARTESIAN_POINT('Ctrl Pts',(18.5865458704213,15.1875141749061,39.4176581829229));
#46102=CARTESIAN_POINT('Ctrl Pts',(18.512475459151,15.1809286172461,39.3334292880801));
#46103=CARTESIAN_POINT('Ctrl Pts',(18.4080698552719,15.1702963969616,39.1915240886494));
#46104=CARTESIAN_POINT('Ctrl Pts',(18.3726224065446,15.1663742420883,39.1379342746715));
#46105=CARTESIAN_POINT('Ctrl Pts',(18.3206147686253,15.159994205808,39.050075440991));
#46106=CARTESIAN_POINT('Ctrl Pts',(18.3022805602356,15.1575970177786,39.0169113899435));
#46107=CARTESIAN_POINT('Ctrl Pts',(18.2798264055172,15.1544489441784,38.9733097338618));
#46108=CARTESIAN_POINT('Ctrl Pts',(18.2748035229787,15.1537297213717,38.9633447709798));
#46109=CARTESIAN_POINT('Ctrl Pts',(18.2667871986205,15.1525568119072,38.9470917498654));
#46110=CARTESIAN_POINT('Ctrl Pts',(18.263740804832,15.1521049646905,38.9408299784408));
#46111=CARTESIAN_POINT('Ctrl Pts',(18.2579536251644,15.1512346580685,38.9287690425657));
#46112=CARTESIAN_POINT('Ctrl Pts',(18.2552077241167,15.1508163819025,38.9229724238086));
#46113=CARTESIAN_POINT('Ctrl Pts',(18.248992974397,15.1498573231739,38.9096821232672));
#46114=CARTESIAN_POINT('Ctrl Pts',(18.2455432496341,15.1493158947734,38.9021796880832));
#46115=CARTESIAN_POINT('Ctrl Pts',(18.2365134720629,15.1478741607111,38.8822049071968));
#46116=CARTESIAN_POINT('Ctrl Pts',(18.2310176625595,15.1469710172888,38.8696952154138));
#46117=CARTESIAN_POINT('Ctrl Pts',(18.1868999874683,15.139503517502,38.7663046210797));
#46118=CARTESIAN_POINT('Ctrl Pts',(18.1551815304772,15.1327079376398,38.6726541272111));
#46119=CARTESIAN_POINT('Ctrl Pts',(18.1078542109622,15.1192276954962,38.4871920801643));
#46120=CARTESIAN_POINT('Ctrl Pts',(18.0914391766159,15.1125805430756,38.3958508109507));
#46121=CARTESIAN_POINT('Ctrl Pts',(18.0786747548679,15.103984302572,38.2756352576924));
#46122=CARTESIAN_POINT('Ctrl Pts',(18.0763116895298,15.1019851890267,38.2475188328068));
#46123=CARTESIAN_POINT('Ctrl Pts',(18.0720921829533,15.0971857104321,38.1794526580731));
#46124=CARTESIAN_POINT('Ctrl Pts',(18.0708594130487,15.0944000276961,38.1394752581004));
#46125=CARTESIAN_POINT('Ctrl Pts',(18.0708759804055,15.090145480618,38.0772988364329));
#46126=CARTESIAN_POINT('Ctrl Pts',(18.0712646576823,15.0886427997716,38.0551122559255));
#46127=CARTESIAN_POINT('Ctrl Pts',(18.0722660625258,15.0867171863381,38.0263236714397));
#46128=CARTESIAN_POINT('Ctrl Pts',(18.0725300991515,15.0862766227344,38.0197122702361));
#46129=CARTESIAN_POINT('Ctrl Pts',(18.0730066727158,15.0855751177809,38.009143077628));
#46130=CARTESIAN_POINT('Ctrl Pts',(18.0731973967014,15.0853129989548,38.0051844297204));
#46131=CARTESIAN_POINT('Ctrl Pts',(18.073584451733,15.084814340807,37.9976348441183));
#46132=CARTESIAN_POINT('Ctrl Pts',(18.0737786219787,15.0845776922221,37.9940439110168));
#46133=CARTESIAN_POINT('Ctrl Pts',(18.0742578372785,15.0840236679026,37.9856184792676));
#46134=CARTESIAN_POINT('Ctrl Pts',(18.0745510466235,15.0837067478324,37.9807844860561));
#46135=CARTESIAN_POINT('Ctrl Pts',(18.0755663250056,15.0826766821078,37.9650281339409));
#46136=CARTESIAN_POINT('Ctrl Pts',(18.0763631682835,15.0819675454294,37.9541105650493));
#46137=CARTESIAN_POINT('Ctrl Pts',(18.0784760588321,15.0802943126343,37.9282014080321));
#46138=CARTESIAN_POINT('Ctrl Pts',(18.0798746973229,15.079334306866,37.9132170629736));
#46139=CARTESIAN_POINT('Ctrl Pts',(18.0856182798852,15.0758581357153,37.858598154672));
#46140=CARTESIAN_POINT('Ctrl Pts',(18.0910165316802,15.0733876090198,37.819082286835));
#46141=CARTESIAN_POINT('Ctrl Pts',(18.1188531923818,15.0631320113997,37.6537206717427));
#46142=CARTESIAN_POINT('Ctrl Pts',(18.1525440759779,15.055648475771,37.5300979534588));
#46143=CARTESIAN_POINT('Ctrl Pts',(18.2311988342254,15.0423483810047,37.3244964157323));
#46144=CARTESIAN_POINT('Ctrl Pts',(18.27032214551,15.0366683151079,37.2407709757419));
#46145=CARTESIAN_POINT('Ctrl Pts',(18.3218691396414,15.0299110609312,37.1483687156214));
#46146=CARTESIAN_POINT('Ctrl Pts',(18.3285784148818,15.0290435529437,37.1366334260572));
#46147=CARTESIAN_POINT('Ctrl Pts',(18.3395622441858,15.0276418023127,37.1178816276831));
#46148=CARTESIAN_POINT('Ctrl Pts',(18.3437593355424,15.0271103363201,37.1108200890934));
#46149=CARTESIAN_POINT('Ctrl Pts',(18.351310421068,15.0261613910522,37.0982983027419));
#46150=CARTESIAN_POINT('Ctrl Pts',(18.354646780932,15.025744555277,37.0928275218107));
#46151=CARTESIAN_POINT('Ctrl Pts',(18.3616763252453,15.0248713174555,37.0814290056135));
#46152=CARTESIAN_POINT('Ctrl Pts',(18.3653745615516,15.0244147351359,37.0755045106534));
#46153=CARTESIAN_POINT('Ctrl Pts',(18.3751149949633,15.0232194273196,37.060087555919));
#46154=CARTESIAN_POINT('Ctrl Pts',(18.3812081469487,15.0224788351204,37.050627759859));
#46155=CARTESIAN_POINT('Ctrl Pts',(18.4086797963715,15.0191706397919,37.0087859087772));
#46156=CARTESIAN_POINT('Ctrl Pts',(18.4309483519988,15.0165701166044,36.9770018959075));
#46157=CARTESIAN_POINT('Ctrl Pts',(18.4939313233235,15.0094197570901,36.8926394066831));
#46158=CARTESIAN_POINT('Ctrl Pts',(18.5364272442127,15.0048062870758,36.8414628793917));
#46159=CARTESIAN_POINT('Ctrl Pts',(18.667701780251,14.9911668571237,36.6990320336801));
#46160=CARTESIAN_POINT('Ctrl Pts',(18.7629663621871,14.9819748753686,36.6142423313337));
#46161=CARTESIAN_POINT('Ctrl Pts',(18.9085123176894,14.969351265367,36.5084678973066));
#46162=CARTESIAN_POINT('Ctrl Pts',(18.9523992111517,14.9657084238926,36.4792429210688));
#46163=CARTESIAN_POINT('Ctrl Pts',(19.0047811865298,14.9615923819726,36.447379032057));
#46164=CARTESIAN_POINT('Ctrl Pts',(19.0121602386957,14.9610177427832,36.4429577062959));
#46165=CARTESIAN_POINT('Ctrl Pts',(19.0233997758683,14.9601505970668,36.4363250478059));
#46166=CARTESIAN_POINT('Ctrl Pts',(19.0272386228386,14.9598558514163,36.4340775382926));
#46167=CARTESIAN_POINT('Ctrl Pts',(19.0341582643769,14.9593271720334,36.4300584058574));
#46168=CARTESIAN_POINT('Ctrl Pts',(19.0372361939428,14.9590929368622,36.4282820092776));
#46169=CARTESIAN_POINT('Ctrl Pts',(19.0439692301107,14.9585825664841,36.4244208675977));
#46170=CARTESIAN_POINT('Ctrl Pts',(19.0476262452673,14.9583066522158,36.422339577254));
#46171=CARTESIAN_POINT('Ctrl Pts',(19.0580209409351,14.9575259641974,36.4164686621131));
#46172=CARTESIAN_POINT('Ctrl Pts',(19.0647747253548,14.9570229641856,36.4127074930724));
#46173=CARTESIAN_POINT('Ctrl Pts',(19.1079721456911,14.9538315073299,36.3889899951918));
#46174=CARTESIAN_POINT('Ctrl Pts',(19.1450329642464,14.9512096608562,36.3701731604945));
#46175=CARTESIAN_POINT('Ctrl Pts',(19.2514578480228,14.9439227361318,36.3203952183265));
#46176=CARTESIAN_POINT('Ctrl Pts',(19.3220578546409,14.9393684297755,36.2923231123525));
#46177=CARTESIAN_POINT('Ctrl Pts',(19.3941040816519,14.9348319053408,36.2684889590753));
#46178=CARTESIAN_POINT('',(18.0708709355256,14.9215670950978,38.101670466408));
#46179=CARTESIAN_POINT('Ctrl Pts',(19.3941039945165,14.7625557686229,36.2684889879012));
#46180=CARTESIAN_POINT('Ctrl Pts',(19.3825170814759,14.7633287170362,36.2723221422098));
#46181=CARTESIAN_POINT('Ctrl Pts',(19.3709654940846,14.7641050973507,36.2762655991737));
#46182=CARTESIAN_POINT('Ctrl Pts',(19.3470290856284,14.7657264678271,36.2846914971796));
#46183=CARTESIAN_POINT('Ctrl Pts',(19.3346527248423,14.7665718818522,36.2891910743904));
#46184=CARTESIAN_POINT('Ctrl Pts',(19.3146469097067,14.7679504381129,36.296697217088));
#46185=CARTESIAN_POINT('Ctrl Pts',(19.3069887168908,14.7684810204803,36.2996263878568));
#46186=CARTESIAN_POINT('Ctrl Pts',(19.2933980211644,14.7694278523957,36.3049242347102));
#46187=CARTESIAN_POINT('Ctrl Pts',(19.2874581362398,14.7698434582092,36.3072737380237));
#46188=CARTESIAN_POINT('Ctrl Pts',(19.2760054960788,14.7706482930595,36.3118697051008));
#46189=CARTESIAN_POINT('Ctrl Pts',(19.2704912476441,14.7710373877188,36.3141122733644));
#46190=CARTESIAN_POINT('Ctrl Pts',(19.2559313623455,14.7720689949999,36.3201122617398));
#46191=CARTESIAN_POINT('Ctrl Pts',(19.2469039046818,14.7727129604863,36.3239130754404));
#46192=CARTESIAN_POINT('Ctrl Pts',(19.2113863830722,14.7752640548029,36.3391864217279));
#46193=CARTESIAN_POINT('Ctrl Pts',(19.1851274521977,14.7771888165935,36.3511836938677));
#46194=CARTESIAN_POINT('Ctrl Pts',(19.1193430360133,14.7821124641708,36.3830428096565));
#46195=CARTESIAN_POINT('Ctrl Pts',(19.0802148840544,14.7851365946205,36.4036823668253));
#46196=CARTESIAN_POINT('Ctrl Pts',(18.9526186235064,14.7953188952831,36.4767007375094));
#46197=CARTESIAN_POINT('Ctrl Pts',(18.8676351296202,14.8026426126488,36.5347989567379));
#46198=CARTESIAN_POINT('Ctrl Pts',(18.7080612505083,14.8172795360261,36.6637143537549));
#46199=CARTESIAN_POINT('Ctrl Pts',(18.6336687812491,14.8245678760486,36.734289351721));
#46200=CARTESIAN_POINT('Ctrl Pts',(18.5553319258502,14.8325138185745,36.8214478193331));
#46201=CARTESIAN_POINT('Ctrl Pts',(18.5455668768958,14.8335095128195,36.8325672221919));
#46202=CARTESIAN_POINT('Ctrl Pts',(18.5322585460864,14.8348724550545,36.8480777271274));
#46203=CARTESIAN_POINT('Ctrl Pts',(18.5286054291828,14.8352472149661,36.8523733043125));
#46204=CARTESIAN_POINT('Ctrl Pts',(18.5227964260123,14.8358440728404,36.8592649179751));
#46205=CARTESIAN_POINT('Ctrl Pts',(18.5206284606786,14.8360670350476,36.8618506585018));
#46206=CARTESIAN_POINT('Ctrl Pts',(18.5161297155703,14.8365301187888,36.8672450136462));
#46207=CARTESIAN_POINT('Ctrl Pts',(18.5138001128867,14.836770149891,36.8700545649531));
#46208=CARTESIAN_POINT('Ctrl Pts',(18.5081971783227,14.8373480519452,36.8768509871864));
#46209=CARTESIAN_POINT('Ctrl Pts',(18.5049318057403,14.8376853527562,36.8808444470318));
#46210=CARTESIAN_POINT('Ctrl Pts',(18.4936205515567,14.8388557098299,36.89479158512));
#46211=CARTESIAN_POINT('Ctrl Pts',(18.485657522621,14.8396830909797,36.9048124630799));
#46212=CARTESIAN_POINT('Ctrl Pts',(18.4446693281657,14.8439645510968,36.9574604197185));
#46213=CARTESIAN_POINT('Ctrl Pts',(18.4133393160563,14.8473155636438,37.0013830573589));
#46214=CARTESIAN_POINT('Ctrl Pts',(18.3493137886308,14.8544785413536,37.0996068567846));
#46215=CARTESIAN_POINT('Ctrl Pts',(18.317369987036,14.858265337978,37.1543212235262));
#46216=CARTESIAN_POINT('Ctrl Pts',(18.2565596030849,14.8661437693364,37.271350940125));
#46217=CARTESIAN_POINT('Ctrl Pts',(18.2282122160191,14.8702295591531,37.3338333431942));
#46218=CARTESIAN_POINT('Ctrl Pts',(18.1716566276983,14.8796380772103,37.4785218755403));
#46219=CARTESIAN_POINT('Ctrl Pts',(18.1455556554264,14.8849926744456,37.5613834283294));
#46220=CARTESIAN_POINT('Ctrl Pts',(18.1219729855613,14.8913894558923,37.6587110420034));
#46221=CARTESIAN_POINT('Ctrl Pts',(18.1189589631229,14.8922478408553,37.6717407157426));
#46222=CARTESIAN_POINT('Ctrl Pts',(18.1143218482917,14.893637680983,37.6927810789366));
#46223=CARTESIAN_POINT('Ctrl Pts',(18.1126137308912,14.8941664356862,37.7007727347712));
#46224=CARTESIAN_POINT('Ctrl Pts',(18.1096581721152,14.8951122867157,37.7150437496867));
#46225=CARTESIAN_POINT('Ctrl Pts',(18.1083911062992,14.8955287544917,37.7213189567283));
#46226=CARTESIAN_POINT('Ctrl Pts',(18.1060070083707,14.89633411947,37.7334369229984));
#46227=CARTESIAN_POINT('Ctrl Pts',(18.1048857182964,14.8967228766726,37.7392787783969));
#46228=CARTESIAN_POINT('Ctrl Pts',(18.1025267576376,14.8975628067071,37.7518834695705));
#46229=CARTESIAN_POINT('Ctrl Pts',(18.1012981884257,14.898014261659,37.7586479047967));
#46230=CARTESIAN_POINT('Ctrl Pts',(18.0984106526094,14.899110315052,37.7750445543664));
#46231=CARTESIAN_POINT('Ctrl Pts',(18.0967886934356,14.8997560682308,37.7846830096993));
#46232=CARTESIAN_POINT('Ctrl Pts',(18.0903074014813,14.9024683268269,37.8250711259566));
#46233=CARTESIAN_POINT('Ctrl Pts',(18.0861197531659,14.9045556203006,37.8559223123455));
#46234=CARTESIAN_POINT('Ctrl Pts',(18.0747503038764,14.9115296362581,37.9581971170406));
#46235=CARTESIAN_POINT('Ctrl Pts',(18.0708085194889,14.9165097739879,38.0299123159641));
#46236=CARTESIAN_POINT('Ctrl Pts',(18.0708707248063,14.9215668540041,38.1016722710962));
#46237=CARTESIAN_POINT('Ctrl Pts',(18.0708707232653,14.9215667286563,38.101670492412));
#46238=CARTESIAN_POINT('Ctrl Pts',(18.0710017404283,14.9322293155351,38.2529726133779));
#46239=CARTESIAN_POINT('Ctrl Pts',(18.0889313147645,14.9432227578084,38.4037348986348));
#46240=CARTESIAN_POINT('Ctrl Pts',(18.1288901782916,14.9550052098152,38.5699757315882));
#46241=CARTESIAN_POINT('Ctrl Pts',(18.133777615627,14.9563491307252,38.5890227310713));
#46242=CARTESIAN_POINT('Ctrl Pts',(18.1424976031405,14.9585893130191,38.6209686453709));
#46243=CARTESIAN_POINT('Ctrl Pts',(18.1461753347472,14.9594927965574,38.6339078751857));
#46244=CARTESIAN_POINT('Ctrl Pts',(18.1514796798755,14.9607394923726,38.6518540293113));
#46245=CARTESIAN_POINT('Ctrl Pts',(18.1529917907639,14.9610889061984,38.6568939936875));
#46246=CARTESIAN_POINT('Ctrl Pts',(18.1555933817275,14.9616799838705,38.6654381028776));
#46247=CARTESIAN_POINT('Ctrl Pts',(18.1566722662579,14.9619222527361,38.6689454178969));
#46248=CARTESIAN_POINT('Ctrl Pts',(18.1587555972969,14.962384641447,38.6756499255739));
#46249=CARTESIAN_POINT('Ctrl Pts',(18.1597583721496,14.9626048594809,38.6788475955318));
#46250=CARTESIAN_POINT('Ctrl Pts',(18.1624344337767,14.9631864317609,38.6873038385007));
#46251=CARTESIAN_POINT('Ctrl Pts',(18.1641219756233,14.963546962936,38.6925579215016));
#46252=CARTESIAN_POINT('Ctrl Pts',(18.1701844730051,14.9648206826069,38.7111587070151));
#46253=CARTESIAN_POINT('Ctrl Pts',(18.174682742171,14.965727013232,38.7244651823075));
#46254=CARTESIAN_POINT('Ctrl Pts',(18.2236061562312,14.9752009919015,38.8641398535692));
#46255=CARTESIAN_POINT('Ctrl Pts',(18.2809395216915,14.9831150931849,38.9856222866736));
#46256=CARTESIAN_POINT('Ctrl Pts',(18.385668460247,14.9951847352943,39.1583483003979));
#46257=CARTESIAN_POINT('Ctrl Pts',(18.423976823261,14.9992598497402,39.2145930735379));
#46258=CARTESIAN_POINT('Ctrl Pts',(18.5075294039111,15.0076858888618,39.324321174371));
#46259=CARTESIAN_POINT('Ctrl Pts',(18.5528739008648,15.0120352672345,39.3775974322869));
#46260=CARTESIAN_POINT('Ctrl Pts',(18.610500179791,15.0173862518684,39.4382910508278));
#46261=CARTESIAN_POINT('Ctrl Pts',(18.6201010914718,15.0182722541408,39.4481882930215));
#46262=CARTESIAN_POINT('Ctrl Pts',(18.6342192964939,15.0195676649752,39.4624334529925));
#46263=CARTESIAN_POINT('Ctrl Pts',(18.6386531403675,15.0199734414555,39.4668637716116));
#46264=CARTESIAN_POINT('Ctrl Pts',(18.647670492156,15.0207966307534,39.4757865565823));
#46265=CARTESIAN_POINT('Ctrl Pts',(18.6522549829831,15.0212140841874,39.4802779120552));
#46266=CARTESIAN_POINT('Ctrl Pts',(18.6612404755007,15.0220302707643,39.4889934139346));
#46267=CARTESIAN_POINT('Ctrl Pts',(18.6656392737165,15.0224289028678,39.4932197310939));
#46268=CARTESIAN_POINT('Ctrl Pts',(18.6775253828868,15.0235036268749,39.5045318479923));
#46269=CARTESIAN_POINT('Ctrl Pts',(18.6850494838382,15.0241813769467,39.5115785341292));
#46270=CARTESIAN_POINT('Ctrl Pts',(18.7131687768133,15.026705135967,39.5374936989384));
#46271=CARTESIAN_POINT('Ctrl Pts',(18.7341156938454,15.028567253217,39.555973734906));
#46272=CARTESIAN_POINT('Ctrl Pts',(18.7573490814075,15.0306146182162,39.5755905235295));
#46273=CARTESIAN_POINT('Ctrl Pts',(18.7592457091535,15.0307816237693,39.5771856647896));
#46274=CARTESIAN_POINT('Ctrl Pts',(18.7659970004889,15.0313756470995,39.5828416004334));
#46275=CARTESIAN_POINT('Ctrl Pts',(18.7708685275807,15.0318034437056,39.5868821193089));
#46276=CARTESIAN_POINT('Ctrl Pts',(18.880176702941,15.0413839856123,39.6766397100555));
#46277=CARTESIAN_POINT('Ctrl Pts',(18.993296241773,15.0509644470984,39.7511611698253));
#46278=CARTESIAN_POINT('Ctrl Pts',(19.1858804051716,15.0664383684951,39.8508399462787));
#46279=CARTESIAN_POINT('Ctrl Pts',(19.2608342202858,15.0722704320492,39.8837788136787));
#46280=CARTESIAN_POINT('Ctrl Pts',(19.3712259614628,15.080414670461,39.9241335631306));
#46281=CARTESIAN_POINT('Ctrl Pts',(19.405132556716,15.0828577765018,39.9354708314618));
#46282=CARTESIAN_POINT('Ctrl Pts',(19.4464307297838,15.0857479807396,39.9480147676338));
#46283=CARTESIAN_POINT('Ctrl Pts',(19.4535368266165,15.0862422697861,39.9501285152242));
#46284=CARTESIAN_POINT('Ctrl Pts',(19.4646291628682,15.0870089436822,39.9533585071972));
#46285=CARTESIAN_POINT('Ctrl Pts',(19.4686070135657,15.08728290572,39.9545029480212));
#46286=CARTESIAN_POINT('Ctrl Pts',(19.4760129032362,15.087791108242,39.9566078618513));
#46287=CARTESIAN_POINT('Ctrl Pts',(19.4794398852097,15.0880255309155,39.9575716399306));
#46288=CARTESIAN_POINT('Ctrl Pts',(19.4872421104714,15.0885575743056,39.9597425904262));
#46289=CARTESIAN_POINT('Ctrl Pts',(19.4916189514371,15.088854850465,39.9609438106565));
#46290=CARTESIAN_POINT('Ctrl Pts',(19.505008422866,15.0897607606897,39.9645677759412));
#46291=CARTESIAN_POINT('Ctrl Pts',(19.5140345933868,15.0903666113415,39.9669406215983));
#46292=CARTESIAN_POINT('Ctrl Pts',(19.6015932486645,15.096200031468,39.9892804416742));
#46293=CARTESIAN_POINT('Ctrl Pts',(19.6813037663588,15.10117276984,40.0043488982309));
#46294=CARTESIAN_POINT('Ctrl Pts',(19.9243903049339,15.1159584016255,40.034603883621));
#46295=CARTESIAN_POINT('Ctrl Pts',(20.0889516302879,15.1255187532477,40.034036160001));
#46296=CARTESIAN_POINT('Ctrl Pts',(20.2904168733236,15.1382023105806,40.0075493186322));
#46297=CARTESIAN_POINT('Ctrl Pts',(20.3292050326199,15.1406863681932,40.0012390881905));
#46298=CARTESIAN_POINT('Ctrl Pts',(20.3788653726925,15.1439328975019,39.9915949096823));
#46299=CARTESIAN_POINT('Ctrl Pts',(20.3899399174842,15.1446611493818,39.9893430405516));
#46300=CARTESIAN_POINT('Ctrl Pts',(20.4078358993412,15.1458451434993,39.9855400721729));
#46301=CARTESIAN_POINT('Ctrl Pts',(20.4146699153154,15.1462989800969,39.984048922868));
#46302=CARTESIAN_POINT('Ctrl Pts',(20.4277456025235,15.1471706424426,39.9811212819063));
#46303=CARTESIAN_POINT('Ctrl Pts',(20.4339885366748,15.1475882714966,39.9796908059837));
#46304=CARTESIAN_POINT('Ctrl Pts',(20.4482007201145,15.1485423935251,39.9763597181838));
#46305=CARTESIAN_POINT('Ctrl Pts',(20.4561651747887,15.1490795095595,39.9744393848178));
#46306=CARTESIAN_POINT('Ctrl Pts',(20.4771654052179,15.1505022897096,39.9692341888015));
#46307=CARTESIAN_POINT('Ctrl Pts',(20.490179305898,15.151390674141,39.9658637434479));
#46308=CARTESIAN_POINT('Ctrl Pts',(20.5894197347014,15.158217686716,39.9390517711754));
#46309=CARTESIAN_POINT('Ctrl Pts',(20.673946386771,15.1643440675916,39.9097842745135));
#46310=CARTESIAN_POINT('Ctrl Pts',(20.9049052988862,15.1819521047212,39.8113855113679));
#46311=CARTESIAN_POINT('Ctrl Pts',(21.0451088356389,15.193730133982,39.7295515177725));
#46312=CARTESIAN_POINT('Ctrl Pts',(21.1976432290568,15.2069848038621,39.6126539078794));
#46313=CARTESIAN_POINT('Ctrl Pts',(21.2213892505422,15.2090602884132,39.5935460170333));
#46314=CARTESIAN_POINT('Ctrl Pts',(21.2500727286646,15.2115724485675,39.569323197854));
#46315=CARTESIAN_POINT('Ctrl Pts',(21.2554463438305,15.2120433068556,39.5647344360943));
#46316=CARTESIAN_POINT('Ctrl Pts',(21.2638698556542,15.2127816011059,39.557460823532));
#46317=CARTESIAN_POINT('Ctrl Pts',(21.2669366244723,15.213050434075,39.5547957432197));
#46318=CARTESIAN_POINT('Ctrl Pts',(21.2726833519682,15.2135542303858,39.5497697741118));
#46319=CARTESIAN_POINT('Ctrl Pts',(21.2753651433426,15.213789345003,39.5474111591748));
#46320=CARTESIAN_POINT('Ctrl Pts',(21.281469795115,15.2143245934729,39.5420120252132));
#46321=CARTESIAN_POINT('Ctrl Pts',(21.2848883899372,15.2146243709207,39.5389667623406));
#46322=CARTESIAN_POINT('Ctrl Pts',(21.29391801812,15.2154163881467,39.530865390543));
#46323=CARTESIAN_POINT('Ctrl Pts',(21.2995103225973,15.2159071199763,39.5257883887399));
#46324=CARTESIAN_POINT('Ctrl Pts',(21.3385239143036,15.2193333352411,39.4899494752967));
#46325=CARTESIAN_POINT('Ctrl Pts',(21.3708824305684,15.2221892972435,39.458045629051));
#46326=CARTESIAN_POINT('Ctrl Pts',(21.4228671277103,15.2268642049187,39.4030376060969));
#46327=CARTESIAN_POINT('Ctrl Pts',(21.4431278438082,15.2287101559551,39.380562387515));
#46328=CARTESIAN_POINT('Ctrl Pts',(21.5714959396856,15.2406343612329,39.231245672687));
#46329=CARTESIAN_POINT('Ctrl Pts',(21.6633022064373,15.2503255900376,39.0913338677388));
#46330=CARTESIAN_POINT('Ctrl Pts',(21.7546434489484,15.263362838157,38.9028690596031));
#46331=CARTESIAN_POINT('Ctrl Pts',(21.7720129821099,15.2660622206113,38.86376823612));
#46332=CARTESIAN_POINT('Ctrl Pts',(21.792434012896,15.2695519318515,38.8133429576412));
#46333=CARTESIAN_POINT('Ctrl Pts',(21.7967026416769,15.2703012490666,38.8025222228319));
#46334=CARTESIAN_POINT('Ctrl Pts',(21.8034072256107,15.2715111205582,38.7850656119356));
#46335=CARTESIAN_POINT('Ctrl Pts',(21.8059050662551,15.2719696111923,38.7784536856085));
#46336=CARTESIAN_POINT('Ctrl Pts',(21.8105905219428,15.272844672462,38.7658418000608));
#46337=CARTESIAN_POINT('Ctrl Pts',(21.8127847931839,15.2732610158293,38.7598444004608));
#46338=CARTESIAN_POINT('Ctrl Pts',(21.817724086413,15.2742133799803,38.7461336799947));
#46339=CARTESIAN_POINT('Ctrl Pts',(21.820449850792,15.2747500273393,38.7384135994957));
#46340=CARTESIAN_POINT('Ctrl Pts',(21.8274184041377,15.2761514799716,38.7182692731368));
#46341=CARTESIAN_POINT('Ctrl Pts',(21.8315835931396,15.2770188071101,38.7058188217716));
#46342=CARTESIAN_POINT('Ctrl Pts',(21.8597854138577,15.2831058275555,38.6185686959296));
#46343=CARTESIAN_POINT('Ctrl Pts',(21.8793568689404,15.2884692535588,38.5424139948449));
#46344=CARTESIAN_POINT('Ctrl Pts',(21.9254910035408,15.3054665577556,38.3031809285054));
#46345=CARTESIAN_POINT('Ctrl Pts',(21.9358114740606,15.3174898856621,38.1377515694563));
#46346=CARTESIAN_POINT('Ctrl Pts',(21.9224695882963,15.3315587564005,37.9354676778912));
#46347=CARTESIAN_POINT('Ctrl Pts',(21.9188920251195,15.3341356213825,37.8979750979097));
#46348=CARTESIAN_POINT('Ctrl Pts',(21.9132852138639,15.3371618568658,37.8531420124475));
#46349=CARTESIAN_POINT('Ctrl Pts',(21.9123077759905,15.3376636294777,37.8456810072378));
#46350=CARTESIAN_POINT('Ctrl Pts',(21.9107217499668,15.3384393506288,37.8341009890665));
#46351=CARTESIAN_POINT('Ctrl Pts',(21.9101434537088,15.3387149358281,37.8299780066767));
#46352=CARTESIAN_POINT('Ctrl Pts',(21.9090462781763,15.3392246014857,37.822335598849));
#46353=CARTESIAN_POINT('Ctrl Pts',(21.9085310159957,15.3394588737509,37.8188157664191));
#46354=CARTESIAN_POINT('Ctrl Pts',(21.9073410949495,15.339988610139,37.8108412147191));
#46355=CARTESIAN_POINT('Ctrl Pts',(21.9066605663013,15.3402837418653,37.8063874295647));
#46356=CARTESIAN_POINT('Ctrl Pts',(21.9045483463365,15.3411766665509,37.7928808795931));
#46357=CARTESIAN_POINT('Ctrl Pts',(21.9030677137793,15.341771791164,37.78383573498));
#46358=CARTESIAN_POINT('Ctrl Pts',(21.8830710705866,15.3494319397087,37.6669100944897));
#46359=CARTESIAN_POINT('Ctrl Pts',(21.8554673429379,15.3560278073103,37.560767298052));
#46360=CARTESIAN_POINT('Ctrl Pts',(21.7912119339226,15.367571884396,37.3788443180618));
#46361=CARTESIAN_POINT('Ctrl Pts',(21.7583458000219,15.3725261118798,37.3020492958186));
#46362=CARTESIAN_POINT('Ctrl Pts',(21.6851460026965,15.3823369386165,37.1576749837671));
#46363=CARTESIAN_POINT('Ctrl Pts',(21.6454512378319,15.3871721320615,37.089959618423));
#46364=CARTESIAN_POINT('Ctrl Pts',(21.591097417306,15.3933717965582,37.0089835692151));
#46365=CARTESIAN_POINT('Ctrl Pts',(21.580210683998,15.3945950364533,36.993274200126));
#46366=CARTESIAN_POINT('Ctrl Pts',(21.5640943762968,15.3963809132185,36.9707413237919));
#46367=CARTESIAN_POINT('Ctrl Pts',(21.5590495446857,15.3969365295344,36.9637866005684));
#46368=CARTESIAN_POINT('Ctrl Pts',(21.5501404688064,15.3979119441622,36.9516757431441));
#46369=CARTESIAN_POINT('Ctrl Pts',(21.5462965087628,15.3983309569206,36.9465047996514));
#46370=CARTESIAN_POINT('Ctrl Pts',(21.5387932639153,15.3991453486652,36.9365162455755));
#46371=CARTESIAN_POINT('Ctrl Pts',(21.5351370754279,15.3995406040156,36.931696394712));
#46372=CARTESIAN_POINT('Ctrl Pts',(21.5263577760805,15.4004859914057,36.9202352569944));
#46373=CARTESIAN_POINT('Ctrl Pts',(21.5212139386252,15.4010369320755,36.9136100731111));
#46374=CARTESIAN_POINT('Ctrl Pts',(21.5025614451121,15.4030243280626,36.8899066949334));
#46375=CARTESIAN_POINT('Ctrl Pts',(21.4888074922623,15.4044704564735,36.8730244955106));
#46376=CARTESIAN_POINT('Ctrl Pts',(21.3766317807976,15.4161181427909,36.7399988022156));
#46377=CARTESIAN_POINT('Ctrl Pts',(21.2650796948774,15.4268853085969,36.6356660403599));
#46378=CARTESIAN_POINT('Ctrl Pts',(21.0764793588935,15.4435871507526,36.4970529223805));
#46379=CARTESIAN_POINT('Ctrl Pts',(21.0074762172974,15.449426375672,36.4528083016758));
#46380=CARTESIAN_POINT('Ctrl Pts',(20.90459061463,15.4575792001072,36.3957295971273));
#46381=CARTESIAN_POINT('Ctrl Pts',(20.8728358933348,15.4600240073143,36.3792502532933));
#46382=CARTESIAN_POINT('Ctrl Pts',(20.8339649084032,15.4629159463888,36.3604310673338));
#46383=CARTESIAN_POINT('Ctrl Pts',(20.827272186175,15.4634103337969,36.3572383197009));
#46384=CARTESIAN_POINT('Ctrl Pts',(20.8168147573747,15.4641771266634,36.3523234440498));
#46385=CARTESIAN_POINT('Ctrl Pts',(20.8130627247348,15.4644511100855,36.3505747519457));
#46386=CARTESIAN_POINT('Ctrl Pts',(20.806073533659,15.4649593316861,36.3473446749764));
#46387=CARTESIAN_POINT('Ctrl Pts',(20.8028379338008,15.4651937521809,36.3458601873363));
#46388=CARTESIAN_POINT('Ctrl Pts',(20.7954681761301,15.4657257642825,36.3425036180366));
#46389=CARTESIAN_POINT('Ctrl Pts',(20.7913315165301,15.4660230114962,36.3406371653817));
#46390=CARTESIAN_POINT('Ctrl Pts',(20.7786701451491,15.4669287457539,36.3349780694795));
#46391=CARTESIAN_POINT('Ctrl Pts',(20.7701243172957,15.4675344509599,36.3312325889039));
#46392=CARTESIAN_POINT('Ctrl Pts',(20.6873271554236,15.4733519215207,36.2956579500781));
#46393=CARTESIAN_POINT('Ctrl Pts',(20.6111625681457,15.4783104116689,36.2684562170631));
#46394=CARTESIAN_POINT('Ctrl Pts',(20.3758533671781,15.4930914553543,36.2007396417898));
#46395=CARTESIAN_POINT('Ctrl Pts',(20.2130665747769,15.5026589739064,36.1756669736538));
#46396=CARTESIAN_POINT('Ctrl Pts',(20.0097017635029,15.5153560958906,36.17049248089));
#46397=CARTESIAN_POINT('Ctrl Pts',(19.9703148218189,15.5178456812455,36.1706965404218));
#46398=CARTESIAN_POINT('Ctrl Pts',(19.9196609864837,15.5210984684024,36.1725104108669));
#46399=CARTESIAN_POINT('Ctrl Pts',(19.908362195965,15.5218272841384,36.1730145362958));
#46400=CARTESIAN_POINT('Ctrl Pts',(19.8900818619955,15.5230119706832,36.1739912993739));
#46401=CARTESIAN_POINT('Ctrl Pts',(19.8830972002918,15.5234659316877,36.1744026263949));
#46402=CARTESIAN_POINT('Ctrl Pts',(19.8697240300732,15.5243376809386,36.1752632018185));
#46403=CARTESIAN_POINT('Ctrl Pts',(19.863335206912,15.5247552716585,36.1757062845576));
#46404=CARTESIAN_POINT('Ctrl Pts',(19.8487825357766,15.5257090949591,36.176788391374));
#46405=CARTESIAN_POINT('Ctrl Pts',(19.8406203564623,15.5262459492187,36.1774475979097));
#46406=CARTESIAN_POINT('Ctrl Pts',(19.8190836109324,15.5276675812764,36.1793250722419));
#46407=CARTESIAN_POINT('Ctrl Pts',(19.8057173347676,15.5285550723517,36.1806310546143));
#46408=CARTESIAN_POINT('Ctrl Pts',(19.7040841139346,15.5353440100847,36.1916338423703));
#46409=CARTESIAN_POINT('Ctrl Pts',(19.6165805906557,15.5414307774726,36.2072736473586));
#46410=CARTESIAN_POINT('Ctrl Pts',(19.4845095896841,15.5509787547618,36.2404145359517));
#46411=CARTESIAN_POINT('Ctrl Pts',(19.4390223915042,15.5543337944147,36.2536291837778));
#46412=CARTESIAN_POINT('Ctrl Pts',(19.3941036417061,15.5577020380306,36.2684891046171));
#46413=CARTESIAN_POINT('Origin',(20.,-1.3495818343519,38.1));
#46414=CARTESIAN_POINT('',(19.3941040087494,16.5227836600514,36.2684889831927));
#46415=CARTESIAN_POINT('',(19.3941040086649,16.3533584392964,36.2684889832207));
#46416=CARTESIAN_POINT('',(19.3941040087494,-1.3495818343519,36.2684889831927));
#46417=CARTESIAN_POINT('',(18.0708704087723,15.8870818343519,38.0987441537647));
#46418=CARTESIAN_POINT('Ctrl Pts',(18.0708704087723,15.8870818343519,38.0987441537647));
#46419=CARTESIAN_POINT('Ctrl Pts',(18.0708258299364,15.8915491171253,38.1672225622242));
#46420=CARTESIAN_POINT('Ctrl Pts',(18.0744317560961,15.8960163998987,38.2357215708611));
#46421=CARTESIAN_POINT('Ctrl Pts',(18.0816682478463,15.9004836826721,38.3038279803632));
#46422=CARTESIAN_POINT('Ctrl Pts',(18.0889052732589,15.9049512948898,38.3719394124415));
#46423=CARTESIAN_POINT('Ctrl Pts',(18.0997733431619,15.9094189071075,38.4396577055612));
#46424=CARTESIAN_POINT('Ctrl Pts',(18.1142007319637,15.9138865193252,38.5065755496506));
#46425=CARTESIAN_POINT('Ctrl Pts',(18.12864536736,15.9183594721557,38.5735733877666));
#46426=CARTESIAN_POINT('Ctrl Pts',(18.1466577168547,15.9228324249861,38.6397683902669));
#46427=CARTESIAN_POINT('Ctrl Pts',(18.1681152028847,15.9273053778166,38.7047649518596));
#46428=CARTESIAN_POINT('Ctrl Pts',(18.189585184612,15.9317809354565,38.7697993639888));
#46429=CARTESIAN_POINT('Ctrl Pts',(18.2145041222011,15.9362564930965,38.8336334924981));
#46430=CARTESIAN_POINT('Ctrl Pts',(18.2427009686494,15.9407320507365,38.8958911177505));
#46431=CARTESIAN_POINT('Ctrl Pts',(18.2709554707479,15.9452167597966,38.95827604461));
#46432=CARTESIAN_POINT('Ctrl Pts',(18.3025010510645,15.9497014688567,39.0190775946588));
#46433=CARTESIAN_POINT('Ctrl Pts',(18.3371204938809,15.9541861779167,39.0779439171186));
#46434=CARTESIAN_POINT('Ctrl Pts',(18.3694527402624,15.9583745965186,39.132921128954));
#46435=CARTESIAN_POINT('Ctrl Pts',(18.4044654725367,15.9625630151205,39.1862103874997));
#46436=CARTESIAN_POINT('Ctrl Pts',(18.4419495711134,15.9667514337224,39.2375506221466));
#46437=CARTESIAN_POINT('Ctrl Pts',(18.4818491621624,15.9712097559364,39.2921992450177));
#46438=CARTESIAN_POINT('Ctrl Pts',(18.5247062532375,15.9756680781504,39.3448540605869));
#46439=CARTESIAN_POINT('Ctrl Pts',(18.5702943928871,15.9801264003644,39.3951773754548));
#46440=CARTESIAN_POINT('Ctrl Pts',(18.6181611336226,15.984807559876,39.4480159664622));
#46441=CARTESIAN_POINT('Ctrl Pts',(18.6690388463395,15.9894887193875,39.4982833864635));
#46442=CARTESIAN_POINT('Ctrl Pts',(18.7226143802393,15.9941698788991,39.5456239259672));
#46443=CARTESIAN_POINT('Ctrl Pts',(18.7735011786153,15.9986161102829,39.5905886386518));
#46444=CARTESIAN_POINT('Ctrl Pts',(18.8268211145396,16.0030623416667,39.6329127937645));
#46445=CARTESIAN_POINT('Ctrl Pts',(18.8822667904418,16.0075085730505,39.6723279012823));
#46446=CARTESIAN_POINT('Ctrl Pts',(18.9376789970235,16.0119521205038,39.7117192161987));
#46447=CARTESIAN_POINT('Ctrl Pts',(18.9952139970152,16.016395667957,39.7482046818366));
#46448=CARTESIAN_POINT('Ctrl Pts',(19.054532306503,16.0208392154103,39.7815568374139));
#46449=CARTESIAN_POINT('Ctrl Pts',(19.1138352521738,16.0252816119567,39.8149003545722));
#46450=CARTESIAN_POINT('Ctrl Pts',(19.1749201606235,16.0297240085031,39.8451119313376));
#46451=CARTESIAN_POINT('Ctrl Pts',(19.2374212105004,16.0341664050495,39.8720090707176));
#46452=CARTESIAN_POINT('Ctrl Pts',(19.2999276115479,16.0386091819419,39.8989085129577));
#46453=CARTESIAN_POINT('Ctrl Pts',(19.3638499406723,16.0430519588342,39.9224927620879));
#46454=CARTESIAN_POINT('Ctrl Pts',(19.4288022734454,16.0474947357266,39.9426273942604));
#46455=CARTESIAN_POINT('Ctrl Pts',(19.4938246176439,16.0519423014407,39.9627837293378));
#46456=CARTESIAN_POINT('Ctrl Pts',(19.5598787088476,16.0563898671548,39.9794828822013));
#46457=CARTESIAN_POINT('Ctrl Pts',(19.6265643407354,16.0608374328689,39.9926405800599));
#46458=CARTESIAN_POINT('Ctrl Pts',(19.6932916668657,16.0652877793602,40.005806504582));
#46459=CARTESIAN_POINT('Ctrl Pts',(19.7606508313349,16.0697381258515,40.015426498345));
#46460=CARTESIAN_POINT('Ctrl Pts',(19.8282351350228,16.0741884723427,40.0214680294138));
#46461=CARTESIAN_POINT('Ctrl Pts',(19.8959337368733,16.0786463452329,40.0275197778832));
#46462=CARTESIAN_POINT('Ctrl Pts',(19.9638577454947,16.083104218123,40.029980970682));
#46463=CARTESIAN_POINT('Ctrl Pts',(20.0316000601817,16.0875620910131,40.0288711706842));
#46464=CARTESIAN_POINT('Ctrl Pts',(20.0564818503092,16.0891994702226,40.0284635405234));
#46465=CARTESIAN_POINT('Ctrl Pts',(20.0813391814739,16.090836849432,40.0275746541172));
#46466=CARTESIAN_POINT('Ctrl Pts',(20.106152139383,16.0924742286414,40.0262072267034));
#46467=CARTESIAN_POINT('Ctrl Pts',(20.173713862901,16.0969325508555,40.0224839401367));
#46468=CARTESIAN_POINT('Ctrl Pts',(20.2412129184433,16.1013908730695,40.0151944025013));
#46469=CARTESIAN_POINT('Ctrl Pts',(20.3082427603914,16.1058491952835,40.0043447580641));
#46470=CARTESIAN_POINT('Ctrl Pts',(20.3786229094988,16.1105303547951,39.9929528232027));
#46471=CARTESIAN_POINT('Ctrl Pts',(20.4484851656179,16.1152115143066,39.9776355018037));
#46472=CARTESIAN_POINT('Ctrl Pts',(20.5173606764793,16.1198926738182,39.9584618606076));
#46473=CARTESIAN_POINT('Ctrl Pts',(20.5827796089495,16.124338905202,39.9402504655422));
#46474=CARTESIAN_POINT('Ctrl Pts',(20.6473079064773,16.1287851365858,39.9185606409435));
#46475=CARTESIAN_POINT('Ctrl Pts',(20.7105530140653,16.1332313679696,39.8935041040106));
#46476=CARTESIAN_POINT('Ctrl Pts',(20.7737599442709,16.1376749154228,39.8684626922474));
#46477=CARTESIAN_POINT('Ctrl Pts',(20.8356847635789,16.1421184628761,39.8400587808877));
#46478=CARTESIAN_POINT('Ctrl Pts',(20.8959518693553,16.1465620103294,39.8084533369978));
#46479=CARTESIAN_POINT('Ctrl Pts',(20.9562033655705,16.1510044068758,39.7768560791175));
#46480=CARTESIAN_POINT('Ctrl Pts',(21.014797564158,16.1554468034222,39.7420591639833));
#46481=CARTESIAN_POINT('Ctrl Pts',(21.071382244746,16.1598891999686,39.7042701276727));
#46482=CARTESIAN_POINT('Ctrl Pts',(21.1279717699611,16.164331976861,39.6664778559672));
#46483=CARTESIAN_POINT('Ctrl Pts',(21.1825510270899,16.1687747537533,39.6256932306903));
#46484=CARTESIAN_POINT('Ctrl Pts',(21.234797179945,16.1732175306457,39.5821668196596));
#46485=CARTESIAN_POINT('Ctrl Pts',(21.2870996483701,16.1776650963598,39.5385934919756));
#46486=CARTESIAN_POINT('Ctrl Pts',(21.3370636152442,16.1821126620739,39.4922727980548));
#46487=CARTESIAN_POINT('Ctrl Pts',(21.3844005403343,16.186560227788,39.4434945853341));
#46488=CARTESIAN_POINT('Ctrl Pts',(21.4317670621634,16.1910105742793,39.3946858747298));
#46489=CARTESIAN_POINT('Ctrl Pts',(21.4765029496675,16.1954609207705,39.3434169593205));
#46490=CARTESIAN_POINT('Ctrl Pts',(21.518359532079,16.1999112672618,39.2900112975282));
#46491=CARTESIAN_POINT('Ctrl Pts',(21.5602869020876,16.204369140152,39.2365153164062));
#46492=CARTESIAN_POINT('Ctrl Pts',(21.599324968236,16.2088270130421,39.1808757818233));
#46493=CARTESIAN_POINT('Ctrl Pts',(21.6352685418066,16.2132848859323,39.1234448461338));
#46494=CARTESIAN_POINT('Ctrl Pts',(21.648470636511,16.2149222651417,39.102350431288));
#46495=CARTESIAN_POINT('Ctrl Pts',(21.6612557070673,16.2165596443511,39.0810145693996));
#46496=CARTESIAN_POINT('Ctrl Pts',(21.6736151911431,16.2181970235605,39.0594554439238));
#46497=CARTESIAN_POINT('Ctrl Pts',(21.7072680933499,16.2226553457745,39.0007533867142));
#46498=CARTESIAN_POINT('Ctrl Pts',(21.737895270719,16.2271136679885,38.9401626624699));
#46499=CARTESIAN_POINT('Ctrl Pts',(21.7652805802521,16.2315719902026,38.8780276536762));
#46500=CARTESIAN_POINT('Ctrl Pts',(21.7940346711506,16.2362531497141,38.8127869928512));
#46501=CARTESIAN_POINT('Ctrl Pts',(21.8192139749583,16.2409343092257,38.7458440483039));
#46502=CARTESIAN_POINT('Ctrl Pts',(21.840621216576,16.2456154687372,38.6776297204874));
#46503=CARTESIAN_POINT('Ctrl Pts',(21.8609541168514,16.250061700121,38.6128387890064));
#46504=CARTESIAN_POINT('Ctrl Pts',(21.8778842710905,16.2545079315048,38.5469015495251));
#46505=CARTESIAN_POINT('Ctrl Pts',(21.8912917135977,16.2589541628886,38.4802081153482));
#46506=CARTESIAN_POINT('Ctrl Pts',(21.904691062814,16.2633977103419,38.4135549401073));
#46507=CARTESIAN_POINT('Ctrl Pts',(21.9145718215884,16.2678412577952,38.3461469581401));
#46508=CARTESIAN_POINT('Ctrl Pts',(21.9208645661169,16.2722848052484,38.2783868704155));
#46509=CARTESIAN_POINT('Ctrl Pts',(21.9271556807847,16.2767272017949,38.2106443329817));
#46510=CARTESIAN_POINT('Ctrl Pts',(21.9298605807061,16.2811695983413,38.1425503616818));
#46511=CARTESIAN_POINT('Ctrl Pts',(21.9289616351069,16.2856119948877,38.0745133920303));
#46512=CARTESIAN_POINT('Ctrl Pts',(21.9280626125424,16.29005477178,38.006470597238));
#46513=CARTESIAN_POINT('Ctrl Pts',(21.9235591412097,16.2944975486724,37.9384853068167));
#46514=CARTESIAN_POINT('Ctrl Pts',(21.9154856831222,16.2989403255648,37.8709647305463));
#46515=CARTESIAN_POINT('Ctrl Pts',(21.9074035227406,16.3033878912789,37.8033713745681));
#46516=CARTESIAN_POINT('Ctrl Pts',(21.8957437563881,16.307835456993,37.7362442226867));
#46517=CARTESIAN_POINT('Ctrl Pts',(21.880592464984,16.3122830227071,37.6699830962096));
#46518=CARTESIAN_POINT('Ctrl Pts',(21.8654317004505,16.3167333691984,37.6036805409059));
#46519=CARTESIAN_POINT('Ctrl Pts',(21.846775202115,16.3211837156896,37.5382455625848));
#46520=CARTESIAN_POINT('Ctrl Pts',(21.8247589484297,16.3256340621809,37.474062833005));
#46521=CARTESIAN_POINT('Ctrl Pts',(21.8027054609903,16.3300919350711,37.4097715579841));
#46522=CARTESIAN_POINT('Ctrl Pts',(21.7772810652795,16.3345498079612,37.3467372140123));
#46523=CARTESIAN_POINT('Ctrl Pts',(21.7486694789839,16.3390076808514,37.2853236162928));
#46524=CARTESIAN_POINT('Ctrl Pts',(21.7381604273121,16.3406450600608,37.2627663674526));
#46525=CARTESIAN_POINT('Ctrl Pts',(21.727221832481,16.3422824392702,37.2404275184496));
#46526=CARTESIAN_POINT('Ctrl Pts',(21.7158642872202,16.3439198184796,37.2183241498474));
#46527=CARTESIAN_POINT('Ctrl Pts',(21.6849395044685,16.3483781406936,37.1581402054823));
#46528=CARTESIAN_POINT('Ctrl Pts',(21.6507833706219,16.3528364629077,37.0994663750406));
#46529=CARTESIAN_POINT('Ctrl Pts',(21.6135671226712,16.3572947851217,37.0426714335011));
#46530=CARTESIAN_POINT('Ctrl Pts',(21.5744907202232,16.3619759446332,36.9830377488924));
#46531=CARTESIAN_POINT('Ctrl Pts',(21.5320404435069,16.3666571041448,36.9254762237944));
#46532=CARTESIAN_POINT('Ctrl Pts',(21.4864703771001,16.3713382636563,36.8703869003203));
#46533=CARTESIAN_POINT('Ctrl Pts',(21.443187284755,16.3757844950401,36.8180622832379));
#46534=CARTESIAN_POINT('Ctrl Pts',(21.397090356213,16.380230726424,36.7679681433413));
#46535=CARTESIAN_POINT('Ctrl Pts',(21.3484415432906,16.3846769578078,36.7204174684971));
#46536=CARTESIAN_POINT('Ctrl Pts',(21.299822096819,16.389120505261,36.6728954972217));
#46537=CARTESIAN_POINT('Ctrl Pts',(21.248654173654,16.3935640527143,36.6279142893029));
#46538=CARTESIAN_POINT('Ctrl Pts',(21.1952377967429,16.3980076001676,36.5857512865658));
#46539=CARTESIAN_POINT('Ctrl Pts',(21.1418352550107,16.402449996714,36.5435992043126));
#46540=CARTESIAN_POINT('Ctrl Pts',(21.0861858026918,16.4068923932604,36.5042641834334));
#46541=CARTESIAN_POINT('Ctrl Pts',(21.028622466044,16.4113347898068,36.4679833397758));
#46542=CARTESIAN_POINT('Ctrl Pts',(20.9710542009795,16.4157775666991,36.4316993898507));
#46543=CARTESIAN_POINT('Ctrl Pts',(20.9115721449349,16.4202203435915,36.3984703968417));
#46544=CARTESIAN_POINT('Ctrl Pts',(20.8505366518943,16.4246631204838,36.3684891104344));
#46545=CARTESIAN_POINT('Ctrl Pts',(20.7894353693477,16.4291106861979,36.3384755075187));
#46546=CARTESIAN_POINT('Ctrl Pts',(20.7267777522623,16.433558251912,36.3117168137485));
#46547=CARTESIAN_POINT('Ctrl Pts',(20.6629460546769,16.4380058176261,36.2883584555745));
#46548=CARTESIAN_POINT('Ctrl Pts',(20.5990744472308,16.4424561641174,36.2649854929194));
#46549=CARTESIAN_POINT('Ctrl Pts',(20.534027769881,16.4469065106087,36.2450172410239));
#46550=CARTESIAN_POINT('Ctrl Pts',(20.4682027292008,16.4513568571,36.2285490224778));
#46551=CARTESIAN_POINT('Ctrl Pts',(20.4022663656128,16.4558147299901,36.2120529529808));
#46552=CARTESIAN_POINT('Ctrl Pts',(20.3355494955993,16.4602726028803,36.199068821404));
#46553=CARTESIAN_POINT('Ctrl Pts',(20.2684573160064,16.4647304757704,36.1896405504768));
#46554=CARTESIAN_POINT('Ctrl Pts',(20.2438143208631,16.4663678549799,36.1861775412844));
#46555=CARTESIAN_POINT('Ctrl Pts',(20.2191207186607,16.4680052341893,36.1831937447171));
#46556=CARTESIAN_POINT('Ctrl Pts',(20.1943966037298,16.4696426133987,36.1806895724354));
#46557=CARTESIAN_POINT('Ctrl Pts',(20.127098987393,16.4740994652675,36.1738733597649));
#46558=CARTESIAN_POINT('Ctrl Pts',(20.0593095425683,16.4785563171364,36.1705874988833));
#46559=CARTESIAN_POINT('Ctrl Pts',(19.9914304332523,16.4830131690052,36.1708890339263));
#46560=CARTESIAN_POINT('Ctrl Pts',(19.9236402064552,16.4874641849662,36.1711901741321));
#46561=CARTESIAN_POINT('Ctrl Pts',(19.8557610364843,16.4919152009273,36.175069395944));
#46562=CARTESIAN_POINT('Ctrl Pts',(19.7882002399354,16.4963662168883,36.1825320293323));
#46563=CARTESIAN_POINT('Ctrl Pts',(19.7207080449641,16.5008127132651,36.1899870851245));
#46564=CARTESIAN_POINT('Ctrl Pts',(19.6535340697983,16.5052592096418,36.2010182803379));
#46565=CARTESIAN_POINT('Ctrl Pts',(19.5870837668045,16.5097057060186,36.2155789373753));
#46566=CARTESIAN_POINT('Ctrl Pts',(19.5219362937988,16.5140650240295,36.229854116999));
#46567=CARTESIAN_POINT('Ctrl Pts',(19.4574848266426,16.5184243420404,36.2475214961663));
#46568=CARTESIAN_POINT('Ctrl Pts',(19.3941040087494,16.5227836600514,36.2684889831927));
#46569=CARTESIAN_POINT('Ctrl Pts',(18.0708704684672,15.888364045083,38.0986555789572));
#46570=CARTESIAN_POINT('Ctrl Pts',(18.0708912412105,15.8863049758138,38.0688484639846));
#46571=CARTESIAN_POINT('Ctrl Pts',(18.0716028362428,15.8842285687181,38.0390467538345));
#46572=CARTESIAN_POINT('Ctrl Pts',(18.0806190769073,15.8707814731016,37.8475435862666));
#46573=CARTESIAN_POINT('Ctrl Pts',(18.108562109285,15.8589884944695,37.6874266600154));
#46574=CARTESIAN_POINT('Ctrl Pts',(18.1650638281681,15.8457398489798,37.5037904775019));
#46575=CARTESIAN_POINT('Ctrl Pts',(18.1746331290121,15.8436810920069,37.47510593915));
#46576=CARTESIAN_POINT('Ctrl Pts',(18.1872605696966,15.8411862927403,37.4400242446107));
#46577=CARTESIAN_POINT('Ctrl Pts',(18.1896841193672,15.8407166131998,37.433405178542));
#46578=CARTESIAN_POINT('Ctrl Pts',(18.1935604131709,15.8399797481432,37.4229955302891));
#46579=CARTESIAN_POINT('Ctrl Pts',(18.1949889051835,15.8397111744467,37.4191960772611));
#46580=CARTESIAN_POINT('Ctrl Pts',(18.1976970829768,15.8392075902526,37.4120614032367));
#46581=CARTESIAN_POINT('Ctrl Pts',(18.1989740254791,15.8389724300697,37.4087252666437));
#46582=CARTESIAN_POINT('Ctrl Pts',(18.2019109386235,15.8384367306763,37.4011156739411));
#46583=CARTESIAN_POINT('Ctrl Pts',(18.2035768796426,15.838136550097,37.3968445779438));
#46584=CARTESIAN_POINT('Ctrl Pts',(18.2080355006489,15.8373427614742,37.3855329562127));
#46585=CARTESIAN_POINT('Ctrl Pts',(18.2108544791983,15.8368506721617,37.378502783401));
#46586=CARTESIAN_POINT('Ctrl Pts',(18.2310304380513,15.8333954792238,37.3290319745208));
#46587=CARTESIAN_POINT('Ctrl Pts',(18.249855880067,15.8305134187825,37.2872015364051));
#46588=CARTESIAN_POINT('Ctrl Pts',(18.2830126667148,15.8258883937181,37.2200337155476));
#46589=CARTESIAN_POINT('Ctrl Pts',(18.2964563063084,15.8241158841955,37.1942819596982));
#46590=CARTESIAN_POINT('Ctrl Pts',(18.3732551148158,15.8144771990911,37.0549356056278));
#46591=CARTESIAN_POINT('Ctrl Pts',(18.4473911111264,15.8068583103847,36.9476695806962));
#46592=CARTESIAN_POINT('Ctrl Pts',(18.5644446688361,15.7958651074082,36.8103245298996));
#46593=CARTESIAN_POINT('Ctrl Pts',(18.5986194346535,15.792757314733,36.7732694842231));
#46594=CARTESIAN_POINT('Ctrl Pts',(18.6492168153398,15.7882578975943,36.7225460963469));
#46595=CARTESIAN_POINT('Ctrl Pts',(18.6644772143478,15.7869132016272,36.7077452447665));
#46596=CARTESIAN_POINT('Ctrl Pts',(18.6918729654712,15.7845180812797,36.6820394036079));
#46597=CARTESIAN_POINT('Ctrl Pts',(18.7039080520054,15.7834720983905,36.6710303615469));
#46598=CARTESIAN_POINT('Ctrl Pts',(18.7220785543886,15.7819012294717,36.6548273774493));
#46599=CARTESIAN_POINT('Ctrl Pts',(18.7281093918435,15.7813811980409,36.6495168364326));
#46600=CARTESIAN_POINT('Ctrl Pts',(18.7388183076559,15.7804600449974,36.6402050871432));
#46601=CARTESIAN_POINT('Ctrl Pts',(18.7434827175248,15.7800595726533,36.6361882750554));
#46602=CARTESIAN_POINT('Ctrl Pts',(18.7528300675857,15.7792584791092,36.6282162898978));
#46603=CARTESIAN_POINT('Ctrl Pts',(18.7575127929514,15.7788578702894,36.6242609754751));
#46604=CARTESIAN_POINT('Ctrl Pts',(18.7702376735659,15.7777711216595,36.6136162671512));
#46605=CARTESIAN_POINT('Ctrl Pts',(18.7783154248599,15.7770832565011,36.6069699358751));
#46606=CARTESIAN_POINT('Ctrl Pts',(18.8089611902156,15.7744807752047,36.5821699790695));
#46607=CARTESIAN_POINT('Ctrl Pts',(18.8318820399488,15.7725487276503,36.5644604543241));
#46608=CARTESIAN_POINT('Ctrl Pts',(19.0190996213222,15.756872714049,36.4264269140187));
#46609=CARTESIAN_POINT('Ctrl Pts',(19.2010276616791,15.7420786631794,36.3323620249649));
#46610=CARTESIAN_POINT('Ctrl Pts',(19.3941040321498,15.7277949589794,36.2684889754514));
#46611=CARTESIAN_POINT('Ctrl Pts',(19.3941036417061,15.5577020380306,36.2684891046171));
#46612=CARTESIAN_POINT('Ctrl Pts',(19.2869970961409,15.5657334489655,36.3039218536502));
#46613=CARTESIAN_POINT('Ctrl Pts',(19.1831232854518,15.5738530125418,36.3487083168368));
#46614=CARTESIAN_POINT('Ctrl Pts',(19.0553917185764,15.5838795943166,36.4176528830577));
#46615=CARTESIAN_POINT('Ctrl Pts',(19.0274780399817,15.5860723441457,36.433633304655));
#46616=CARTESIAN_POINT('Ctrl Pts',(18.993831322998,15.5887058060737,36.4540295367776));
#46617=CARTESIAN_POINT('Ctrl Pts',(18.9877083263234,15.5891846387715,36.4577881550207));
#46618=CARTESIAN_POINT('Ctrl Pts',(18.9781335750634,15.5899326002304,36.4637395420871));
#46619=CARTESIAN_POINT('Ctrl Pts',(18.974667628943,15.5902031862987,36.4659091805605));
#46620=CARTESIAN_POINT('Ctrl Pts',(18.9681912005816,15.5907084484641,36.4699920609818));
#46621=CARTESIAN_POINT('Ctrl Pts',(18.9651791590267,15.5909432865005,36.4719026112726));
#46622=CARTESIAN_POINT('Ctrl Pts',(18.9582835531318,15.5914805940458,36.4763033893199));
#46623=CARTESIAN_POINT('Ctrl Pts',(18.9544036140944,15.5917826917262,36.4787991987169));
#46624=CARTESIAN_POINT('Ctrl Pts',(18.9442349812674,15.5925739393219,36.4853919629071));
#46625=CARTESIAN_POINT('Ctrl Pts',(18.9379611040761,15.5930616241092,36.4895117894826));
#46626=CARTESIAN_POINT('Ctrl Pts',(18.8946445730371,15.5964264221926,36.5183193873449));
#46627=CARTESIAN_POINT('Ctrl Pts',(18.8584387820557,15.5992271802138,36.544248451166));
#46628=CARTESIAN_POINT('Ctrl Pts',(18.812831010448,15.6027852741695,36.5793612334981));
#46629=CARTESIAN_POINT('Ctrl Pts',(18.8025831017928,15.603586801466,36.5874176874242));
#46630=CARTESIAN_POINT('Ctrl Pts',(18.6959617403419,15.6119565832057,36.673001423528));
#46631=CARTESIAN_POINT('Ctrl Pts',(18.6071716438318,15.6192085344496,36.7595250644808));
#46632=CARTESIAN_POINT('Ctrl Pts',(18.4846420144578,15.6306457413503,36.9043457506566));
#46633=CARTESIAN_POINT('Ctrl Pts',(18.4446274980962,15.6346721667358,36.956883998806));
#46634=CARTESIAN_POINT('Ctrl Pts',(18.385597510942,15.6412050888006,37.0432417770369));
#46635=CARTESIAN_POINT('Ctrl Pts',(18.3647721701891,15.6436470086323,37.0757622540142));
#46636=CARTESIAN_POINT('Ctrl Pts',(18.3391665132472,15.6468458065496,37.1185210825483));
#46637=CARTESIAN_POINT('Ctrl Pts',(18.3334798199011,15.6475697182027,37.1282082441341));
#46638=CARTESIAN_POINT('Ctrl Pts',(18.3243973422061,15.648748382999,37.1439942430759));
#46639=CARTESIAN_POINT('Ctrl Pts',(18.3209494343859,15.6492012624353,37.1500629125732));
#46640=CARTESIAN_POINT('Ctrl Pts',(18.3143988270053,15.6500722639972,37.1617397378559));
#46641=CARTESIAN_POINT('Ctrl Pts',(18.3112909880277,15.6504901958677,37.167344916303));
#46642=CARTESIAN_POINT('Ctrl Pts',(18.3042594265255,15.6514466535268,37.1801771422932));
#46643=CARTESIAN_POINT('Ctrl Pts',(18.3003538894875,15.6519858131637,37.1874139615466));
#46644=CARTESIAN_POINT('Ctrl Pts',(18.2901370557493,15.6534175664577,37.206638480791));
#46645=CARTESIAN_POINT('Ctrl Pts',(18.2839056546269,15.6543129357391,37.218667897973));
#46646=CARTESIAN_POINT('Ctrl Pts',(18.2356481551378,15.6614265674354,37.3142791795196));
#46647=CARTESIAN_POINT('Ctrl Pts',(18.1996322050242,15.6678514045526,37.4007391986645));
#46648=CARTESIAN_POINT('Ctrl Pts',(18.1196494045866,15.6856107167885,37.6404706421115));
#46649=CARTESIAN_POINT('Ctrl Pts',(18.0881546282936,15.6971993715924,37.7971291161458));
#46650=CARTESIAN_POINT('Ctrl Pts',(18.0741080035625,15.7101467503915,37.9846162497938));
#46651=CARTESIAN_POINT('Ctrl Pts',(18.0725988536963,15.7121076618656,38.013406506713));
#46652=CARTESIAN_POINT('Ctrl Pts',(18.0715274966347,15.7145005989365,38.0491613869317));
#46653=CARTESIAN_POINT('Ctrl Pts',(18.0713570150662,15.714963153547,38.0561023792882));
#46654=CARTESIAN_POINT('Ctrl Pts',(18.0711466967848,15.7156913730726,38.0670792116388));
#46655=CARTESIAN_POINT('Ctrl Pts',(18.0710820472771,15.715958373322,38.0711144320343));
#46656=CARTESIAN_POINT('Ctrl Pts',(18.0709839831674,15.7164606873023,38.0787265745219));
#46657=CARTESIAN_POINT('Ctrl Pts',(18.070947854407,15.7166961410382,38.0823033437412));
#46658=CARTESIAN_POINT('Ctrl Pts',(18.0708878345154,15.7172346571461,38.0905034407253));
#46659=CARTESIAN_POINT('Ctrl Pts',(18.0708706149258,15.7175373470127,38.0951267672208));
#46660=CARTESIAN_POINT('Ctrl Pts',(18.0708687175602,15.7184937220807,38.1097777941016));
#46661=CARTESIAN_POINT('Ctrl Pts',(18.0709456043656,15.7191441023902,38.1198055367509));
#46662=CARTESIAN_POINT('Ctrl Pts',(18.0725489127073,15.7258284678507,38.2234717436469));
#46663=CARTESIAN_POINT('Ctrl Pts',(18.0808141358278,15.7315243111535,38.3168952652223));
#46664=CARTESIAN_POINT('Ctrl Pts',(18.1239389744769,15.7476723293987,38.5823360778873));
#46665=CARTESIAN_POINT('Ctrl Pts',(18.175474274834,15.7579487416281,38.7506564847968));
#46666=CARTESIAN_POINT('Ctrl Pts',(18.2572446703788,15.7703215911005,38.9274842366739));
#46667=CARTESIAN_POINT('Ctrl Pts',(18.2657369204047,15.7715743681337,38.9451377561642));
#46668=CARTESIAN_POINT('Ctrl Pts',(18.2780829696466,15.7733530898951,38.9698325298594));
#46669=CARTESIAN_POINT('Ctrl Pts',(18.2817143116101,15.7738713533578,38.9769841385757));
#46670=CARTESIAN_POINT('Ctrl Pts',(18.2881197570375,15.7747771804813,38.9894065806581));
#46671=CARTESIAN_POINT('Ctrl Pts',(18.2908738881414,15.7751640441944,38.9946876351029));
#46672=CARTESIAN_POINT('Ctrl Pts',(18.2966886942705,15.7759754567683,39.0057127103645));
#46673=CARTESIAN_POINT('Ctrl Pts',(18.299754065628,15.7764001668133,39.0114541562005));
#46674=CARTESIAN_POINT('Ctrl Pts',(18.307115635575,15.7774130159262,39.0250760202525));
#46675=CARTESIAN_POINT('Ctrl Pts',(18.3114378612145,15.77800206908,39.0329421275891));
#46676=CARTESIAN_POINT('Ctrl Pts',(18.3262071033728,15.7799963451693,39.0593821040779));
#46677=CARTESIAN_POINT('Ctrl Pts',(18.3369066344292,15.7814105163175,39.0778123941949));
#46678=CARTESIAN_POINT('Ctrl Pts',(18.3977756341009,15.7892943747446,39.1787711966674));
#46679=CARTESIAN_POINT('Ctrl Pts',(18.4537753268077,15.795975443966,39.2576072008973));
#46680=CARTESIAN_POINT('Ctrl Pts',(18.5988347376314,15.8120167046537,39.4324173471321));
#46681=CARTESIAN_POINT('Ctrl Pts',(18.6922247669043,15.8214620944786,39.5241922487582));
#46682=CARTESIAN_POINT('Ctrl Pts',(18.8273877902515,15.8335304431883,39.6324275422832));
#46683=CARTESIAN_POINT('Ctrl Pts',(18.8614799810774,15.8364540505741,39.6579237378771));
#46684=CARTESIAN_POINT('Ctrl Pts',(18.9024682167112,15.8398058305002,39.6865123538986));
#46685=CARTESIAN_POINT('Ctrl Pts',(18.9085703629601,15.8403007085932,39.6907164474301));
#46686=CARTESIAN_POINT('Ctrl Pts',(18.9184869940928,15.8410980990487,39.6974646142678));
#46687=CARTESIAN_POINT('Ctrl Pts',(18.9222865184618,15.8414020057658,39.7000303836402));
#46688=CARTESIAN_POINT('Ctrl Pts',(18.9290559442393,15.8419405538096,39.7045666357803));
#46689=CARTESIAN_POINT('Ctrl Pts',(18.932022190421,15.8421755475241,39.7065424545358));
#46690=CARTESIAN_POINT('Ctrl Pts',(18.9384188786956,15.8426801756568,39.7107777475625));
#46691=CARTESIAN_POINT('Ctrl Pts',(18.9418510593831,15.8429496286759,39.713034484877));
#46692=CARTESIAN_POINT('Ctrl Pts',(18.9513770459187,15.8436939548103,39.7192545502481));
#46693=CARTESIAN_POINT('Ctrl Pts',(18.9574861632985,15.8441673067411,39.7231944747047));
#46694=CARTESIAN_POINT('Ctrl Pts',(18.9918147323132,15.8468057779922,39.7450600826409));
#46695=CARTESIAN_POINT('Ctrl Pts',(19.0204761370866,15.8489281310645,39.7622856369383));
#46696=CARTESIAN_POINT('Ctrl Pts',(19.1130622147582,15.8555794946669,39.8147031302438));
#46697=CARTESIAN_POINT('Ctrl Pts',(19.1785450580316,15.8599836043246,39.8470200338396));
#46698=CARTESIAN_POINT('Ctrl Pts',(19.3978167480666,15.874256711025,39.9401715287537));
#46699=CARTESIAN_POINT('Ctrl Pts',(19.5575809925073,15.8839960978198,39.9849709489789));
#46700=CARTESIAN_POINT('Ctrl Pts',(19.741617304748,15.8957939248933,40.0118606410352));
#46701=CARTESIAN_POINT('Ctrl Pts',(19.7621863248979,15.8971192127927,40.0145279655806));
#46702=CARTESIAN_POINT('Ctrl Pts',(19.7909587415547,15.8989840057287,40.0177882658027));
#46703=CARTESIAN_POINT('Ctrl Pts',(19.7991294676282,15.899514791359,40.0186612796394));
#46704=CARTESIAN_POINT('Ctrl Pts',(19.813280958913,15.9004363244824,40.0200819314596));
#46705=CARTESIAN_POINT('Ctrl Pts',(19.8192592099493,15.9008263094618,40.0206538962762));
#46706=CARTESIAN_POINT('Ctrl Pts',(19.831683892206,15.9016382905178,40.0217840961897));
#46707=CARTESIAN_POINT('Ctrl Pts',(19.8381306473514,15.9020604215699,40.0223378307354));
#46708=CARTESIAN_POINT('Ctrl Pts',(19.8533099954289,15.9030563484596,40.02356474031));
#46709=CARTESIAN_POINT('Ctrl Pts',(19.8620445700562,15.9036309777231,40.0242108935067));
#46710=CARTESIAN_POINT('Ctrl Pts',(19.8907857816746,15.9055270648773,40.0261403689782));
#46711=CARTESIAN_POINT('Ctrl Pts',(19.9108074904933,15.9068563147904,40.0271712719554));
#46712=CARTESIAN_POINT('Ctrl Pts',(20.0166666201352,15.9139311224526,40.0309687453286));
#46713=CARTESIAN_POINT('Ctrl Pts',(20.1025899923874,15.9198423254634,40.028312663476));
#46714=CARTESIAN_POINT('Ctrl Pts',(20.3225121917313,15.9353708769068,40.006773311396));
#46715=CARTESIAN_POINT('Ctrl Pts',(20.4552192054987,15.9451469449962,39.9795136485195));
#46716=CARTESIAN_POINT('Ctrl Pts',(20.5995649313296,15.9557553068453,39.9336661778171));
#46717=CARTESIAN_POINT('Ctrl Pts',(20.6150811552164,15.9568948008357,39.9285198820794));
#46718=CARTESIAN_POINT('Ctrl Pts',(20.6636095378439,15.9604524176345,39.9117367463128));
#46719=CARTESIAN_POINT('Ctrl Pts',(20.6963737282762,15.9628452633845,39.8993975832509));
#46720=CARTESIAN_POINT('Ctrl Pts',(20.7352565521427,15.9656593243584,39.8835327841649));
#46721=CARTESIAN_POINT('Ctrl Pts',(20.7417124800203,15.9661256939503,39.8808576558203));
#46722=CARTESIAN_POINT('Ctrl Pts',(20.7522616973358,15.9668861735468,39.8764190826822));
#46723=CARTESIAN_POINT('Ctrl Pts',(20.7563635958752,15.967181479647,39.8746764579557));
#46724=CARTESIAN_POINT('Ctrl Pts',(20.7637258773089,15.9677107510131,39.8715185501777));
#46725=CARTESIAN_POINT('Ctrl Pts',(20.7669884039073,15.9679450208548,39.8701084650987));
#46726=CARTESIAN_POINT('Ctrl Pts',(20.7740986930358,15.9684549872236,39.8670120029411));
#46727=CARTESIAN_POINT('Ctrl Pts',(20.7779448407974,15.9687304654288,39.8653220756013));
#46728=CARTESIAN_POINT('Ctrl Pts',(20.7888238260632,15.9695086837216,39.860499588454));
#46729=CARTESIAN_POINT('Ctrl Pts',(20.7958435731577,15.9700096677815,39.8573374295857));
#46730=CARTESIAN_POINT('Ctrl Pts',(20.8400547107147,15.9731586927237,39.8371025577971));
#46731=CARTESIAN_POINT('Ctrl Pts',(20.8767169876627,15.9757421504856,39.8188906625709));
#46732=CARTESIAN_POINT('Ctrl Pts',(21.1017175270485,15.9915914328455,39.6980481150119));
#46733=CARTESIAN_POINT('Ctrl Pts',(21.2724227389719,16.0037652492423,39.5657755505596));
#46734=CARTESIAN_POINT('Ctrl Pts',(21.4221805566214,16.0176209350939,39.403451286135));
#46735=CARTESIAN_POINT('Ctrl Pts',(21.4264586119289,16.0180197334227,39.3987681155713));
#46736=CARTESIAN_POINT('Ctrl Pts',(21.4492062243499,16.0201565495294,39.3736184198046));
#46737=CARTESIAN_POINT('Ctrl Pts',(21.4672578155048,16.0219101934134,39.3527796858451));
#46738=CARTESIAN_POINT('Ctrl Pts',(21.4914029399349,16.024341247279,39.3236686629225));
#46739=CARTESIAN_POINT('Ctrl Pts',(21.4978867322923,16.0250029016052,39.3157232647534));
#46740=CARTESIAN_POINT('Ctrl Pts',(21.508119262313,16.0260615121883,39.3029779437222));
#46741=CARTESIAN_POINT('Ctrl Pts',(21.5119092150417,16.0264568223624,39.2982112361784));
#46742=CARTESIAN_POINT('Ctrl Pts',(21.5196497931874,16.0272709012468,39.2883805425136));
#46743=CARTESIAN_POINT('Ctrl Pts',(21.5235978217379,16.0276897654326,39.2833146173721));
#46744=CARTESIAN_POINT('Ctrl Pts',(21.5326859620323,16.0286625306022,39.2715322570529));
#46745=CARTESIAN_POINT('Ctrl Pts',(21.5378073182029,16.0292171552301,39.2648015864387));
#46746=CARTESIAN_POINT('Ctrl Pts',(21.5539176154117,16.0309826429167,39.2433374095512));
#46747=CARTESIAN_POINT('Ctrl Pts',(21.5647400614439,16.0321998892498,39.2284807876686));
#46748=CARTESIAN_POINT('Ctrl Pts',(21.6174000396667,16.0382827099655,39.1539770830104));
#46749=CARTESIAN_POINT('Ctrl Pts',(21.656042610418,16.0432661215702,39.0921548099639));
#46750=CARTESIAN_POINT('Ctrl Pts',(21.7602152333657,16.0583711125733,38.9023829117062));
#46751=CARTESIAN_POINT('Ctrl Pts',(21.815049972143,16.0687664173458,38.7691517164068));
#46752=CARTESIAN_POINT('Ctrl Pts',(21.8583464299399,16.0798248207854,38.6179550335928));
#46753=CARTESIAN_POINT('Ctrl Pts',(21.8619647960517,16.0807811953353,38.604793010247));
#46754=CARTESIAN_POINT('Ctrl Pts',(21.8765968061019,16.0847865554465,38.5492691126538));
#46755=CARTESIAN_POINT('Ctrl Pts',(21.8863077688563,16.0877958052176,38.506573485836));
#46756=CARTESIAN_POINT('Ctrl Pts',(21.8959661438272,16.091233408145,38.4562453224704));
#46757=CARTESIAN_POINT('Ctrl Pts',(21.8973312991366,16.0917323021278,38.4489015535523));
#46758=CARTESIAN_POINT('Ctrl Pts',(21.8994686545502,16.0925348780592,38.4370201329837));
#46759=CARTESIAN_POINT('Ctrl Pts',(21.9002673136042,16.0928399833277,38.4324874096735));
#46760=CARTESIAN_POINT('Ctrl Pts',(21.9016559350232,16.0933798484322,38.4244379393035));
#46761=CARTESIAN_POINT('Ctrl Pts',(21.9022523758598,16.0936149672875,38.4209223752977));
#46762=CARTESIAN_POINT('Ctrl Pts',(21.9035129904778,16.0941189622365,38.41336500823));
#46763=CARTESIAN_POINT('Ctrl Pts',(21.9041740395822,16.0943876616608,38.4093227457755));
#46764=CARTESIAN_POINT('Ctrl Pts',(21.9059641175534,16.0951277795626,38.3981533321763));
#46765=CARTESIAN_POINT('Ctrl Pts',(21.9070660540942,16.0955977049496,38.3910218140008));
#46766=CARTESIAN_POINT('Ctrl Pts',(21.9129288647931,16.0981807192963,38.3516149174707));
#46767=CARTESIAN_POINT('Ctrl Pts',(21.9169107556176,16.1002531274229,38.3192267528916));
#46768=CARTESIAN_POINT('Ctrl Pts',(21.9268512776214,16.1066780338116,38.2170238135291));
#46769=CARTESIAN_POINT('Ctrl Pts',(21.9298304492828,16.1109152445045,38.146973058454));
#46770=CARTESIAN_POINT('Ctrl Pts',(21.9269596624187,16.1252991119664,37.907136373432));
#46771=CARTESIAN_POINT('Ctrl Pts',(21.902526078526,16.1352823332234,37.7383940334527));
#46772=CARTESIAN_POINT('Ctrl Pts',(21.8508071594415,16.1473439614687,37.5555122877789));
#46773=CARTESIAN_POINT('Ctrl Pts',(21.8449799101426,16.1486405512961,37.5360823714243));
#46774=CARTESIAN_POINT('Ctrl Pts',(21.8363899095221,16.1504705897332,37.5090002257812));
#46775=CARTESIAN_POINT('Ctrl Pts',(21.833883363494,16.1509957333026,37.5012676401687));
#46776=CARTESIAN_POINT('Ctrl Pts',(21.8294471914287,16.1519101756742,37.4878714776959));
#46777=CARTESIAN_POINT('Ctrl Pts',(21.8275399348718,16.1522987403073,37.4822005672105));
#46778=CARTESIAN_POINT('Ctrl Pts',(21.8235099535232,16.1531103893557,37.4704000605686));
#46779=CARTESIAN_POINT('Ctrl Pts',(21.8213826342789,16.1535336203286,37.4642721241306));
#46780=CARTESIAN_POINT('Ctrl Pts',(21.8162790875504,16.1545368745571,37.4498067960898));
#46781=CARTESIAN_POINT('Ctrl Pts',(21.8132763167223,16.1551177660886,37.4414789896335));
#46782=CARTESIAN_POINT('Ctrl Pts',(21.8030994121153,16.1570560499383,37.4138520654741));
#46783=CARTESIAN_POINT('Ctrl Pts',(21.7956738475728,16.1584217208557,37.3946477081509));
#46784=CARTESIAN_POINT('Ctrl Pts',(21.7540038472708,16.16583713931,37.2918038083168));
#46785=CARTESIAN_POINT('Ctrl Pts',(21.7142259252815,16.1720710294932,37.2105418146579));
#46786=CARTESIAN_POINT('Ctrl Pts',(21.6072983958624,16.1870841695487,37.0261189922751));
#46787=CARTESIAN_POINT('Ctrl Pts',(21.535687663546,16.1959494295251,36.9259939225626));
#46788=CARTESIAN_POINT('Ctrl Pts',(21.446113193511,16.2055419127306,36.8230958078543));
#46789=CARTESIAN_POINT('Ctrl Pts',(21.4370710713829,16.2064952558663,36.8129279606627));
#46790=CARTESIAN_POINT('Ctrl Pts',(21.3984569386715,16.2105013188572,36.7704207395617));
#46791=CARTESIAN_POINT('Ctrl Pts',(21.3678925207309,16.2135142061465,36.7389953846546));
#46792=CARTESIAN_POINT('Ctrl Pts',(21.3308925545814,16.2169554499253,36.7034602069073));
#46793=CARTESIAN_POINT('Ctrl Pts',(21.3254734278085,16.2174545122743,36.698315805132));
#46794=CARTESIAN_POINT('Ctrl Pts',(21.3166675937732,16.2182573055299,36.6900531236828));
#46795=CARTESIAN_POINT('Ctrl Pts',(21.3132994395944,16.2185624609764,36.6869153140806));
#46796=CARTESIAN_POINT('Ctrl Pts',(21.3073022842271,16.2191023813366,36.681368261367));
#46797=CARTESIAN_POINT('Ctrl Pts',(21.3046778052385,16.2193375055471,36.6789542240014));
#46798=CARTESIAN_POINT('Ctrl Pts',(21.2990246834704,16.2198414745197,36.6737832559247));
#46799=CARTESIAN_POINT('Ctrl Pts',(21.2959939567884,16.2201101428084,36.67102869375));
#46800=CARTESIAN_POINT('Ctrl Pts',(21.2876007113126,16.2208500869718,36.663448920715));
#46801=CARTESIAN_POINT('Ctrl Pts',(21.2822197962694,16.2213198709107,36.6586440435366));
#46802=CARTESIAN_POINT('Ctrl Pts',(21.2523803710457,16.2239006280113,36.6322983358931));
#46803=CARTESIAN_POINT('Ctrl Pts',(21.2274042923977,16.2259710040507,36.6113483360834));
#46804=CARTESIAN_POINT('Ctrl Pts',(21.1472007481222,16.2323868092534,36.5474651060373));
#46805=CARTESIAN_POINT('Ctrl Pts',(21.0901599992564,16.2366173288045,36.5068939345288));
#46806=CARTESIAN_POINT('Ctrl Pts',(20.8873717884223,16.2510063943458,36.3786613475407));
#46807=CARTESIAN_POINT('Ctrl Pts',(20.7323481303306,16.2610000385843,36.3072099643337));
#46808=CARTESIAN_POINT('Ctrl Pts',(20.5506201225371,16.2730725399204,36.2510082750945));
#46809=CARTESIAN_POINT('Ctrl Pts',(20.531174649527,16.2743674328571,36.2453285033589));
#46810=CARTESIAN_POINT('Ctrl Pts',(20.5038105973388,16.2761954658364,36.2378014492333));
#46811=CARTESIAN_POINT('Ctrl Pts',(20.4959638526631,16.2767203253261,36.2356962656227));
#46812=CARTESIAN_POINT('Ctrl Pts',(20.4823168372403,16.2776344112656,36.2321271967539));
#46813=CARTESIAN_POINT('Ctrl Pts',(20.4765225791104,16.2780229049668,36.2306405988007));
#46814=CARTESIAN_POINT('Ctrl Pts',(20.4644300846062,16.278834540476,36.2275979753454));
#46815=CARTESIAN_POINT('Ctrl Pts',(20.4581307350189,16.2792578294344,36.2260467259486));
#46816=CARTESIAN_POINT('Ctrl Pts',(20.4432125706244,16.2802614650448,36.2224527622065));
#46817=CARTESIAN_POINT('Ctrl Pts',(20.434587334874,16.2808426817892,36.2204375889954));
#46818=CARTESIAN_POINT('Ctrl Pts',(20.4058397606352,16.282783174912,36.2139295514483));
#46819=CARTESIAN_POINT('Ctrl Pts',(20.3856598772002,16.2841507557915,36.2097000101705));
#46820=CARTESIAN_POINT('Ctrl Pts',(20.2764405878086,16.2915842950627,36.1886301936745));
#46821=CARTESIAN_POINT('Ctrl Pts',(20.1863786603329,16.2978354107713,36.1777584165985));
#46822=CARTESIAN_POINT('Ctrl Pts',(20.0037008364913,16.3107178574364,36.1686662355575));
#46823=CARTESIAN_POINT('Ctrl Pts',(19.9112963063757,16.3173377122446,36.1707011108718));
#46824=CARTESIAN_POINT('Ctrl Pts',(19.7338807752746,16.3300094562802,36.1873837410124));
#46825=CARTESIAN_POINT('Ctrl Pts',(19.6489849581971,16.3360532915388,36.2011286245633));
#46826=CARTESIAN_POINT('Ctrl Pts',(19.556151955251,16.3424575820897,36.2226004069515));
#46827=CARTESIAN_POINT('Ctrl Pts',(19.5470400522203,16.3430839158982,36.2247779829559));
#46828=CARTESIAN_POINT('Ctrl Pts',(19.5335308176872,16.3440087721624,36.2281106545147));
#46829=CARTESIAN_POINT('Ctrl Pts',(19.5291212900785,16.3443100588853,36.2292150146577));
#46830=CARTESIAN_POINT('Ctrl Pts',(19.5212648856942,16.3448457472243,36.2312121777692));
#46831=CARTESIAN_POINT('Ctrl Pts',(19.5178165464636,16.3450804867097,36.2320989447926));
#46832=CARTESIAN_POINT('Ctrl Pts',(19.5103695401307,16.3455865873703,36.2340359968137));
#46833=CARTESIAN_POINT('Ctrl Pts',(19.5063717969718,16.3458577564778,36.2350895875706));
#46834=CARTESIAN_POINT('Ctrl Pts',(19.4952366903268,16.3466116892272,36.2380625190705));
#46835=CARTESIAN_POINT('Ctrl Pts',(19.488106829744,16.3470928666756,36.2400100623306));
#46836=CARTESIAN_POINT('Ctrl Pts',(19.4518241462968,16.3495343189641,36.2501452218776));
#46837=CARTESIAN_POINT('Ctrl Pts',(19.4228546889411,16.3514599956209,36.2589777535486));
#46838=CARTESIAN_POINT('Ctrl Pts',(19.3941040086649,16.3533584392964,36.2684889832207));
#46839=CARTESIAN_POINT('Origin',(20.,-1.3495818343519,38.1));
#46840=CARTESIAN_POINT('',(19.3941042778786,17.3167366370521,36.2684888941601));
#46841=CARTESIAN_POINT('',(19.3941038273433,17.1441450759092,36.2684890432051));
#46842=CARTESIAN_POINT('',(19.3941040087494,-1.3495818343519,36.2684889831927));
#46843=CARTESIAN_POINT('',(18.0708706155933,16.6808318343519,38.1015411420322));
#46844=CARTESIAN_POINT('Ctrl Pts',(19.3941042778785,17.3167366370521,36.2684888941601));
#46845=CARTESIAN_POINT('Ctrl Pts',(19.4281871155912,17.3145880936754,36.2572136987753));
#46846=CARTESIAN_POINT('Ctrl Pts',(19.46260186465,17.3124312953361,36.2468841883503));
#46847=CARTESIAN_POINT('Ctrl Pts',(19.5829650804439,17.304887334255,36.2143977898005));
#46848=CARTESIAN_POINT('Ctrl Pts',(19.6701023250286,17.2994185812263,36.1972182799032));
#46849=CARTESIAN_POINT('Ctrl Pts',(19.7714268990586,17.2928953712717,36.18441204836));
#46850=CARTESIAN_POINT('Ctrl Pts',(19.7847656655755,17.2920335568093,36.18286749816));
#46851=CARTESIAN_POINT('Ctrl Pts',(19.8062624355353,17.2906392378957,36.1806054706029));
#46852=CARTESIAN_POINT('Ctrl Pts',(19.8144109346658,17.2901094624296,36.179800453392));
#46853=CARTESIAN_POINT('Ctrl Pts',(19.8289411902752,17.2891624473647,36.1784583133964));
#46854=CARTESIAN_POINT('Ctrl Pts',(19.8353209993806,17.2887458419386,36.1779010444703));
#46855=CARTESIAN_POINT('Ctrl Pts',(19.8486769192441,17.2878719685739,36.1768014034601));
#46856=CARTESIAN_POINT('Ctrl Pts',(19.8556534306891,17.2874145147964,36.1762651996013));
#46857=CARTESIAN_POINT('Ctrl Pts',(19.8739153474177,17.28621442272,36.1749615157659));
#46858=CARTESIAN_POINT('Ctrl Pts',(19.8852047239045,17.2854698900579,36.174255328249));
#46859=CARTESIAN_POINT('Ctrl Pts',(19.9358376520919,17.2821183369448,36.1715348821427));
#46860=CARTESIAN_POINT('Ctrl Pts',(19.9752287091522,17.2794773243628,36.1706269110206));
#46861=CARTESIAN_POINT('Ctrl Pts',(20.1787082841269,17.265650624921,36.1721687849205));
#46862=CARTESIAN_POINT('Ctrl Pts',(20.3419495258714,17.253858496796,36.194344631026));
#46863=CARTESIAN_POINT('Ctrl Pts',(20.5783598985063,17.2364751141869,36.2578375345807));
#46864=CARTESIAN_POINT('Ctrl Pts',(20.6549620945363,17.2308080596357,36.2836601153899));
#46865=CARTESIAN_POINT('Ctrl Pts',(20.7383646899343,17.2247527887509,36.317740987687));
#46866=CARTESIAN_POINT('Ctrl Pts',(20.7469757608084,17.2241290478238,36.3213328519177));
#46867=CARTESIAN_POINT('Ctrl Pts',(20.7597361889154,17.2232072659518,36.3267645180577));
#46868=CARTESIAN_POINT('Ctrl Pts',(20.7639055024686,17.2229064868673,36.328556651905));
#46869=CARTESIAN_POINT('Ctrl Pts',(20.7713340820626,17.2223713488074,36.3317808496668));
#46870=CARTESIAN_POINT('Ctrl Pts',(20.7745957361451,17.2221366547824,36.333207234558));
#46871=CARTESIAN_POINT('Ctrl Pts',(20.7816416246043,17.2216302521696,36.3363118009727));
#46872=CARTESIAN_POINT('Ctrl Pts',(20.7854244030634,17.2213587377764,36.337993132655));
#46873=CARTESIAN_POINT('Ctrl Pts',(20.7959682379737,17.2206028700787,36.3427202531467));
#46874=CARTESIAN_POINT('Ctrl Pts',(20.8027172779841,17.2201201162039,36.3457929083102));
#46875=CARTESIAN_POINT('Ctrl Pts',(20.84191862705,17.2173213742833,36.3639138361014));
#46876=CARTESIAN_POINT('Ctrl Pts',(20.8739674772866,17.2150544910922,36.3798246057999));
#46877=CARTESIAN_POINT('Ctrl Pts',(20.9778730853969,17.2077154139262,36.4350632768938));
#46878=CARTESIAN_POINT('Ctrl Pts',(21.0476732303559,17.2027997698563,36.4780773414972));
#46879=CARTESIAN_POINT('Ctrl Pts',(21.2387556794776,17.1888041565934,36.6133293554147));
#46880=CARTESIAN_POINT('Ctrl Pts',(21.3521221612718,17.1797765042327,36.715635660708));
#46881=CARTESIAN_POINT('Ctrl Pts',(21.4666200602742,17.1687542590053,36.8465877075465));
#46882=CARTESIAN_POINT('Ctrl Pts',(21.4806748970894,17.1673637889837,36.8632225082155));
#46883=CARTESIAN_POINT('Ctrl Pts',(21.4997488994942,17.1654219495028,36.8865890421413));
#46884=CARTESIAN_POINT('Ctrl Pts',(21.5050106001505,17.1648802892535,36.8931213797629));
#46885=CARTESIAN_POINT('Ctrl Pts',(21.5139936709352,17.163945031626,36.904423853835));
#46886=CARTESIAN_POINT('Ctrl Pts',(21.517735540974,17.1635522521395,36.9091776021621));
#46887=CARTESIAN_POINT('Ctrl Pts',(21.5254163031002,17.1627393173712,36.919030409412));
#46888=CARTESIAN_POINT('Ctrl Pts',(21.5293521288331,17.1623190485116,36.9241317522757));
#46889=CARTESIAN_POINT('Ctrl Pts',(21.5384763259027,17.1613360186798,36.9360812027116));
#46890=CARTESIAN_POINT('Ctrl Pts',(21.5436446186186,17.1607724854494,36.9429444008907));
#46891=CARTESIAN_POINT('Ctrl Pts',(21.5601610435394,17.1589496089931,36.9651848987605));
#46892=CARTESIAN_POINT('Ctrl Pts',(21.5713262743592,17.1576832814578,36.9806959792602));
#46893=CARTESIAN_POINT('Ctrl Pts',(21.6271218040417,17.1511757134947,37.0606892435713));
#46894=CARTESIAN_POINT('Ctrl Pts',(21.6680153232685,17.1457972521931,37.1276758365361));
#46895=CARTESIAN_POINT('Ctrl Pts',(21.7437826644862,17.1344675250176,37.2707053720839));
#46896=CARTESIAN_POINT('Ctrl Pts',(21.7780204811686,17.1285129506588,37.3469069363996));
#46897=CARTESIAN_POINT('Ctrl Pts',(21.845512231974,17.1147494020431,37.5276279218981));
#46898=CARTESIAN_POINT('Ctrl Pts',(21.8750164121986,17.1069615102386,37.6332618751013));
#46899=CARTESIAN_POINT('Ctrl Pts',(21.8971077617695,17.0989890865743,37.7498447409936));
#46900=CARTESIAN_POINT('Ctrl Pts',(21.8987500320998,17.098376455114,37.7588623607206));
#46901=CARTESIAN_POINT('Ctrl Pts',(21.9011036501247,17.0974678623231,37.7723297879298));
#46902=CARTESIAN_POINT('Ctrl Pts',(21.9018637507879,17.0971692735105,37.7767707766027));
#46903=CARTESIAN_POINT('Ctrl Pts',(21.9031961446014,17.096636499546,37.7847229045073));
#46904=CARTESIAN_POINT('Ctrl Pts',(21.9037742888977,17.0964019915165,37.7882329886122));
#46905=CARTESIAN_POINT('Ctrl Pts',(21.905007978081,17.0958942368306,37.7958544873169));
#46906=CARTESIAN_POINT('Ctrl Pts',(21.9056599229384,17.0956211937426,37.79996642129));
#46907=CARTESIAN_POINT('Ctrl Pts',(21.9074527515177,17.0948567319759,37.8115157322452));
#46908=CARTESIAN_POINT('Ctrl Pts',(21.90856345719,17.0943669721446,37.8189578209101));
#46909=CARTESIAN_POINT('Ctrl Pts',(21.9149698209953,17.0914402952128,37.8636730003941));
#46910=CARTESIAN_POINT('Ctrl Pts',(21.9192174248217,17.0890578768056,37.9010909816715));
#46911=CARTESIAN_POINT('Ctrl Pts',(21.9361722578641,17.076441613781,38.1030481244513));
#46912=CARTESIAN_POINT('Ctrl Pts',(21.9288237836707,17.066909168669,38.2685877918623));
#46913=CARTESIAN_POINT('Ctrl Pts',(21.886992507127,17.0520938115641,38.508635064019));
#46914=CARTESIAN_POINT('Ctrl Pts',(21.8687754774423,17.047224201557,38.5851796416428));
#46915=CARTESIAN_POINT('Ctrl Pts',(21.8421278896749,17.0413627331971,38.6729570505444));
#46916=CARTESIAN_POINT('Ctrl Pts',(21.8381857813128,17.0405198042687,38.6854809675704));
#46917=CARTESIAN_POINT('Ctrl Pts',(21.8315783806381,17.039144505992,38.7057476598368));
#46918=CARTESIAN_POINT('Ctrl Pts',(21.8289910464911,17.0386146764053,38.7135155582986));
#46919=CARTESIAN_POINT('Ctrl Pts',(21.8242977037496,17.0376686871039,38.7273127048152));
#46920=CARTESIAN_POINT('Ctrl Pts',(21.8222110437213,17.0372531668932,38.7333484444092));
#46921=CARTESIAN_POINT('Ctrl Pts',(21.8177519505329,17.0363756875683,38.7460420717497));
#46922=CARTESIAN_POINT('Ctrl Pts',(21.8153728250399,17.0359135131126,38.7526974919599));
#46923=CARTESIAN_POINT('Ctrl Pts',(21.8089817574152,17.034687518446,38.7702707301721));
#46924=CARTESIAN_POINT('Ctrl Pts',(21.8049076032049,17.0339216514101,38.7811654602706));
#46925=CARTESIAN_POINT('Ctrl Pts',(21.7853930729776,17.0303242772647,38.8319448833872));
#46926=CARTESIAN_POINT('Ctrl Pts',(21.7687286524114,17.0274523476216,38.8713431151353));
#46927=CARTESIAN_POINT('Ctrl Pts',(21.6807703592888,17.0131834111643,39.0614242660291));
#46928=CARTESIAN_POINT('Ctrl Pts',(21.5914669370899,17.001172778885,39.202969059165));
#46929=CARTESIAN_POINT('Ctrl Pts',(21.4661724424056,16.9872604410897,39.3540981044645));
#46930=CARTESIAN_POINT('Ctrl Pts',(21.4467014677595,16.9851676096115,39.3765103494249));
#46931=CARTESIAN_POINT('Ctrl Pts',(21.3957926806449,16.9798835546014,39.4324476308416));
#46932=CARTESIAN_POINT('Ctrl Pts',(21.3636577081549,16.9767201228571,39.4653176688622));
#46933=CARTESIAN_POINT('Ctrl Pts',(21.3248885332307,16.9731280992817,39.5022376274033));
#46934=CARTESIAN_POINT('Ctrl Pts',(21.3193696432545,16.9726218326444,39.5074316105119));
#46935=CARTESIAN_POINT('Ctrl Pts',(21.3104623290637,16.9718130301125,39.5157160978284));
#46936=CARTESIAN_POINT('Ctrl Pts',(21.3070933115626,16.9715089982495,39.518827213402));
#46937=CARTESIAN_POINT('Ctrl Pts',(21.3010801010035,16.9709697336735,39.5243405102416));
#46938=CARTESIAN_POINT('Ctrl Pts',(21.2984402946963,16.9707341501535,39.5267473918853));
#46939=CARTESIAN_POINT('Ctrl Pts',(21.2927872830349,16.9702321323524,39.5318729228909));
#46940=CARTESIAN_POINT('Ctrl Pts',(21.2897721854437,16.9699658593025,39.5345893966195));
#46941=CARTESIAN_POINT('Ctrl Pts',(21.281499594735,16.9692392544401,39.5419954848587));
#46942=CARTESIAN_POINT('Ctrl Pts',(21.2762248848906,16.968780327066,39.5466659035823));
#46943=CARTESIAN_POINT('Ctrl Pts',(21.2482171053427,16.9663657139601,39.5711926000204));
#46944=CARTESIAN_POINT('Ctrl Pts',(21.2250444879024,16.964444714477,39.5905434770603));
#46945=CARTESIAN_POINT('Ctrl Pts',(21.0747367525486,16.9523928928381,39.7101872467629));
#46946=CARTESIAN_POINT('Ctrl Pts',(20.9358428206229,16.9430217029138,39.7946895349736));
#46947=CARTESIAN_POINT('Ctrl Pts',(20.7064178950063,16.9278169286061,39.8973610059144));
#46948=CARTESIAN_POINT('Ctrl Pts',(20.6223981801577,16.9223089650795,39.9281548646624));
#46949=CARTESIAN_POINT('Ctrl Pts',(20.5236107877748,16.9157405151792,39.9567595060637));
#46950=CARTESIAN_POINT('Ctrl Pts',(20.5106292669834,16.9148757410076,39.9603714299476));
#46951=CARTESIAN_POINT('Ctrl Pts',(20.489686815378,16.9134775584102,39.9659626609822));
#46952=CARTESIAN_POINT('Ctrl Pts',(20.4817490886396,16.9129469037005,39.9680277410985));
#46953=CARTESIAN_POINT('Ctrl Pts',(20.4675886719125,16.9119988853508,39.9716154595967));
#46954=CARTESIAN_POINT('Ctrl Pts',(20.461371074914,16.9115821607335,39.9731578482037));
#46955=CARTESIAN_POINT('Ctrl Pts',(20.4483530300245,16.9107086209183,39.9763184648224));
#46956=CARTESIAN_POINT('Ctrl Pts',(20.4415512495908,16.9102516227865,39.9779307529276));
#46957=CARTESIAN_POINT('Ctrl Pts',(20.4237505924778,16.9090540319972,39.9820481508835));
#46958=CARTESIAN_POINT('Ctrl Pts',(20.4127383702476,16.908311559457,39.9844937875892));
#46959=CARTESIAN_POINT('Ctrl Pts',(20.3634782489339,16.9049827500904,39.9949811819017));
#46960=CARTESIAN_POINT('Ctrl Pts',(20.3250150257307,16.9023629858092,40.0019555659445));
#46961=CARTESIAN_POINT('Ctrl Pts',(20.21992409561,16.8951438960991,40.0177305136863));
#46962=CARTESIAN_POINT('Ctrl Pts',(20.1530102890439,16.8904794074338,40.0242253433794));
#46963=CARTESIAN_POINT('Ctrl Pts',(19.9689033532457,16.8774972245874,40.0324313494698));
#46964=CARTESIAN_POINT('Ctrl Pts',(19.8516811132925,16.8690544046441,40.0269815365718));
#46965=CARTESIAN_POINT('Ctrl Pts',(19.7218971844104,16.8598193273474,40.0090298512959));
#46966=CARTESIAN_POINT('Ctrl Pts',(19.7081354343519,16.858841788071,40.0069743675738));
#46967=CARTESIAN_POINT('Ctrl Pts',(19.6468562091218,16.854499593023,39.9971426709642));
#46968=CARTESIAN_POINT('Ctrl Pts',(19.5996129992631,16.8511803084583,39.9877372672365));
#46969=CARTESIAN_POINT('Ctrl Pts',(19.5453030545746,16.8474335774071,39.9747938876659));
#46970=CARTESIAN_POINT('Ctrl Pts',(19.5378495243433,16.8469209070608,39.972970468549));
#46971=CARTESIAN_POINT('Ctrl Pts',(19.5259321670112,16.8461038785093,39.9699795537022));
#46972=CARTESIAN_POINT('Ctrl Pts',(19.5214613974063,16.8457979766243,39.9688404555933));
#46973=CARTESIAN_POINT('Ctrl Pts',(19.5135328720823,16.845256612305,39.9667900460725));
#46974=CARTESIAN_POINT('Ctrl Pts',(19.5100735145414,16.8450207889507,39.965885147141));
#46975=CARTESIAN_POINT('Ctrl Pts',(19.5027095711172,16.8445196230953,39.9639369945216));
#46976=CARTESIAN_POINT('Ctrl Pts',(19.4988057473897,16.8442544348125,39.9628910897039));
#46977=CARTESIAN_POINT('Ctrl Pts',(19.4881793775291,16.8435338534812,39.9600082723597));
#46978=CARTESIAN_POINT('Ctrl Pts',(19.4814633710813,16.8430798261188,39.9581471661116));
#46979=CARTESIAN_POINT('Ctrl Pts',(19.4466954266358,16.8407358893149,39.9483092637592));
#46980=CARTESIAN_POINT('Ctrl Pts',(19.4188151889925,16.8388783010891,39.9397330034957));
#46981=CARTESIAN_POINT('Ctrl Pts',(19.3356094989334,16.8333711660076,39.9120575064723));
#46982=CARTESIAN_POINT('Ctrl Pts',(19.280945267054,16.8298020628967,39.8910690970269));
#46983=CARTESIAN_POINT('Ctrl Pts',(19.0761997057163,16.816330260708,39.80156849493));
#46984=CARTESIAN_POINT('Ctrl Pts',(18.9341882198839,16.8067016513006,39.7164115031853));
#46985=CARTESIAN_POINT('Ctrl Pts',(18.7999675471508,16.796001752138,39.6104640384852));
#46986=CARTESIAN_POINT('Ctrl Pts',(18.7952145825897,16.7956206545821,39.6066756771933));
#46987=CARTESIAN_POINT('Ctrl Pts',(18.787140488361,16.7949694397525,39.6001775674453));
#46988=CARTESIAN_POINT('Ctrl Pts',(18.7838103236156,16.7946997258505,39.5974790814781));
#46989=CARTESIAN_POINT('Ctrl Pts',(18.7757232510012,16.7940419789368,39.5908812266464));
#46990=CARTESIAN_POINT('Ctrl Pts',(18.77097596805,16.7936535222693,39.5869701804986));
#46991=CARTESIAN_POINT('Ctrl Pts',(18.7486382180114,16.7918143952374,39.5683871893661));
#46992=CARTESIAN_POINT('Ctrl Pts',(18.7312918630492,16.7903529082178,39.5534258975904));
#46993=CARTESIAN_POINT('Ctrl Pts',(18.7071292097087,16.7882670030527,39.531823333334));
#46994=CARTESIAN_POINT('Ctrl Pts',(18.7000888825141,16.7876530336796,39.5254346774271));
#46995=CARTESIAN_POINT('Ctrl Pts',(18.6887199836951,16.7866512888932,39.5149638410944));
#46996=CARTESIAN_POINT('Ctrl Pts',(18.6843625108631,16.7862648442354,39.5109131612635));
#46997=CARTESIAN_POINT('Ctrl Pts',(18.6756218710228,16.7854845848731,39.5027122173662));
#46998=CARTESIAN_POINT('Ctrl Pts',(18.6712393084315,16.785090749409,39.4985614095984));
#46999=CARTESIAN_POINT('Ctrl Pts',(18.6607374380898,16.7841406426356,39.4885209686807));
#47000=CARTESIAN_POINT('Ctrl Pts',(18.6546374464177,16.7835835161957,39.4826114008394));
#47001=CARTESIAN_POINT('Ctrl Pts',(18.6352255108945,16.7817934739054,39.463555347721));
#47002=CARTESIAN_POINT('Ctrl Pts',(18.6220660503181,16.7805538975073,39.4502557465257));
#47003=CARTESIAN_POINT('Ctrl Pts',(18.5915747533609,16.7776185452663,39.4185297527463));
#47004=CARTESIAN_POINT('Ctrl Pts',(18.5744081437317,16.7759160735809,39.3999500538575));
#47005=CARTESIAN_POINT('Ctrl Pts',(18.5144420850611,16.7697857674479,39.3324311869077));
#47006=CARTESIAN_POINT('Ctrl Pts',(18.4737605416144,16.7652784345264,39.2816770242643));
#47007=CARTESIAN_POINT('Ctrl Pts',(18.3553176578211,16.7510396579551,39.1175650204416));
#47008=CARTESIAN_POINT('Ctrl Pts',(18.2870491594544,16.7410914972882,38.9978953179414));
#47009=CARTESIAN_POINT('Ctrl Pts',(18.213946410057,16.7283350701578,38.8304838333039));
#47010=CARTESIAN_POINT('Ctrl Pts',(18.1972867661624,16.725218063774,38.7883457049693));
#47011=CARTESIAN_POINT('Ctrl Pts',(18.1795995125193,16.7216725343194,38.7385464366185));
#47012=CARTESIAN_POINT('Ctrl Pts',(18.1771159181849,16.721168515013,38.7314215037241));
#47013=CARTESIAN_POINT('Ctrl Pts',(18.1731933416226,16.7203626014581,38.7199523600361));
#47014=CARTESIAN_POINT('Ctrl Pts',(18.1717279325836,16.7200592278309,38.7156173684854));
#47015=CARTESIAN_POINT('Ctrl Pts',(18.1691463606597,16.719520699493,38.7078900076647));
#47016=CARTESIAN_POINT('Ctrl Pts',(18.1680241782992,16.7192851975376,38.7044997101753));
#47017=CARTESIAN_POINT('Ctrl Pts',(18.165644958836,16.7187828667323,38.6972442204242));
#47018=CARTESIAN_POINT('Ctrl Pts',(18.1643907222123,16.7185162016301,38.6933781727775));
#47019=CARTESIAN_POINT('Ctrl Pts',(18.1609874359256,16.717787417369,38.6827738564739));
#47020=CARTESIAN_POINT('Ctrl Pts',(18.158863182502,16.7173267167846,38.6760276049391));
#47021=CARTESIAN_POINT('Ctrl Pts',(18.1477572945606,16.7148858924912,38.6400681310749));
#47022=CARTESIAN_POINT('Ctrl Pts',(18.1394331483969,16.7129413547455,38.6106543561473));
#47023=CARTESIAN_POINT('Ctrl Pts',(18.0914719636826,16.70088054343,38.424395222669));
#47024=CARTESIAN_POINT('Ctrl Pts',(18.0709952650174,16.6915185538119,38.2632773658475));
#47025=CARTESIAN_POINT('Ctrl Pts',(18.0708705729314,16.6817303897375,38.101486781031));
#47026=CARTESIAN_POINT('Ctrl Pts',(19.3941040087494,16.5227836600514,36.2684889831927));
#47027=CARTESIAN_POINT('Ctrl Pts',(19.3295148449261,16.5272260878162,36.2898562122619));
#47028=CARTESIAN_POINT('Ctrl Pts',(19.2660380494538,16.531668515581,36.3146505999152));
#47029=CARTESIAN_POINT('Ctrl Pts',(19.2040551538421,16.5361109433459,36.3427253035525));
#47030=CARTESIAN_POINT('Ctrl Pts',(19.1420684686983,16.5405536427134,36.3708017236309));
#47031=CARTESIAN_POINT('Ctrl Pts',(19.0815763128461,16.544996342081,36.4021586519863));
#47032=CARTESIAN_POINT('Ctrl Pts',(19.0229383238685,16.5494390414485,36.4366019604631));
#47033=CARTESIAN_POINT('Ctrl Pts',(18.964238019985,16.5538864620966,36.4710818720289));
#47034=CARTESIAN_POINT('Ctrl Pts',(18.9073962411138,16.5583338827446,36.5086544587853));
#47035=CARTESIAN_POINT('Ctrl Pts',(18.8527452760582,16.5627813033926,36.5490811899737));
#47036=CARTESIAN_POINT('Ctrl Pts',(18.7980613409524,16.5672314070982,36.5895323099604));
#47037=CARTESIAN_POINT('Ctrl Pts',(18.7455712304066,16.5716815108037,36.6328406872743));
#47038=CARTESIAN_POINT('Ctrl Pts',(18.6955734437814,16.5761316145093,36.6787280639048));
#47039=CARTESIAN_POINT('Ctrl Pts',(18.6454900528359,16.5805893375142,36.7246940071671));
#47040=CARTESIAN_POINT('Ctrl Pts',(18.5979078468069,16.5850470605191,36.7732474100531));
#47041=CARTESIAN_POINT('Ctrl Pts',(18.5530871921838,16.589504783524,36.8240744992447));
#47042=CARTESIAN_POINT('Ctrl Pts',(18.5334450984166,16.5914583251219,36.8463488381677));
#47043=CARTESIAN_POINT('Ctrl Pts',(18.5143328255968,16.5934118667198,36.8690594374671));
#47044=CARTESIAN_POINT('Ctrl Pts',(18.4957696697059,16.5953654083177,36.8921781297214));
#47045=CARTESIAN_POINT('Ctrl Pts',(18.4535300638365,16.5998106022076,36.944783648674));
#47046=CARTESIAN_POINT('Ctrl Pts',(18.4139654211078,16.6042557960976,36.9997171835828));
#47047=CARTESIAN_POINT('Ctrl Pts',(18.3773430117714,16.6087009899876,37.0566750959299));
#47048=CARTESIAN_POINT('Ctrl Pts',(18.3407736908796,16.6131397400516,37.1135504411539));
#47049=CARTESIAN_POINT('Ctrl Pts',(18.3071384107541,16.6175784901157,37.1724439311144));
#47050=CARTESIAN_POINT('Ctrl Pts',(18.2766639897095,16.6220172401797,37.2330192894095));
#47051=CARTESIAN_POINT('Ctrl Pts',(18.2462230981501,16.6264511065085,37.2935279996597));
#47052=CARTESIAN_POINT('Ctrl Pts',(18.2189363873649,16.6308849728373,37.3557144662688));
#47053=CARTESIAN_POINT('Ctrl Pts',(18.1949861550876,16.6353188391661,37.4192154697891));
#47054=CARTESIAN_POINT('Ctrl Pts',(18.1710517467709,16.6397497760316,37.4826745180844));
#47055=CARTESIAN_POINT('Ctrl Pts',(18.1504496195063,16.6441807128971,37.5474459179093));
#47056=CARTESIAN_POINT('Ctrl Pts',(18.1333143395094,16.6486116497626,37.6131456051151));
#47057=CARTESIAN_POINT('Ctrl Pts',(18.1161856421353,16.6530408844565,37.6788200533834));
#47058=CARTESIAN_POINT('Ctrl Pts',(18.1025212694212,16.6574701191505,37.7454216006164));
#47059=CARTESIAN_POINT('Ctrl Pts',(18.0924056487478,16.6618993538444,37.8125520082335));
#47060=CARTESIAN_POINT('Ctrl Pts',(18.0822874619202,16.6663297121569,37.8796994456486));
#47061=CARTESIAN_POINT('Ctrl Pts',(18.0757198989312,16.6707600704694,37.947375520813));
#47062=CARTESIAN_POINT('Ctrl Pts',(18.0727358351024,16.6751904287819,38.0151743222739));
#47063=CARTESIAN_POINT('Ctrl Pts',(18.0714692472317,16.6770708973052,38.0439515685084));
#47064=CARTESIAN_POINT('Ctrl Pts',(18.0708476156394,16.6789513658286,38.0727508773751));
#47065=CARTESIAN_POINT('Ctrl Pts',(18.0708706155933,16.6808318343519,38.1015411420322));
#47066=CARTESIAN_POINT('',(18.0708705531879,16.5088527686983,38.0985390611445));
#47067=CARTESIAN_POINT('Ctrl Pts',(19.3941040086649,16.3533584392964,36.2684889832207));
#47068=CARTESIAN_POINT('Ctrl Pts',(19.3892758720374,16.3536772472466,36.2700862155613));
#47069=CARTESIAN_POINT('Ctrl Pts',(19.3844539050878,16.3539952867857,36.2717025877808));
#47070=CARTESIAN_POINT('Ctrl Pts',(19.3036135955524,16.3593220282272,36.2991571688369));
#47071=CARTESIAN_POINT('Ctrl Pts',(19.2292683506885,16.3641458421739,36.3296995152239));
#47072=CARTESIAN_POINT('Ctrl Pts',(19.0150878285822,16.3783853895655,36.4337480053713));
#47073=CARTESIAN_POINT('Ctrl Pts',(18.8821542772439,16.3877359897341,36.5198538405314));
#47074=CARTESIAN_POINT('Ctrl Pts',(18.7460531018636,16.3990146866174,36.633865659235));
#47075=CARTESIAN_POINT('Ctrl Pts',(18.7311073465873,16.4002783176956,36.6467814628489));
#47076=CARTESIAN_POINT('Ctrl Pts',(18.7105131007799,16.4020563815016,36.665138506828));
#47077=CARTESIAN_POINT('Ctrl Pts',(18.7046951223494,16.4025629024981,36.6703884307929));
#47078=CARTESIAN_POINT('Ctrl Pts',(18.6941083082209,16.4034924436621,36.6800592511146));
#47079=CARTESIAN_POINT('Ctrl Pts',(18.6893295089091,16.4039149969786,36.684469109109));
#47080=CARTESIAN_POINT('Ctrl Pts',(18.6802040288119,16.4047276634437,36.6929758960852));
#47081=CARTESIAN_POINT('Ctrl Pts',(18.6758538943057,16.4051176122385,36.6970690237963));
#47082=CARTESIAN_POINT('Ctrl Pts',(18.6653935398326,16.4060615138464,36.7070033712748));
#47083=CARTESIAN_POINT('Ctrl Pts',(18.6593026105019,16.4066163240264,36.7128646363392));
#47084=CARTESIAN_POINT('Ctrl Pts',(18.6386789552232,16.4085128418678,36.7329733877274));
#47085=CARTESIAN_POINT('Ctrl Pts',(18.6243336658668,16.4098627627312,36.747410324934));
#47086=CARTESIAN_POINT('Ctrl Pts',(18.5907218837777,16.4131012150043,36.7823247242782));
#47087=CARTESIAN_POINT('Ctrl Pts',(18.5716698310308,16.414998403525,36.8030012599432));
#47088=CARTESIAN_POINT('Ctrl Pts',(18.5025802854964,16.4221139922531,36.8813507630506));
#47089=CARTESIAN_POINT('Ctrl Pts',(18.4555328128699,16.4274425041934,36.9415568101993));
#47090=CARTESIAN_POINT('Ctrl Pts',(18.3424271484451,16.4415385188585,37.1054753230042));
#47091=CARTESIAN_POINT('Ctrl Pts',(18.2824882795144,16.4504065451616,37.2129933448711));
#47092=CARTESIAN_POINT('Ctrl Pts',(18.2157287901588,16.4620030874774,37.3652839764697));
#47093=CARTESIAN_POINT('Ctrl Pts',(18.1996283741878,16.4649905415365,37.4056700557658));
#47094=CARTESIAN_POINT('Ctrl Pts',(18.1823798919577,16.4684063222219,37.4535827448098));
#47095=CARTESIAN_POINT('Ctrl Pts',(18.1798955768499,16.4689042044245,37.4606112151402));
#47096=CARTESIAN_POINT('Ctrl Pts',(18.1759448517806,16.4697054742374,37.4719979979293));
#47097=CARTESIAN_POINT('Ctrl Pts',(18.1744532031112,16.4700102778456,37.4763473788992));
#47098=CARTESIAN_POINT('Ctrl Pts',(18.1718325418937,16.4705498109589,37.4840787277562));
#47099=CARTESIAN_POINT('Ctrl Pts',(18.1706973415091,16.4707848978146,37.4874585296661));
#47100=CARTESIAN_POINT('Ctrl Pts',(18.1682772127539,16.4712890498219,37.494730648508));
#47101=CARTESIAN_POINT('Ctrl Pts',(18.1669953197539,16.4715579371223,37.4986239112319));
#47102=CARTESIAN_POINT('Ctrl Pts',(18.1634868383316,16.4722991035999,37.5093950342462));
#47103=CARTESIAN_POINT('Ctrl Pts',(18.1612864589617,16.4727698827081,37.5162814577283));
#47104=CARTESIAN_POINT('Ctrl Pts',(18.1493104754225,16.4753665741367,37.5545018722405));
#47105=CARTESIAN_POINT('Ctrl Pts',(18.1402964179168,16.4774512964463,37.5860711902189));
#47106=CARTESIAN_POINT('Ctrl Pts',(18.0915649400639,16.489648591173,37.7748657998577));
#47107=CARTESIAN_POINT('Ctrl Pts',(18.0709933689859,16.4990290997554,37.9363641887504));
#47108=CARTESIAN_POINT('Ctrl Pts',(18.0708705531879,16.5088527686983,38.0985390611445));
#47109=CARTESIAN_POINT('Ctrl Pts',(18.0708705515757,16.508852897749,38.0985411915881));
#47110=CARTESIAN_POINT('Ctrl Pts',(18.0708048840684,16.5141131180069,38.1853799573665));
#47111=CARTESIAN_POINT('Ctrl Pts',(18.0766025970578,16.51947261588,38.2721161168967));
#47112=CARTESIAN_POINT('Ctrl Pts',(18.0896070740216,16.5256819604477,38.368418578429));
#47113=CARTESIAN_POINT('Ctrl Pts',(18.0910745387327,16.526345734488,38.3786633121205));
#47114=CARTESIAN_POINT('Ctrl Pts',(18.0936889979285,16.5274698009348,38.3959247591256));
#47115=CARTESIAN_POINT('Ctrl Pts',(18.0947924896503,16.527928736344,38.4029479162796));
#47116=CARTESIAN_POINT('Ctrl Pts',(18.0968949595824,16.5287756866617,38.4158630624971));
#47117=CARTESIAN_POINT('Ctrl Pts',(18.0978825470846,16.5291633405541,38.4217568384629));
#47118=CARTESIAN_POINT('Ctrl Pts',(18.0999771375618,16.5299651381418,38.4339102989339));
#47119=CARTESIAN_POINT('Ctrl Pts',(18.1010877264973,16.5303793902422,38.4401692835154));
#47120=CARTESIAN_POINT('Ctrl Pts',(18.1036471904395,16.5313104256268,38.4541905276434));
#47121=CARTESIAN_POINT('Ctrl Pts',(18.1051128237493,16.531827731907,38.4619495743343));
#47122=CARTESIAN_POINT('Ctrl Pts',(18.108959006785,16.5331464364166,38.4816473737806));
#47123=CARTESIAN_POINT('Ctrl Pts',(18.1114049782844,16.5339498899954,38.4935728501705));
#47124=CARTESIAN_POINT('Ctrl Pts',(18.1265076518352,16.5387135329302,38.5638219446732));
#47125=CARTESIAN_POINT('Ctrl Pts',(18.141751243414,16.5427551525522,38.6215502180609));
#47126=CARTESIAN_POINT('Ctrl Pts',(18.1722239688591,16.5497658266291,38.7184960156624));
#47127=CARTESIAN_POINT('Ctrl Pts',(18.18610533051,16.5526947584643,38.7580944548697));
#47128=CARTESIAN_POINT('Ctrl Pts',(18.2539947573515,16.5659249763226,38.9332433614372));
#47129=CARTESIAN_POINT('Ctrl Pts',(18.3219828480587,16.5765116980917,39.0628530756643));
#47130=CARTESIAN_POINT('Ctrl Pts',(18.4239828347039,16.589094361589,39.2130980059608));
#47131=CARTESIAN_POINT('Ctrl Pts',(18.4448545091076,16.5915347533597,39.2420771329861));
#47132=CARTESIAN_POINT('Ctrl Pts',(18.4710167783678,16.5944221893445,39.2763535997964));
#47133=CARTESIAN_POINT('Ctrl Pts',(18.4755474239509,16.5949163212764,39.2822190285856));
#47134=CARTESIAN_POINT('Ctrl Pts',(18.4826606387968,16.5956828051361,39.2913189951439));
#47135=CARTESIAN_POINT('Ctrl Pts',(18.4852199445685,16.5959567330136,39.294571500461));
#47136=CARTESIAN_POINT('Ctrl Pts',(18.4900001824561,16.59646490507,39.3006064224812));
#47137=CARTESIAN_POINT('Ctrl Pts',(18.4922183285059,16.596699331235,39.3033909016249));
#47138=CARTESIAN_POINT('Ctrl Pts',(18.4972823988856,16.5972314246571,39.3097119383247));
#47139=CARTESIAN_POINT('Ctrl Pts',(18.5001331011952,16.5975287470949,39.3132445958398));
#47140=CARTESIAN_POINT('Ctrl Pts',(18.5088848943855,16.5984349386969,39.3240120350952));
#47141=CARTESIAN_POINT('Ctrl Pts',(18.5148261652614,16.599041021927,39.3312142012477));
#47142=CARTESIAN_POINT('Ctrl Pts',(18.5730932063897,16.6049005083537,39.4008115314335));
#47143=CARTESIAN_POINT('Ctrl Pts',(18.6292751009563,16.609896526903,39.4598861798208));
#47144=CARTESIAN_POINT('Ctrl Pts',(18.7188166577528,16.6172623210434,39.5428306656738));
#47145=CARTESIAN_POINT('Ctrl Pts',(18.7494671964654,16.6196903702658,39.5694757293745));
#47146=CARTESIAN_POINT('Ctrl Pts',(18.8639114875287,16.6285115260933,39.662788351631));
#47147=CARTESIAN_POINT('Ctrl Pts',(18.9523683812009,16.6348854436372,39.7234131928609));
#47148=CARTESIAN_POINT('Ctrl Pts',(19.0756163316627,16.6436501439676,39.7935958702582));
#47149=CARTESIAN_POINT('Ctrl Pts',(19.1062972069616,16.6458219306448,39.8099845728939));
#47150=CARTESIAN_POINT('Ctrl Pts',(19.1520433312004,16.6490564619415,39.8328531238861));
#47151=CARTESIAN_POINT('Ctrl Pts',(19.1667758854631,16.6500975693242,39.8399850604511));
#47152=CARTESIAN_POINT('Ctrl Pts',(19.1935668655181,16.6519908898884,39.8525361274739));
#47153=CARTESIAN_POINT('Ctrl Pts',(19.205593736679,16.6528408561154,39.8580204644013));
#47154=CARTESIAN_POINT('Ctrl Pts',(19.2244219360543,16.6541719556873,39.8663735991807));
#47155=CARTESIAN_POINT('Ctrl Pts',(19.2311851318865,16.6546501866125,39.8693277596945));
#47156=CARTESIAN_POINT('Ctrl Pts',(19.2380142396075,16.6551332130436,39.8722641622308));
#47157=CARTESIAN_POINT('Ctrl Pts',(19.2380634440926,16.6551366933101,39.8722853169116));
#47158=CARTESIAN_POINT('Ctrl Pts',(19.2381632319464,16.6551437513867,39.8723282141785));
#47159=CARTESIAN_POINT('Ctrl Pts',(19.2382138152254,16.6551473291908,39.8723499565881));
#47160=CARTESIAN_POINT('Ctrl Pts',(19.2383164044322,16.6551545854396,39.8723940477069));
#47161=CARTESIAN_POINT('Ctrl Pts',(19.2383684103648,16.6551582638849,39.872416396272));
#47162=CARTESIAN_POINT('Ctrl Pts',(19.2384738903531,16.6551657246338,39.8724617188005));
#47163=CARTESIAN_POINT('Ctrl Pts',(19.2385273644588,16.6551695069413,39.8724846926304));
#47164=CARTESIAN_POINT('Ctrl Pts',(19.2386358275189,16.6551771787209,39.8725312852934));
#47165=CARTESIAN_POINT('Ctrl Pts',(19.2386908167319,16.6551810682118,39.872554904073));
#47166=CARTESIAN_POINT('Ctrl Pts',(19.2388023593083,16.6551889578468,39.8726028073129));
#47167=CARTESIAN_POINT('Ctrl Pts',(19.2388589126022,16.6551929579866,39.8726270915686));
#47168=CARTESIAN_POINT('Ctrl Pts',(19.2389736369529,16.655201072713,39.8726763482528));
#47169=CARTESIAN_POINT('Ctrl Pts',(19.2390318080577,16.6552051873039,39.8727013205154));
#47170=CARTESIAN_POINT('Ctrl Pts',(19.2391498044112,16.6552135335072,39.8727519682716));
#47171=CARTESIAN_POINT('Ctrl Pts',(19.2392096391798,16.6552177657938,39.872777647654));
#47172=CARTESIAN_POINT('Ctrl Pts',(19.2393310307579,16.6552263521934,39.8728297381919));
#47173=CARTESIAN_POINT('Ctrl Pts',(19.239392586876,16.6552307062581,39.8728561488419));
#47174=CARTESIAN_POINT('Ctrl Pts',(19.2395174778464,16.6552395402259,39.8729097256056));
#47175=CARTESIAN_POINT('Ctrl Pts',(19.2395808117616,16.6552440200634,39.8729368910955));
#47176=CARTESIAN_POINT('Ctrl Pts',(19.2397093165288,16.6552531096956,39.8729920018303));
#47177=CARTESIAN_POINT('Ctrl Pts',(19.2397744865614,16.6552577194331,39.873019946488));
#47178=CARTESIAN_POINT('Ctrl Pts',(19.2399067242232,16.6552670731584,39.8730766408542));
#47179=CARTESIAN_POINT('Ctrl Pts',(19.2399737909936,16.6552718170861,39.8731053899437));
#47180=CARTESIAN_POINT('Ctrl Pts',(19.240109883194,16.6552814435134,39.8731637185887));
#47181=CARTESIAN_POINT('Ctrl Pts',(19.2401789081103,16.6552863259773,39.8731932976581));
#47182=CARTESIAN_POINT('Ctrl Pts',(19.2403005649729,16.6552949313769,39.8732454225508));
#47183=CARTESIAN_POINT('Ctrl Pts',(19.2403531921221,16.6552986539672,39.8732679683169));
#47184=CARTESIAN_POINT('Ctrl Pts',(19.240465576667,16.6553066035246,39.8733161085656));
#47185=CARTESIAN_POINT('Ctrl Pts',(19.2405253344068,16.6553108305185,39.8733417023936));
#47186=CARTESIAN_POINT('Ctrl Pts',(19.2406529615775,16.6553198583138,39.8733963565965));
#47187=CARTESIAN_POINT('Ctrl Pts',(19.240720831173,16.6553246591301,39.8734254160053));
#47188=CARTESIAN_POINT('Ctrl Pts',(19.2408657821892,16.6553349123986,39.8734874691633));
#47189=CARTESIAN_POINT('Ctrl Pts',(19.2409428725203,16.6553403654852,39.8735204653889));
#47190=CARTESIAN_POINT('Ctrl Pts',(19.2411075500892,16.6553520142095,39.8735909380246));
#47191=CARTESIAN_POINT('Ctrl Pts',(19.2411951362286,16.6553582097745,39.8736284122364));
#47192=CARTESIAN_POINT('Ctrl Pts',(19.24138225509,16.6553714460176,39.8737084556729));
#47193=CARTESIAN_POINT('Ctrl Pts',(19.2414817871999,16.6553784866591,39.8737510224011));
#47194=CARTESIAN_POINT('Ctrl Pts',(19.241694451821,16.6553935300632,39.8738419511439));
#47195=CARTESIAN_POINT('Ctrl Pts',(19.241807584085,16.6554015328172,39.873890310162));
#47196=CARTESIAN_POINT('Ctrl Pts',(19.2420493345522,16.6554186338536,39.8739936203969));
#47197=CARTESIAN_POINT('Ctrl Pts',(19.2421779532428,16.6554277321819,39.8740485680812));
#47198=CARTESIAN_POINT('Ctrl Pts',(19.2482003280666,16.6558537499625,39.8766206354833));
#47199=CARTESIAN_POINT('Ctrl Pts',(19.2541065239219,16.6562716561318,39.8791083580916));
#47200=CARTESIAN_POINT('Ctrl Pts',(19.2676169838662,16.657227917164,39.8847199380488));
#47201=CARTESIAN_POINT('Ctrl Pts',(19.2752289989173,16.6577669049676,39.8878246927638));
#47202=CARTESIAN_POINT('Ctrl Pts',(19.2954290224283,16.6591979030618,39.8959135813905));
#47203=CARTESIAN_POINT('Ctrl Pts',(19.3080498709512,16.660092684301,39.9008139430155));
#47204=CARTESIAN_POINT('Ctrl Pts',(19.4073701333949,16.6671409334648,39.9381792961426));
#47205=CARTESIAN_POINT('Ctrl Pts',(19.4962399461726,16.6734965042636,39.9644930833565));
#47206=CARTESIAN_POINT('Ctrl Pts',(19.7428410696045,16.6912302729811,40.0185889517726));
#47207=CARTESIAN_POINT('Ctrl Pts',(19.902682996777,16.7028729836506,40.0332980420404));
#47208=CARTESIAN_POINT('Ctrl Pts',(20.0915535513515,16.7158892770902,40.0271754745477));
#47209=CARTESIAN_POINT('Ctrl Pts',(20.1205808260772,16.7178669469609,40.0255772776378));
#47210=CARTESIAN_POINT('Ctrl Pts',(20.1565032150207,16.7202773680959,40.0227838573251));
#47211=CARTESIAN_POINT('Ctrl Pts',(20.1634408436874,16.720741170757,40.0222065738543));
#47212=CARTESIAN_POINT('Ctrl Pts',(20.1743993201883,16.7214709050329,40.0212349553996));
#47213=CARTESIAN_POINT('Ctrl Pts',(20.1784222308775,16.7217381811788,40.0208655301726));
#47214=CARTESIAN_POINT('Ctrl Pts',(20.1860040828835,16.7222407148417,40.0201452618601));
#47215=CARTESIAN_POINT('Ctrl Pts',(20.1895631666149,16.7224761140691,40.0197971641791));
#47216=CARTESIAN_POINT('Ctrl Pts',(20.1977144711185,16.7230141229276,40.0189770335114));
#47217=CARTESIAN_POINT('Ctrl Pts',(20.2023059783428,16.7233163625422,40.0184984126789));
#47218=CARTESIAN_POINT('Ctrl Pts',(20.2145340923705,16.7241192276073,40.0171793611415));
#47219=CARTESIAN_POINT('Ctrl Pts',(20.2221675666111,16.7246182784717,40.0163097757611));
#47220=CARTESIAN_POINT('Ctrl Pts',(20.2778328036758,16.728243173976,40.0096314456327));
#47221=CARTESIAN_POINT('Ctrl Pts',(20.3256407191787,16.731278701166,40.0020626551314));
#47222=CARTESIAN_POINT('Ctrl Pts',(20.3869701489886,16.7351301078639,39.9899724884853));
#47223=CARTESIAN_POINT('Ctrl Pts',(20.400792424318,16.7359952863547,39.9870896509842));
#47224=CARTESIAN_POINT('Ctrl Pts',(20.4519075089283,16.7391881925269,39.9758418935097));
#47225=CARTESIAN_POINT('Ctrl Pts',(20.4889818762031,16.7414911980869,39.9665208590865));
#47226=CARTESIAN_POINT('Ctrl Pts',(20.6006214650739,16.7484490032239,39.9348980801802));
#47227=CARTESIAN_POINT('Ctrl Pts',(20.674134766144,16.7530648098837,39.9091819639176));
#47228=CARTESIAN_POINT('Ctrl Pts',(20.8082117080879,16.7618228256356,39.8529696283095));
#47229=CARTESIAN_POINT('Ctrl Pts',(20.8691089693926,16.7659408105452,39.8235884450813));
#47230=CARTESIAN_POINT('Ctrl Pts',(20.962730954298,16.7726075730337,39.7721935251985));
#47231=CARTESIAN_POINT('Ctrl Pts',(20.9965397206275,16.7750882517998,39.7522682358746));
#47232=CARTESIAN_POINT('Ctrl Pts',(21.0392677385793,16.7783309555674,39.7252977320796));
#47233=CARTESIAN_POINT('Ctrl Pts',(21.048766416575,16.7790588621646,39.7191847161454));
#47234=CARTESIAN_POINT('Ctrl Pts',(21.0640582328197,16.780242432276,39.7091524306178));
#47235=CARTESIAN_POINT('Ctrl Pts',(21.069884795773,16.7806961926983,39.7052843951885));
#47236=CARTESIAN_POINT('Ctrl Pts',(21.0810070467701,16.7815678019452,39.6978133016485));
#47237=CARTESIAN_POINT('Ctrl Pts',(21.0863060848072,16.7819854545864,39.6942153777166));
#47238=CARTESIAN_POINT('Ctrl Pts',(21.0983440428411,16.7829397600718,39.6859539970318));
#47239=CARTESIAN_POINT('Ctrl Pts',(21.1050713249971,16.7834770368238,39.6812738789735));
#47240=CARTESIAN_POINT('Ctrl Pts',(21.1227614361319,16.7849005219975,39.6687989847128));
#47241=CARTESIAN_POINT('Ctrl Pts',(21.1336727518421,16.7857894550613,39.6609322769185));
#47242=CARTESIAN_POINT('Ctrl Pts',(21.2165287255565,16.7926250389024,39.5998687658727));
#47243=CARTESIAN_POINT('Ctrl Pts',(21.2847656267366,16.7987599608654,39.5418465712944));
#47244=CARTESIAN_POINT('Ctrl Pts',(21.4645927727506,16.816401581958,39.3660068648197));
#47245=CARTESIAN_POINT('Ctrl Pts',(21.5657164710697,16.828205867248,39.2385666477072));
#47246=CARTESIAN_POINT('Ctrl Pts',(21.6652937100119,16.8414500383529,39.0742907730592));
#47247=CARTESIAN_POINT('Ctrl Pts',(21.6802697807159,16.8434962242681,39.0482295937541));
#47248=CARTESIAN_POINT('Ctrl Pts',(21.6979935662528,16.8459779650842,39.0156472584597));
#47249=CARTESIAN_POINT('Ctrl Pts',(21.7013216099445,16.8464467500478,39.0094486441043));
#47250=CARTESIAN_POINT('Ctrl Pts',(21.7065148357539,16.8471825295303,38.9996477779586));
#47251=CARTESIAN_POINT('Ctrl Pts',(21.7084026537535,16.8474509055507,38.9960576892344));
#47252=CARTESIAN_POINT('Ctrl Pts',(21.7119320062898,16.8479543272985,38.9892941737394));
#47253=CARTESIAN_POINT('Ctrl Pts',(21.7135760290826,16.8481895215035,38.9861221780354));
#47254=CARTESIAN_POINT('Ctrl Pts',(21.7173116908061,16.848725562675,38.9788652763391));
#47255=CARTESIAN_POINT('Ctrl Pts',(21.719397570841,16.8490260493152,38.9747774641543));
#47256=CARTESIAN_POINT('Ctrl Pts',(21.7248945865409,16.8498211862155,38.9639090422948));
#47257=CARTESIAN_POINT('Ctrl Pts',(21.728280367606,16.8503143095044,38.9571155952236));
#47258=CARTESIAN_POINT('Ctrl Pts',(21.7519959245775,16.8537938231324,38.9088192654342));
#47259=CARTESIAN_POINT('Ctrl Pts',(21.7708705153623,16.8566978739915,38.8666138102017));
#47260=CARTESIAN_POINT('Ctrl Pts',(21.8391703937921,16.8679347553882,38.697865264324));
#47261=CARTESIAN_POINT('Ctrl Pts',(21.8766928425007,16.8758695684353,38.5669261176721));
#47262=CARTESIAN_POINT('Ctrl Pts',(21.9114395305059,16.8880053667299,38.3687293978406));
#47263=CARTESIAN_POINT('Ctrl Pts',(21.9194472444387,16.891995210404,38.3038081702987));
#47264=CARTESIAN_POINT('Ctrl Pts',(21.926900042496,16.8984745513019,38.2003501407733));
#47265=CARTESIAN_POINT('Ctrl Pts',(21.9285142459604,16.9009008495183,38.1620194394894));
#47266=CARTESIAN_POINT('Ctrl Pts',(21.9291223062796,16.9040819392762,38.1124615190334));
#47267=CARTESIAN_POINT('Ctrl Pts',(21.9291621446617,16.9048042228001,38.1012542044362));
#47268=CARTESIAN_POINT('Ctrl Pts',(21.9290683459695,16.9059808887089,38.0830733388994));
#47269=CARTESIAN_POINT('Ctrl Pts',(21.9289945478482,16.9064334093115,38.076099633173));
#47270=CARTESIAN_POINT('Ctrl Pts',(21.9287803398671,16.9073041668063,38.0627165418849));
#47271=CARTESIAN_POINT('Ctrl Pts',(21.9286457913376,16.907722215872,38.0563071447044));
#47272=CARTESIAN_POINT('Ctrl Pts',(21.9282654232338,16.908679566519,38.0416661958792));
#47273=CARTESIAN_POINT('Ctrl Pts',(21.9279988380418,16.9092195060696,38.0334353539084));
#47274=CARTESIAN_POINT('Ctrl Pts',(21.9271527729192,16.9106546886913,38.0116293930573));
#47275=CARTESIAN_POINT('Ctrl Pts',(21.9264825667578,16.9115527286651,37.998058456264));
#47276=CARTESIAN_POINT('Ctrl Pts',(21.9199643883761,16.9187840503034,37.8893881361967));
#47277=CARTESIAN_POINT('Ctrl Pts',(21.9072226524958,16.9253319313523,37.7948486711656));
#47278=CARTESIAN_POINT('Ctrl Pts',(21.8673310773225,16.9389177790299,37.60582563805));
#47279=CARTESIAN_POINT('Ctrl Pts',(21.8398413969882,16.9459449686918,37.5116840336201));
#47280=CARTESIAN_POINT('Ctrl Pts',(21.7845941813676,16.95708606465,37.3649995230995));
#47281=CARTESIAN_POINT('Ctrl Pts',(21.7613546738252,16.9612346648168,37.3109291466405));
#47282=CARTESIAN_POINT('Ctrl Pts',(21.722908729966,16.9673030829408,37.2316774103787));
#47283=CARTESIAN_POINT('Ctrl Pts',(21.7095403446508,16.9692941492747,37.2056451202246));
#47284=CARTESIAN_POINT('Ctrl Pts',(21.6922568738773,16.9717185355463,37.1737938157794));
#47285=CARTESIAN_POINT('Ctrl Pts',(21.6888964114489,16.9721833274401,37.1676802383608));
#47286=CARTESIAN_POINT('Ctrl Pts',(21.6835360864481,16.9729142622165,37.1580524703537));
#47287=CARTESIAN_POINT('Ctrl Pts',(21.6815582541132,16.9731817569379,37.1545261813513));
#47288=CARTESIAN_POINT('Ctrl Pts',(21.6778104741126,16.9736844655346,37.1478932026651));
#47289=CARTESIAN_POINT('Ctrl Pts',(21.6760429967702,16.9739198224689,37.1447852525284));
#47290=CARTESIAN_POINT('Ctrl Pts',(21.6719763595535,16.9744574334195,37.1376804741705));
#47291=CARTESIAN_POINT('Ctrl Pts',(21.6696715048969,16.974759319374,37.1336869640118));
#47292=CARTESIAN_POINT('Ctrl Pts',(21.6634975756277,16.9755606233294,37.1230777365469));
#47293=CARTESIAN_POINT('Ctrl Pts',(21.6596033100083,16.9760584764191,37.1164766646993));
#47294=CARTESIAN_POINT('Ctrl Pts',(21.631070971093,16.9796530335569,37.068764236932));
#47295=CARTESIAN_POINT('Ctrl Pts',(21.604945388601,16.9826611177903,37.0285566342898));
#47296=CARTESIAN_POINT('Ctrl Pts',(21.5694738780134,16.9864586609536,36.9781794713609));
#47297=CARTESIAN_POINT('Ctrl Pts',(21.5614823107467,16.9872970414794,36.9670822805398));
#47298=CARTESIAN_POINT('Ctrl Pts',(21.4832965562056,16.9953455826715,36.8609116690367));
#47299=CARTESIAN_POINT('Ctrl Pts',(21.4046218278169,17.0022856152925,36.7723899072505));
#47300=CARTESIAN_POINT('Ctrl Pts',(21.2522960428598,17.0148599307573,36.6298026482158));
#47301=CARTESIAN_POINT('Ctrl Pts',(21.1819961387515,17.0203998380739,36.5727122814233));
#47302=CARTESIAN_POINT('Ctrl Pts',(21.0910933403258,17.02744775451,36.5089367640741));
#47303=CARTESIAN_POINT('Ctrl Pts',(21.0740421841855,17.0287647619614,36.4973770772044));
#47304=CARTESIAN_POINT('Ctrl Pts',(21.0494021113822,17.0306624653907,36.4812424004517));
#47305=CARTESIAN_POINT('Ctrl Pts',(21.0419613227749,17.0312348306714,36.4764429313934));
#47306=CARTESIAN_POINT('Ctrl Pts',(21.0290124117632,17.032229815672,36.4682162843196));
#47307=CARTESIAN_POINT('Ctrl Pts',(21.0235195109459,17.0326515529918,36.46476532347));
#47308=CARTESIAN_POINT('Ctrl Pts',(21.0129275177004,17.033464204081,36.4581850917118));
#47309=CARTESIAN_POINT('Ctrl Pts',(21.0078310612019,17.0338549611085,36.4550517029655));
#47310=CARTESIAN_POINT('Ctrl Pts',(20.9957771612093,17.0347785962841,36.447717804969));
#47311=CARTESIAN_POINT('Ctrl Pts',(20.9888076290942,17.0353121990037,36.4435374812456));
#47312=CARTESIAN_POINT('Ctrl Pts',(20.9643595421604,17.0371826099326,36.4290827995079));
#47313=CARTESIAN_POINT('Ctrl Pts',(20.9467461110923,17.0385276869294,36.4190403438669));
#47314=CARTESIAN_POINT('Ctrl Pts',(20.7800809126728,17.0512370168745,36.3274650817796));
#47315=CARTESIAN_POINT('Ctrl Pts',(20.621055989094,17.0633270664663,36.2656959297271));
#47316=CARTESIAN_POINT('Ctrl Pts',(20.3880287364013,17.0804222288587,36.2090011340592));
#47317=CARTESIAN_POINT('Ctrl Pts',(20.3191543659163,17.0853884480983,36.1961657438722));
#47318=CARTESIAN_POINT('Ctrl Pts',(20.2173956455247,17.0924801451444,36.1828810552826));
#47319=CARTESIAN_POINT('Ctrl Pts',(20.1849565924284,17.0947044193416,36.1794799442602));
#47320=CARTESIAN_POINT('Ctrl Pts',(20.1452522744402,17.0973703724086,36.1763325679926));
#47321=CARTESIAN_POINT('Ctrl Pts',(20.1380566183715,17.0978512644894,36.1758027683279));
#47322=CARTESIAN_POINT('Ctrl Pts',(20.126771776997,17.0986017211274,36.1750355203207));
#47323=CARTESIAN_POINT('Ctrl Pts',(20.1226846117667,17.0988727587352,36.1747707102059));
#47324=CARTESIAN_POINT('Ctrl Pts',(20.1150374748267,17.0993784055375,36.1742996983896));
#47325=CARTESIAN_POINT('Ctrl Pts',(20.1114778130096,17.0996131794006,36.1740903526583));
#47326=CARTESIAN_POINT('Ctrl Pts',(20.1033218899369,17.100149743641,36.1736333864251));
#47327=CARTESIAN_POINT('Ctrl Pts',(20.0987253138087,17.1004511660056,36.1733923449928));
#47328=CARTESIAN_POINT('Ctrl Pts',(20.0866662398352,17.1012394816692,36.172803246054));
#47329=CARTESIAN_POINT('Ctrl Pts',(20.0792024183489,17.1017249273355,36.1724820761246));
#47330=CARTESIAN_POINT('Ctrl Pts',(20.0279739035153,17.1050410096144,36.170575770234));
#47331=CARTESIAN_POINT('Ctrl Pts',(19.9841642853814,17.1077977712606,36.1704377925896));
#47332=CARTESIAN_POINT('Ctrl Pts',(19.9369685161855,17.1107185364186,36.1718969770219));
#47333=CARTESIAN_POINT('Ctrl Pts',(19.9335530689153,17.1109296275034,36.1720116595888));
#47334=CARTESIAN_POINT('Ctrl Pts',(19.8085918932259,17.1186432322514,36.1765400102261));
#47335=CARTESIAN_POINT('Ctrl Pts',(19.6877269909218,17.1257872421719,36.1924295107725));
#47336=CARTESIAN_POINT('Ctrl Pts',(19.5100385753546,17.1367334237182,36.2331420115103));
#47337=CARTESIAN_POINT('Ctrl Pts',(19.4516240808264,17.1404040562064,36.2494603274301));
#47338=CARTESIAN_POINT('Ctrl Pts',(19.3941038273433,17.1441450759092,36.2684890432051));
#47339=CARTESIAN_POINT('Origin',(20.,-1.3495818343519,38.1));
#47340=CARTESIAN_POINT('',(19.3941040099181,18.1086029180356,36.2684889828061));
#47341=CARTESIAN_POINT('',(19.3941039849792,17.9383397493623,36.2684889910563));
#47342=CARTESIAN_POINT('',(19.3941040087494,-1.3495818343519,36.2684889831927));
#47343=CARTESIAN_POINT('Ctrl Pts',(19.3941040099181,18.1086029180356,36.2684889828061));
#47344=CARTESIAN_POINT('Ctrl Pts',(19.4118925383936,18.1073231984833,36.2626042253727));
#47345=CARTESIAN_POINT('Ctrl Pts',(19.4297674431853,18.1060547358816,36.2569784117878));
#47346=CARTESIAN_POINT('Ctrl Pts',(19.4548261523261,18.1043034292345,36.2494911535087));
#47347=CARTESIAN_POINT('Ctrl Pts',(19.4619415653936,18.1038091547017,36.2474097483609));
#47348=CARTESIAN_POINT('Ctrl Pts',(19.4730482051212,18.1030424978933,36.2442302149794));
#47349=CARTESIAN_POINT('Ctrl Pts',(19.4770311717749,18.1027685385463,36.2431038546473));
#47350=CARTESIAN_POINT('Ctrl Pts',(19.4844465176776,18.1022603376764,36.2410325884398));
#47351=CARTESIAN_POINT('Ctrl Pts',(19.4878778550252,18.1020259139842,36.2400843730626));
#47352=CARTESIAN_POINT('Ctrl Pts',(19.4956899539437,18.1014938639647,36.2379488368605));
#47353=CARTESIAN_POINT('Ctrl Pts',(19.5000722862947,18.1011965822233,36.2367674759141));
#47354=CARTESIAN_POINT('Ctrl Pts',(19.5134785406461,18.1002906405667,36.2332042078609));
#47355=CARTESIAN_POINT('Ctrl Pts',(19.5225157773626,18.099684764339,36.2308722661144));
#47356=CARTESIAN_POINT('Ctrl Pts',(19.6102157059773,18.0938486371635,36.2089200241802));
#47357=CARTESIAN_POINT('Ctrl Pts',(19.6900353381661,18.0888734817033,36.1942086492662));
#47358=CARTESIAN_POINT('Ctrl Pts',(19.9332760717362,18.074087065427,36.1650713069205));
#47359=CARTESIAN_POINT('Ctrl Pts',(20.0978087127406,18.0645279247874,36.166393570264));
#47360=CARTESIAN_POINT('Ctrl Pts',(20.2991118818064,18.0518466700567,36.1937950672755));
#47361=CARTESIAN_POINT('Ctrl Pts',(20.3378558179994,18.049363557701,36.200279423009));
#47362=CARTESIAN_POINT('Ctrl Pts',(20.3874553776625,18.0461180973221,36.21014588673));
#47363=CARTESIAN_POINT('Ctrl Pts',(20.3985181124923,18.0453899407151,36.2124477373304));
#47364=CARTESIAN_POINT('Ctrl Pts',(20.4163948641007,18.0442060627775,36.2163315585643));
#47365=CARTESIAN_POINT('Ctrl Pts',(20.4232217271286,18.0437522463795,36.2178536593391));
#47366=CARTESIAN_POINT('Ctrl Pts',(20.4362837856676,18.0428805965614,36.2208406034761));
#47367=CARTESIAN_POINT('Ctrl Pts',(20.4425202703756,18.0424629596926,36.2222994413824));
#47368=CARTESIAN_POINT('Ctrl Pts',(20.4567179752734,18.0415087832948,36.2256952275226));
#47369=CARTESIAN_POINT('Ctrl Pts',(20.464674309474,18.0409716204638,36.2276518828765));
#47370=CARTESIAN_POINT('Ctrl Pts',(20.4856536365578,18.0395486376356,36.232953164777));
#47371=CARTESIAN_POINT('Ctrl Pts',(20.4986543557239,18.038660096089,36.2363833125745));
#47372=CARTESIAN_POINT('Ctrl Pts',(20.5978633149255,18.03182676355,36.2636713159341));
#47373=CARTESIAN_POINT('Ctrl Pts',(20.6823414646879,18.0256938153348,36.2933596084965));
#47374=CARTESIAN_POINT('Ctrl Pts',(20.9131470930805,18.0080612837136,36.3929745257305));
#47375=CARTESIAN_POINT('Ctrl Pts',(21.0531639647008,17.9962644847465,36.4756182898083));
#47376=CARTESIAN_POINT('Ctrl Pts',(21.205059700778,17.9830173562508,36.5932538459348));
#47377=CARTESIAN_POINT('Ctrl Pts',(21.2284788021932,17.9809628522973,36.6122860026398));
#47378=CARTESIAN_POINT('Ctrl Pts',(21.2568041645154,17.9784724696886,36.6364305725844));
#47379=CARTESIAN_POINT('Ctrl Pts',(21.2621400485983,17.9780030918089,36.6410295827833));
#47380=CARTESIAN_POINT('Ctrl Pts',(21.2705100424778,17.9772665926524,36.6483239835229));
#47381=CARTESIAN_POINT('Ctrl Pts',(21.273560977239,17.9769980854496,36.6509998402827));
#47382=CARTESIAN_POINT('Ctrl Pts',(21.2792817985447,17.9764945556946,36.6560493779564));
#47383=CARTESIAN_POINT('Ctrl Pts',(21.2819535043678,17.9762593838645,36.6584208201161));
#47384=CARTESIAN_POINT('Ctrl Pts',(21.288040014378,17.9757235688279,36.663853590367));
#47385=CARTESIAN_POINT('Ctrl Pts',(21.2914504979222,17.9754232848245,36.6669196808877));
#47386=CARTESIAN_POINT('Ctrl Pts',(21.3004685120442,17.9746290411675,36.6750853867043));
#47387=CARTESIAN_POINT('Ctrl Pts',(21.3060570458569,17.9741366030221,36.6802059996072));
#47388=CARTESIAN_POINT('Ctrl Pts',(21.3453284545495,17.97067323034,36.7166173590701));
#47389=CARTESIAN_POINT('Ctrl Pts',(21.3779165668895,17.9677837737747,36.7490733189066));
#47390=CARTESIAN_POINT('Ctrl Pts',(21.4295724695379,17.9631135437123,36.8043360701767));
#47391=CARTESIAN_POINT('Ctrl Pts',(21.4493266779553,17.9613039127331,36.8264715265518));
#47392=CARTESIAN_POINT('Ctrl Pts',(21.5766436967247,17.9494143031022,36.9759369436844));
#47393=CARTESIAN_POINT('Ctrl Pts',(21.6678210560629,17.9397218858216,37.1162841720173));
#47394=CARTESIAN_POINT('Ctrl Pts',(21.7582953243033,17.9266846652254,37.3051617910635));
#47395=CARTESIAN_POINT('Ctrl Pts',(21.7754761284208,17.9239868220147,37.3443186442393));
#47396=CARTESIAN_POINT('Ctrl Pts',(21.7956576152852,17.9204988438613,37.3948109883221));
#47397=CARTESIAN_POINT('Ctrl Pts',(21.7998762110594,17.9197496696103,37.4056489153392));
#47398=CARTESIAN_POINT('Ctrl Pts',(21.8065004587066,17.9185399729726,37.423133248058));
#47399=CARTESIAN_POINT('Ctrl Pts',(21.8089680712289,17.9180815131348,37.429755997963));
#47400=CARTESIAN_POINT('Ctrl Pts',(21.8135960750535,17.9172064738151,37.4423887021355));
#47401=CARTESIAN_POINT('Ctrl Pts',(21.8157631278886,17.9167901213956,37.4483961293169));
#47402=CARTESIAN_POINT('Ctrl Pts',(21.820640459409,17.9158376847898,37.4621301700074));
#47403=CARTESIAN_POINT('Ctrl Pts',(21.8233314396808,17.915300973691,37.4698634592071));
#47404=CARTESIAN_POINT('Ctrl Pts',(21.8302097171325,17.913899248518,37.4900431230368));
#47405=CARTESIAN_POINT('Ctrl Pts',(21.8343192467537,17.9130317109787,37.5025153667216));
#47406=CARTESIAN_POINT('Ctrl Pts',(21.8621572879076,17.9069373598143,37.5899977240461));
#47407=CARTESIAN_POINT('Ctrl Pts',(21.8814020138474,17.9015664073956,37.6663461714946));
#47408=CARTESIAN_POINT('Ctrl Pts',(21.926408496641,17.8845678755002,37.9057979591838));
#47409=CARTESIAN_POINT('Ctrl Pts',(21.9359561248284,17.8725522417409,38.071169461438));
#47410=CARTESIAN_POINT('Ctrl Pts',(21.9217008124161,17.8584912562595,38.2732786460712));
#47411=CARTESIAN_POINT('Ctrl Pts',(21.917953697406,17.8559150443154,38.3107452920163));
#47412=CARTESIAN_POINT('Ctrl Pts',(21.9121446312209,17.8528894701586,38.3555427111758));
#47413=CARTESIAN_POINT('Ctrl Pts',(21.9111333961986,17.8523877319157,38.3629986966895));
#47414=CARTESIAN_POINT('Ctrl Pts',(21.9094948995196,17.8516120518263,38.3745707880648));
#47415=CARTESIAN_POINT('Ctrl Pts',(21.9088979061786,17.8513364735977,38.3786910001237));
#47416=CARTESIAN_POINT('Ctrl Pts',(21.9077660589251,17.850826813554,38.3863282669433));
#47417=CARTESIAN_POINT('Ctrl Pts',(21.9072348194431,17.8505925399766,38.3898457449876));
#47418=CARTESIAN_POINT('Ctrl Pts',(21.9060086786201,17.8500627913441,38.3978149998396));
#47419=CARTESIAN_POINT('Ctrl Pts',(21.905307910748,17.8497676487444,38.4022658157372));
#47420=CARTESIAN_POINT('Ctrl Pts',(21.9031342364536,17.8488746609396,38.4157635990298));
#47421=CARTESIAN_POINT('Ctrl Pts',(21.9016124137082,17.8482794846267,38.4248027224624));
#47422=CARTESIAN_POINT('Ctrl Pts',(21.88108920582,17.8406209264802,38.5416122681688));
#47423=CARTESIAN_POINT('Ctrl Pts',(21.8530123106157,17.8340264779236,38.647604613245));
#47424=CARTESIAN_POINT('Ctrl Pts',(21.7879615680553,17.8224864414853,38.8291720982697));
#47425=CARTESIAN_POINT('Ctrl Pts',(21.7547697802853,17.817534779018,38.9057798127984));
#47426=CARTESIAN_POINT('Ctrl Pts',(21.6809243565284,17.8077234430567,39.0498397900059));
#47427=CARTESIAN_POINT('Ctrl Pts',(21.6408979395498,17.8028849308972,39.1174252450024));
#47428=CARTESIAN_POINT('Ctrl Pts',(21.5861427964035,17.7966812750198,39.1982072440891));
#47429=CARTESIAN_POINT('Ctrl Pts',(21.5751808696584,17.7954575763647,39.2138731111288));
#47430=CARTESIAN_POINT('Ctrl Pts',(21.5589575305216,17.7936711498592,39.2363396572517));
#47431=CARTESIAN_POINT('Ctrl Pts',(21.5538804253971,17.793115448697,39.2432725039365));
#47432=CARTESIAN_POINT('Ctrl Pts',(21.5449155792835,17.7921399347723,39.2553440732947));
#47433=CARTESIAN_POINT('Ctrl Pts',(21.541048067607,17.7917209080448,39.2604977063565));
#47434=CARTESIAN_POINT('Ctrl Pts',(21.5334996652656,17.7909065257766,39.2704520187741));
#47435=CARTESIAN_POINT('Ctrl Pts',(21.5298218651462,17.790511294044,39.2752549558051));
#47436=CARTESIAN_POINT('Ctrl Pts',(21.5209917332053,17.7895660220169,39.2866747801002));
#47437=CARTESIAN_POINT('Ctrl Pts',(21.5158187596667,17.7890151735486,39.2932754796357));
#47438=CARTESIAN_POINT('Ctrl Pts',(21.4970653567611,17.7870284569142,39.31688604061));
#47439=CARTESIAN_POINT('Ctrl Pts',(21.4832407404018,17.7855829242982,39.3336989740883));
#47440=CARTESIAN_POINT('Ctrl Pts',(21.370372898292,17.7739258380785,39.4663244048278));
#47441=CARTESIAN_POINT('Ctrl Pts',(21.2582264811461,17.7631474187531,39.5702423589567));
#47442=CARTESIAN_POINT('Ctrl Pts',(21.0689348433601,17.7464425533277,39.7079825149376));
#47443=CARTESIAN_POINT('Ctrl Pts',(20.9998173153705,17.7406112843658,39.7518463842731));
#47444=CARTESIAN_POINT('Ctrl Pts',(20.8967893918773,17.7324679970661,39.8083877320062));
#47445=CARTESIAN_POINT('Ctrl Pts',(20.8649838068752,17.730025078358,39.8247096192004));
#47446=CARTESIAN_POINT('Ctrl Pts',(20.8260535130041,17.7271350641949,39.8433396426975));
#47447=CARTESIAN_POINT('Ctrl Pts',(20.8193478083841,17.7266407850355,39.8465012709508));
#47448=CARTESIAN_POINT('Ctrl Pts',(20.8088699341412,17.7258741226311,39.8513677851575));
#47449=CARTESIAN_POINT('Ctrl Pts',(20.8051103107286,17.7256001622782,39.8530992777373));
#47450=CARTESIAN_POINT('Ctrl Pts',(20.7981067897734,17.7250919605112,39.8562974641224));
#47451=CARTESIAN_POINT('Ctrl Pts',(20.7948644356946,17.7248575369217,39.8577672654692));
#47452=CARTESIAN_POINT('Ctrl Pts',(20.7874789972542,17.7243254883749,39.8610905670619));
#47453=CARTESIAN_POINT('Ctrl Pts',(20.7833334353033,17.7240282079958,39.8629384239635));
#47454=CARTESIAN_POINT('Ctrl Pts',(20.7706436801045,17.7231222746209,39.8685412000521));
#47455=CARTESIAN_POINT('Ctrl Pts',(20.762078571648,17.7225164052385,39.8722488304663));
#47456=CARTESIAN_POINT('Ctrl Pts',(20.6788649250874,17.7166810366408,39.9075551979002));
#47457=CARTESIAN_POINT('Ctrl Pts',(20.6023113760885,17.7117065587598,39.9344857258165));
#47458=CARTESIAN_POINT('Ctrl Pts',(20.3665569866555,17.6969203627755,40.0010626799827));
#47459=CARTESIAN_POINT('Ctrl Pts',(20.2038103148295,17.6873608829233,40.0253217744567));
#47460=CARTESIAN_POINT('Ctrl Pts',(20.0006833195611,17.6746789836716,40.0295297437341));
#47461=CARTESIAN_POINT('Ctrl Pts',(19.961398130099,17.6721956070027,40.0291436067419));
#47462=CARTESIAN_POINT('Ctrl Pts',(19.9108632608321,17.6689498473738,40.0271027192245));
#47463=CARTESIAN_POINT('Ctrl Pts',(19.8995768095378,17.6682216637664,40.0265475396934));
#47464=CARTESIAN_POINT('Ctrl Pts',(19.8813132082476,17.6670377526727,40.0254882307833));
#47465=CARTESIAN_POINT('Ctrl Pts',(19.8743326691789,17.666583930318,40.0250452465468));
#47466=CARTESIAN_POINT('Ctrl Pts',(19.8609650901427,17.6657122763461,40.0241239234207));
#47467=CARTESIAN_POINT('Ctrl Pts',(19.8545777095706,17.6652946413202,40.0236517186411));
#47468=CARTESIAN_POINT('Ctrl Pts',(19.8400250367448,17.6643404792608,40.0225029771382));
#47469=CARTESIAN_POINT('Ctrl Pts',(19.8318615092212,17.6638033289915,40.0218062156222));
#47470=CARTESIAN_POINT('Ctrl Pts',(19.8103141274487,17.6623804012654,40.0198287924061));
#47471=CARTESIAN_POINT('Ctrl Pts',(19.7969389885318,17.6614919025972,40.0184601983193));
#47472=CARTESIAN_POINT('Ctrl Pts',(19.6947210385149,17.6546603080292,40.0069199731989));
#47473=CARTESIAN_POINT('Ctrl Pts',(19.6066809751332,17.6485291662192,39.990723400181));
#47474=CARTESIAN_POINT('Ctrl Pts',(19.3632897158655,17.6309034189659,39.9282099086753));
#47475=CARTESIAN_POINT('Ctrl Pts',(19.212191915359,17.6191118337248,39.8683626782545));
#47476=CARTESIAN_POINT('Ctrl Pts',(19.043837546314,17.6058626322531,39.7757718409627));
#47477=CARTESIAN_POINT('Ctrl Pts',(19.0176724466505,17.6038023215361,39.7605693995809));
#47478=CARTESIAN_POINT('Ctrl Pts',(18.9858631155754,17.6013059089861,39.741072406246));
#47479=CARTESIAN_POINT('Ctrl Pts',(18.9798722728871,17.600836119417,39.7373550888729));
#47480=CARTESIAN_POINT('Ctrl Pts',(18.9704642763188,17.6000991209037,39.7314457482434));
#47481=CARTESIAN_POINT('Ctrl Pts',(18.967033505964,17.5998305229565,39.729275685313));
#47482=CARTESIAN_POINT('Ctrl Pts',(18.9605967001205,17.599326918891,39.7251757127561));
#47483=CARTESIAN_POINT('Ctrl Pts',(18.9575892099003,17.5990917629391,39.7232483057331));
#47484=CARTESIAN_POINT('Ctrl Pts',(18.9507345848953,17.5985561056465,39.7188284829377));
#47485=CARTESIAN_POINT('Ctrl Pts',(18.9468909707872,17.598255962729,39.7163307032178));
#47486=CARTESIAN_POINT('Ctrl Pts',(18.9367217851823,17.5974623397868,39.7096705661399));
#47487=CARTESIAN_POINT('Ctrl Pts',(18.9304116779904,17.5969703774822,39.7054845746948));
#47488=CARTESIAN_POINT('Ctrl Pts',(18.8862134354731,17.5935267295442,39.6757881572355));
#47489=CARTESIAN_POINT('Ctrl Pts',(18.8492137031909,17.59065544682,39.648974013418));
#47490=CARTESIAN_POINT('Ctrl Pts',(18.7897710514215,17.5859992803231,39.6025882491681));
#47491=CARTESIAN_POINT('Ctrl Pts',(18.7667690405704,17.5841861444455,39.5837678672533));
#47492=CARTESIAN_POINT('Ctrl Pts',(18.6570936630613,17.5754359098643,39.4897177034113));
#47493=CARTESIAN_POINT('Ctrl Pts',(18.5768163269402,17.5686887543726,39.4073875049407));
#47494=CARTESIAN_POINT('Ctrl Pts',(18.4664635073572,17.5581170463351,39.2719229011525));
#47495=CARTESIAN_POINT('Ctrl Pts',(18.4307857151483,17.5544444831011,39.2237006307591));
#47496=CARTESIAN_POINT('Ctrl Pts',(18.3840787503288,17.5491938562941,39.1539994466186));
#47497=CARTESIAN_POINT('Ctrl Pts',(18.3711167748953,17.5476829191788,39.1338547680373));
#47498=CARTESIAN_POINT('Ctrl Pts',(18.3490275472192,17.5450071361184,39.0980781207879));
#47499=CARTESIAN_POINT('Ctrl Pts',(18.3397388002028,17.5438481559237,39.0825490766422));
#47500=CARTESIAN_POINT('Ctrl Pts',(18.3264577867222,17.5421393259518,39.0596195344377));
#47501=CARTESIAN_POINT('Ctrl Pts',(18.3222930846104,17.5415956627208,39.0523196379774));
#47502=CARTESIAN_POINT('Ctrl Pts',(18.3150338679249,17.5406340120544,39.0394002568107));
#47503=CARTESIAN_POINT('Ctrl Pts',(18.3119194140304,17.5402167420926,39.0337920766176));
#47504=CARTESIAN_POINT('Ctrl Pts',(18.3058947595475,17.5394002842184,39.0228148709993));
#47505=CARTESIAN_POINT('Ctrl Pts',(18.302981965041,17.5390011944096,39.0174473496889));
#47506=CARTESIAN_POINT('Ctrl Pts',(18.2952042948898,17.5379236830919,39.0029513587995));
#47507=CARTESIAN_POINT('Ctrl Pts',(18.2903873266715,17.5372435879305,38.9937975456882));
#47508=CARTESIAN_POINT('Ctrl Pts',(18.2727277611512,17.5347017555788,38.9595735055242));
#47509=CARTESIAN_POINT('Ctrl Pts',(18.2603616546485,17.5328236112877,38.9342627189391));
#47510=CARTESIAN_POINT('Ctrl Pts',(18.2477996478815,17.5308054884993,38.9070562103519));
#47511=CARTESIAN_POINT('Ctrl Pts',(18.2470469457882,17.5306841213707,38.9054200086445));
#47512=CARTESIAN_POINT('Ctrl Pts',(18.1781034665633,17.5195266732942,38.7549982476611));
#47513=CARTESIAN_POINT('Ctrl Pts',(18.1291330819691,17.50783057734,38.5981633331092));
#47514=CARTESIAN_POINT('Ctrl Pts',(18.0848760386854,17.489793819444,38.3487689649297));
#47515=CARTESIAN_POINT('Ctrl Pts',(18.0753806866286,17.4834612818344,38.2594682013972));
#47516=CARTESIAN_POINT('Ctrl Pts',(18.0717263166812,17.4766534019954,38.1585662706702));
#47517=CARTESIAN_POINT('Ctrl Pts',(18.0714172442492,17.4758986732864,38.1473072396621));
#47518=CARTESIAN_POINT('Ctrl Pts',(18.0711152466552,17.4748231012477,38.1311475055862));
#47519=CARTESIAN_POINT('Ctrl Pts',(18.0710423641021,17.4744980594845,38.1262487906072));
#47520=CARTESIAN_POINT('Ctrl Pts',(18.0709482487533,17.4739356415033,38.117745209663));
#47521=CARTESIAN_POINT('Ctrl Pts',(18.0709184571446,17.4736977962621,38.1141404862414));
#47522=CARTESIAN_POINT('Ctrl Pts',(18.0708799478177,17.4732336793544,38.1070893228041));
#47523=CARTESIAN_POINT('Ctrl Pts',(18.0708703611119,17.4730073581601,38.1036429461361));
#47524=CARTESIAN_POINT('Ctrl Pts',(18.0708693982257,17.472388062245,38.0941912351593));
#47525=CARTESIAN_POINT('Ctrl Pts',(18.070896827741,17.4719961188606,38.0881858736622));
#47526=CARTESIAN_POINT('Ctrl Pts',(18.0711274071889,17.4703730295024,38.0632243279425));
#47527=CARTESIAN_POINT('Ctrl Pts',(18.0715819316287,17.4691550794148,38.0442707557716));
#47528=CARTESIAN_POINT('Ctrl Pts',(18.0735232595446,17.4659657751023,37.9941559548935));
#47529=CARTESIAN_POINT('Ctrl Pts',(18.0754866312828,17.4640159203536,37.9630178426873));
#47530=CARTESIAN_POINT('Ctrl Pts',(18.0903074492742,17.4535111332103,37.7935398740277));
#47531=CARTESIAN_POINT('Ctrl Pts',(18.1173257451411,17.4454043963285,37.6568444483357));
#47532=CARTESIAN_POINT('Ctrl Pts',(18.1869115785594,17.4313288350367,37.4343224430347));
#47533=CARTESIAN_POINT('Ctrl Pts',(18.2215703195123,17.4255376757858,37.3466072988216));
#47534=CARTESIAN_POINT('Ctrl Pts',(18.2683858522368,17.418657163266,37.2495654342183));
#47535=CARTESIAN_POINT('Ctrl Pts',(18.2744075236705,17.4177867994886,37.2374125563218));
#47536=CARTESIAN_POINT('Ctrl Pts',(18.2842873157464,17.4163813224155,37.2179907928233));
#47537=CARTESIAN_POINT('Ctrl Pts',(18.2880647449704,17.4158490098224,37.2106811957506));
#47538=CARTESIAN_POINT('Ctrl Pts',(18.2948678638846,17.4148990960941,37.1977206414477));
#47539=CARTESIAN_POINT('Ctrl Pts',(18.2978751928127,17.414482143134,37.1920601442882));
#47540=CARTESIAN_POINT('Ctrl Pts',(18.3042150619795,17.4136092146317,37.1802692306864));
#47541=CARTESIAN_POINT('Ctrl Pts',(18.3075527589765,17.413153061573,37.1741417072553));
#47542=CARTESIAN_POINT('Ctrl Pts',(18.3163455203352,17.4119601109682,37.1582059093984));
#47543=CARTESIAN_POINT('Ctrl Pts',(18.3218530018213,17.4112214602914,37.148427007793));
#47544=CARTESIAN_POINT('Ctrl Pts',(18.3466371663738,17.4079344063016,37.1053054699215));
#47545=CARTESIAN_POINT('Ctrl Pts',(18.3668233149437,17.4053535989622,37.0724984555972));
#47546=CARTESIAN_POINT('Ctrl Pts',(18.4241002075291,17.3982733530597,36.9853668299652));
#47547=CARTESIAN_POINT('Ctrl Pts',(18.4630066037813,17.3937118192467,36.932302676801));
#47548=CARTESIAN_POINT('Ctrl Pts',(18.5880297443326,17.3797818986968,36.7788836309515));
#47549=CARTESIAN_POINT('Ctrl Pts',(18.6818185119012,17.3702236525022,36.6852900730718));
#47550=CARTESIAN_POINT('Ctrl Pts',(18.7885694746814,17.3605993881295,36.5986649310363));
#47551=CARTESIAN_POINT('Ctrl Pts',(18.7927178673631,17.3602272253861,36.5953270255304));
#47552=CARTESIAN_POINT('Ctrl Pts',(18.8314099969384,17.3567734759212,36.56445735214));
#47553=CARTESIAN_POINT('Ctrl Pts',(18.866879228292,17.3537356999173,36.5380999255529));
#47554=CARTESIAN_POINT('Ctrl Pts',(18.9093860567517,17.3502695504009,36.508723824417));
#47555=CARTESIAN_POINT('Ctrl Pts',(18.9155717218329,17.3497693372931,36.504501972999));
#47556=CARTESIAN_POINT('Ctrl Pts',(18.9256032804263,17.3489650583872,36.4977405071107));
#47557=CARTESIAN_POINT('Ctrl Pts',(18.9294338896121,17.3486595597016,36.495178515234));
#47558=CARTESIAN_POINT('Ctrl Pts',(18.9362452312241,17.3481192605502,36.4906581880005));
#47559=CARTESIAN_POINT('Ctrl Pts',(18.9392222475974,17.3478840988925,36.4886943689302));
#47560=CARTESIAN_POINT('Ctrl Pts',(18.9456268841808,17.3473803045836,36.4844949287534));
#47561=CARTESIAN_POINT('Ctrl Pts',(18.9490561700199,17.3471118470737,36.4822619589121));
#47562=CARTESIAN_POINT('Ctrl Pts',(18.9585377044504,17.3463730809225,36.4761309574922));
#47563=CARTESIAN_POINT('Ctrl Pts',(18.9646047834258,17.3459042563914,36.4722558156308));
#47564=CARTESIAN_POINT('Ctrl Pts',(18.998070730984,17.3433387569583,36.4511433948529));
#47565=CARTESIAN_POINT('Ctrl Pts',(19.0258802789082,17.341282115695,36.4345626902992));
#47566=CARTESIAN_POINT('Ctrl Pts',(19.1623974783928,17.3314787247161,36.3577582494407));
#47567=CARTESIAN_POINT('Ctrl Pts',(19.2762675852966,17.3241649283083,36.3074713211389));
#47568=CARTESIAN_POINT('Ctrl Pts',(19.3941042778785,17.3167366370521,36.2684888941601));
#47569=CARTESIAN_POINT('Ctrl Pts',(19.3941038273433,17.1441450759092,36.2684890432051));
#47570=CARTESIAN_POINT('Ctrl Pts',(19.3466248561783,17.1472330276451,36.2841959254401));
#47571=CARTESIAN_POINT('Ctrl Pts',(19.2997551437927,17.1503686465276,36.3017494977559));
#47572=CARTESIAN_POINT('Ctrl Pts',(19.2399626035716,17.1545108494447,36.3268377160733));
#47573=CARTESIAN_POINT('Ctrl Pts',(19.2263901883899,17.1554607606846,36.3327170093857));
#47574=CARTESIAN_POINT('Ctrl Pts',(19.2058106178431,17.1569164892568,36.341914149156));
#47575=CARTESIAN_POINT('Ctrl Pts',(19.1987534281107,17.1574184785392,36.3451192172076));
#47576=CARTESIAN_POINT('Ctrl Pts',(19.186508805378,17.1582944063562,36.3507694492945));
#47577=CARTESIAN_POINT('Ctrl Pts',(19.1813125692244,17.1586676838802,36.3531953936529));
#47578=CARTESIAN_POINT('Ctrl Pts',(19.1696707294073,17.1595075407258,36.3586939253644));
#47579=CARTESIAN_POINT('Ctrl Pts',(19.163231240171,17.1599745517349,36.361779190253));
#47580=CARTESIAN_POINT('Ctrl Pts',(19.1460522088869,17.1612271021231,36.370127529649));
#47581=CARTESIAN_POINT('Ctrl Pts',(19.1353443726138,17.1620148494721,36.3754547762477));
#47582=CARTESIAN_POINT('Ctrl Pts',(19.0880756679491,17.165524107264,36.3995222880841));
#47583=CARTESIAN_POINT('Ctrl Pts',(19.0520717705113,17.1682824582813,36.4193268987948));
#47584=CARTESIAN_POINT('Ctrl Pts',(18.8819208397601,17.1817466190809,36.5201287164591));
#47585=CARTESIAN_POINT('Ctrl Pts',(18.757361200035,17.192988669626,36.6161106409262));
#47586=CARTESIAN_POINT('Ctrl Pts',(18.603357035822,17.2083624659885,36.7679029118649));
#47587=CARTESIAN_POINT('Ctrl Pts',(18.5628708565167,17.212567769212,36.8116851789057));
#47588=CARTESIAN_POINT('Ctrl Pts',(18.5054677623278,17.218708179541,36.8798416234997));
#47589=CARTESIAN_POINT('Ctrl Pts',(18.4869801654571,17.2207163440911,36.9028432481728));
#47590=CARTESIAN_POINT('Ctrl Pts',(18.4647705805944,17.2231585398011,36.9318124670456));
#47591=CARTESIAN_POINT('Ctrl Pts',(18.460544959657,17.223624583518,36.9373867088218));
#47592=CARTESIAN_POINT('Ctrl Pts',(18.4539223589926,17.2243570373054,36.9462223506294));
#47593=CARTESIAN_POINT('Ctrl Pts',(18.4515052155018,17.2246248084857,36.9494684535655));
#47594=CARTESIAN_POINT('Ctrl Pts',(18.4469724342115,17.2251277394576,36.9555959129854));
#47595=CARTESIAN_POINT('Ctrl Pts',(18.4448546143096,17.2253630440113,36.958475508769));
#47596=CARTESIAN_POINT('Ctrl Pts',(18.4400273386381,17.2259001566168,36.9650775140074));
#47597=CARTESIAN_POINT('Ctrl Pts',(18.4373231973705,17.2262015990583,36.9688037460218));
#47598=CARTESIAN_POINT('Ctrl Pts',(18.4301669489574,17.2270009466881,36.9787394920532));
#47599=CARTESIAN_POINT('Ctrl Pts',(18.4257382930485,17.2274972990487,36.9849659119414));
#47600=CARTESIAN_POINT('Ctrl Pts',(18.3941205226583,17.2310543931837,37.0299824490496));
#47601=CARTESIAN_POINT('Ctrl Pts',(18.3683287675448,17.2340285880918,37.0697396972218));
#47602=CARTESIAN_POINT('Ctrl Pts',(18.3347048283782,17.2380705512396,37.1260058294533));
#47603=CARTESIAN_POINT('Ctrl Pts',(18.3256054359271,17.2391829480689,37.1417330602599));
#47604=CARTESIAN_POINT('Ctrl Pts',(18.2340295586326,17.2505978997766,37.3052993094812));
#47605=CARTESIAN_POINT('Ctrl Pts',(18.1711329317403,17.2604053948541,37.4632509139808));
#47606=CARTESIAN_POINT('Ctrl Pts',(18.1176245190937,17.2739379495544,37.675008797129));
#47607=CARTESIAN_POINT('Ctrl Pts',(18.1074155606695,17.2770273077828,37.7230670163355));
#47608=CARTESIAN_POINT('Ctrl Pts',(18.0969799969047,17.2809549122344,37.7834475823612));
#47609=CARTESIAN_POINT('Ctrl Pts',(18.0950215768474,17.2817381665362,37.7954548282611));
#47610=CARTESIAN_POINT('Ctrl Pts',(18.0920872617245,17.2829897432161,37.8145824494882));
#47611=CARTESIAN_POINT('Ctrl Pts',(18.0910373375921,17.2834557367545,37.8216912753144));
#47612=CARTESIAN_POINT('Ctrl Pts',(18.0891324357876,17.2843368247811,37.8351071583112));
#47613=CARTESIAN_POINT('Ctrl Pts',(18.0882689034234,17.2847516447674,37.8414129193153));
#47614=CARTESIAN_POINT('Ctrl Pts',(18.0863921324074,17.285689241329,37.8556410905807));
#47615=CARTESIAN_POINT('Ctrl Pts',(18.0853968629311,17.2862125731413,37.8635657135242));
#47616=CARTESIAN_POINT('Ctrl Pts',(18.082973899544,17.2875569089069,37.8838774337265));
#47617=CARTESIAN_POINT('Ctrl Pts',(18.0816170590858,17.2883801080357,37.8962724536678));
#47618=CARTESIAN_POINT('Ctrl Pts',(18.0739981010538,17.293475326153,37.9727174843485));
#47619=CARTESIAN_POINT('Ctrl Pts',(18.0708247853875,17.2978424889978,38.0370276239346));
#47620=CARTESIAN_POINT('Ctrl Pts',(18.0709935737147,17.31428569618,38.2746646705139));
#47621=CARTESIAN_POINT('Ctrl Pts',(18.0944642165516,17.326905137099,38.4471231725448));
#47622=CARTESIAN_POINT('Ctrl Pts',(18.1522690508712,17.3420340636733,38.6561813429429));
#47623=CARTESIAN_POINT('Ctrl Pts',(18.1653254647837,17.3450344570083,38.6978439437836));
#47624=CARTESIAN_POINT('Ctrl Pts',(18.182257501738,17.3484631941258,38.7460731132526));
#47625=CARTESIAN_POINT('Ctrl Pts',(18.1847706380065,17.3489616776403,38.7531007773961));
#47626=CARTESIAN_POINT('Ctrl Pts',(18.1888988060585,17.3497637237206,38.764436745071));
#47627=CARTESIAN_POINT('Ctrl Pts',(18.1904885463405,17.3500687066338,38.7687540826491));
#47628=CARTESIAN_POINT('Ctrl Pts',(18.1933377586298,17.3506084370403,38.7764072855746));
#47629=CARTESIAN_POINT('Ctrl Pts',(18.1945910478656,17.350843542876,38.7797453837177));
#47630=CARTESIAN_POINT('Ctrl Pts',(18.1973043402401,17.3513476013438,38.7869117128464));
#47631=CARTESIAN_POINT('Ctrl Pts',(18.1987672828435,17.3516163768279,38.7907387656566));
#47632=CARTESIAN_POINT('Ctrl Pts',(18.202842378769,17.3523569191907,38.8012982167963));
#47633=CARTESIAN_POINT('Ctrl Pts',(18.2054801919365,17.3528271901558,38.8080207390469));
#47634=CARTESIAN_POINT('Ctrl Pts',(18.2202726030742,17.3554157298151,38.8451057299544));
#47635=CARTESIAN_POINT('Ctrl Pts',(18.2331608717979,17.3574931123817,38.8751722125266));
#47636=CARTESIAN_POINT('Ctrl Pts',(18.2761570799848,17.3639403345041,38.9688245067489));
#47637=CARTESIAN_POINT('Ctrl Pts',(18.3089827411975,17.3681939570088,39.0311029445779));
#47638=CARTESIAN_POINT('Ctrl Pts',(18.4321675306111,17.3825664174381,39.2367138311544));
#47639=CARTESIAN_POINT('Ctrl Pts',(18.5379298023348,17.3925253510255,39.3698669711246));
#47640=CARTESIAN_POINT('Ctrl Pts',(18.6743206414446,17.4045595746219,39.5016167243006));
#47641=CARTESIAN_POINT('Ctrl Pts',(18.6891525735954,17.4058579860225,39.5154978553391));
#47642=CARTESIAN_POINT('Ctrl Pts',(18.7102345621578,17.4076909110989,39.5346128448678));
#47643=CARTESIAN_POINT('Ctrl Pts',(18.7163031315144,17.4082170978098,39.5400455707443));
#47644=CARTESIAN_POINT('Ctrl Pts',(18.7268918840167,17.4091328494995,39.5494047497403));
#47645=CARTESIAN_POINT('Ctrl Pts',(18.7313963123563,17.4095216750882,39.5533489209093));
#47646=CARTESIAN_POINT('Ctrl Pts',(18.7408167274394,17.4103333765274,39.5615204686079));
#47647=CARTESIAN_POINT('Ctrl Pts',(18.745735804203,17.4107563967674,39.5657441521222));
#47648=CARTESIAN_POINT('Ctrl Pts',(18.7574079098118,17.4117582610419,39.5756644294138));
#47649=CARTESIAN_POINT('Ctrl Pts',(18.7641789183464,17.4123379667334,39.5813395493941));
#47650=CARTESIAN_POINT('Ctrl Pts',(18.7867791445147,17.4142682099094,39.6000191298299));
#47651=CARTESIAN_POINT('Ctrl Pts',(18.802776063946,17.4156269320817,39.6128175786455));
#47652=CARTESIAN_POINT('Ctrl Pts',(18.8897476775748,17.422976644437,39.6801563748743));
#47653=CARTESIAN_POINT('Ctrl Pts',(18.9642397515028,17.4291481241327,39.7299542979281));
#47654=CARTESIAN_POINT('Ctrl Pts',(19.1486718032791,17.4441067151472,39.8354863733714));
#47655=CARTESIAN_POINT('Ctrl Pts',(19.261025986186,17.452984531183,39.8862217786245));
#47656=CARTESIAN_POINT('Ctrl Pts',(19.3889141819031,17.4624891808049,39.929826107515));
#47657=CARTESIAN_POINT('Ctrl Pts',(19.4004228934086,17.4633391538937,39.933629396558));
#47658=CARTESIAN_POINT('Ctrl Pts',(19.455728660759,17.4673960066795,39.9513299343031));
#47659=CARTESIAN_POINT('Ctrl Pts',(19.4999811172282,17.470559376807,39.9637692235998));
#47660=CARTESIAN_POINT('Ctrl Pts',(19.5520036764247,17.474151338079,39.9764059482038));
#47661=CARTESIAN_POINT('Ctrl Pts',(19.559378511362,17.4746576011455,39.9781514041098));
#47662=CARTESIAN_POINT('Ctrl Pts',(19.5712321317639,17.4754663986526,39.9808832235179));
#47663=CARTESIAN_POINT('Ctrl Pts',(19.5757043909413,17.4757704290377,39.9818971338925));
#47664=CARTESIAN_POINT('Ctrl Pts',(19.5836669684329,17.4763096914001,39.9836725100422));
#47665=CARTESIAN_POINT('Ctrl Pts',(19.587155832155,17.4765452741794,39.9844402384101));
#47666=CARTESIAN_POINT('Ctrl Pts',(19.5946127442826,17.4770472908224,39.9860594368512));
#47667=CARTESIAN_POINT('Ctrl Pts',(19.5985813462079,17.4773135634536,39.9869080771393));
#47668=CARTESIAN_POINT('Ctrl Pts',(19.6094465586485,17.47804016809,39.9891956487217));
#47669=CARTESIAN_POINT('Ctrl Pts',(19.6163485046463,17.4784990956531,39.990609352446));
#47670=CARTESIAN_POINT('Ctrl Pts',(19.65286083927,17.4809137231423,39.9978798762687));
#47671=CARTESIAN_POINT('Ctrl Pts',(19.6825997944283,17.4828347362874,40.0030793407236));
#47672=CARTESIAN_POINT('Ctrl Pts',(19.8725655977788,17.4948865477706,40.0317148910949));
#47673=CARTESIAN_POINT('Ctrl Pts',(20.0350985655018,17.5042577192961,40.0355987150944));
#47674=CARTESIAN_POINT('Ctrl Pts',(20.2851990713135,17.5194657339569,40.0100272144236));
#47675=CARTESIAN_POINT('Ctrl Pts',(20.3734259668508,17.5249770849946,39.994753912069));
#47676=CARTESIAN_POINT('Ctrl Pts',(20.4733252013152,17.531547366867,39.9702103055575));
#47677=CARTESIAN_POINT('Ctrl Pts',(20.486348052393,17.5324102894167,39.9668660612038));
#47678=CARTESIAN_POINT('Ctrl Pts',(20.5072487393737,17.5338060542022,39.9612652696919));
#47679=CARTESIAN_POINT('Ctrl Pts',(20.5151491624077,17.534336158201,39.9590941409254));
#47680=CARTESIAN_POINT('Ctrl Pts',(20.5292003551183,17.5352835470267,39.955136265343));
#47681=CARTESIAN_POINT('Ctrl Pts',(20.5353565452275,17.5357001958642,39.9533690799954));
#47682=CARTESIAN_POINT('Ctrl Pts',(20.5482170732703,17.5365739408031,39.949607937051));
#47683=CARTESIAN_POINT('Ctrl Pts',(20.5549195839117,17.5370312216496,39.947608111439));
#47684=CARTESIAN_POINT('Ctrl Pts',(20.5724213148242,17.538230368128,39.9422823018381));
#47685=CARTESIAN_POINT('Ctrl Pts',(20.5832023213006,17.5389741226529,39.938897845064));
#47686=CARTESIAN_POINT('Ctrl Pts',(20.6313222100164,17.542317078688,39.9233259550193));
#47687=CARTESIAN_POINT('Ctrl Pts',(20.6683110936727,17.5449500583316,39.9100953489295));
#47688=CARTESIAN_POINT('Ctrl Pts',(20.8574433734043,17.5587547674413,39.8358569272763));
#47689=CARTESIAN_POINT('Ctrl Pts',(21.001744542772,17.5705318381154,39.7567734683448));
#47690=CARTESIAN_POINT('Ctrl Pts',(21.1998579473352,17.5879264461201,39.6127643095402));
#47691=CARTESIAN_POINT('Ctrl Pts',(21.2623724759653,17.5936170823236,39.5610044185568));
#47692=CARTESIAN_POINT('Ctrl Pts',(21.3282496806731,17.599694283249,39.4990648460413));
#47693=CARTESIAN_POINT('Ctrl Pts',(21.3350027157138,17.6003182247579,39.4926224956073));
#47694=CARTESIAN_POINT('Ctrl Pts',(21.3449700499153,17.6012402440448,39.4829745916844));
#47695=CARTESIAN_POINT('Ctrl Pts',(21.3482200955699,17.6015410619824,39.4798064108276));
#47696=CARTESIAN_POINT('Ctrl Pts',(21.353999339144,17.6020762415774,39.4741328245952));
#47697=CARTESIAN_POINT('Ctrl Pts',(21.3565328051478,17.6023109385029,39.4716318672685));
#47698=CARTESIAN_POINT('Ctrl Pts',(21.3619969692124,17.6028173160104,39.4662078703431));
#47699=CARTESIAN_POINT('Ctrl Pts',(21.364925180861,17.6030888025655,39.4632824140943));
#47700=CARTESIAN_POINT('Ctrl Pts',(21.3730716440955,17.6038445161755,39.4550910581509));
#47701=CARTESIAN_POINT('Ctrl Pts',(21.3782690598935,17.6043271448513,39.4498044001195));
#47702=CARTESIAN_POINT('Ctrl Pts',(21.4083439720949,17.6071236847536,39.4188582545511));
#47703=CARTESIAN_POINT('Ctrl Pts',(21.4325368891581,17.6093885813076,39.3925394750878));
#47704=CARTESIAN_POINT('Ctrl Pts',(21.5096300775044,17.6167178575088,39.3038463451829));
#47705=CARTESIAN_POINT('Ctrl Pts',(21.5593003139187,17.6216261639669,39.2387773101809));
#47706=CARTESIAN_POINT('Ctrl Pts',(21.6892672435962,17.6356251438701,39.0440001113353));
#47707=CARTESIAN_POINT('Ctrl Pts',(21.7585163967497,17.6446626504381,38.9076966251383));
#47708=CARTESIAN_POINT('Ctrl Pts',(21.818508038011,17.6556957447508,38.7442397311345));
#47709=CARTESIAN_POINT('Ctrl Pts',(21.8256608063975,17.6570855495057,38.7236817093173));
#47710=CARTESIAN_POINT('Ctrl Pts',(21.8350853582162,17.6590266058653,38.6950416909375));
#47711=CARTESIAN_POINT('Ctrl Pts',(21.8376547229854,17.6595681586443,38.6870587716318));
#47712=CARTESIAN_POINT('Ctrl Pts',(21.8419877299355,17.6605032796091,38.6732890668786));
#47713=CARTESIAN_POINT('Ctrl Pts',(21.8437763678392,17.6608960304524,38.6675102249748));
#47714=CARTESIAN_POINT('Ctrl Pts',(21.8474139708435,17.6617089518437,38.6555589031751));
#47715=CARTESIAN_POINT('Ctrl Pts',(21.8492592483525,17.6621292361721,38.6493853886505));
#47716=CARTESIAN_POINT('Ctrl Pts',(21.8534931797216,17.6631123817712,38.6349574103007));
#47717=CARTESIAN_POINT('Ctrl Pts',(21.8558576621185,17.6636760158572,38.6266960528046));
#47718=CARTESIAN_POINT('Ctrl Pts',(21.8633049126199,17.6654995541002,38.6000029217329));
#47719=CARTESIAN_POINT('Ctrl Pts',(21.8681687514959,17.666766449678,38.5815117761461));
#47720=CARTESIAN_POINT('Ctrl Pts',(21.8915917510684,17.6732790334548,38.4867598634691));
#47721=CARTESIAN_POINT('Ctrl Pts',(21.9057570415868,17.6786621811664,38.4094993058944));
#47722=CARTESIAN_POINT('Ctrl Pts',(21.9251905969021,17.689993402563,38.2487962414999));
#47723=CARTESIAN_POINT('Ctrl Pts',(21.9298227348872,17.6959444392223,38.1654355077597));
#47724=CARTESIAN_POINT('Ctrl Pts',(21.9280277087644,17.7097022743309,37.9726112312428));
#47725=CARTESIAN_POINT('Ctrl Pts',(21.9176989792529,17.7174879696582,37.8634514941308));
#47726=CARTESIAN_POINT('Ctrl Pts',(21.8965296096757,17.7254584885785,37.746726703887));
#47727=CARTESIAN_POINT('Ctrl Pts',(21.894829535186,17.7260711825722,37.7377188621129));
#47728=CARTESIAN_POINT('Ctrl Pts',(21.8921981235457,17.726979849171,37.7243018242794));
#47729=CARTESIAN_POINT('Ctrl Pts',(21.8913154718088,17.7272784498782,37.7198833795929));
#47730=CARTESIAN_POINT('Ctrl Pts',(21.8897082486846,17.7278112360272,37.7119820279318));
#47731=CARTESIAN_POINT('Ctrl Pts',(21.8889895189443,17.7280457444157,37.7084980079196));
#47732=CARTESIAN_POINT('Ctrl Pts',(21.8874087570839,17.7285534894885,37.7009410170887));
#47733=CARTESIAN_POINT('Ctrl Pts',(21.8865431790448,17.7288265226612,37.6968688519004));
#47734=CARTESIAN_POINT('Ctrl Pts',(21.8840763292713,17.7295909307443,37.6854453626619));
#47735=CARTESIAN_POINT('Ctrl Pts',(21.8824452031833,17.7300806471755,37.678100458161));
#47736=CARTESIAN_POINT('Ctrl Pts',(21.8723971659813,17.7330065240863,37.6340731439594));
#47737=CARTESIAN_POINT('Ctrl Pts',(21.8629505878155,17.7353882204672,37.5976310672761));
#47738=CARTESIAN_POINT('Ctrl Pts',(21.8064155138722,17.7479958606223,37.4031551790334));
#47739=CARTESIAN_POINT('Ctrl Pts',(21.7402764417537,17.7575213592455,37.2513667855273));
#47740=CARTESIAN_POINT('Ctrl Pts',(21.6152072292645,17.7723360313542,37.04224289614));
#47741=CARTESIAN_POINT('Ctrl Pts',(21.5706897695516,17.7772136543459,36.9772017748685));
#47742=CARTESIAN_POINT('Ctrl Pts',(21.5142594828009,17.7830839248084,36.904703691549));
#47743=CARTESIAN_POINT('Ctrl Pts',(21.5060870001048,17.7839271011124,36.8944225530173));
#47744=CARTESIAN_POINT('Ctrl Pts',(21.4926496943841,17.785302723046,36.8778680510072));
#47745=CARTESIAN_POINT('Ctrl Pts',(21.4874486905661,17.7858326269113,36.871543244381));
#47746=CARTESIAN_POINT('Ctrl Pts',(21.4781199918583,17.7867786984135,36.8603449541104));
#47747=CARTESIAN_POINT('Ctrl Pts',(21.4740080424017,17.7871942261246,36.8554584649629));
#47748=CARTESIAN_POINT('Ctrl Pts',(21.4652948229567,17.7880716692282,36.8452077524058));
#47749=CARTESIAN_POINT('Ctrl Pts',(21.4606881966393,17.7885337996984,36.8398482262944));
#47750=CARTESIAN_POINT('Ctrl Pts',(21.4484240255622,17.7897595566925,36.8257372231469));
#47751=CARTESIAN_POINT('Ctrl Pts',(21.440716716112,17.7905252286306,36.8170295731357));
#47752=CARTESIAN_POINT('Ctrl Pts',(21.4043176802565,17.7941202805483,36.7766478710943));
#47753=CARTESIAN_POINT('Ctrl Pts',(21.3746591992962,17.7969900195519,36.7458653682859));
#47754=CARTESIAN_POINT('Ctrl Pts',(21.2244128649905,17.8112582015957,36.5999508609197));
#47755=CARTESIAN_POINT('Ctrl Pts',(21.0902821087874,17.8232706425524,36.4998120957231));
#47756=CARTESIAN_POINT('Ctrl Pts',(20.8802439507439,17.8403445285271,36.3817948428981));
#47757=CARTESIAN_POINT('Ctrl Pts',(20.8134411866314,17.8455396673875,36.3491789203812));
#47758=CARTESIAN_POINT('Ctrl Pts',(20.7363634780279,17.8511549138419,36.3169135302131));
#47759=CARTESIAN_POINT('Ctrl Pts',(20.7277845233722,17.8517747563765,36.3133947759825));
#47760=CARTESIAN_POINT('Ctrl Pts',(20.7149799634452,17.8526919122638,36.3082503803218));
#47761=CARTESIAN_POINT('Ctrl Pts',(20.7107736232267,17.8529919246929,36.3065775998645));
#47762=CARTESIAN_POINT('Ctrl Pts',(20.7032497179992,17.8535262322872,36.3036161163975));
#47763=CARTESIAN_POINT('Ctrl Pts',(20.699934448287,17.8537608582476,36.3023217774193));
#47764=CARTESIAN_POINT('Ctrl Pts',(20.6927477068169,17.85426772133,36.2995388438284));
#47765=CARTESIAN_POINT('Ctrl Pts',(20.6888750193855,17.854539761022,36.2980535611039));
#47766=CARTESIAN_POINT('Ctrl Pts',(20.6780304031597,17.8552985806597,36.2939344216713));
#47767=CARTESIAN_POINT('Ctrl Pts',(20.6710478643705,17.8557837408721,36.2913284242389));
#47768=CARTESIAN_POINT('Ctrl Pts',(20.6298724774408,17.858625575113,36.2762323738592));
#47769=CARTESIAN_POINT('Ctrl Pts',(20.5953441533021,17.8609313606338,36.2646707527295));
#47770=CARTESIAN_POINT('Ctrl Pts',(20.4796924579722,17.8684646130713,36.2295533124873));
#47771=CARTESIAN_POINT('Ctrl Pts',(20.3973469004971,17.8735259282211,36.2103456677576));
#47772=CARTESIAN_POINT('Ctrl Pts',(20.1673218110452,17.8874580321404,36.1723987900647));
#47773=CARTESIAN_POINT('Ctrl Pts',(20.01835609449,17.8962919318777,36.165239088503));
#47774=CARTESIAN_POINT('Ctrl Pts',(19.8481377877441,17.9071002964135,36.1767312007854));
#47775=CARTESIAN_POINT('Ctrl Pts',(19.8262505782811,17.9085025986021,36.1785848753013));
#47776=CARTESIAN_POINT('Ctrl Pts',(19.7960264935889,17.910458331585,36.1816652488226));
#47777=CARTESIAN_POINT('Ctrl Pts',(19.7876582961799,17.9110018673493,36.1825734939668));
#47778=CARTESIAN_POINT('Ctrl Pts',(19.7732786832577,17.9119394979649,36.1842294775124));
#47779=CARTESIAN_POINT('Ctrl Pts',(19.7672643038432,17.9123327652671,36.184950824484));
#47780=CARTESIAN_POINT('Ctrl Pts',(19.7548640498272,17.9131458998751,36.1864973523323));
#47781=CARTESIAN_POINT('Ctrl Pts',(19.748478717145,17.9135658771755,36.1873262015472));
#47782=CARTESIAN_POINT('Ctrl Pts',(19.7336100889894,17.9145468258784,36.1893319694351));
#47783=CARTESIAN_POINT('Ctrl Pts',(19.7251302967363,17.9151085596906,36.190533438378));
#47784=CARTESIAN_POINT('Ctrl Pts',(19.6979023691977,17.9169197516906,36.1945763876707));
#47785=CARTESIAN_POINT('Ctrl Pts',(19.6791885123543,17.9181760695534,36.1976377666332));
#47786=CARTESIAN_POINT('Ctrl Pts',(19.5844616783375,17.9245957942414,36.2145714753432));
#47787=CARTESIAN_POINT('Ctrl Pts',(19.5092953440221,17.9298922813303,36.2327241611409));
#47788=CARTESIAN_POINT('Ctrl Pts',(19.4216019214197,17.9363075520093,36.2595632930522));
#47789=CARTESIAN_POINT('Ctrl Pts',(19.4078265464337,17.9373222382774,36.2639493266696));
#47790=CARTESIAN_POINT('Ctrl Pts',(19.3941039849792,17.9383397493623,36.2684889910563));
#47791=CARTESIAN_POINT('Origin',(20.,-1.3495818343519,38.1));
#47792=CARTESIAN_POINT('',(19.3941040358239,18.9053562004634,36.268488974236));
#47793=CARTESIAN_POINT('',(19.3941040087494,18.7329718898071,36.2684889831927));
#47794=CARTESIAN_POINT('',(19.3941040087494,-1.3495818343519,36.2684889831927));
#47795=CARTESIAN_POINT('',(18.0708707114912,18.2691024802153,38.0983431603818));
#47796=CARTESIAN_POINT('Ctrl Pts',(19.3941040358239,18.9053562004634,36.268488974236));
#47797=CARTESIAN_POINT('Ctrl Pts',(19.4279865928287,18.9028884425737,36.257280030224));
#47798=CARTESIAN_POINT('Ctrl Pts',(19.4621774215529,18.9003957441515,36.2470122283997));
#47799=CARTESIAN_POINT('Ctrl Pts',(19.6279301066995,18.8883134741058,36.202210854192));
#47800=CARTESIAN_POINT('Ctrl Pts',(19.7625999656545,18.87846861129,36.180708736018));
#47801=CARTESIAN_POINT('Ctrl Pts',(19.9444078487693,18.8657482504664,36.1711210718187));
#47802=CARTESIAN_POINT('Ctrl Pts',(19.9904840652544,18.8625766649059,36.1703433869034));
#47803=CARTESIAN_POINT('Ctrl Pts',(20.0441435471345,18.8589755877585,36.1713601636353));
#47804=CARTESIAN_POINT('Ctrl Pts',(20.0517384120818,18.8584680646239,36.1715489602943));
#47805=CARTESIAN_POINT('Ctrl Pts',(20.0639211133723,18.8576576473258,36.1719238274883));
#47806=CARTESIAN_POINT('Ctrl Pts',(20.0685096516886,18.8573532478843,36.1720814165407));
#47807=CARTESIAN_POINT('Ctrl Pts',(20.0766680465245,18.8568135715132,36.1723907725738));
#47808=CARTESIAN_POINT('Ctrl Pts',(20.0802380916115,18.8565779417876,36.1725360775168));
#47809=CARTESIAN_POINT('Ctrl Pts',(20.0878588872093,18.8560760957557,36.1728674629983));
#47810=CARTESIAN_POINT('Ctrl Pts',(20.0919094542126,18.8558100392864,36.1730563962044));
#47811=CARTESIAN_POINT('Ctrl Pts',(20.1029805800088,18.8550846378359,36.1736077824848));
#47812=CARTESIAN_POINT('Ctrl Pts',(20.1099998867849,18.8546266895134,36.1739958452306));
#47813=CARTESIAN_POINT('Ctrl Pts',(20.1469385480426,18.8522264016984,36.176240601705));
#47814=CARTESIAN_POINT('Ctrl Pts',(20.1768156307629,18.8503182619047,36.1787562275007));
#47815=CARTESIAN_POINT('Ctrl Pts',(20.3677859082086,18.8382660162591,36.1993288814617));
#47816=CARTESIAN_POINT('Ctrl Pts',(20.5261336682632,18.8288854925308,36.236934522012));
#47817=CARTESIAN_POINT('Ctrl Pts',(20.7617214358697,18.8136638026088,36.325363683888));
#47818=CARTESIAN_POINT('Ctrl Pts',(20.8432163549248,18.8081487846095,36.3626063647711));
#47819=CARTESIAN_POINT('Ctrl Pts',(20.9336379624654,18.8015744429003,36.4117928055435));
#47820=CARTESIAN_POINT('Ctrl Pts',(20.9453825693801,18.8007114187338,36.4183415450199));
#47821=CARTESIAN_POINT('Ctrl Pts',(20.964171898234,18.79931552053,36.4290774265798));
#47822=CARTESIAN_POINT('Ctrl Pts',(20.9712602129664,18.7987853855734,36.4331876857271));
#47823=CARTESIAN_POINT('Ctrl Pts',(20.9838422407657,18.797837960456,36.4405910614918));
#47824=CARTESIAN_POINT('Ctrl Pts',(20.9893461761992,18.7974213064506,36.4438666352287));
#47825=CARTESIAN_POINT('Ctrl Pts',(21.0008261948645,18.7965475702287,36.4507764235942));
#47826=CARTESIAN_POINT('Ctrl Pts',(21.0067990193744,18.7960903033636,36.4544158454446));
#47827=CARTESIAN_POINT('Ctrl Pts',(21.0223683947148,18.7948912373375,36.4640192286843));
#47828=CARTESIAN_POINT('Ctrl Pts',(21.0319324603638,18.7941475497584,36.4700350903479));
#47829=CARTESIAN_POINT('Ctrl Pts',(21.0744964436095,18.7908053466849,36.4973328936649));
#47830=CARTESIAN_POINT('Ctrl Pts',(21.1068927751893,18.7881730718187,36.5195340988735));
#47831=CARTESIAN_POINT('Ctrl Pts',(21.2708892342792,18.7743702751573,36.6394372117908));
#47832=CARTESIAN_POINT('Ctrl Pts',(21.3903082149122,18.7625945067091,36.7526217243822));
#47833=CARTESIAN_POINT('Ctrl Pts',(21.5452710390451,18.7451989200551,36.942305347138));
#47834=CARTESIAN_POINT('Ctrl Pts',(21.5925746065654,18.7395062365368,37.0082908594777));
#47835=CARTESIAN_POINT('Ctrl Pts',(21.6405370062164,18.7334271307516,37.0849788209207));
#47836=CARTESIAN_POINT('Ctrl Pts',(21.6454285534588,18.7328031707232,37.0929277350625));
#47837=CARTESIAN_POINT('Ctrl Pts',(21.6526129269065,18.7318811289652,37.1047946589798));
#47838=CARTESIAN_POINT('Ctrl Pts',(21.6549498358871,18.7315803068929,37.1086856206448));
#47839=CARTESIAN_POINT('Ctrl Pts',(21.6590951614778,18.731045122223,37.1156431158905));
#47840=CARTESIAN_POINT('Ctrl Pts',(21.6609088378502,18.7308104243373,37.1187064337312));
#47841=CARTESIAN_POINT('Ctrl Pts',(21.664812923785,18.7303040473092,37.1253423073996));
#47842=CARTESIAN_POINT('Ctrl Pts',(21.6669003140247,18.730032562181,37.1289165675148));
#47843=CARTESIAN_POINT('Ctrl Pts',(21.6726941395154,18.7292768587188,37.1389111230811));
#47844=CARTESIAN_POINT('Ctrl Pts',(21.6763751438252,18.7287942386887,37.1453461909082));
#47845=CARTESIAN_POINT('Ctrl Pts',(21.6975841375381,18.7259978670986,37.1829243442474));
#47846=CARTESIAN_POINT('Ctrl Pts',(21.7142824358835,18.7237331232623,37.2145307535176));
#47847=CARTESIAN_POINT('Ctrl Pts',(21.7662636980626,18.7164046056339,37.3199103185352));
#47848=CARTESIAN_POINT('Ctrl Pts',(21.7977382892531,18.7114968679667,37.3954670749589));
#47849=CARTESIAN_POINT('Ctrl Pts',(21.8738690109192,18.6974976324576,37.6169066532795));
#47850=CARTESIAN_POINT('Ctrl Pts',(21.9061587211823,18.6884593674046,37.7663581157598));
#47851=CARTESIAN_POINT('Ctrl Pts',(21.9225827392108,18.6774254373416,37.9397130966413));
#47852=CARTESIAN_POINT('Ctrl Pts',(21.9242687082187,18.6760356831469,37.9614137158783));
#47853=CARTESIAN_POINT('Ctrl Pts',(21.9260951240433,18.6740946853724,37.9915082624133));
#47854=CARTESIAN_POINT('Ctrl Pts',(21.9265485424183,18.6735531398232,37.9998820991973));
#47855=CARTESIAN_POINT('Ctrl Pts',(21.9272350225703,18.6726180273037,38.0143009977634));
#47856=CARTESIAN_POINT('Ctrl Pts',(21.927494277311,18.6722252776356,38.0203447380468));
#47857=CARTESIAN_POINT('Ctrl Pts',(21.9279709641847,18.6714123548817,38.0328283071692));
#47858=CARTESIAN_POINT('Ctrl Pts',(21.9281845662766,18.670992067998,38.0392681982428));
#47859=CARTESIAN_POINT('Ctrl Pts',(21.9286077367307,18.670008909832,38.0542988125277));
#47860=CARTESIAN_POINT('Ctrl Pts',(21.9287921734676,18.6694452656836,38.0628900517682));
#47861=CARTESIAN_POINT('Ctrl Pts',(21.9292018549228,18.667621667027,38.090600472372));
#47862=CARTESIAN_POINT('Ctrl Pts',(21.9292002484896,18.6663547204668,38.109721361915));
#47863=CARTESIAN_POINT('Ctrl Pts',(21.9277410707954,18.6598416983572,38.2073210527086));
#47864=CARTESIAN_POINT('Ctrl Pts',(21.9217791785243,18.6544581425518,38.2856486197102));
#47865=CARTESIAN_POINT('Ctrl Pts',(21.8996781125919,18.643126792372,38.4460079327577));
#47866=CARTESIAN_POINT('Ctrl Pts',(21.8829458212707,18.6371760651468,38.5277988937013));
#47867=CARTESIAN_POINT('Ctrl Pts',(21.8321443296497,18.6234187330786,38.7138121255422));
#47868=CARTESIAN_POINT('Ctrl Pts',(21.7943791787877,18.6156332331695,38.8167477653367));
#47869=CARTESIAN_POINT('Ctrl Pts',(21.7442055763267,18.6076628822398,38.9242411610009));
#47870=CARTESIAN_POINT('Ctrl Pts',(21.7402692573582,18.6070501814031,38.9325199721509));
#47871=CARTESIAN_POINT('Ctrl Pts',(21.7343102672356,18.606141506179,38.9448258727096));
#47872=CARTESIAN_POINT('Ctrl Pts',(21.7323323265838,18.605842903625,38.9488742954846));
#47873=CARTESIAN_POINT('Ctrl Pts',(21.7287673888927,18.6053101148966,38.9561066095845));
#47874=CARTESIAN_POINT('Ctrl Pts',(21.7271857580987,18.6050756057683,38.9592930638519));
#47875=CARTESIAN_POINT('Ctrl Pts',(21.7237340492838,18.6045678598723,38.9661990622883));
#47876=CARTESIAN_POINT('Ctrl Pts',(21.7218607471181,18.604294826613,38.969916925064));
#47877=CARTESIAN_POINT('Ctrl Pts',(21.7165682537206,18.6035304201946,38.980336635482));
#47878=CARTESIAN_POINT('Ctrl Pts',(21.7131218246948,18.6030407054971,38.9870246782026));
#47879=CARTESIAN_POINT('Ctrl Pts',(21.6922015669189,18.6001148778458,39.0270451897662));
#47880=CARTESIAN_POINT('Ctrl Pts',(21.6737931588567,18.5977332267981,39.0598832445379));
#47881=CARTESIAN_POINT('Ctrl Pts',(21.5696369614075,18.5851261390324,39.233563757592));
#47882=CARTESIAN_POINT('Ctrl Pts',(21.467056640143,18.5756010858206,39.363519889001));
#47883=CARTESIAN_POINT('Ctrl Pts',(21.2928922685819,18.5607864625144,39.5339370312864));
#47884=CARTESIAN_POINT('Ctrl Pts',(21.2332835541578,18.5559083310408,39.5855151377765));
#47885=CARTESIAN_POINT('Ctrl Pts',(21.1602557659134,18.5500375004795,39.6412727244261));
#47886=CARTESIAN_POINT('Ctrl Pts',(21.1497359160123,18.5491943069441,39.6491360053703));
#47887=CARTESIAN_POINT('Ctrl Pts',(21.1325281305167,18.5478186616568,39.6617264952663));
#47888=CARTESIAN_POINT('Ctrl Pts',(21.1258888255783,18.5472887518036,39.66651969712));
#47889=CARTESIAN_POINT('Ctrl Pts',(21.1140175554239,18.5463426726037,39.67497562828));
#47890=CARTESIAN_POINT('Ctrl Pts',(21.1087975084621,18.5459271432117,39.6786549423681));
#47891=CARTESIAN_POINT('Ctrl Pts',(21.0977626717661,18.5450496996428,39.6863510390286));
#47892=CARTESIAN_POINT('Ctrl Pts',(21.0919438975729,18.5445875704024,39.690361916317));
#47893=CARTESIAN_POINT('Ctrl Pts',(21.0764928330725,18.5433618238192,39.700887553645));
#47894=CARTESIAN_POINT('Ctrl Pts',(21.0668235698513,18.5425961611333,39.7073472679779));
#47895=CARTESIAN_POINT('Ctrl Pts',(21.0213486366556,18.5390012350159,39.7371364685813));
#47896=CARTESIAN_POINT('Ctrl Pts',(20.9848349623899,18.5361316160571,39.7593578463153));
#47897=CARTESIAN_POINT('Ctrl Pts',(20.8024049678732,18.5218634648756,39.8622375198034));
#47898=CARTESIAN_POINT('Ctrl Pts',(20.6472064754203,18.5098509131442,39.9249495083712));
#47899=CARTESIAN_POINT('Ctrl Pts',(20.4572099081198,18.4959375204752,39.9744017679639));
#47900=CARTESIAN_POINT('Ctrl Pts',(20.4283265846151,18.4938456205883,39.9812122014931));
#47901=CARTESIAN_POINT('Ctrl Pts',(20.354319242381,18.4885607628087,39.9968695137484));
#47902=CARTESIAN_POINT('Ctrl Pts',(20.3090116240405,18.485395651227,40.0047752310021));
#47903=CARTESIAN_POINT('Ctrl Pts',(20.2559523982726,18.4818019558225,40.0120900541216));
#47904=CARTESIAN_POINT('Ctrl Pts',(20.2484377585391,18.481295617541,40.0130809418328));
#47905=CARTESIAN_POINT('Ctrl Pts',(20.2363672141464,18.4804867229273,40.0146002529206));
#47906=CARTESIAN_POINT('Ctrl Pts',(20.23181501808,18.480182670097,40.01515675256));
#47907=CARTESIAN_POINT('Ctrl Pts',(20.2237133447715,18.4796433820441,40.0161178611919));
#47908=CARTESIAN_POINT('Ctrl Pts',(20.2201646815855,18.4794077959006,40.0165288498716));
#47909=CARTESIAN_POINT('Ctrl Pts',(20.2125823913388,18.4789057879544,40.0173856554739));
#47910=CARTESIAN_POINT('Ctrl Pts',(20.2085484999104,18.4786395273031,40.0178286025767));
#47911=CARTESIAN_POINT('Ctrl Pts',(20.1975087096364,18.4779129913451,40.0190055984819));
#47912=CARTESIAN_POINT('Ctrl Pts',(20.1905000546746,18.4774541200304,40.0197140178416));
#47913=CARTESIAN_POINT('Ctrl Pts',(20.1534525944717,18.4750403299827,40.0232538033017));
#47914=CARTESIAN_POINT('Ctrl Pts',(20.1233524050859,18.4731200694443,40.0254187389954));
#47915=CARTESIAN_POINT('Ctrl Pts',(19.931466875929,18.4610682259363,40.0347011196064));
#47916=CARTESIAN_POINT('Ctrl Pts',(19.7693640057219,18.4516965015293,40.022130225164));
#47917=CARTESIAN_POINT('Ctrl Pts',(19.523117959376,18.4364876902177,39.9713969670692));
#47918=CARTESIAN_POINT('Ctrl Pts',(19.4368844454189,18.4309761353501,39.9472793050387));
#47919=CARTESIAN_POINT('Ctrl Pts',(19.3399759327773,18.4244056264147,39.9127580000953));
#47920=CARTESIAN_POINT('Ctrl Pts',(19.3273579228201,18.4235426967808,39.9081139227264));
#47921=CARTESIAN_POINT('Ctrl Pts',(19.3071306139714,18.4221469219908,39.9004281997334));
#47922=CARTESIAN_POINT('Ctrl Pts',(19.2994902051603,18.4216168151261,39.8974692521485));
#47923=CARTESIAN_POINT('Ctrl Pts',(19.2859112233468,18.4206694220664,39.8921107103568));
#47924=CARTESIAN_POINT('Ctrl Pts',(19.279965279406,18.4202527718719,39.8897300295323));
#47925=CARTESIAN_POINT('Ctrl Pts',(19.2685206941146,18.419447274567,39.8850814993782));
#47926=CARTESIAN_POINT('Ctrl Pts',(19.2630204616251,18.4190585685583,39.8828177397166));
#47927=CARTESIAN_POINT('Ctrl Pts',(19.2484957368356,18.4180278404939,39.8767610213651));
#47928=CARTESIAN_POINT('Ctrl Pts',(19.2394895883261,18.4173843669203,39.8729247847466));
#47929=CARTESIAN_POINT('Ctrl Pts',(19.2047780672397,18.4148870883174,39.8578259983877));
#47930=CARTESIAN_POINT('Ctrl Pts',(19.1792915255596,18.4130167389818,39.8460720554327));
#47931=CARTESIAN_POINT('Ctrl Pts',(19.1157950825728,18.4082609821854,39.815091275985));
#47932=CARTESIAN_POINT('Ctrl Pts',(19.0781502118757,18.405352447107,39.7951545449619));
#47933=CARTESIAN_POINT('Ctrl Pts',(18.951568167736,18.3952640196245,39.7226528447727));
#47934=CARTESIAN_POINT('Ctrl Pts',(18.8662141408769,18.3879106766327,39.6642049910201));
#47935=CARTESIAN_POINT('Ctrl Pts',(18.7485382815897,18.377106009697,39.5689126724992));
#47936=CARTESIAN_POINT('Ctrl Pts',(18.7122662266137,18.3736728269615,39.537220521548));
#47937=CARTESIAN_POINT('Ctrl Pts',(18.6635745399251,18.368949740658,39.4913521595892));
#47938=CARTESIAN_POINT('Ctrl Pts',(18.6501195729557,18.3676317706043,39.47830211078));
#47939=CARTESIAN_POINT('Ctrl Pts',(18.6282397353287,18.365469779963,39.4564529576632));
#47940=CARTESIAN_POINT('Ctrl Pts',(18.6197043500747,18.3646215120667,39.4477665898224));
#47941=CARTESIAN_POINT('Ctrl Pts',(18.5862182690156,18.361275996785,39.4130363828288));
#47942=CARTESIAN_POINT('Ctrl Pts',(18.5619159151269,18.3588086015177,39.3863739339686));
#47943=CARTESIAN_POINT('Ctrl Pts',(18.5337694767405,18.3559182821019,39.3536986790859));
#47944=CARTESIAN_POINT('Ctrl Pts',(18.5291945236669,18.3554474121623,39.3483283141154));
#47945=CARTESIAN_POINT('Ctrl Pts',(18.521764521934,18.3546810940101,39.3395089640379));
#47946=CARTESIAN_POINT('Ctrl Pts',(18.5188918870594,18.3543844192641,39.3360749812733));
#47947=CARTESIAN_POINT('Ctrl Pts',(18.5137594279751,18.3538536935155,39.3298959956339));
#47948=CARTESIAN_POINT('Ctrl Pts',(18.511495224394,18.3536193302982,39.3271547301269));
#47949=CARTESIAN_POINT('Ctrl Pts',(18.5065824144553,18.3531103133785,39.3211732004809));
#47950=CARTESIAN_POINT('Ctrl Pts',(18.5039367753411,18.3528358717413,39.3179305805471));
#47951=CARTESIAN_POINT('Ctrl Pts',(18.4965009742207,18.3520635205958,39.3087561241266));
#47952=CARTESIAN_POINT('Ctrl Pts',(18.4917353301862,18.3515673253521,39.3028043808685));
#47953=CARTESIAN_POINT('Ctrl Pts',(18.4625108914312,18.348515978153,39.2658595885145));
#47954=CARTESIAN_POINT('Ctrl Pts',(18.4389710669212,18.3460208678525,39.234147489685));
#47955=CARTESIAN_POINT('Ctrl Pts',(18.3462116290715,18.3359278021567,39.1008192724799));
#47956=CARTESIAN_POINT('Ctrl Pts',(18.2858046671633,18.3286983579506,38.9934175308054));
#47957=CARTESIAN_POINT('Ctrl Pts',(18.2176969925881,18.3186159956408,38.8395868333897));
#47958=CARTESIAN_POINT('Ctrl Pts',(18.2008303435292,18.3158887646577,38.7975535797615));
#47959=CARTESIAN_POINT('Ctrl Pts',(18.1765130489254,18.3115224209491,38.7301841915164));
#47960=CARTESIAN_POINT('Ctrl Pts',(18.1680764458122,18.3099056265385,38.7052212738422));
#47961=CARTESIAN_POINT('Ctrl Pts',(18.1451153433479,18.3051807115958,38.6323970628846));
#47962=CARTESIAN_POINT('Ctrl Pts',(18.1319383003056,18.3020388113213,38.5841369009836));
#47963=CARTESIAN_POINT('Ctrl Pts',(18.1177952202452,18.2980259177535,38.5230932404615));
#47964=CARTESIAN_POINT('Ctrl Pts',(18.1150601675272,18.2972116968971,38.5107365806387));
#47965=CARTESIAN_POINT('Ctrl Pts',(18.1109254715718,18.2959173272052,38.4911448223578));
#47966=CARTESIAN_POINT('Ctrl Pts',(18.1094453317726,18.2954397353801,38.4839269331126));
#47967=CARTESIAN_POINT('Ctrl Pts',(18.1067673281757,18.2945483255462,38.4704765639346));
#47968=CARTESIAN_POINT('Ctrl Pts',(18.1055587967007,18.2941348516338,38.4642462899228));
#47969=CARTESIAN_POINT('Ctrl Pts',(18.1032531762537,18.2933235075824,38.4520383207266));
#47970=CARTESIAN_POINT('Ctrl Pts',(18.1021535483972,18.2929257230616,38.4460611757613));
#47971=CARTESIAN_POINT('Ctrl Pts',(18.0997488500494,18.2920308691293,38.432633929072));
#47972=CARTESIAN_POINT('Ctrl Pts',(18.0984593192382,18.2915333157581,38.4251811807504));
#47973=CARTESIAN_POINT('Ctrl Pts',(18.095328484002,18.2902792790412,38.4064310570249));
#47974=CARTESIAN_POINT('Ctrl Pts',(18.0935438599705,18.2895210313382,38.3951246400291));
#47975=CARTESIAN_POINT('Ctrl Pts',(18.0778019814019,18.2824029989518,38.2892847239816));
#47976=CARTESIAN_POINT('Ctrl Pts',(18.0707886681054,18.2758266780971,38.1938697863096));
#47977=CARTESIAN_POINT('Ctrl Pts',(18.0708707114912,18.2691024802153,38.0983431603818));
#47978=CARTESIAN_POINT('Ctrl Pts',(18.0708707098941,18.2691026111891,38.0983450210486));
#47979=CARTESIAN_POINT('Ctrl Pts',(18.0709927887356,18.2590858989335,37.9560435925063));
#47980=CARTESIAN_POINT('Ctrl Pts',(18.0868588827055,18.2487689296965,37.8141939336366));
#47981=CARTESIAN_POINT('Ctrl Pts',(18.1270478385106,18.2360716426373,37.6360873122555));
#47982=CARTESIAN_POINT('Ctrl Pts',(18.1371422810743,18.2333104483011,37.5970820586233));
#47983=CARTESIAN_POINT('Ctrl Pts',(18.1506036166244,18.23009793581,37.5510607131297));
#47984=CARTESIAN_POINT('Ctrl Pts',(18.1527996249639,18.2295866233175,37.543715807505));
#47985=CARTESIAN_POINT('Ctrl Pts',(18.156264691227,18.2287993813945,37.5323731359882));
#47986=CARTESIAN_POINT('Ctrl Pts',(18.1575030700035,18.2285217381387,37.5283661929623));
#47987=CARTESIAN_POINT('Ctrl Pts',(18.1598152317272,18.2280101752501,37.5209704568609));
#47988=CARTESIAN_POINT('Ctrl Pts',(18.1608853062107,18.2277760517167,37.5175806178726));
#47989=CARTESIAN_POINT('Ctrl Pts',(18.1633208047732,18.2272490508019,37.5099389590244));
#47990=CARTESIAN_POINT('Ctrl Pts',(18.1646916227376,18.226956491189,37.5056889201785));
#47991=CARTESIAN_POINT('Ctrl Pts',(18.1682544544884,18.226206353967,37.4947727247075));
#47992=CARTESIAN_POINT('Ctrl Pts',(18.1704681282575,18.2257500051746,37.4881136280383));
#47993=CARTESIAN_POINT('Ctrl Pts',(18.1840886098786,18.2229992349661,37.4478757676948));
#47994=CARTESIAN_POINT('Ctrl Pts',(18.196384057608,18.2207530073682,37.4146022275572));
#47995=CARTESIAN_POINT('Ctrl Pts',(18.2616062774572,18.2098320683145,37.2520352118364));
#47996=CARTESIAN_POINT('Ctrl Pts',(18.3275546142103,18.2016718832744,37.128407939038));
#47997=CARTESIAN_POINT('Ctrl Pts',(18.4461706633492,18.1890107699173,36.9545011753525));
#47998=CARTESIAN_POINT('Ctrl Pts',(18.4892419832452,18.1847059514516,36.8982670404358));
#47999=CARTESIAN_POINT('Ctrl Pts',(18.5527205047,18.178623330714,36.8242097016456));
#48000=CARTESIAN_POINT('Ctrl Pts',(18.5705581466442,18.1769398363856,36.8042551538008));
#48001=CARTESIAN_POINT('Ctrl Pts',(18.6021370776523,18.1739975714233,36.7703744207057));
#48002=CARTESIAN_POINT('Ctrl Pts',(18.6156859794422,18.1727467061579,36.7562739941704));
#48003=CARTESIAN_POINT('Ctrl Pts',(18.6353993109885,18.1709415702723,36.7363728270069));
#48004=CARTESIAN_POINT('Ctrl Pts',(18.6413915057379,18.1703947811229,36.7304025909208));
#48005=CARTESIAN_POINT('Ctrl Pts',(18.652065087305,18.1694240592722,36.7199070978753));
#48006=CARTESIAN_POINT('Ctrl Pts',(18.6567305132805,18.169000835926,36.7153657408262));
#48007=CARTESIAN_POINT('Ctrl Pts',(18.6657058841987,18.1681886414293,36.70671710914));
#48008=CARTESIAN_POINT('Ctrl Pts',(18.6700120357579,18.1677998428589,36.702605991474));
#48009=CARTESIAN_POINT('Ctrl Pts',(18.6812601820085,18.166786465465,36.6919663848167));
#48010=CARTESIAN_POINT('Ctrl Pts',(18.6882315761584,18.1661605576443,36.6854693478907));
#48011=CARTESIAN_POINT('Ctrl Pts',(18.7122253482798,18.1640134625408,36.663438107282));
#48012=CARTESIAN_POINT('Ctrl Pts',(18.7294772451185,18.1624817388153,36.6481579022675));
#48013=CARTESIAN_POINT('Ctrl Pts',(18.7514540215372,18.1605446002153,36.6293845368507));
#48014=CARTESIAN_POINT('Ctrl Pts',(18.7559272159538,18.1601510287671,36.6255984917529));
#48015=CARTESIAN_POINT('Ctrl Pts',(18.7647635617159,18.1593749618448,36.6181883827864));
#48016=CARTESIAN_POINT('Ctrl Pts',(18.7691255852936,18.1589925207967,36.6145630604229));
#48017=CARTESIAN_POINT('Ctrl Pts',(18.8808201560189,18.1492163804646,36.5225623552322));
#48018=CARTESIAN_POINT('Ctrl Pts',(18.9973611441368,18.1393626800269,36.4460423973926));
#48019=CARTESIAN_POINT('Ctrl Pts',(19.193876158995,18.1236100169408,36.3454649978827));
#48020=CARTESIAN_POINT('Ctrl Pts',(19.2689651970021,18.1177790844306,36.3128742318829));
#48021=CARTESIAN_POINT('Ctrl Pts',(19.3618940954089,18.1109345064276,36.2793813001041));
#48022=CARTESIAN_POINT('Ctrl Pts',(19.3779634961239,18.1097640782246,36.2738285480579));
#48023=CARTESIAN_POINT('Ctrl Pts',(19.3941040099181,18.1086029180356,36.2684889828061));
#48024=CARTESIAN_POINT('',(18.0708700800916,18.0972931656481,38.1005558905092));
#48025=CARTESIAN_POINT('Ctrl Pts',(19.3941039849792,17.9383397493623,36.2684889910563));
#48026=CARTESIAN_POINT('Ctrl Pts',(19.3277365019718,17.9432608167489,36.2904445202804));
#48027=CARTESIAN_POINT('Ctrl Pts',(19.2626045320947,17.94825059431,36.3159934977218));
#48028=CARTESIAN_POINT('Ctrl Pts',(19.0990040968448,17.9610814169626,36.3906637379445));
#48029=CARTESIAN_POINT('Ctrl Pts',(19.0030818212519,17.9689029729662,36.4447706847563));
#48030=CARTESIAN_POINT('Ctrl Pts',(18.904715536788,17.9769053466831,36.5119261875009));
#48031=CARTESIAN_POINT('Ctrl Pts',(18.8971859309992,17.9775176980835,36.5171457342324));
#48032=CARTESIAN_POINT('Ctrl Pts',(18.8860098446164,17.9784259575908,36.5250114976304));
#48033=CARTESIAN_POINT('Ctrl Pts',(18.8823351203309,17.97872449042,36.5276170737809));
#48034=CARTESIAN_POINT('Ctrl Pts',(18.875857808555,17.9792504694546,36.5322440145261));
#48035=CARTESIAN_POINT('Ctrl Pts',(18.8730515018359,17.9794782698759,36.5342600536114));
#48036=CARTESIAN_POINT('Ctrl Pts',(18.8702364811364,17.9797066930512,36.5362938419746));
#48037=CARTESIAN_POINT('Ctrl Pts',(18.8702224061067,17.9797078351591,36.5363040111524));
#48038=CARTESIAN_POINT('Ctrl Pts',(18.8701944404558,17.9797101044071,36.5363242168478));
#48039=CARTESIAN_POINT('Ctrl Pts',(18.8701805493144,17.9797112315895,36.5363342537338));
#48040=CARTESIAN_POINT('Ctrl Pts',(18.8701529457148,17.9797134714514,36.5363541989603));
#48041=CARTESIAN_POINT('Ctrl Pts',(18.8701392339535,17.9797145840743,36.5363641067899));
#48042=CARTESIAN_POINT('Ctrl Pts',(18.8701119880107,17.979716794907,36.5363837946793));
#48043=CARTESIAN_POINT('Ctrl Pts',(18.8700984530356,17.9797178931811,36.5363935753054));
#48044=CARTESIAN_POINT('Ctrl Pts',(18.8700715554113,17.9797200757425,36.5364130125634));
#48045=CARTESIAN_POINT('Ctrl Pts',(18.8700581932288,17.979721159992,36.5364226688512));
#48046=CARTESIAN_POINT('Ctrl Pts',(18.8700316384551,17.9797233147261,36.5364418593885));
#48047=CARTESIAN_POINT('Ctrl Pts',(18.8700184458732,17.9797243852101,36.5364513936247));
#48048=CARTESIAN_POINT('Ctrl Pts',(18.8699922271578,17.9797265126685,36.5364703423106));
#48049=CARTESIAN_POINT('Ctrl Pts',(18.8699792009983,17.979727569645,36.5364797567726));
#48050=CARTESIAN_POINT('Ctrl Pts',(18.8699533116913,17.9797296703675,36.5364984683748));
#48051=CARTESIAN_POINT('Ctrl Pts',(18.8699404486903,17.9797307141015,36.5365077654028));
#48052=CARTESIAN_POINT('Ctrl Pts',(18.8699148828083,17.9797327885738,36.5365262442089));
#48053=CARTESIAN_POINT('Ctrl Pts',(18.8699021799507,17.9797338193101,36.536535425964));
#48054=CARTESIAN_POINT('Ctrl Pts',(18.8698769312513,17.979735868039,36.5365536764501));
#48055=CARTESIAN_POINT('Ctrl Pts',(18.8698643855199,17.9797368860226,36.5365627450955));
#48056=CARTESIAN_POINT('Ctrl Pts',(18.8665249059686,17.9800078570793,36.5389767393582));
#48057=CARTESIAN_POINT('Ctrl Pts',(18.8632056188321,17.9802770777515,36.5413923056859));
#48058=CARTESIAN_POINT('Ctrl Pts',(18.8563288971778,17.9808346597385,36.5464304013698));
#48059=CARTESIAN_POINT('Ctrl Pts',(18.8527727084887,17.981122906609,36.5490546006509));
#48060=CARTESIAN_POINT('Ctrl Pts',(18.8436975604666,17.9818583307661,36.5557996682553));
#48061=CARTESIAN_POINT('Ctrl Pts',(18.8381915396358,17.9823043688936,36.559937955469));
#48062=CARTESIAN_POINT('Ctrl Pts',(18.8222387969623,17.9835966206416,36.5720621711873));
#48063=CARTESIAN_POINT('Ctrl Pts',(18.8118511912981,17.98443798512,36.5801256994036));
#48064=CARTESIAN_POINT('Ctrl Pts',(18.6795083383585,17.9951680270764,36.6850448182652));
#48065=CARTESIAN_POINT('Ctrl Pts',(18.5696174930387,18.0042309761275,36.7962299322465));
#48066=CARTESIAN_POINT('Ctrl Pts',(18.4085889332594,18.0200426334144,37.0043369298933));
#48067=CARTESIAN_POINT('Ctrl Pts',(18.3501040333848,18.026599804252,37.0945621384814));
#48068=CARTESIAN_POINT('Ctrl Pts',(18.2929082324169,18.0343332591703,37.201350440622));
#48069=CARTESIAN_POINT('Ctrl Pts',(18.2865179946428,18.035219407154,37.2135956143202));
#48070=CARTESIAN_POINT('Ctrl Pts',(18.2764986973697,18.0366454652541,37.2333081720509));
#48071=CARTESIAN_POINT('Ctrl Pts',(18.2727853177892,18.0371824400009,37.2407323450648));
#48072=CARTESIAN_POINT('Ctrl Pts',(18.2662849442655,18.0381377069583,37.2539409672086));
#48073=CARTESIAN_POINT('Ctrl Pts',(18.2634786782526,18.0385553251934,37.2597158344308));
#48074=CARTESIAN_POINT('Ctrl Pts',(18.2576977755182,18.0394266500136,37.2717646915404));
#48075=CARTESIAN_POINT('Ctrl Pts',(18.2547280826925,18.0398805192784,37.2780409376645));
#48076=CARTESIAN_POINT('Ctrl Pts',(18.2471126302361,18.0410609237232,37.2943630302245));
#48077=CARTESIAN_POINT('Ctrl Pts',(18.2425193802715,18.0417892404303,37.3044329564387));
#48078=CARTESIAN_POINT('Ctrl Pts',(18.2229428513685,18.0449661634383,37.3483481917766));
#48079=CARTESIAN_POINT('Ctrl Pts',(18.2088496002262,18.0474445565694,37.3825792892292));
#48080=CARTESIAN_POINT('Ctrl Pts',(18.1737736068415,18.054165550835,37.4752640666428));
#48081=CARTESIAN_POINT('Ctrl Pts',(18.1546152883436,18.0584627071874,37.5343571908967));
#48082=CARTESIAN_POINT('Ctrl Pts',(18.0935163511218,18.0748294278555,37.7592688521627));
#48083=CARTESIAN_POINT('Ctrl Pts',(18.07083099567,18.0873145772518,37.9294803634274));
#48084=CARTESIAN_POINT('Ctrl Pts',(18.0708700503369,18.0989811937323,38.1004406959586));
#48085=CARTESIAN_POINT('Ctrl Pts',(18.0708700800916,18.0972931656481,38.1005558905092));
#48086=CARTESIAN_POINT('Ctrl Pts',(18.0708789271142,18.0993153349082,38.1312580803398));
#48087=CARTESIAN_POINT('Ctrl Pts',(18.0716206740858,18.1013375041683,38.1619487263116));
#48088=CARTESIAN_POINT('Ctrl Pts',(18.0730939131179,18.1033596734284,38.1926039374795));
#48089=CARTESIAN_POINT('Ctrl Pts',(18.0763419964673,18.1078179956423,38.2601901735182));
#48090=CARTESIAN_POINT('Ctrl Pts',(18.0831566834011,18.1122763178562,38.3277388219117));
#48091=CARTESIAN_POINT('Ctrl Pts',(18.0935346887358,18.1167346400701,38.394843303886));
#48092=CARTESIAN_POINT('Ctrl Pts',(18.1044314108777,18.1214157995817,38.4653018237035));
#48093=CARTESIAN_POINT('Ctrl Pts',(18.1192570644502,18.1260969590932,38.5352700676509));
#48094=CARTESIAN_POINT('Ctrl Pts',(18.137945881509,18.1307781186048,38.6042787093571));
#48095=CARTESIAN_POINT('Ctrl Pts',(18.1556967837643,18.1352243499884,38.669824091381));
#48096=CARTESIAN_POINT('Ctrl Pts',(18.1769322927136,18.1396705813721,38.7345033216825));
#48097=CARTESIAN_POINT('Ctrl Pts',(18.2015434544663,18.1441168127558,38.7979230693471));
#48098=CARTESIAN_POINT('Ctrl Pts',(18.2261397598962,18.148560360209,38.8613045342093));
#48099=CARTESIAN_POINT('Ctrl Pts',(18.2541074979079,18.1530039076621,38.923427565825));
#48100=CARTESIAN_POINT('Ctrl Pts',(18.2852883467481,18.1574474551153,38.9839154388866));
#48101=CARTESIAN_POINT('Ctrl Pts',(18.3164611195515,18.1618898516615,39.044387645207));
#48102=CARTESIAN_POINT('Ctrl Pts',(18.3508451250287,18.1663322482078,39.1032250956793));
#48103=CARTESIAN_POINT('Ctrl Pts',(18.3882353091368,18.1707746447541,39.1600741191948));
#48104=CARTESIAN_POINT('Ctrl Pts',(18.4256286944911,18.1752174216464,39.2169280099697));
#48105=CARTESIAN_POINT('Ctrl Pts',(18.4660284961405,18.1796601985386,39.2717927253538));
#48106=CARTESIAN_POINT('Ctrl Pts',(18.5091864227286,18.1841029754308,39.3243436750861));
#48107=CARTESIAN_POINT('Ctrl Pts',(18.5523908687846,18.1885505411448,39.3769512689255));
#48108=CARTESIAN_POINT('Ctrl Pts',(18.5983590580795,18.1929981068588,39.4272397392126));
#48109=CARTESIAN_POINT('Ctrl Pts',(18.6468031794314,18.1974456725728,39.4749185145684));
#48110=CARTESIAN_POINT('Ctrl Pts',(18.6952775897809,18.2018960190639,39.5226271004001));
#48111=CARTESIAN_POINT('Ctrl Pts',(18.7462306433898,18.2063463655551,39.5677224177369));
#48112=CARTESIAN_POINT('Ctrl Pts',(18.7993406385498,18.2107967120463,39.6099535273187));
#48113=CARTESIAN_POINT('Ctrl Pts',(18.85254045301,18.2152545849363,39.6522560578956));
#48114=CARTESIAN_POINT('Ctrl Pts',(18.9079040862449,18.2197124578263,39.6916844300659));
#48115=CARTESIAN_POINT('Ctrl Pts',(18.9650808375466,18.2241703307163,39.7280309837613));
#48116=CARTESIAN_POINT('Ctrl Pts',(18.9860818903373,18.2258077099267,39.7413810932995));
#48117=CARTESIAN_POINT('Ctrl Pts',(19.0073273168203,18.2274450891371,39.7543158869174));
#48118=CARTESIAN_POINT('Ctrl Pts',(19.0287989942023,18.2290824683474,39.7668266746238));
#48119=CARTESIAN_POINT('Ctrl Pts',(19.0872629441823,18.2335407905619,39.800891552447));
#48120=CARTESIAN_POINT('Ctrl Pts',(19.1476367921603,18.2379991127763,39.8319440618328));
#48121=CARTESIAN_POINT('Ctrl Pts',(19.2095776841387,18.2424574349907,39.8597656433424));
#48122=CARTESIAN_POINT('Ctrl Pts',(19.2746145257327,18.2471385945022,39.8889778121011));
#48123=CARTESIAN_POINT('Ctrl Pts',(19.3413787477654,18.2518197540137,39.9146272530517));
#48124=CARTESIAN_POINT('Ctrl Pts',(19.4094408477271,18.2565009135252,39.9365136657718));
#48125=CARTESIAN_POINT('Ctrl Pts',(19.4740871910489,18.2609471449094,39.9573016895264));
#48126=CARTESIAN_POINT('Ctrl Pts',(19.539903742999,18.2653933762936,39.9746951125107));
#48127=CARTESIAN_POINT('Ctrl Pts',(19.6065012435478,18.2698396076778,39.9885712286198));
#48128=CARTESIAN_POINT('Ctrl Pts',(19.67305854307,18.2742831551314,40.0024389685271));
#48129=CARTESIAN_POINT('Ctrl Pts',(19.7403953742742,18.2787267025851,40.0127935129869));
#48130=CARTESIAN_POINT('Ctrl Pts',(19.8081095343543,18.2831702500388,40.0195626080163));
#48131=CARTESIAN_POINT('Ctrl Pts',(19.8758061560391,18.2876126465856,40.0263299498073));
#48132=CARTESIAN_POINT('Ctrl Pts',(19.9438794220707,18.2920550431324,40.0295136368982));
#48133=CARTESIAN_POINT('Ctrl Pts',(20.0119210310178,18.2964974396792,40.0290931667287));
#48134=CARTESIAN_POINT('Ctrl Pts',(20.079968465503,18.3009402165719,40.0286726605597));
#48135=CARTESIAN_POINT('Ctrl Pts',(20.1479837444357,18.3053829934647,40.0246473903624));
#48136=CARTESIAN_POINT('Ctrl Pts',(20.2155594257593,18.3098257703574,40.0170489536958));
#48137=CARTESIAN_POINT('Ctrl Pts',(20.2832079461876,18.3142733360719,40.0094423267556));
#48138=CARTESIAN_POINT('Ctrl Pts',(20.3504154326781,18.3187209017864,39.9982549038406));
#48139=CARTESIAN_POINT('Ctrl Pts',(20.4167814684665,18.3231684675009,39.9835699520971));
#48140=CARTESIAN_POINT('Ctrl Pts',(20.4831889986744,18.3276188139925,39.9688758187964));
#48141=CARTESIAN_POINT('Ctrl Pts',(20.5487535562374,18.3320691604842,39.9506799371097));
#48142=CARTESIAN_POINT('Ctrl Pts',(20.6130895226733,18.3365195069758,39.9291155770176));
#48143=CARTESIAN_POINT('Ctrl Pts',(20.6775342937034,18.3409773798663,39.9075147474111));
#48144=CARTESIAN_POINT('Ctrl Pts',(20.7407458698446,18.3454352527569,39.8825342538263));
#48145=CARTESIAN_POINT('Ctrl Pts',(20.8023591529402,18.3498931256474,39.8543552509663));
#48146=CARTESIAN_POINT('Ctrl Pts',(20.8249897462869,18.3515305048537,39.8440050874528));
#48147=CARTESIAN_POINT('Ctrl Pts',(20.8474049658539,18.3531678840601,39.8332238555599));
#48148=CARTESIAN_POINT('Ctrl Pts',(20.8695876570089,18.3548052632665,39.8220220276401));
#48149=CARTESIAN_POINT('Ctrl Pts',(20.9299875841307,18.3592635854801,39.791521238297));
#48150=CARTESIAN_POINT('Ctrl Pts',(20.9889001583487,18.3637219076937,39.757778558256));
#48151=CARTESIAN_POINT('Ctrl Pts',(21.0459554096211,18.3681802299074,39.7209626269549));
#48152=CARTESIAN_POINT('Ctrl Pts',(21.1058624148533,18.372861389419,39.6823065499085));
#48153=CARTESIAN_POINT('Ctrl Pts',(21.1637210377508,18.3775425489306,39.6402621100675));
#48154=CARTESIAN_POINT('Ctrl Pts',(21.2191294593047,18.3822237084422,39.5950805725296));
#48155=CARTESIAN_POINT('Ctrl Pts',(21.2717571602427,18.3866699398256,39.5521665103929));
#48156=CARTESIAN_POINT('Ctrl Pts',(21.3221742267561,18.391116171209,39.5064229963557));
#48157=CARTESIAN_POINT('Ctrl Pts',(21.3700658366063,18.3955624025924,39.4581097747474));
#48158=CARTESIAN_POINT('Ctrl Pts',(21.4179285370851,18.4000059500453,39.4098257170128));
#48159=CARTESIAN_POINT('Ctrl Pts',(21.4632684585658,18.4044494974982,39.3589753783089));
#48160=CARTESIAN_POINT('Ctrl Pts',(21.5058060562462,18.4088930449511,39.305856823123));
#48161=CARTESIAN_POINT('Ctrl Pts',(21.5483326364202,18.4133354414971,39.2527520259784));
#48162=CARTESIAN_POINT('Ctrl Pts',(21.5880580257213,18.4177778380432,39.1973805635166));
#48163=CARTESIAN_POINT('Ctrl Pts',(21.6247427722402,18.4222202345892,39.1400737863023));
#48164=CARTESIAN_POINT('Ctrl Pts',(21.6614306596078,18.4266630114812,39.082762102637));
#48165=CARTESIAN_POINT('Ctrl Pts',(21.6950771238612,18.4311057883732,39.0235151920824));
#48166=CARTESIAN_POINT('Ctrl Pts',(21.7254868859807,18.4355485652652,38.9626920442479));
#48167=CARTESIAN_POINT('Ctrl Pts',(21.7559294264579,18.4399961309789,38.901803335792));
#48168=CARTESIAN_POINT('Ctrl Pts',(21.7831280828116,18.4444436966927,38.8393354419349));
#48169=CARTESIAN_POINT('Ctrl Pts',(21.8069347440799,18.4488912624064,38.7756695845877));
#48170=CARTESIAN_POINT('Ctrl Pts',(21.8307562901244,18.4533416088974,38.711963921069));
#48171=CARTESIAN_POINT('Ctrl Pts',(21.8511814729861,18.4577919553883,38.6470592739138));
#48172=CARTESIAN_POINT('Ctrl Pts',(21.8681121826909,18.4622423018792,38.5813516695534));
#48173=CARTESIAN_POINT('Ctrl Pts',(21.8850715255088,18.466700174769,38.5155329408929));
#48174=CARTESIAN_POINT('Ctrl Pts',(21.8985245059642,18.4711580476588,38.4489090282691));
#48175=CARTESIAN_POINT('Ctrl Pts',(21.9084243529671,18.4756159205486,38.3818848096334));
#48176=CARTESIAN_POINT('Ctrl Pts',(21.912060572323,18.4772532997609,38.3572667765423));
#48177=CARTESIAN_POINT('Ctrl Pts',(21.9152179467829,18.4788906789733,38.3325947676987));
#48178=CARTESIAN_POINT('Ctrl Pts',(21.9178959233884,18.4805280581856,38.3078888740416));
#48179=CARTESIAN_POINT('Ctrl Pts',(21.9251876261883,18.484986380399,38.2406186695197));
#48180=CARTESIAN_POINT('Ctrl Pts',(21.9289501929268,18.4894447026124,38.1728314808468));
#48181=CARTESIAN_POINT('Ctrl Pts',(21.9291237019229,18.4939030248258,38.1049294603374));
#48182=CARTESIAN_POINT('Ctrl Pts',(21.9293058833016,18.4985841843374,38.0336335391473));
#48183=CARTESIAN_POINT('Ctrl Pts',(21.9255306696707,18.503265343849,37.9622115332449));
#48184=CARTESIAN_POINT('Ctrl Pts',(21.9177901148132,18.5079465033606,37.8911372880935));
#48185=CARTESIAN_POINT('Ctrl Pts',(21.9104380265441,18.5123927347438,37.8236299667682));
#48186=CARTESIAN_POINT('Ctrl Pts',(21.8995090759222,18.5168389661269,37.7564369038082));
#48187=CARTESIAN_POINT('Ctrl Pts',(21.8850497851158,18.5212851975101,37.6899635814528));
#48188=CARTESIAN_POINT('Ctrl Pts',(21.8705992225398,18.5257287449627,37.6235303851648));
#48189=CARTESIAN_POINT('Ctrl Pts',(21.8526226517929,18.5301722924153,37.557816548496));
#48190=CARTESIAN_POINT('Ctrl Pts',(21.8312179433442,18.5346158398679,37.493218819611));
#48191=CARTESIAN_POINT('Ctrl Pts',(21.8098187788502,18.5390582364137,37.428637821946));
#48192=CARTESIAN_POINT('Ctrl Pts',(21.7849933945691,18.5435006329594,37.3651728260429));
#48193=CARTESIAN_POINT('Ctrl Pts',(21.7568894075675,18.5479430295052,37.3032050662328));
#48194=CARTESIAN_POINT('Ctrl Pts',(21.7287830143787,18.5523858063969,37.2412320009111));
#48195=CARTESIAN_POINT('Ctrl Pts',(21.6973976674127,18.5568285832886,37.1807568741046));
#48196=CARTESIAN_POINT('Ctrl Pts',(21.6629282141081,18.5612713601803,37.1221389098531));
#48197=CARTESIAN_POINT('Ctrl Pts',(21.6284216065481,18.5657189258937,37.0634577619243));
#48198=CARTESIAN_POINT('Ctrl Pts',(21.5908245101539,18.5701664916071,37.0066381965217));
#48199=CARTESIAN_POINT('Ctrl Pts',(21.5503760975718,18.5746140573206,36.9520119717618));
#48200=CARTESIAN_POINT('Ctrl Pts',(21.5099023951951,18.5790644038112,36.8973515927322));
#48201=CARTESIAN_POINT('Ctrl Pts',(21.466574143152,18.5835147503018,36.8448876632989));
#48202=CARTESIAN_POINT('Ctrl Pts',(21.4206701504348,18.5879650967924,36.7949180559967));
#48203=CARTESIAN_POINT('Ctrl Pts',(21.3746885251648,18.5924229696819,36.744863940399));
#48204=CARTESIAN_POINT('Ctrl Pts',(21.3261228195484,18.5968808425714,36.6973129082982));
#48205=CARTESIAN_POINT('Ctrl Pts',(21.27528721341,18.6013387154609,36.6525245839003));
#48206=CARTESIAN_POINT('Ctrl Pts',(21.2566152667401,18.6029760946755,36.6360738072082));
#48207=CARTESIAN_POINT('Ctrl Pts',(21.2376373892696,18.6046134738901,36.6199953370601));
#48208=CARTESIAN_POINT('Ctrl Pts',(21.2183701336408,18.6062508531047,36.6043005735269));
#48209=CARTESIAN_POINT('Ctrl Pts',(21.1659084723098,18.6107091753216,36.5615662378739));
#48210=CARTESIAN_POINT('Ctrl Pts',(21.1110920955775,18.6151674975385,36.521510967239));
#48211=CARTESIAN_POINT('Ctrl Pts',(21.0542257384865,18.6196258197553,36.4844039337716));
#48212=CARTESIAN_POINT('Ctrl Pts',(20.9945170688538,18.6243069792665,36.4454422046282));
#48213=CARTESIAN_POINT('Ctrl Pts',(20.9325484801317,18.6289881387777,36.409731573502));
#48214=CARTESIAN_POINT('Ctrl Pts',(20.8687131405122,18.6336692982889,36.3775366371381));
#48215=CARTESIAN_POINT('Ctrl Pts',(20.808081433792,18.6381155296755,36.3469574320908));
#48216=CARTESIAN_POINT('Ctrl Pts',(20.7457663349597,18.6425617610622,36.3195498029366));
#48217=CARTESIAN_POINT('Ctrl Pts',(20.6821333135934,18.6470079924488,36.2954954421265));
#48218=CARTESIAN_POINT('Ctrl Pts',(20.6185387037704,18.6514515399049,36.271455601531));
#48219=CARTESIAN_POINT('Ctrl Pts',(20.5536282098857,18.655895087361,36.2507651879098));
#48220=CARTESIAN_POINT('Ctrl Pts',(20.4877879254899,18.6603386348171,36.2335580650215));
#48221=CARTESIAN_POINT('Ctrl Pts',(20.4219646941437,18.6647810313663,36.2163553988867));
#48222=CARTESIAN_POINT('Ctrl Pts',(20.355212627337,18.6692234279155,36.2026343568969));
#48223=CARTESIAN_POINT('Ctrl Pts',(20.2879318834082,18.6736658244648,36.1924786272712));
#48224=CARTESIAN_POINT('Ctrl Pts',(20.2206453790846,18.6781086013599,36.1823220281396));
#48225=CARTESIAN_POINT('Ctrl Pts',(20.1528305957856,18.6825513782551,36.1757314182156));
#48226=CARTESIAN_POINT('Ctrl Pts',(20.0848949372993,18.6869941551503,36.1727388847069));
#48227=CARTESIAN_POINT('Ctrl Pts',(20.0168860516933,18.6914417208671,36.1697431255783));
#48228=CARTESIAN_POINT('Ctrl Pts',(19.9487565244515,18.695889286584,36.1703532028808));
#48229=CARTESIAN_POINT('Ctrl Pts',(19.8809148468747,18.7003368523008,36.1745490701643));
#48230=CARTESIAN_POINT('Ctrl Pts',(19.8130307522546,18.7047871987949,36.1787475608541));
#48231=CARTESIAN_POINT('Ctrl Pts',(19.7454353552026,18.7092375452889,36.186536246299));
#48232=CARTESIAN_POINT('Ctrl Pts',(19.6785302969749,18.7136878917829,36.1978433852764));
#48233=CARTESIAN_POINT('Ctrl Pts',(19.6115120893214,18.7181457646757,36.2091696468181));
#48234=CARTESIAN_POINT('Ctrl Pts',(19.5451870305379,18.7226036375686,36.2240261268957));
#48235=CARTESIAN_POINT('Ctrl Pts',(19.4799439301978,18.7270615104614,36.2422905929177));
#48236=CARTESIAN_POINT('Ctrl Pts',(19.455980103236,18.7286988896488,36.2489991414236));
#48237=CARTESIAN_POINT('Ctrl Pts',(19.4321620631573,18.7303362688363,36.2561669850272));
#48238=CARTESIAN_POINT('Ctrl Pts',(19.4085083833019,18.7319736480237,36.2637864437175));
#48239=CARTESIAN_POINT('Ctrl Pts',(19.4037014960229,18.7323063952849,36.2653348657505));
#48240=CARTESIAN_POINT('Ctrl Pts',(19.398899982941,18.732639142546,36.2669023907506));
#48241=CARTESIAN_POINT('Ctrl Pts',(19.3941040087494,18.7329718898071,36.2684889831927));
#48242=CARTESIAN_POINT('Origin',(20.,-1.3495818343519,38.1));
#48243=CARTESIAN_POINT('',(19.3941041453487,19.6985952145508,36.2684889380033));
#48244=CARTESIAN_POINT('',(19.3941040005193,19.5258959448669,36.2684889859154));
#48245=CARTESIAN_POINT('',(19.3941040087494,-1.3495818343519,36.2684889831927));
#48246=CARTESIAN_POINT('Ctrl Pts',(19.3941041453486,19.6985952145508,36.2684889380033));
#48247=CARTESIAN_POINT('Ctrl Pts',(19.4450720666877,19.6953436865102,36.2516278592469));
#48248=CARTESIAN_POINT('Ctrl Pts',(19.4967669479744,19.6920519773128,36.2368866026938));
#48249=CARTESIAN_POINT('Ctrl Pts',(19.5872481096025,19.6862432079621,36.2151336500013));
#48250=CARTESIAN_POINT('Ctrl Pts',(19.6257066615318,19.6837600036393,36.2071213884289));
#48251=CARTESIAN_POINT('Ctrl Pts',(19.6755084276242,19.6805144398755,36.1983229870329));
#48252=CARTESIAN_POINT('Ctrl Pts',(19.6866527598072,19.6797862746826,36.1964549544536));
#48253=CARTESIAN_POINT('Ctrl Pts',(19.7047208584644,19.6786023867189,36.1935893126101));
#48254=CARTESIAN_POINT('Ctrl Pts',(19.711634877699,19.6781485689502,36.1925312493969));
#48255=CARTESIAN_POINT('Ctrl Pts',(19.7248907374021,19.6772769191734,36.1905764030618));
#48256=CARTESIAN_POINT('Ctrl Pts',(19.7312316006745,19.676859283731,36.189673555441));
#48257=CARTESIAN_POINT('Ctrl Pts',(19.7456939561376,19.6759051143159,36.1876877546404));
#48258=CARTESIAN_POINT('Ctrl Pts',(19.7538180439075,19.6753679570666,36.1866249377858));
#48259=CARTESIAN_POINT('Ctrl Pts',(19.7752910791765,19.6739449970673,36.1839547934479));
#48260=CARTESIAN_POINT('Ctrl Pts',(19.7886502929527,19.6730564728975,36.1824352374703));
#48261=CARTESIAN_POINT('Ctrl Pts',(19.8909905440559,19.6662238034002,36.1718768750724));
#48262=CARTESIAN_POINT('Ctrl Pts',(19.9804742634496,19.6600915429246,36.1688976224292));
#48263=CARTESIAN_POINT('Ctrl Pts',(20.2316577276156,19.642461665015,36.1779959611759));
#48264=CARTESIAN_POINT('Ctrl Pts',(20.3920906973116,19.6306669272838,36.2042082385043));
#48265=CARTESIAN_POINT('Ctrl Pts',(20.5763214509395,19.6174190056741,36.2587209840939));
#48266=CARTESIAN_POINT('Ctrl Pts',(20.6050808027085,19.6153622280458,36.2679704417416));
#48267=CARTESIAN_POINT('Ctrl Pts',(20.6402685646424,19.6128694846665,36.2802065019418));
#48268=CARTESIAN_POINT('Ctrl Pts',(20.6469115693081,19.6123999458869,36.2825573913535));
#48269=CARTESIAN_POINT('Ctrl Pts',(20.6573602689549,19.6116632518081,36.2863196241069));
#48270=CARTESIAN_POINT('Ctrl Pts',(20.6611745644145,19.6113947093778,36.2877066393029));
#48271=CARTESIAN_POINT('Ctrl Pts',(20.6683378568902,19.6108911508514,36.2903370956704));
#48272=CARTESIAN_POINT('Ctrl Pts',(20.671687738482,19.6106559852612,36.2915777869976));
#48273=CARTESIAN_POINT('Ctrl Pts',(20.6793295390427,19.6101202319867,36.2944322338715));
#48274=CARTESIAN_POINT('Ctrl Pts',(20.6836191611811,19.6098200032003,36.2960519895978));
#48275=CARTESIAN_POINT('Ctrl Pts',(20.69498156031,19.6090260028816,36.3003887662237));
#48276=CARTESIAN_POINT('Ctrl Pts',(20.7020442616477,19.6085337513689,36.3031322193441));
#48277=CARTESIAN_POINT('Ctrl Pts',(20.7516096732668,19.6050870164219,36.3227223834682));
#48278=CARTESIAN_POINT('Ctrl Pts',(20.7935217398094,19.6022130868392,36.3410352917277));
#48279=CARTESIAN_POINT('Ctrl Pts',(20.8709346850246,19.596910671452,36.3781909061901));
#48280=CARTESIAN_POINT('Ctrl Pts',(20.9065731311006,19.5944719941572,36.3966858093375));
#48281=CARTESIAN_POINT('Ctrl Pts',(21.0353392133235,19.585579747793,36.4686974476995));
#48282=CARTESIAN_POINT('Ctrl Pts',(21.1245271061465,19.579249798928,36.5288493356327));
#48283=CARTESIAN_POINT('Ctrl Pts',(21.2699502421611,19.5679478801657,36.6456844163888));
#48284=CARTESIAN_POINT('Ctrl Pts',(21.3285378578071,19.563070066982,36.6990030662686));
#48285=CARTESIAN_POINT('Ctrl Pts',(21.3970638577969,19.5568191566934,36.7695399359665));
#48286=CARTESIAN_POINT('Ctrl Pts',(21.4102395078475,19.5555900523645,36.7835138082815));
#48287=CARTESIAN_POINT('Ctrl Pts',(21.4290154720382,19.55379715977,36.8040326216604));
#48288=CARTESIAN_POINT('Ctrl Pts',(21.4347843222286,19.5532404707329,36.8104223133957));
#48289=CARTESIAN_POINT('Ctrl Pts',(21.444797592595,19.5522638104782,36.8216635720516));
#48290=CARTESIAN_POINT('Ctrl Pts',(21.4490608538908,19.5518446309552,36.8264982345394));
#48291=CARTESIAN_POINT('Ctrl Pts',(21.4572751243033,19.5510303845625,36.8359081080643));
#48292=CARTESIAN_POINT('Ctrl Pts',(21.461229020697,19.5506354435315,36.8404807080284));
#48293=CARTESIAN_POINT('Ctrl Pts',(21.4706059137799,19.5496915613067,36.851428474423));
#48294=CARTESIAN_POINT('Ctrl Pts',(21.4760090049088,19.5491418173647,36.8578204550754));
#48295=CARTESIAN_POINT('Ctrl Pts',(21.4952462139623,19.5471631334401,36.8808812418922));
#48296=CARTESIAN_POINT('Ctrl Pts',(21.5088405160797,19.5457246306201,36.8977471068365));
#48297=CARTESIAN_POINT('Ctrl Pts',(21.6168046330804,19.5339626365527,37.0364093936724));
#48298=CARTESIAN_POINT('Ctrl Pts',(21.6965386268226,19.5230580575429,37.1688606242217));
#48299=CARTESIAN_POINT('Ctrl Pts',(21.7926845956981,19.506318879313,37.382841529062));
#48300=CARTESIAN_POINT('Ctrl Pts',(21.8210722022559,19.5005761306837,37.4583365240643));
#48301=CARTESIAN_POINT('Ctrl Pts',(21.8550280454731,19.4925391297536,37.5692747715017));
#48302=CARTESIAN_POINT('Ctrl Pts',(21.8644647222796,19.4901173817071,37.6034418380367));
#48303=CARTESIAN_POINT('Ctrl Pts',(21.8747269826856,19.4872489673208,37.6450318842951));
#48304=CARTESIAN_POINT('Ctrl Pts',(21.8764573343121,19.4867559189422,37.6522220161931));
#48305=CARTESIAN_POINT('Ctrl Pts',(21.8790907223582,19.4859907450418,37.663447925789));
#48306=CARTESIAN_POINT('Ctrl Pts',(21.8800221786886,19.4857170521077,37.6674768621368));
#48307=CARTESIAN_POINT('Ctrl Pts',(21.8817315189482,19.4852090882355,37.6749803247635));
#48308=CARTESIAN_POINT('Ctrl Pts',(21.8825127314461,19.4849746367145,37.6784539764126));
#48309=CARTESIAN_POINT('Ctrl Pts',(21.8842691623348,19.4844421938637,37.6863661865534));
#48310=CARTESIAN_POINT('Ctrl Pts',(21.8852383156825,19.4841445491747,37.6908060339177));
#48311=CARTESIAN_POINT('Ctrl Pts',(21.8881558937132,19.4832363995607,37.7044023340271));
#48312=CARTESIAN_POINT('Ctrl Pts',(21.8900534014347,19.4826286981317,37.7135697468165));
#48313=CARTESIAN_POINT('Ctrl Pts',(21.9084459662552,19.4765574017428,37.8058074632603));
#48314=CARTESIAN_POINT('Ctrl Pts',(21.9195226661703,19.4713724424426,37.8898764808825));
#48315=CARTESIAN_POINT('Ctrl Pts',(21.9320124983956,19.4598106414727,38.0813224927145));
#48316=CARTESIAN_POINT('Ctrl Pts',(21.9300690586937,19.4534950127833,38.188627698923));
#48317=CARTESIAN_POINT('Ctrl Pts',(21.9112254697708,19.4422127118766,38.373883479013));
#48318=CARTESIAN_POINT('Ctrl Pts',(21.8983957625082,19.43733954541,38.4519748630206));
#48319=CARTESIAN_POINT('Ctrl Pts',(21.8765434173371,19.4310942230102,38.5477675947507));
#48320=CARTESIAN_POINT('Ctrl Pts',(21.8719952854018,19.4298657574009,38.566416793531));
#48321=CARTESIAN_POINT('Ctrl Pts',(21.8650059611557,19.4280736291312,38.593324840563));
#48322=CARTESIAN_POINT('Ctrl Pts',(21.8627864732165,19.4275170571197,38.6016404935037));
#48323=CARTESIAN_POINT('Ctrl Pts',(21.8588076293095,19.4265405331711,38.6161572434294));
#48324=CARTESIAN_POINT('Ctrl Pts',(21.8570726889956,19.4261213722608,38.6223649383649));
#48325=CARTESIAN_POINT('Ctrl Pts',(21.8536502720967,19.4253071112306,38.6343779317725));
#48326=CARTESIAN_POINT('Ctrl Pts',(21.8519665501002,19.4249121367109,38.6401842288741));
#48327=CARTESIAN_POINT('Ctrl Pts',(21.8478862505894,19.423968092992,38.6540117736719));
#48328=CARTESIAN_POINT('Ctrl Pts',(21.8454647133025,19.4234182204107,38.6620254698071));
#48329=CARTESIAN_POINT('Ctrl Pts',(21.8365868932361,19.4214386019765,38.6907291226157));
#48330=CARTESIAN_POINT('Ctrl Pts',(21.8298343990209,19.4199992814802,38.711325052741));
#48331=CARTESIAN_POINT('Ctrl Pts',(21.7723371871785,19.4082489441412,38.8772033569532));
#48332=CARTESIAN_POINT('Ctrl Pts',(21.7047302169484,19.3973584360644,39.01602443409));
#48333=CARTESIAN_POINT('Ctrl Pts',(21.5776462431174,19.3806230929494,39.2131433939542));
#48334=CARTESIAN_POINT('Ctrl Pts',(21.5296992873417,19.374870503537,39.2781670624535));
#48335=CARTESIAN_POINT('Ctrl Pts',(21.4550176825506,19.3668216735174,39.3671717560366));
#48336=CARTESIAN_POINT('Ctrl Pts',(21.4314711366642,19.3643975594919,39.3937122914088));
#48337=CARTESIAN_POINT('Ctrl Pts',(21.4021443421209,19.3615267309661,39.424986233868));
#48338=CARTESIAN_POINT('Ctrl Pts',(21.3970532826923,19.3610335450384,39.4303531131852));
#48339=CARTESIAN_POINT('Ctrl Pts',(21.3890679805113,19.3602682051111,39.4386746451258));
#48340=CARTESIAN_POINT('Ctrl Pts',(21.3861949617295,19.3599944826119,39.4416494284491));
#48341=CARTESIAN_POINT('Ctrl Pts',(21.3808307476517,19.3594864927861,39.447168022063));
#48342=CARTESIAN_POINT('Ctrl Pts',(21.3783421001483,19.3592520446986,39.4497141507026));
#48343=CARTESIAN_POINT('Ctrl Pts',(21.372661390296,19.3587196468601,39.4554939725149));
#48344=CARTESIAN_POINT('Ctrl Pts',(21.3694649483432,19.3584220435173,39.4587232824368));
#48345=CARTESIAN_POINT('Ctrl Pts',(21.3596503603843,19.3575141451976,39.4685689712746));
#48346=CARTESIAN_POINT('Ctrl Pts',(21.3529953345434,19.3569066514613,39.4751486337439));
#48347=CARTESIAN_POINT('Ctrl Pts',(21.2859861874224,19.3508672100184,39.5404415593539));
#48348=CARTESIAN_POINT('Ctrl Pts',(21.2218887321146,19.3457106441534,39.5952003657285));
#48349=CARTESIAN_POINT('Ctrl Pts',(21.068282226226,19.3341543407665,39.7099290911365));
#48350=CARTESIAN_POINT('Ctrl Pts',(20.9769295745816,19.3278182468496,39.7669455683943));
#48351=CARTESIAN_POINT('Ctrl Pts',(20.8108627474162,19.3165078459909,39.8522313143818));
#48352=CARTESIAN_POINT('Ctrl Pts',(20.7382700510883,19.3116279718792,39.8840314227108));
#48353=CARTESIAN_POINT('Ctrl Pts',(20.6458981760785,19.3053745840151,39.9178908445439));
#48354=CARTESIAN_POINT('Ctrl Pts',(20.6277646190432,19.3041451975773,39.9242321993967));
#48355=CARTESIAN_POINT('Ctrl Pts',(20.6013715413927,19.3023519680904,39.9330218078398));
#48356=CARTESIAN_POINT('Ctrl Pts',(20.5931851812922,19.3017952280787,39.9356873414509));
#48357=CARTESIAN_POINT('Ctrl Pts',(20.5788388433847,19.3008185091516,39.9402526189426));
#48358=CARTESIAN_POINT('Ctrl Pts',(20.5726866306861,19.3003993222265,39.9421764653505));
#48359=CARTESIAN_POINT('Ctrl Pts',(20.5607466989577,19.2995850840942,39.9458445860728));
#48360=CARTESIAN_POINT('Ctrl Pts',(20.5549601892242,19.2991901588316,39.9475925642055));
#48361=CARTESIAN_POINT('Ctrl Pts',(20.5411430862195,19.2982463505971,39.951695642823));
#48362=CARTESIAN_POINT('Ctrl Pts',(20.5331052493393,19.2976966651614,39.9540257233425));
#48363=CARTESIAN_POINT('Ctrl Pts',(20.5042138946991,19.2957184017191,39.9621975993413));
#48364=CARTESIAN_POINT('Ctrl Pts',(20.4832781574332,19.2942802661506,39.9677402679551));
#48365=CARTESIAN_POINT('Ctrl Pts',(20.3125840944265,19.2825130422236,40.0098689605594));
#48366=CARTESIAN_POINT('Ctrl Pts',(20.1590536403926,19.2716021474951,40.0287280325526));
#48367=CARTESIAN_POINT('Ctrl Pts',(19.9244406995905,19.2548612125593,40.0293303338055));
#48368=CARTESIAN_POINT('Ctrl Pts',(19.8439897192502,19.2491228451965,40.0244966058679));
#48369=CARTESIAN_POINT('Ctrl Pts',(19.7289161547196,19.2410911133007,40.010316936358));
#48370=CARTESIAN_POINT('Ctrl Pts',(19.6938835775469,19.2386704205275,40.0050171587509));
#48371=CARTESIAN_POINT('Ctrl Pts',(19.651736395961,19.2358030840346,39.9974482059737));
#48372=CARTESIAN_POINT('Ctrl Pts',(19.6444659718951,19.2353100979693,39.9960993622347));
#48373=CARTESIAN_POINT('Ctrl Pts',(19.6331421769379,19.2345449997506,39.9939310949199));
#48374=CARTESIAN_POINT('Ctrl Pts',(19.6290834773675,19.2342713206704,39.993140403848));
#48375=CARTESIAN_POINT('Ctrl Pts',(19.6215347350776,19.2337633693316,39.9916445958848));
#48376=CARTESIAN_POINT('Ctrl Pts',(19.618044135358,19.2335289165715,39.990942873721));
#48377=CARTESIAN_POINT('Ctrl Pts',(19.6101024412371,19.2329964541702,39.9893234513936));
#48378=CARTESIAN_POINT('Ctrl Pts',(19.6056526410239,19.2326987912737,39.9883996854022));
#48379=CARTESIAN_POINT('Ctrl Pts',(19.5940861156019,19.2319267381675,39.9859558405408));
#48380=CARTESIAN_POINT('Ctrl Pts',(19.5869745731398,19.2314537003442,39.984411185184));
#48381=CARTESIAN_POINT('Ctrl Pts',(19.5408534729607,19.2283955848688,39.9741198616671));
#48382=CARTESIAN_POINT('Ctrl Pts',(19.502111895418,19.2258719484957,39.9642019090557));
#48383=CARTESIAN_POINT('Ctrl Pts',(19.4473033568271,19.2223301999119,39.9483399223784));
#48384=CARTESIAN_POINT('Ctrl Pts',(19.4309665588301,19.221278189424,39.9433759844735));
#48385=CARTESIAN_POINT('Ctrl Pts',(19.2923859472791,19.2123692471506,39.8992503289609));
#48386=CARTESIAN_POINT('Ctrl Pts',(19.1742620739815,19.2048545266816,39.8481932884131));
#48387=CARTESIAN_POINT('Ctrl Pts',(18.9866830634279,19.19189445825,39.7438296160297));
#48388=CARTESIAN_POINT('Ctrl Pts',(18.9141934864965,19.1865982271348,39.6968746206688));
#48389=CARTESIAN_POINT('Ctrl Pts',(18.8289971432027,19.1798438790131,39.6331988625736));
#48390=CARTESIAN_POINT('Ctrl Pts',(18.8130890398742,19.1785585489264,39.6209170809926));
#48391=CARTESIAN_POINT('Ctrl Pts',(18.7905211566732,19.1766985450429,39.6029239324556));
#48392=CARTESIAN_POINT('Ctrl Pts',(18.783703569337,19.1761317469183,39.5974119031835));
#48393=CARTESIAN_POINT('Ctrl Pts',(18.7719188923142,19.1751432978828,39.5877503945955));
#48394=CARTESIAN_POINT('Ctrl Pts',(18.7669346347629,19.1747224969671,39.583622002745));
#48395=CARTESIAN_POINT('Ctrl Pts',(18.7573671819744,19.1739093965603,39.5756158978629));
#48396=CARTESIAN_POINT('Ctrl Pts',(18.7527811220519,19.1735172431074,39.5717417122524));
#48397=CARTESIAN_POINT('Ctrl Pts',(18.7419671935788,19.172586791467,39.5625195389416));
#48398=CARTESIAN_POINT('Ctrl Pts',(18.7357552696216,19.1720477425517,39.557153115501));
#48399=CARTESIAN_POINT('Ctrl Pts',(18.7140065591769,19.1701441642938,39.5381208475781));
#48400=CARTESIAN_POINT('Ctrl Pts',(18.6986560307569,19.1687709899912,39.5242452455318));
#48401=CARTESIAN_POINT('Ctrl Pts',(18.5623517787118,19.1563029174824,39.3969940754952));
#48402=CARTESIAN_POINT('Ctrl Pts',(18.456282740426,19.1445218917116,39.2687345441868));
#48403=CARTESIAN_POINT('Ctrl Pts',(18.3348668565016,19.1282825548101,39.076073766007));
#48404=CARTESIAN_POINT('Ctrl Pts',(18.304350245548,19.1238751604866,39.0220418128906));
#48405=CARTESIAN_POINT('Ctrl Pts',(18.2571630108873,19.1165556478289,38.9281982465478));
#48406=CARTESIAN_POINT('Ctrl Pts',(18.2391269934606,19.1136014338433,38.8891261149081));
#48407=CARTESIAN_POINT('Ctrl Pts',(18.2193803784843,19.1101952269226,38.8422918423713));
#48408=CARTESIAN_POINT('Ctrl Pts',(18.2163931226765,19.1096747857568,38.8350849801464));
#48409=CARTESIAN_POINT('Ctrl Pts',(18.2118562782806,19.1088765341861,38.8239491839253));
#48410=CARTESIAN_POINT('Ctrl Pts',(18.2102757777372,19.1085969346908,38.8200330544664));
#48411=CARTESIAN_POINT('Ctrl Pts',(18.2073892744807,19.108083529655,38.8128127148643));
#48412=CARTESIAN_POINT('Ctrl Pts',(18.2060795479295,19.1078495088071,38.8095101068849));
#48413=CARTESIAN_POINT('Ctrl Pts',(18.2031572756354,19.1073249322055,38.8020814797013));
#48414=CARTESIAN_POINT('Ctrl Pts',(18.2015498172477,19.1070346810466,38.7979535237887));
#48415=CARTESIAN_POINT('Ctrl Pts',(18.1974747715305,19.1062944016079,38.7873812441126));
#48416=CARTESIAN_POINT('Ctrl Pts',(18.1950274905477,19.1058455483315,38.7809290841404));
#48417=CARTESIAN_POINT('Ctrl Pts',(18.1808481821289,19.1032186673913,38.7429322767487));
#48418=CARTESIAN_POINT('Ctrl Pts',(18.1699078159981,19.1010839772322,38.7110958829762));
#48419=CARTESIAN_POINT('Ctrl Pts',(18.1171494330601,19.0901038169597,38.5434139665161));
#48420=CARTESIAN_POINT('Ctrl Pts',(18.0896019951648,19.0818077924057,38.4035292550389));
#48421=CARTESIAN_POINT('Ctrl Pts',(18.0731693937776,19.0700277856654,38.2083869054541));
#48422=CARTESIAN_POINT('Ctrl Pts',(18.0708998576667,19.06677159649,38.154735945049));
#48423=CARTESIAN_POINT('Ctrl Pts',(18.0708405336757,19.0601259833274,38.047037329303));
#48424=CARTESIAN_POINT('Ctrl Pts',(18.0730802280306,19.0567388060469,37.9930390220168));
#48425=CARTESIAN_POINT('Ctrl Pts',(18.0786629930108,19.0524510066424,37.9262913183339));
#48426=CARTESIAN_POINT('Ctrl Pts',(18.0798736154291,19.0516172565417,37.9133847419403));
#48427=CARTESIAN_POINT('Ctrl Pts',(18.0819834858798,19.0502987050167,37.893092917687));
#48428=CARTESIAN_POINT('Ctrl Pts',(18.0827955512464,19.0498166249753,37.8856988374519));
#48429=CARTESIAN_POINT('Ctrl Pts',(18.0843063968132,19.0489621934366,37.8726386869787));
#48430=CARTESIAN_POINT('Ctrl Pts',(18.0849876070335,19.0485903956126,37.8669706422672));
#48431=CARTESIAN_POINT('Ctrl Pts',(18.086608664564,19.0477353202312,37.8539699089489));
#48432=CARTESIAN_POINT('Ctrl Pts',(18.0875655183115,19.0472515155099,37.8466394685128));
#48433=CARTESIAN_POINT('Ctrl Pts',(18.0903358956867,19.0459061103242,37.8263260881715));
#48434=CARTESIAN_POINT('Ctrl Pts',(18.0922396282903,19.045041698526,37.8133560551673));
#48435=CARTESIAN_POINT('Ctrl Pts',(18.104103395452,19.0399798686261,37.7378901712751));
#48436=CARTESIAN_POINT('Ctrl Pts',(18.1170005986991,19.0356908817312,37.6759019367349));
#48437=CARTESIAN_POINT('Ctrl Pts',(18.172561706311,19.0204299960564,37.4621586618875));
#48438=CARTESIAN_POINT('Ctrl Pts',(18.2307402348806,19.0090224172787,37.315091480492));
#48439=CARTESIAN_POINT('Ctrl Pts',(18.312548660812,18.9969778469887,37.1649972625554));
#48440=CARTESIAN_POINT('Ctrl Pts',(18.3190845663261,18.9960366179365,37.1532975870443));
#48441=CARTESIAN_POINT('Ctrl Pts',(18.3495360791105,18.9917485655328,37.1000972094078));
#48442=CARTESIAN_POINT('Ctrl Pts',(18.374872494873,18.9884470837344,37.0594240949823));
#48443=CARTESIAN_POINT('Ctrl Pts',(18.4059900989788,18.9847179830776,37.0133842865465));
#48444=CARTESIAN_POINT('Ctrl Pts',(18.4103188832894,18.9842060189076,37.0070611978567));
#48445=CARTESIAN_POINT('Ctrl Pts',(18.4173124014179,18.9833898970632,36.996975168647));
#48446=CARTESIAN_POINT('Ctrl Pts',(18.4199530945883,18.9830842010024,36.9931957756318));
#48447=CARTESIAN_POINT('Ctrl Pts',(18.4246656173793,18.9825430683793,36.9865023920771));
#48448=CARTESIAN_POINT('Ctrl Pts',(18.4267320273631,18.9823072720096,36.9835846530051));
#48449=CARTESIAN_POINT('Ctrl Pts',(18.4311525889381,18.9818060150649,36.9773795362099));
#48450=CARTESIAN_POINT('Ctrl Pts',(18.4335089636096,18.9815407094704,36.9740938144905));
#48451=CARTESIAN_POINT('Ctrl Pts',(18.4399596391441,18.9808194771465,36.9651584647831));
#48452=CARTESIAN_POINT('Ctrl Pts',(18.4440743366094,18.9803649202693,36.9595235332574));
#48453=CARTESIAN_POINT('Ctrl Pts',(18.4656100668299,18.9780134668609,36.9303646087596));
#48454=CARTESIAN_POINT('Ctrl Pts',(18.48353537507,18.9761491388541,36.9072155758794));
#48455=CARTESIAN_POINT('Ctrl Pts',(18.5390689781861,18.9706144781517,36.8387753298248));
#48456=CARTESIAN_POINT('Ctrl Pts',(18.5782316603997,18.9670255381835,36.794786225617));
#48457=CARTESIAN_POINT('Ctrl Pts',(18.6876666813502,18.9575806870015,36.6826459768143));
#48458=CARTESIAN_POINT('Ctrl Pts',(18.7612115035457,18.9518042810597,36.6179356887756));
#48459=CARTESIAN_POINT('Ctrl Pts',(18.9154896320085,18.9401489516138,36.5017301011671));
#48460=CARTESIAN_POINT('Ctrl Pts',(18.9957678457011,18.9342918513032,36.4501080202648));
#48461=CARTESIAN_POINT('Ctrl Pts',(19.0914669957831,18.9273381220598,36.3981495400453));
#48462=CARTESIAN_POINT('Ctrl Pts',(19.1034769382696,18.9264661251862,36.3917922865043));
#48463=CARTESIAN_POINT('Ctrl Pts',(19.1228718226222,18.9250585174983,36.3817868171329));
#48464=CARTESIAN_POINT('Ctrl Pts',(19.1302148555712,18.9245257211837,36.3780580206053));
#48465=CARTESIAN_POINT('Ctrl Pts',(19.1433160567111,18.9235752535755,36.3715104056125));
#48466=CARTESIAN_POINT('Ctrl Pts',(19.1490648589008,18.9231582331296,36.3686730405306));
#48467=CARTESIAN_POINT('Ctrl Pts',(19.1610966907538,18.9222854787511,36.3628090401666));
#48468=CARTESIAN_POINT('Ctrl Pts',(19.1673821932796,18.9218295688681,36.3597877201389));
#48469=CARTESIAN_POINT('Ctrl Pts',(19.1838104083296,18.9206379537884,36.3520003729702));
#48470=CARTESIAN_POINT('Ctrl Pts',(19.1939783953937,18.9199004031342,36.3472885834794));
#48471=CARTESIAN_POINT('Ctrl Pts',(19.23912257793,18.9166252632111,36.326844924855));
#48472=CARTESIAN_POINT('Ctrl Pts',(19.2745201939101,18.9140555587858,36.3120704521873));
#48473=CARTESIAN_POINT('Ctrl Pts',(19.3380287010232,18.9094386430806,36.2877593874139));
#48474=CARTESIAN_POINT('Ctrl Pts',(19.3659600201675,18.9074060049298,36.2777995081405));
#48475=CARTESIAN_POINT('Ctrl Pts',(19.3941040358239,18.9053562004634,36.268488974236));
#48476=CARTESIAN_POINT('',(18.0708707698807,18.8910431656481,38.0982765153061));
#48477=CARTESIAN_POINT('Ctrl Pts',(19.3941040087494,18.7329718898071,36.2684889831927));
#48478=CARTESIAN_POINT('Ctrl Pts',(19.3298530882588,18.7374296531232,36.2897443154305));
#48479=CARTESIAN_POINT('Ctrl Pts',(19.2665971548675,18.7418874164393,36.3144260076521));
#48480=CARTESIAN_POINT('Ctrl Pts',(19.2047269033099,18.7463451797554,36.3424211942047));
#48481=CARTESIAN_POINT('Ctrl Pts',(19.1403324023001,18.7509848157215,36.3715585586625));
#48482=CARTESIAN_POINT('Ctrl Pts',(19.0774396255052,18.7556244516877,36.4042855416477));
#48483=CARTESIAN_POINT('Ctrl Pts',(19.0164715912724,18.7602640876538,36.4404173940036));
#48484=CARTESIAN_POINT('Ctrl Pts',(18.9580479481332,18.7647100967698,36.4750413485818));
#48485=CARTESIAN_POINT('Ctrl Pts',(18.9013920663298,18.7691561058858,36.5127913535199));
#48486=CARTESIAN_POINT('Ctrl Pts',(18.8468535916639,18.7736021150017,36.5534567843602));
#48487=CARTESIAN_POINT('Ctrl Pts',(18.7923468103982,18.7780455404527,36.594098583704));
#48488=CARTESIAN_POINT('Ctrl Pts',(18.7399553898737,18.7824889659038,36.6376521538038));
#48489=CARTESIAN_POINT('Ctrl Pts',(18.6899997011006,18.7869323913548,36.6838637869952));
#48490=CARTESIAN_POINT('Ctrl Pts',(18.6400558261219,18.7913747660002,36.730064491807));
#48491=CARTESIAN_POINT('Ctrl Pts',(18.5925469010025,18.7958171406457,36.7789216767792));
#48492=CARTESIAN_POINT('Ctrl Pts',(18.5477585210014,18.8002595152912,36.830142825521));
#48493=CARTESIAN_POINT('Ctrl Pts',(18.5029652977025,18.8047023703234,36.8813695131832));
#48494=CARTESIAN_POINT('Ctrl Pts',(18.4608935259458,18.8091452253556,36.9349602989744));
#48495=CARTESIAN_POINT('Ctrl Pts',(18.421789162117,18.8135880803878,36.9905888462394));
#48496=CARTESIAN_POINT('Ctrl Pts',(18.3826421080963,18.81803578568,37.0462781231293));
#48497=CARTESIAN_POINT('Ctrl Pts',(18.3464692088349,18.8224834909722,37.104009195492));
#48498=CARTESIAN_POINT('Ctrl Pts',(18.3134730224323,18.8269311962645,37.1634268256903));
#48499=CARTESIAN_POINT('Ctrl Pts',(18.2804555392723,18.831381772243,37.2228828058617));
#48500=CARTESIAN_POINT('Ctrl Pts',(18.2506190645463,18.8358323482216,37.2840270667302));
#48501=CARTESIAN_POINT('Ctrl Pts',(18.2241188731087,18.8402829242001,37.3464823956593));
#48502=CARTESIAN_POINT('Ctrl Pts',(18.1975743674798,18.8447409425278,37.4090421637356));
#48503=CARTESIAN_POINT('Ctrl Pts',(18.1743774426708,18.8491989608554,37.4729169108286));
#48504=CARTESIAN_POINT('Ctrl Pts',(18.1546338850032,18.853656979183,37.5377131883803));
#48505=CARTESIAN_POINT('Ctrl Pts',(18.148670593706,18.8550034671029,37.5572840825687));
#48506=CARTESIAN_POINT('Ctrl Pts',(18.1430219876732,18.8563499550229,37.5769389731496));
#48507=CARTESIAN_POINT('Ctrl Pts',(18.1376900600936,18.8576964429428,37.5966668651619));
#48508=CARTESIAN_POINT('Ctrl Pts',(18.1153926025753,18.8633272878381,37.6791664541953));
#48509=CARTESIAN_POINT('Ctrl Pts',(18.0985664791579,18.8689581327334,37.7632031113543));
#48510=CARTESIAN_POINT('Ctrl Pts',(18.0873818825785,18.8745889776287,37.848137946862));
#48511=CARTESIAN_POINT('Ctrl Pts',(18.0764875166079,18.8800737069685,37.9308687968393));
#48512=CARTESIAN_POINT('Ctrl Pts',(18.0709456587466,18.8855584363083,38.0144519820069));
#48513=CARTESIAN_POINT('Ctrl Pts',(18.0708707698807,18.8910431656481,38.0982765153061));
#48514=CARTESIAN_POINT('Ctrl Pts',(18.0708707514445,18.8906962854919,38.098297276432));
#48515=CARTESIAN_POINT('Ctrl Pts',(18.0707906498881,18.8961279122774,38.1890496793503));
#48516=CARTESIAN_POINT('Ctrl Pts',(18.0771143768436,18.9016047975629,38.2796889011574));
#48517=CARTESIAN_POINT('Ctrl Pts',(18.0945784531256,18.9094020141416,38.4034535409684));
#48518=CARTESIAN_POINT('Ctrl Pts',(18.1002652032124,18.9115621796977,38.4372281166426));
#48519=CARTESIAN_POINT('Ctrl Pts',(18.1088383024623,18.9144118889741,38.4809950696164));
#48520=CARTESIAN_POINT('Ctrl Pts',(18.1109108385906,18.9150761028551,38.4911418449372));
#48521=CARTESIAN_POINT('Ctrl Pts',(18.1145443264148,18.9162007928593,38.5082279306263));
#48522=CARTESIAN_POINT('Ctrl Pts',(18.1160621540314,18.9166599095217,38.5151762646294));
#48523=CARTESIAN_POINT('Ctrl Pts',(18.1191379160774,18.9175697357968,38.5288923010251));
#48524=CARTESIAN_POINT('Ctrl Pts',(18.1206940418777,18.9180203820005,38.5356603014891));
#48525=CARTESIAN_POINT('Ctrl Pts',(18.1237590521184,18.9188898985739,38.5486687884058));
#48526=CARTESIAN_POINT('Ctrl Pts',(18.1252626150435,18.9193085939407,38.5549104439087));
#48527=CARTESIAN_POINT('Ctrl Pts',(18.1287809599841,18.9202707709,38.5692022211786));
#48528=CARTESIAN_POINT('Ctrl Pts',(18.1308165731257,18.9208149127047,38.5772470357692));
#48529=CARTESIAN_POINT('Ctrl Pts',(18.1363761821166,18.9222686196259,38.5986374881804));
#48530=CARTESIAN_POINT('Ctrl Pts',(18.1399915614944,18.9231810979369,38.6119586615496));
#48531=CARTESIAN_POINT('Ctrl Pts',(18.1727572078703,18.9311771051349,38.7277558081209));
#48532=CARTESIAN_POINT('Ctrl Pts',(18.2102023315209,18.9385317273811,38.8276750477035));
#48533=CARTESIAN_POINT('Ctrl Pts',(18.2848351165201,18.950874838632,38.9856672731724));
#48534=CARTESIAN_POINT('Ctrl Pts',(18.3172265037518,18.9557511408271,39.0457641994098));
#48535=CARTESIAN_POINT('Ctrl Pts',(18.3891686105606,18.9656080080847,39.1637980136889));
#48536=CARTESIAN_POINT('Ctrl Pts',(18.4288351832321,18.9705808123152,39.2215553381599));
#48537=CARTESIAN_POINT('Ctrl Pts',(18.4931045497217,18.9778773835261,39.3050128380167));
#48538=CARTESIAN_POINT('Ctrl Pts',(18.5154186923663,18.9802908761362,39.3323995156586));
#48539=CARTESIAN_POINT('Ctrl Pts',(18.5433164774905,18.9831530124948,39.3647808967306));
#48540=CARTESIAN_POINT('Ctrl Pts',(18.5481915395274,18.98364767971,39.3703738819675));
#48541=CARTESIAN_POINT('Ctrl Pts',(18.5558373109765,18.9844148110008,39.3790441068246));
#48542=CARTESIAN_POINT('Ctrl Pts',(18.5585858005894,18.9846888552475,39.3821407122887));
#48543=CARTESIAN_POINT('Ctrl Pts',(18.5637159031975,18.9851971311477,39.3878832332648));
#48544=CARTESIAN_POINT('Ctrl Pts',(18.5660948480465,18.9854315454793,39.3905313807794));
#48545=CARTESIAN_POINT('Ctrl Pts',(18.5715224320732,18.9859634687333,39.3965396169135));
#48546=CARTESIAN_POINT('Ctrl Pts',(18.5745755979911,18.9862606337284,39.3998955402232));
#48547=CARTESIAN_POINT('Ctrl Pts',(18.5839393811803,18.9871658682378,39.4101151910373));
#48548=CARTESIAN_POINT('Ctrl Pts',(18.5902880581646,18.9877711603867,39.4169440912465));
#48549=CARTESIAN_POINT('Ctrl Pts',(18.6516553300898,18.9935446270373,39.4820009736538));
#48550=CARTESIAN_POINT('Ctrl Pts',(18.7102086178773,18.99846379317,39.5368025678053));
#48551=CARTESIAN_POINT('Ctrl Pts',(18.8988367481208,19.0132325226787,39.6924903988199));
#48552=CARTESIAN_POINT('Ctrl Pts',(19.0385214428604,19.0228200872732,39.7805191474336));
#48553=CARTESIAN_POINT('Ctrl Pts',(19.2114467774253,19.0347173185124,39.8607989697987));
#48554=CARTESIAN_POINT('Ctrl Pts',(19.2354356793378,19.0363665234294,39.871347085743));
#48555=CARTESIAN_POINT('Ctrl Pts',(19.2774226156965,19.0392559826455,39.8887972754145));
#48556=CARTESIAN_POINT('Ctrl Pts',(19.2953233188535,19.0404887606648,39.8959244141232));
#48557=CARTESIAN_POINT('Ctrl Pts',(19.3213625452887,19.0422846203926,39.9058426550988));
#48558=CARTESIAN_POINT('Ctrl Pts',(19.329418087354,19.0428405443534,39.9088494642769));
#48559=CARTESIAN_POINT('Ctrl Pts',(19.3435727206139,19.043818113442,39.9140252710871));
#48560=CARTESIAN_POINT('Ctrl Pts',(19.349663173035,19.0442389796953,39.9162176265688));
#48561=CARTESIAN_POINT('Ctrl Pts',(19.3614218152065,19.0450520413457,39.920383608365));
#48562=CARTESIAN_POINT('Ctrl Pts',(19.3670884163065,19.0454440899248,39.9223615188978));
#48563=CARTESIAN_POINT('Ctrl Pts',(19.3805212896988,19.046374034607,39.9269800140273));
#48564=CARTESIAN_POINT('Ctrl Pts',(19.3882953066201,19.0469126794931,39.9295975537703));
#48565=CARTESIAN_POINT('Ctrl Pts',(19.4157035295922,19.0488134915824,39.9386317917897));
#48566=CARTESIAN_POINT('Ctrl Pts',(19.4354232952824,19.0501842709797,39.9447824585889));
#48567=CARTESIAN_POINT('Ctrl Pts',(19.6159199254433,19.0627643895206,39.9979149630277));
#48568=CARTESIAN_POINT('Ctrl Pts',(19.7820487445648,19.0746758760273,40.0240770974184));
#48569=CARTESIAN_POINT('Ctrl Pts',(20.0207665283856,19.0917017002924,40.0303380376165));
#48570=CARTESIAN_POINT('Ctrl Pts',(20.0921656977009,19.096768124827,40.0282487097215));
#48571=CARTESIAN_POINT('Ctrl Pts',(20.1956632830447,19.1039485014327,40.0194567164022));
#48572=CARTESIAN_POINT('Ctrl Pts',(20.2279652136805,19.1061657258914,40.0158889251795));
#48573=CARTESIAN_POINT('Ctrl Pts',(20.2676182481678,19.1088460980912,40.0104919858527));
#48574=CARTESIAN_POINT('Ctrl Pts',(20.2750668288834,19.109347777236,40.0094337901562));
#48575=CARTESIAN_POINT('Ctrl Pts',(20.2866272773809,19.1101233854474,40.0077223831495));
#48576=CARTESIAN_POINT('Ctrl Pts',(20.2907434412172,19.1103989504252,40.0070994047271));
#48577=CARTESIAN_POINT('Ctrl Pts',(20.2983732193016,19.1109085976733,40.0059193671554));
#48578=CARTESIAN_POINT('Ctrl Pts',(20.3018872794348,19.1111428716309,40.0053659183884));
#48579=CARTESIAN_POINT('Ctrl Pts',(20.3098488707188,19.1116726359383,40.0040894245128));
#48580=CARTESIAN_POINT('Ctrl Pts',(20.314295403677,19.1119677937435,40.0033605174724));
#48581=CARTESIAN_POINT('Ctrl Pts',(20.3277806210479,19.1128608757421,40.0011013805808));
#48582=CARTESIAN_POINT('Ctrl Pts',(20.3368111500519,19.11345613021,39.9995222694242));
#48583=CARTESIAN_POINT('Ctrl Pts',(20.4534515621832,19.1211122342419,39.9782681261434));
#48584=CARTESIAN_POINT('Ctrl Pts',(20.5592274462939,19.1277044941696,39.9495355010542));
#48585=CARTESIAN_POINT('Ctrl Pts',(20.7404239761828,19.1392471380287,39.883335193607));
#48586=CARTESIAN_POINT('Ctrl Pts',(20.8168949191811,19.1442035541571,39.849626913998));
#48587=CARTESIAN_POINT('Ctrl Pts',(20.9605196114213,19.1540177554338,39.7748428487155));
#48588=CARTESIAN_POINT('Ctrl Pts',(21.0278173895146,19.1588540783821,39.7344068545603));
#48589=CARTESIAN_POINT('Ctrl Pts',(21.1082167820642,19.1650551008631,39.6791654447412));
#48590=CARTESIAN_POINT('Ctrl Pts',(21.1238091029239,19.1662784964438,39.6681074569081));
#48591=CARTESIAN_POINT('Ctrl Pts',(21.1461680883278,19.1680645594553,39.6517458222036));
#48592=CARTESIAN_POINT('Ctrl Pts',(21.1530680057146,19.1686202042484,39.6466255376471));
#48593=CARTESIAN_POINT('Ctrl Pts',(21.1650818638899,19.1695956518826,39.6375852247139));
#48594=CARTESIAN_POINT('Ctrl Pts',(21.1702108364198,19.170014669007,39.633685322833));
#48595=CARTESIAN_POINT('Ctrl Pts',(21.1801173168731,19.1708290567045,39.6260741373759));
#48596=CARTESIAN_POINT('Ctrl Pts',(21.1848970997114,19.1712243035831,39.6223659271176));
#48597=CARTESIAN_POINT('Ctrl Pts',(21.1962617935754,19.1721696505606,39.6134631223066));
#48598=CARTESIAN_POINT('Ctrl Pts',(21.2028303807807,19.1727205591319,39.6082479811598));
#48599=CARTESIAN_POINT('Ctrl Pts',(21.2263271732758,19.1747077205613,39.5893415439728));
#48600=CARTESIAN_POINT('Ctrl Pts',(21.2430567944686,19.1761536435346,39.5754071677336));
#48601=CARTESIAN_POINT('Ctrl Pts',(21.3749712492519,19.1878113260224,39.4616970897988));
#48602=CARTESIAN_POINT('Ctrl Pts',(21.4781786390825,19.1985899540993,39.3488935199546));
#48603=CARTESIAN_POINT('Ctrl Pts',(21.6147140008288,19.2152943951347,39.1587383294762));
#48604=CARTESIAN_POINT('Ctrl Pts',(21.6581355057822,19.2211250727037,39.0893515415398));
#48605=CARTESIAN_POINT('Ctrl Pts',(21.7140198620851,19.2292676491691,38.9859772138713));
#48606=CARTESIAN_POINT('Ctrl Pts',(21.7301395638964,19.2317104257583,38.9540709578044));
#48607=CARTESIAN_POINT('Ctrl Pts',(21.7485223977939,19.2346002939951,38.9150257287601));
#48608=CARTESIAN_POINT('Ctrl Pts',(21.7516415512461,19.2350945639704,38.9083003120531));
#48609=CARTESIAN_POINT('Ctrl Pts',(21.7564417174681,19.235861214793,38.8977920669434));
#48610=CARTESIAN_POINT('Ctrl Pts',(21.7581494143675,19.2361351726784,38.894021615889));
#48611=CARTESIAN_POINT('Ctrl Pts',(21.7613032844763,19.2366433714789,38.8869980752235));
#48612=CARTESIAN_POINT('Ctrl Pts',(21.7627525747353,19.2368777945587,38.8837465093373));
#48613=CARTESIAN_POINT('Ctrl Pts',(21.7660291691425,19.2374098439672,38.8763402156537));
#48614=CARTESIAN_POINT('Ctrl Pts',(21.7678508142366,19.2377071257072,38.872183045881));
#48615=CARTESIAN_POINT('Ctrl Pts',(21.7733733963565,19.2386130699385,38.8594580026542));
#48616=CARTESIAN_POINT('Ctrl Pts',(21.7770269116391,19.2392189487111,38.8508695122983));
#48617=CARTESIAN_POINT('Ctrl Pts',(21.8118139471688,19.2450554854268,38.7674177964319));
#48618=CARTESIAN_POINT('Ctrl Pts',(21.8382652102286,19.2500310076296,38.6906782584562));
#48619=CARTESIAN_POINT('Ctrl Pts',(21.9033471766848,19.2648175440783,38.4544988936035));
#48620=CARTESIAN_POINT('Ctrl Pts',(21.9265731119114,19.2743765017034,38.2916121687378));
#48621=CARTESIAN_POINT('Ctrl Pts',(21.9294953394293,19.2870574120657,38.0884795069982));
#48622=CARTESIAN_POINT('Ctrl Pts',(21.9288609128268,19.289540385216,38.0492040682617));
#48623=CARTESIAN_POINT('Ctrl Pts',(21.9265011223943,19.29278568671,37.998690281669));
#48624=CARTESIAN_POINT('Ctrl Pts',(21.9258746890966,19.293513827801,37.9874082299503));
#48625=CARTESIAN_POINT('Ctrl Pts',(21.924700084137,19.2946976858565,37.9691525112911));
#48626=CARTESIAN_POINT('Ctrl Pts',(21.9242130250149,19.2951514979984,37.9621750697146));
#48627=CARTESIAN_POINT('Ctrl Pts',(21.9232072916015,19.2960231432618,37.948813715414));
#48628=CARTESIAN_POINT('Ctrl Pts',(21.922694747192,19.2964407798532,37.942429423489));
#48629=CARTESIAN_POINT('Ctrl Pts',(21.9214540792651,19.2973949606404,37.9278840173042));
#48630=CARTESIAN_POINT('Ctrl Pts',(21.9207057394289,19.2979321281679,37.9197247957701));
#48631=CARTESIAN_POINT('Ctrl Pts',(21.9185921225952,19.2993551342344,37.8981891622268));
#48632=CARTESIAN_POINT('Ctrl Pts',(21.9171389541849,19.3002436944753,37.8848220225304));
#48633=CARTESIAN_POINT('Ctrl Pts',(21.9049485371264,19.30707784857,37.7826408870221));
#48634=CARTESIAN_POINT('Ctrl Pts',(21.8881863972404,19.3132116524389,37.6946684533206));
#48635=CARTESIAN_POINT('Ctrl Pts',(21.8240870167428,19.330847364444,37.4515476346088));
#48636=CARTESIAN_POINT('Ctrl Pts',(21.7632278327173,19.3426465971593,37.3007452078152));
#48637=CARTESIAN_POINT('Ctrl Pts',(21.6695501463812,19.3558927494013,37.1330187138656));
#48638=CARTESIAN_POINT('Ctrl Pts',(21.6542418935626,19.3579445363137,37.1070576523065));
#48639=CARTESIAN_POINT('Ctrl Pts',(21.6346130505554,19.3604320959398,37.0754843528617));
#48640=CARTESIAN_POINT('Ctrl Pts',(21.6308626449337,19.360901279858,37.0695247827274));
#48641=CARTESIAN_POINT('Ctrl Pts',(21.6248997907977,19.3616375432812,37.0601636236867));
#48642=CARTESIAN_POINT('Ctrl Pts',(21.6227091432955,19.3619060072656,37.0567483253507));
#48643=CARTESIAN_POINT('Ctrl Pts',(21.6185694220651,19.362409500905,37.0503389376814));
#48644=CARTESIAN_POINT('Ctrl Pts',(21.6166228294264,19.3626446795766,37.0473433858009));
#48645=CARTESIAN_POINT('Ctrl Pts',(21.6121577868753,19.363180567156,37.0405138660463));
#48646=CARTESIAN_POINT('Ctrl Pts',(21.6096339779518,19.3634809164968,37.0366834639127));
#48647=CARTESIAN_POINT('Ctrl Pts',(21.6029018196531,19.3642754490069,37.0265449171148));
#48648=CARTESIAN_POINT('Ctrl Pts',(21.5986698467693,19.3647681089002,37.0202524443057));
#48649=CARTESIAN_POINT('Ctrl Pts',(21.5684907184055,19.3682349692436,36.975945851198));
#48650=CARTESIAN_POINT('Ctrl Pts',(21.5412251838817,19.3711275117729,36.9388425691465));
#48651=CARTESIAN_POINT('Ctrl Pts',(21.4281852725925,19.3823720202558,36.7960235515076));
#48652=CARTESIAN_POINT('Ctrl Pts',(21.3326523810961,19.3903226700516,36.6985326085782));
#48653=CARTESIAN_POINT('Ctrl Pts',(21.1772583148209,19.4024726781103,36.570335873975));
#48654=CARTESIAN_POINT('Ctrl Pts',(21.1247953903617,19.406459354497,36.5313560835936));
#48655=CARTESIAN_POINT('Ctrl Pts',(21.0385666749033,19.4129340534054,36.4738414877088));
#48656=CARTESIAN_POINT('Ctrl Pts',(21.0060485440344,19.4153589954491,36.4535255069986));
#48657=CARTESIAN_POINT('Ctrl Pts',(20.963272794036,19.4185385476312,36.4285414643524));
#48658=CARTESIAN_POINT('Ctrl Pts',(20.9535482498931,19.4192606893972,36.4229747054285));
#48659=CARTESIAN_POINT('Ctrl Pts',(20.9376938149794,19.4204371813263,36.4140814083175));
#48660=CARTESIAN_POINT('Ctrl Pts',(20.93159331664,19.4208896707444,36.4107027855618));
#48661=CARTESIAN_POINT('Ctrl Pts',(20.919849620341,19.4217604072261,36.4042817646799));
#48662=CARTESIAN_POINT('Ctrl Pts',(20.9142093028479,19.422178466675,36.4012342696634));
#48663=CARTESIAN_POINT('Ctrl Pts',(20.9012883686087,19.42313589576,36.3943360035748));
#48664=CARTESIAN_POINT('Ctrl Pts',(20.8939981112202,19.4236759037267,36.3905036514571));
#48665=CARTESIAN_POINT('Ctrl Pts',(20.8746134024453,19.4251113871404,36.3804713827115));
#48666=CARTESIAN_POINT('Ctrl Pts',(20.8624777674202,19.4260096613587,36.3743524826535));
#48667=CARTESIAN_POINT('Ctrl Pts',(20.7646150946882,19.4332515272699,36.3262993834132));
#48668=CARTESIAN_POINT('Ctrl Pts',(20.6759619835534,19.4398104457271,36.2906574498809));
#48669=CARTESIAN_POINT('Ctrl Pts',(20.4915627983093,19.4534201399859,36.2319707448975));
#48670=CARTESIAN_POINT('Ctrl Pts',(20.3959467059997,19.4604600938781,36.2093937787486));
#48671=CARTESIAN_POINT('Ctrl Pts',(20.241168989698,19.4715951044553,36.1851081024778));
#48672=CARTESIAN_POINT('Ctrl Pts',(20.1829151524675,19.4757259341796,36.1786680388432));
#48673=CARTESIAN_POINT('Ctrl Pts',(20.0953347120372,19.4817717569566,36.1730061311067));
#48674=CARTESIAN_POINT('Ctrl Pts',(20.0661736991428,19.4837574347634,36.1717844136512));
#48675=CARTESIAN_POINT('Ctrl Pts',(20.0300253983929,19.4861762050208,36.1710910814191));
#48676=CARTESIAN_POINT('Ctrl Pts',(20.0230556645701,19.4866405999431,36.1709951838509));
#48677=CARTESIAN_POINT('Ctrl Pts',(20.0120438484697,19.4873710530011,36.1709033621507));
#48678=CARTESIAN_POINT('Ctrl Pts',(20.0080021209366,19.4876384600408,36.1708823625154));
#48679=CARTESIAN_POINT('Ctrl Pts',(20.0003846181427,19.4881410983609,36.1708667245096));
#48680=CARTESIAN_POINT('Ctrl Pts',(19.9968089663945,19.4883764721597,36.1708693252981));
#48681=CARTESIAN_POINT('Ctrl Pts',(19.9886202559793,19.4889142423174,36.1708980487425));
#48682=CARTESIAN_POINT('Ctrl Pts',(19.9840072711198,19.4892162698322,36.1709307760915));
#48683=CARTESIAN_POINT('Ctrl Pts',(19.9717234068829,19.4900181986092,36.1710619911814));
#48684=CARTESIAN_POINT('Ctrl Pts',(19.9640528272603,19.4905165310908,36.1711896897076));
#48685=CARTESIAN_POINT('Ctrl Pts',(19.9082870676032,19.4941231277532,36.172450856004));
#48686=CARTESIAN_POINT('Ctrl Pts',(19.8602438938308,19.4971421006209,36.175337411719));
#48687=CARTESIAN_POINT('Ctrl Pts',(19.7959945716255,19.5011204470937,36.18161668354));
#48688=CARTESIAN_POINT('Ctrl Pts',(19.7796553017627,19.5021270191859,36.1834246686603));
#48689=CARTESIAN_POINT('Ctrl Pts',(19.6497183711775,19.5101041366138,36.1994862134574));
#48690=CARTESIAN_POINT('Ctrl Pts',(19.5375685047347,19.5168343289807,36.2236180944196));
#48691=CARTESIAN_POINT('Ctrl Pts',(19.4168111704594,19.5244522547812,36.261093811437));
#48692=CARTESIAN_POINT('Ctrl Pts',(19.4054396628868,19.5251732142282,36.2647389497829));
#48693=CARTESIAN_POINT('Ctrl Pts',(19.3941040005193,19.5258959448669,36.2684889859154));
#48694=CARTESIAN_POINT('Origin',(20.,-1.3495818343519,38.1));
#48695=CARTESIAN_POINT('',(19.3941040087494,20.489691467393,36.2684889831927));
#48696=CARTESIAN_POINT('',(19.3941039696621,20.3190989370965,36.2684889961235));
#48697=CARTESIAN_POINT('',(19.3941040087494,-1.3495818343519,36.2684889831927));
#48698=CARTESIAN_POINT('',(18.0708701870214,19.8542362730884,38.1008494569394));
#48699=CARTESIAN_POINT('Ctrl Pts',(19.3941040087494,20.489691467393,36.2684889831927));
#48700=CARTESIAN_POINT('Ctrl Pts',(19.4003737701409,20.4892600094623,36.2664148360768));
#48701=CARTESIAN_POINT('Ctrl Pts',(19.4066542566161,20.4888303778034,36.2643728589592));
#48702=CARTESIAN_POINT('Ctrl Pts',(19.448459657195,20.4859868203442,36.2510176304672));
#48703=CARTESIAN_POINT('Ctrl Pts',(19.4842984026903,20.4836268337685,36.240703127972));
#48704=CARTESIAN_POINT('Ctrl Pts',(19.6764534995626,20.4712729270058,36.191384880702));
#48705=CARTESIAN_POINT('Ctrl Pts',(19.8369044177153,20.4619517070475,36.1710354838721));
#48706=CARTESIAN_POINT('Ctrl Pts',(20.0807375178535,20.4471561321505,36.1707865775156));
#48707=CARTESIAN_POINT('Ctrl Pts',(20.1633544411664,20.4420432668475,36.1760208621107));
#48708=CARTESIAN_POINT('Ctrl Pts',(20.2585168863516,20.4359139170974,36.1882240844466));
#48709=CARTESIAN_POINT('Ctrl Pts',(20.2716417480344,20.4350633368021,36.1900447967326));
#48710=CARTESIAN_POINT('Ctrl Pts',(20.2928798372764,20.4336780389967,36.1932143325977));
#48711=CARTESIAN_POINT('Ctrl Pts',(20.3010051703234,20.4331459238618,36.1944801065095));
#48712=CARTESIAN_POINT('Ctrl Pts',(20.3154295486177,20.4321974117733,36.1968217136535));
#48713=CARTESIAN_POINT('Ctrl Pts',(20.3217318467426,20.431781667431,36.1978769737692));
#48714=CARTESIAN_POINT('Ctrl Pts',(20.3349736125639,20.4309053149536,36.2001618744381));
#48715=CARTESIAN_POINT('Ctrl Pts',(20.3419118044627,20.4304444995495,36.2013982670901));
#48716=CARTESIAN_POINT('Ctrl Pts',(20.3601945091911,20.4292258058689,36.2047597288448));
#48717=CARTESIAN_POINT('Ctrl Pts',(20.3715268561706,20.4284659235933,36.206948612631));
#48718=CARTESIAN_POINT('Ctrl Pts',(20.4238094756681,20.4249388651305,36.2175347252619));
#48719=CARTESIAN_POINT('Ctrl Pts',(20.4644968816419,20.4221331606981,36.2271593311256));
#48720=CARTESIAN_POINT('Ctrl Pts',(20.6664597507865,20.40788773265,36.2819196234114));
#48721=CARTESIAN_POINT('Ctrl Pts',(20.8216704057554,20.395823118403,36.3465963751211));
#48722=CARTESIAN_POINT('Ctrl Pts',(20.9742527073621,20.3833267818593,36.4349313818391));
#48723=CARTESIAN_POINT('Ctrl Pts',(20.9819277349018,20.3826966256383,36.4394459457519));
#48724=CARTESIAN_POINT('Ctrl Pts',(21.0077735404067,20.3805697593032,36.4548906776616));
#48725=CARTESIAN_POINT('Ctrl Pts',(21.0257957161072,20.3790786018366,36.4660675079296));
#48726=CARTESIAN_POINT('Ctrl Pts',(21.0822395945951,20.3743900623568,36.5023744307044));
#48727=CARTESIAN_POINT('Ctrl Pts',(21.1199537210303,20.3712296218914,36.5285820268466));
#48728=CARTESIAN_POINT('Ctrl Pts',(21.1627629848999,20.3676406247315,36.5606552716684));
#48729=CARTESIAN_POINT('Ctrl Pts',(21.1687993348274,20.3671345249312,36.5652335450576));
#48730=CARTESIAN_POINT('Ctrl Pts',(21.1784451768992,20.366325955649,36.5726393545231));
#48731=CARTESIAN_POINT('Ctrl Pts',(21.1820717582957,20.3660219911553,36.5754443481381));
#48732=CARTESIAN_POINT('Ctrl Pts',(21.1885060175996,20.3654828150865,36.5804577129283));
#48733=CARTESIAN_POINT('Ctrl Pts',(21.1913175983449,20.3652472530296,36.5826609816062));
#48734=CARTESIAN_POINT('Ctrl Pts',(21.1973107455981,20.3647452329412,36.5873843819638));
#48735=CARTESIAN_POINT('Ctrl Pts',(21.2004904782079,20.3644789363776,36.5899067439605));
#48736=CARTESIAN_POINT('Ctrl Pts',(21.2091688514344,20.3637522186699,36.5968357049795));
#48737=CARTESIAN_POINT('Ctrl Pts',(21.2146514138149,20.3632932026094,36.6012624793627));
#48738=CARTESIAN_POINT('Ctrl Pts',(21.243502961599,20.3608773869767,36.6248203375419));
#48739=CARTESIAN_POINT('Ctrl Pts',(21.2664460462865,20.3589553133393,36.6444694059582));
#48740=CARTESIAN_POINT('Ctrl Pts',(21.4093897776415,20.3469033168646,36.7728304710716));
#48741=CARTESIAN_POINT('Ctrl Pts',(21.5157737961787,20.3375327060044,36.8957572323788));
#48742=CARTESIAN_POINT('Ctrl Pts',(21.6551366525536,20.3223255683894,37.1049802836952));
#48743=CARTESIAN_POINT('Ctrl Pts',(21.6994757243467,20.3168144994628,37.1827646391397));
#48744=CARTESIAN_POINT('Ctrl Pts',(21.7440884481492,20.3102445025727,37.2754523481984));
#48745=CARTESIAN_POINT('Ctrl Pts',(21.7497929198497,20.3093815509407,37.2876281220833));
#48746=CARTESIAN_POINT('Ctrl Pts',(21.7587680157842,20.3079857314959,37.307317995174));
#48747=CARTESIAN_POINT('Ctrl Pts',(21.762118918262,20.307455601923,37.3147951804669));
#48748=CARTESIAN_POINT('Ctrl Pts',(21.7680042324441,20.3065081625159,37.3281550558815));
#48749=CARTESIAN_POINT('Ctrl Pts',(21.7705571863148,20.3060914886762,37.334029483568));
#48750=CARTESIAN_POINT('Ctrl Pts',(21.7758368708076,20.3052176860876,37.3463456392927));
#48751=CARTESIAN_POINT('Ctrl Pts',(21.7785579099802,20.3047603725557,37.3527896910399));
#48752=CARTESIAN_POINT('Ctrl Pts',(21.7855830949605,20.303561128059,37.3696827575806));
#48753=CARTESIAN_POINT('Ctrl Pts',(21.789830527572,20.3028173079436,37.3801549215465));
#48754=CARTESIAN_POINT('Ctrl Pts',(21.8084299061664,20.2994739109204,37.4271946880162));
#48755=CARTESIAN_POINT('Ctrl Pts',(21.8217540209026,20.2968405480562,37.4641559785782));
#48756=CARTESIAN_POINT('Ctrl Pts',(21.8847996115625,20.2830336747431,37.657340703669));
#48757=CARTESIAN_POINT('Ctrl Pts',(21.9155796983059,20.2712546804561,37.8190137207699));
#48758=CARTESIAN_POINT('Ctrl Pts',(21.930484721245,20.2538623153076,38.0634575314035));
#48759=CARTESIAN_POINT('Ctrl Pts',(21.9303169727918,20.2481754728189,38.1445670231513));
#48760=CARTESIAN_POINT('Ctrl Pts',(21.9244409134107,20.2421017467532,38.234747273721));
#48761=CARTESIAN_POINT('Ctrl Pts',(21.9237664989189,20.2414778086436,38.2440559725197));
#48762=CARTESIAN_POINT('Ctrl Pts',(21.9226637112822,20.2405557773619,38.257884172203));
#48763=CARTESIAN_POINT('Ctrl Pts',(21.9222869117001,20.2402549444014,38.2624074772468));
#48764=CARTESIAN_POINT('Ctrl Pts',(21.9215860834899,20.2397197359984,38.2704762601647));
#48765=CARTESIAN_POINT('Ctrl Pts',(21.921268202413,20.239485025263,38.2740222016194));
#48766=CARTESIAN_POINT('Ctrl Pts',(21.9205594917211,20.2389786191623,38.2816891020133));
#48767=CARTESIAN_POINT('Ctrl Pts',(21.9201652154525,20.2387071178283,38.28580968003));
#48768=CARTESIAN_POINT('Ctrl Pts',(21.9190277193192,20.2379513364583,38.2973072231957));
#48769=CARTESIAN_POINT('Ctrl Pts',(21.9182552203285,20.2374686551939,38.3046813178255));
#48770=CARTESIAN_POINT('Ctrl Pts',(21.9135104383686,20.2346712922682,38.3475853321041));
#48771=CARTESIAN_POINT('Ctrl Pts',(21.9085933188767,20.2324056576276,38.3830064169601));
#48772=CARTESIAN_POINT('Ctrl Pts',(21.889195558839,20.2250727663824,38.4989697712635));
#48773=CARTESIAN_POINT('Ctrl Pts',(21.8705757360531,20.2201617540855,38.5787331131643));
#48774=CARTESIAN_POINT('Ctrl Pts',(21.8029641689762,20.2061641918161,38.8028933201032));
#48775=CARTESIAN_POINT('Ctrl Pts',(21.7418774490001,20.1971304880754,38.9429682626295));
#48776=CARTESIAN_POINT('Ctrl Pts',(21.6539641619233,20.1861016074642,39.0931863013645));
#48777=CARTESIAN_POINT('Ctrl Pts',(21.6426514600384,20.184711567242,39.1117868342778));
#48778=CARTESIAN_POINT('Ctrl Pts',(21.6265480396728,20.1827702336645,39.1372822038935));
#48779=CARTESIAN_POINT('Ctrl Pts',(21.622023180089,20.1822286427838,39.1443436673326));
#48780=CARTESIAN_POINT('Ctrl Pts',(21.6141555000811,20.1812934733463,39.1564474312123));
#48781=CARTESIAN_POINT('Ctrl Pts',(21.6108347155179,20.1809007123259,39.1615039666706));
#48782=CARTESIAN_POINT('Ctrl Pts',(21.6039279490535,20.1800877861318,39.1719138061243));
#48783=CARTESIAN_POINT('Ctrl Pts',(21.6003388248393,20.1796675072494,39.1772649244924));
#48784=CARTESIAN_POINT('Ctrl Pts',(21.5919009893504,20.1786844025845,39.1897098829243));
#48785=CARTESIAN_POINT('Ctrl Pts',(21.587031587146,20.1781208041822,39.1967894630298));
#48786=CARTESIAN_POINT('Ctrl Pts',(21.5711766741923,20.1762975005698,39.2195141190028));
#48787=CARTESIAN_POINT('Ctrl Pts',(21.5600061435348,20.1750308064343,39.2350281017775));
#48788=CARTESIAN_POINT('Ctrl Pts',(21.5018191277852,20.1685200280092,39.3133581990986));
#48789=CARTESIAN_POINT('Ctrl Pts',(21.4512381610161,20.1631385692436,39.3734220790766));
#48790=CARTESIAN_POINT('Ctrl Pts',(21.3396191206589,20.1518076081176,39.490655754728));
#48791=CARTESIAN_POINT('Ctrl Pts',(21.2782352683836,20.1458550071135,39.5472787744822));
#48792=CARTESIAN_POINT('Ctrl Pts',(21.1282938938944,20.1320944440345,39.6685901398657));
#48793=CARTESIAN_POINT('Ctrl Pts',(21.0374888772426,20.1243075787417,39.7300750890072));
#48794=CARTESIAN_POINT('Ctrl Pts',(20.9339500509643,20.1163360914232,39.7880058845919));
#48795=CARTESIAN_POINT('Ctrl Pts',(20.9259193923395,20.1157234634645,39.7924242527095));
#48796=CARTESIAN_POINT('Ctrl Pts',(20.9138945509943,20.1148148777526,39.7989289583606));
#48797=CARTESIAN_POINT('Ctrl Pts',(20.9099241988567,20.1145162924837,39.8010587318643));
#48798=CARTESIAN_POINT('Ctrl Pts',(20.9028057230424,20.1139835257834,39.8048451653439));
#48799=CARTESIAN_POINT('Ctrl Pts',(20.8996604563077,20.1137490214714,39.8065070393645));
#48800=CARTESIAN_POINT('Ctrl Pts',(20.8928242438943,20.1132412762867,39.8100949559024));
#48801=CARTESIAN_POINT('Ctrl Pts',(20.8891316636332,20.1129682389719,39.8120177493889));
#48802=CARTESIAN_POINT('Ctrl Pts',(20.8787481064662,20.1122037974739,39.8173820000232));
#48803=CARTESIAN_POINT('Ctrl Pts',(20.8720430878048,20.1117140520603,39.820796334889));
#48804=CARTESIAN_POINT('Ctrl Pts',(20.8316730017611,20.108787551232,39.8410570624259));
#48805=CARTESIAN_POINT('Ctrl Pts',(20.7975380820846,20.1064052882328,39.856955645222));
#48806=CARTESIAN_POINT('Ctrl Pts',(20.6114211785716,20.0937908323632,39.9370975943917));
#48807=CARTESIAN_POINT('Ctrl Pts',(20.4521296888376,20.084259855219,39.9826451868081));
#48808=CARTESIAN_POINT('Ctrl Pts',(20.2112119950715,20.0694446065732,40.0191449631258));
#48809=CARTESIAN_POINT('Ctrl Pts',(20.1328135344972,20.0645732723176,40.0261584024903));
#48810=CARTESIAN_POINT('Ctrl Pts',(20.0410869297276,20.0587099148586,40.0287371068022));
#48811=CARTESIAN_POINT('Ctrl Pts',(20.0279586103288,20.0578669399302,40.0289720748049));
#48812=CARTESIAN_POINT('Ctrl Pts',(20.0066417668936,20.0564915852999,40.0291359416528));
#48813=CARTESIAN_POINT('Ctrl Pts',(19.9984541510758,20.0559617457923,40.0291467547585));
#48814=CARTESIAN_POINT('Ctrl Pts',(19.9838806731041,20.0550157506369,40.0290732251716));
#48815=CARTESIAN_POINT('Ctrl Pts',(19.9774947933731,20.0546002345826,40.029009293605));
#48816=CARTESIAN_POINT('Ctrl Pts',(19.9640425569834,20.0537227763279,40.0288078107569));
#48817=CARTESIAN_POINT('Ctrl Pts',(19.9569764170965,20.0532606188512,40.028663132231));
#48818=CARTESIAN_POINT('Ctrl Pts',(19.9382845129511,20.0520346979228,40.0281776446066));
#48819=CARTESIAN_POINT('Ctrl Pts',(19.9266609056931,20.0512688880094,40.0277705251759));
#48820=CARTESIAN_POINT('Ctrl Pts',(19.8723227018726,20.0476721196193,40.0253751688434));
#48821=CARTESIAN_POINT('Ctrl Pts',(19.8296810551059,20.0448007543591,40.0220723192203));
#48822=CARTESIAN_POINT('Ctrl Pts',(19.621517706548,20.0305321820696,39.9989676574683));
#48823=CARTESIAN_POINT('Ctrl Pts',(19.4589481812864,20.0185212663477,39.9591858631507));
#48824=CARTESIAN_POINT('Ctrl Pts',(19.2343013014001,20.0014495686247,39.8722196713413));
#48825=CARTESIAN_POINT('Ctrl Pts',(19.166646686512,19.9962550564477,39.8414310083441));
#48826=CARTESIAN_POINT('Ctrl Pts',(19.0927234829816,19.9906402366373,39.8024916717616));
#48827=CARTESIAN_POINT('Ctrl Pts',(19.0845489837594,19.9900202472735,39.7981101307208));
#48828=CARTESIAN_POINT('Ctrl Pts',(19.0724316744723,19.9891029190971,39.7915023064882));
#48829=CARTESIAN_POINT('Ctrl Pts',(19.0684647368697,19.9888028796957,39.7893209008237));
#48830=CARTESIAN_POINT('Ctrl Pts',(19.0616156964443,19.9882853745138,39.7855231751664));
#48831=CARTESIAN_POINT('Ctrl Pts',(19.0587300356605,19.9880675005104,39.783913397426));
#48832=CARTESIAN_POINT('Ctrl Pts',(19.0558353878591,19.9878491161366,39.7822888403319));
#48833=CARTESIAN_POINT('Ctrl Pts',(19.0558223181413,19.9878481301057,39.7822815050415));
#48834=CARTESIAN_POINT('Ctrl Pts',(19.0557964587149,19.9878461791754,39.7822669912174));
#48835=CARTESIAN_POINT('Ctrl Pts',(19.0557836688964,19.9878452142677,39.7822598126307));
#48836=CARTESIAN_POINT('Ctrl Pts',(19.0557583637688,19.9878433051685,39.7822456091527));
#48837=CARTESIAN_POINT('Ctrl Pts',(19.055745848148,19.9878423609534,39.7822385840945));
#48838=CARTESIAN_POINT('Ctrl Pts',(19.055721083711,19.9878404926579,39.782224683373));
#48839=CARTESIAN_POINT('Ctrl Pts',(19.0557088356575,19.9878395686349,39.7822178081456));
#48840=CARTESIAN_POINT('Ctrl Pts',(19.0556846016916,19.9878377403712,39.7822042044908));
#48841=CARTESIAN_POINT('Ctrl Pts',(19.0556726156993,19.9878368361244,39.7821974760261));
#48842=CARTESIAN_POINT('Ctrl Pts',(19.0556488995763,19.9878350469392,39.7821841623941));
#48843=CARTESIAN_POINT('Ctrl Pts',(19.0556371695779,19.9878341620105,39.7821775773081));
#48844=CARTESIAN_POINT('Ctrl Pts',(19.0556149503129,19.9878324857611,39.782165103363));
#48845=CARTESIAN_POINT('Ctrl Pts',(19.0556044603603,19.987831694388,39.7821592141511));
#48846=CARTESIAN_POINT('Ctrl Pts',(19.055583533059,19.9878301156146,39.7821474650024));
#48847=CARTESIAN_POINT('Ctrl Pts',(19.0555730956278,19.987829328208,39.7821416050206));
#48848=CARTESIAN_POINT('Ctrl Pts',(19.0555522720801,19.9878277572705,39.7821299136122));
#48849=CARTESIAN_POINT('Ctrl Pts',(19.0555418865022,19.98782697378,39.7821240824892));
#48850=CARTESIAN_POINT('Ctrl Pts',(19.0555211666731,19.9878254106755,39.7821124488089));
#48851=CARTESIAN_POINT('Ctrl Pts',(19.0555108325336,19.9878246310698,39.7821066463156));
#48852=CARTESIAN_POINT('Ctrl Pts',(19.0554902167756,19.9878230758247,39.782095070569));
#48853=CARTESIAN_POINT('Ctrl Pts',(19.0554799345472,19.9878223001394,39.7820892969745));
#48854=CARTESIAN_POINT('Ctrl Pts',(19.0554594193368,19.9878207524879,39.7820777771905));
#48855=CARTESIAN_POINT('Ctrl Pts',(19.0554491873856,19.9878199805995,39.782072031581));
#48856=CARTESIAN_POINT('Ctrl Pts',(19.0519432002418,19.9875554930758,39.7801032513371));
#48857=CARTESIAN_POINT('Ctrl Pts',(19.0484535323508,19.9872924769294,39.7781293011416));
#48858=CARTESIAN_POINT('Ctrl Pts',(19.0388907116957,19.9865723168476,39.772680617711));
#48859=CARTESIAN_POINT('Ctrl Pts',(19.0328301950448,19.9861165644643,39.7691836582528));
#48860=CARTESIAN_POINT('Ctrl Pts',(19.0193217612953,19.9851018868962,39.7612909253694));
#48861=CARTESIAN_POINT('Ctrl Pts',(19.0118840577534,19.9845440034456,39.756877858411));
#48862=CARTESIAN_POINT('Ctrl Pts',(18.9889695117246,19.9828269030545,39.7430726218083));
#48863=CARTESIAN_POINT('Ctrl Pts',(18.9735945575059,19.9816771439145,39.7335122307388));
#48864=CARTESIAN_POINT('Ctrl Pts',(18.9140856136334,19.977226997675,39.6953366130109));
#48865=CARTESIAN_POINT('Ctrl Pts',(18.8709918687905,19.9740041243062,39.6651359170821));
#48866=CARTESIAN_POINT('Ctrl Pts',(18.7189588231242,19.962428226304,39.5490377515313));
#48867=CARTESIAN_POINT('Ctrl Pts',(18.6181340363325,19.9543162195343,39.4532273600515));
#48868=CARTESIAN_POINT('Ctrl Pts',(18.4863238528572,19.9418282736787,39.2977360580864));
#48869=CARTESIAN_POINT('Ctrl Pts',(18.4467441915504,19.9377662233058,39.2459416007988));
#48870=CARTESIAN_POINT('Ctrl Pts',(18.4027813614186,19.9328005428525,39.1819388202106));
#48871=CARTESIAN_POINT('Ctrl Pts',(18.3958004422882,19.9319970485034,39.1715608976178));
#48872=CARTESIAN_POINT('Ctrl Pts',(18.384521403601,19.9306735365962,39.1544360768183));
#48873=CARTESIAN_POINT('Ctrl Pts',(18.3801633899499,19.9301557493874,39.147728919658));
#48874=CARTESIAN_POINT('Ctrl Pts',(18.3724121512867,19.9292230926605,39.135635493439));
#48875=CARTESIAN_POINT('Ctrl Pts',(18.3690036191451,19.9288087951847,39.1302591346693));
#48876=CARTESIAN_POINT('Ctrl Pts',(18.3618081080542,19.9279252062136,39.1187842824862));
#48877=CARTESIAN_POINT('Ctrl Pts',(18.3580284432119,19.9274556550819,39.1126813385448));
#48878=CARTESIAN_POINT('Ctrl Pts',(18.347952775824,19.9261891543135,39.0962076674093));
#48879=CARTESIAN_POINT('Ctrl Pts',(18.3417204808408,19.9253899101199,39.0857985455884));
#48880=CARTESIAN_POINT('Ctrl Pts',(18.3109722631222,19.9213653498243,39.0333264016633));
#48881=CARTESIAN_POINT('Ctrl Pts',(18.2879586301262,19.9180869924393,38.9904080509311));
#48882=CARTESIAN_POINT('Ctrl Pts',(18.1937215998474,19.9033946155962,38.7974741855524));
#48883=CARTESIAN_POINT('Ctrl Pts',(18.1404230227594,19.8914011227261,38.6395083032005));
#48884=CARTESIAN_POINT('Ctrl Pts',(18.101595012653,19.8773424045315,38.4444994512527));
#48885=CARTESIAN_POINT('Ctrl Pts',(18.0960045662866,19.8750354701613,38.4121264920453));
#48886=CARTESIAN_POINT('Ctrl Pts',(18.0874485233809,19.870937757559,38.3537218757529));
#48887=CARTESIAN_POINT('Ctrl Pts',(18.0841812655951,19.8691376835596,38.3277425383711));
#48888=CARTESIAN_POINT('Ctrl Pts',(18.0798398901284,19.8663202441359,38.2864483784812));
#48889=CARTESIAN_POINT('Ctrl Pts',(18.0784180241057,19.8652875669206,38.2711741556486));
#48890=CARTESIAN_POINT('Ctrl Pts',(18.0767161523157,19.8638827102765,38.2501816528894));
#48891=CARTESIAN_POINT('Ctrl Pts',(18.0762792202875,19.8635024160761,38.2444771656254));
#48892=CARTESIAN_POINT('Ctrl Pts',(18.0756237848887,19.862898973685,38.2353891940913));
#48893=CARTESIAN_POINT('Ctrl Pts',(18.0753888167711,19.8626749270359,38.2320069884387));
#48894=CARTESIAN_POINT('Ctrl Pts',(18.0749368562799,19.8622279809938,38.2252434810152));
#48895=CARTESIAN_POINT('Ctrl Pts',(18.0747198550971,19.8620050866324,38.2218622200099));
#48896=CARTESIAN_POINT('Ctrl Pts',(18.0742918900555,19.8615476980728,38.2149071306376));
#48897=CARTESIAN_POINT('Ctrl Pts',(18.0740819632888,19.8613132609208,38.2113332374332));
#48898=CARTESIAN_POINT('Ctrl Pts',(18.0736138254768,19.8607657116984,38.2029655762043));
#48899=CARTESIAN_POINT('Ctrl Pts',(18.07336355577,19.860453029011,38.1981713615322));
#48900=CARTESIAN_POINT('Ctrl Pts',(18.0725608731067,19.8593761387495,38.1816075671736));
#48901=CARTESIAN_POINT('Ctrl Pts',(18.072098377572,19.8586166108388,38.1698336116703));
#48902=CARTESIAN_POINT('Ctrl Pts',(18.0711698321106,19.856640967472,38.1389930577971));
#48903=CARTESIAN_POINT('Ctrl Pts',(18.070878585341,19.8554331419902,38.1199221704454));
#48904=CARTESIAN_POINT('Ctrl Pts',(18.0708701870214,19.8542362730884,38.1008494569394));
#48905=CARTESIAN_POINT('Ctrl Pts',(18.0708701880617,19.854236421143,38.1008518162642));
#48906=CARTESIAN_POINT('Ctrl Pts',(18.0708091100297,19.8455561160718,37.9625268542006));
#48907=CARTESIAN_POINT('Ctrl Pts',(18.0856255279444,19.8374582510131,37.8245739329577));
#48908=CARTESIAN_POINT('Ctrl Pts',(18.1392321285082,19.8223474198742,37.5785004745513));
#48909=CARTESIAN_POINT('Ctrl Pts',(18.1731169954809,19.81543300587,37.4699905304631));
#48910=CARTESIAN_POINT('Ctrl Pts',(18.221990390201,19.8072380567716,37.351371453203));
#48911=CARTESIAN_POINT('Ctrl Pts',(18.2278029484105,19.8062848414889,37.3377136599847));
#48912=CARTESIAN_POINT('Ctrl Pts',(18.2368941054824,19.8048250838618,37.3170182590075));
#48913=CARTESIAN_POINT('Ctrl Pts',(18.2400586284611,19.8043224026619,37.3099309094431));
#48914=CARTESIAN_POINT('Ctrl Pts',(18.2458887641138,19.8034059624922,37.2970824306239));
#48915=CARTESIAN_POINT('Ctrl Pts',(18.2485402184746,19.8029926909948,37.2913149666476));
#48916=CARTESIAN_POINT('Ctrl Pts',(18.2543217979133,19.8020989806512,37.2789006458326));
#48917=CARTESIAN_POINT('Ctrl Pts',(18.2574615171412,19.8016182177089,37.272258393035));
#48918=CARTESIAN_POINT('Ctrl Pts',(18.2660729604281,19.8003117563123,37.2543065425659));
#48919=CARTESIAN_POINT('Ctrl Pts',(18.2716172731191,19.7994835666037,37.2430323580796));
#48920=CARTESIAN_POINT('Ctrl Pts',(18.2992494156332,19.7954173258601,37.1882023421582));
#48921=CARTESIAN_POINT('Ctrl Pts',(18.3228738648243,19.7921261874945,37.1454452756538));
#48922=CARTESIAN_POINT('Ctrl Pts',(18.362825455119,19.7868291677138,37.0792082988996));
#48923=CARTESIAN_POINT('Ctrl Pts',(18.3780970858714,19.7848587384307,37.055113882836));
#48924=CARTESIAN_POINT('Ctrl Pts',(18.4811127871359,19.7719141658629,36.9002861888563));
#48925=CARTESIAN_POINT('Ctrl Pts',(18.5840357248168,19.7604827095395,36.7803905230257));
#48926=CARTESIAN_POINT('Ctrl Pts',(18.7245931820472,19.7471767133356,36.652258960152));
#48927=CARTESIAN_POINT('Ctrl Pts',(18.7493737309762,19.7449067313305,36.6307992433851));
#48928=CARTESIAN_POINT('Ctrl Pts',(18.7848481676727,19.7417745606744,36.6016270374404));
#48929=CARTESIAN_POINT('Ctrl Pts',(18.7950913406793,19.740883366401,36.593377733195));
#48930=CARTESIAN_POINT('Ctrl Pts',(18.8108271566163,19.7395352653638,36.5809680863722));
#48931=CARTESIAN_POINT('Ctrl Pts',(18.8162588305159,19.7390736745732,36.576731522965));
#48932=CARTESIAN_POINT('Ctrl Pts',(18.8252127795837,19.7383190380686,36.569824494193));
#48933=CARTESIAN_POINT('Ctrl Pts',(18.8287216918494,19.7380248766503,36.5671369214369));
#48934=CARTESIAN_POINT('Ctrl Pts',(18.835507601989,19.7374590636384,36.5619763117143));
#48935=CARTESIAN_POINT('Ctrl Pts',(18.8387833144664,19.7371873014419,36.5595016323373));
#48936=CARTESIAN_POINT('Ctrl Pts',(18.8420791353039,19.7369152622612,36.5570282477525));
#48937=CARTESIAN_POINT('Ctrl Pts',(18.8420913312268,19.7369142556209,36.5570190954155));
#48938=CARTESIAN_POINT('Ctrl Pts',(18.8421158820842,19.7369122292541,36.5570006718676));
#48939=CARTESIAN_POINT('Ctrl Pts',(18.8421282370558,19.736911209525,36.5569914006348));
#48940=CARTESIAN_POINT('Ctrl Pts',(18.8421531089581,19.7369091567387,36.556972737101));
#48941=CARTESIAN_POINT('Ctrl Pts',(18.8421656259683,19.7369081236756,36.5569633447467));
#48942=CARTESIAN_POINT('Ctrl Pts',(18.8421908252211,19.7369060439525,36.5569444365321));
#48943=CARTESIAN_POINT('Ctrl Pts',(18.8422035072118,19.736904997314,36.5569349208673));
#48944=CARTESIAN_POINT('Ctrl Pts',(18.8422290394414,19.7369028901931,36.5569157637882));
#48945=CARTESIAN_POINT('Ctrl Pts',(18.8422418897859,19.7369018297025,36.5569061223012));
#48946=CARTESIAN_POINT('Ctrl Pts',(18.8422677614208,19.7368996946565,36.5568867115732));
#48947=CARTESIAN_POINT('Ctrl Pts',(18.8422807834257,19.7368986200426,36.5568769418029));
#48948=CARTESIAN_POINT('Ctrl Pts',(18.8423070023105,19.7368964564275,36.5568572715809));
#48949=CARTESIAN_POINT('Ctrl Pts',(18.8423201986639,19.7368953674703,36.5568473715311));
#48950=CARTESIAN_POINT('Ctrl Pts',(18.8423467697354,19.7368931748822,36.556827438153));
#48951=CARTESIAN_POINT('Ctrl Pts',(18.8423601443966,19.7368920712567,36.5568174048746));
#48952=CARTESIAN_POINT('Ctrl Pts',(18.8423870753308,19.7368898490659,36.556797202625));
#48953=CARTESIAN_POINT('Ctrl Pts',(18.8424006316561,19.736888730497,36.5567870336221));
#48954=CARTESIAN_POINT('Ctrl Pts',(18.8424279292402,19.7368864781472,36.5567665574541));
#48955=CARTESIAN_POINT('Ctrl Pts',(18.8424416708629,19.736885344337,36.5567562500238));
#48956=CARTESIAN_POINT('Ctrl Pts',(18.8424693430418,19.7368830611766,36.556735494024));
#48957=CARTESIAN_POINT('Ctrl Pts',(18.842483273294,19.7368819118521,36.5567250456905));
#48958=CARTESIAN_POINT('Ctrl Pts',(18.842511326397,19.7368795973629,36.556704005159));
#48959=CARTESIAN_POINT('Ctrl Pts',(18.8425254494117,19.7368784321852,36.5566934128463));
#48960=CARTESIAN_POINT('Ctrl Pts',(18.8425538919978,19.7368760856652,36.5566720814127));
#48961=CARTESIAN_POINT('Ctrl Pts',(18.8425682113416,19.7368749043422,36.556661342471));
#48962=CARTESIAN_POINT('Ctrl Pts',(18.8425970504491,19.736872525215,36.5566397149077));
#48963=CARTESIAN_POINT('Ctrl Pts',(18.8426115703182,19.7368713274027,36.5566288262158));
#48964=CARTESIAN_POINT('Ctrl Pts',(18.8453866452453,19.7366424035945,36.5545478124496));
#48965=CARTESIAN_POINT('Ctrl Pts',(18.8481527114923,19.7364152045513,36.5524851253677));
#48966=CARTESIAN_POINT('Ctrl Pts',(18.8545696927986,19.7358903763614,36.5477266465612));
#48967=CARTESIAN_POINT('Ctrl Pts',(18.8582245929671,19.7355931248567,36.5450363112323));
#48968=CARTESIAN_POINT('Ctrl Pts',(18.869422791922,19.734687365083,36.5368541997474));
#48969=CARTESIAN_POINT('Ctrl Pts',(18.876996605687,19.7340816388856,36.531404130722));
#48970=CARTESIAN_POINT('Ctrl Pts',(18.9507572628083,19.728245639569,36.4791345080919));
#48971=CARTESIAN_POINT('Ctrl Pts',(19.0198030212804,19.7232704718756,36.4364698257077));
#48972=CARTESIAN_POINT('Ctrl Pts',(19.1884639327844,19.7117301072578,36.3464108328363));
#48973=CARTESIAN_POINT('Ctrl Pts',(19.2897609130543,19.7052518514458,36.3030075020567));
#48974=CARTESIAN_POINT('Ctrl Pts',(19.3941041453486,19.6985952145508,36.2684889380033));
#48975=CARTESIAN_POINT('Ctrl Pts',(19.3941040005193,19.5258959448669,36.2684889859154));
#48976=CARTESIAN_POINT('Ctrl Pts',(19.3415821206899,19.5292445953932,36.2858641458948));
#48977=CARTESIAN_POINT('Ctrl Pts',(19.2898298048738,19.5326322553754,36.3054911807356));
#48978=CARTESIAN_POINT('Ctrl Pts',(19.2030432776394,19.5385283134163,36.3427484989325));
#48979=CARTESIAN_POINT('Ctrl Pts',(19.1675765517045,19.5410017085718,36.3592691986031));
#48980=CARTESIAN_POINT('Ctrl Pts',(19.1225592024759,19.5442361646493,36.3819291247166));
#48981=CARTESIAN_POINT('Ctrl Pts',(19.1125249506485,19.5449633252282,36.3870908040291));
#48982=CARTESIAN_POINT('Ctrl Pts',(19.0963482812722,19.5461459791928,36.395592477484));
#48983=CARTESIAN_POINT('Ctrl Pts',(19.0901776263136,19.5465995749868,36.3988784059397));
#48984=CARTESIAN_POINT('Ctrl Pts',(19.0783873460837,19.547471069662,36.405239336154));
#48985=CARTESIAN_POINT('Ctrl Pts',(19.072764899316,19.5478887734634,36.4083089354191));
#48986=CARTESIAN_POINT('Ctrl Pts',(19.0599800054246,19.548843476423,36.4153717879625));
#48987=CARTESIAN_POINT('Ctrl Pts',(19.0528275613209,19.5493811013265,36.4193828006046));
#48988=CARTESIAN_POINT('Ctrl Pts',(19.033995280774,19.5508061143219,36.4301021416205));
#48989=CARTESIAN_POINT('Ctrl Pts',(19.0223599220834,19.5516962364436,36.4368873046387));
#48990=CARTESIAN_POINT('Ctrl Pts',(18.9346299025045,19.5584828628202,36.4892858555637));
#48991=CARTESIAN_POINT('Ctrl Pts',(18.8617032176302,19.564564300891,36.5399712077307));
#48992=CARTESIAN_POINT('Ctrl Pts',(18.6674534305352,19.5820293040815,36.6958692655711));
#48993=CARTESIAN_POINT('Ctrl Pts',(18.5553910253139,19.5937053146319,36.8114485461492));
#48994=CARTESIAN_POINT('Ctrl Pts',(18.4395692318108,19.6070058566656,36.9652605107531));
#48995=CARTESIAN_POINT('Ctrl Pts',(18.4208584871502,19.6091999753845,36.9914467660389));
#48996=CARTESIAN_POINT('Ctrl Pts',(18.3987803971043,19.6118348490982,37.0240399752427));
#48997=CARTESIAN_POINT('Ctrl Pts',(18.3947836363795,19.6123137718489,37.0300118591568));
#48998=CARTESIAN_POINT('Ctrl Pts',(18.3885648676515,19.6130618423814,37.0394170974552));
#48999=CARTESIAN_POINT('Ctrl Pts',(18.3863202999148,19.6133324481579,37.042835346201));
#49000=CARTESIAN_POINT('Ctrl Pts',(18.3821382779975,19.6138377269317,37.0492484937209));
#49001=CARTESIAN_POINT('Ctrl Pts',(18.3801982817636,19.6140725619882,37.0522415959099));
#49002=CARTESIAN_POINT('Ctrl Pts',(18.3757683865344,19.6146098364044,37.0591179217868));
#49003=CARTESIAN_POINT('Ctrl Pts',(18.3732841087053,19.6149119041044,37.0630047034698));
#49004=CARTESIAN_POINT('Ctrl Pts',(18.3667952438504,19.6157030217426,37.0732375691009));
#49005=CARTESIAN_POINT('Ctrl Pts',(18.3628136534178,19.6161906073289,37.0795982477356));
#49006=CARTESIAN_POINT('Ctrl Pts',(18.3354870599342,19.6195532597479,37.1238247995337));
#49007=CARTESIAN_POINT('Ctrl Pts',(18.3134186791527,19.6223520812968,37.1624683940899));
#49008=CARTESIAN_POINT('Ctrl Pts',(18.2330347889182,19.6330253904887,37.3152692855635));
#49009=CARTESIAN_POINT('Ctrl Pts',(18.184812631099,19.6405369101579,37.4343663126572));
#49010=CARTESIAN_POINT('Ctrl Pts',(18.1215139347474,19.6540652691665,37.6503183865293));
#49011=CARTESIAN_POINT('Ctrl Pts',(18.1013118793282,19.6599757960112,37.7451712908246));
#49012=CARTESIAN_POINT('Ctrl Pts',(18.0854535891291,19.6674709217803,37.8622815225971));
#49013=CARTESIAN_POINT('Ctrl Pts',(18.0829409932539,19.6688346858568,37.8834757729418));
#49014=CARTESIAN_POINT('Ctrl Pts',(18.0798714525872,19.6707878959632,37.913641282179));
#49015=CARTESIAN_POINT('Ctrl Pts',(18.0790247131448,19.67136831644,37.9225819819815));
#49016=CARTESIAN_POINT('Ctrl Pts',(18.0776719661654,19.6723728088424,37.9380127757344));
#49017=CARTESIAN_POINT('Ctrl Pts',(18.0771363197066,19.6727959510853,37.9445001743605));
#49018=CARTESIAN_POINT('Ctrl Pts',(18.0761735484981,19.6736081609936,37.9569272801874));
#49019=CARTESIAN_POINT('Ctrl Pts',(18.0757410718514,19.6739970569009,37.9628665075173));
#49020=CARTESIAN_POINT('Ctrl Pts',(18.0746874911003,19.6750110646436,37.9783231088647));
#49021=CARTESIAN_POINT('Ctrl Pts',(18.074109462834,19.6756375087594,37.9878431629173));
#49022=CARTESIAN_POINT('Ctrl Pts',(18.0723734082309,19.6777884155946,38.0204285011433));
#49023=CARTESIAN_POINT('Ctrl Pts',(18.0715590161227,19.6793234654075,38.0435093447891));
#49024=CARTESIAN_POINT('Ctrl Pts',(18.071058997622,19.6812590414813,38.0723839147349));
#49025=CARTESIAN_POINT('Ctrl Pts',(18.070984842271,19.6816476510426,38.0781697719728));
#49026=CARTESIAN_POINT('Ctrl Pts',(18.0708898030658,19.6824166638025,38.0895967615056));
#49027=CARTESIAN_POINT('Ctrl Pts',(18.0708676302825,19.6827970246205,38.0952378284071));
#49028=CARTESIAN_POINT('Ctrl Pts',(18.0708935746107,19.686644300265,38.152186426451));
#49029=CARTESIAN_POINT('Ctrl Pts',(18.0729637986998,19.6901702229334,38.2034684945277));
#49030=CARTESIAN_POINT('Ctrl Pts',(18.0884522498189,19.7036367555213,38.3961104757965));
#49031=CARTESIAN_POINT('Ctrl Pts',(18.115415396985,19.7139011109103,38.535925591211));
#49032=CARTESIAN_POINT('Ctrl Pts',(18.161471180383,19.7248559260875,38.6844118298183));
#49033=CARTESIAN_POINT('Ctrl Pts',(18.1656128373047,19.7258057191734,38.6972848213081));
#49034=CARTESIAN_POINT('Ctrl Pts',(18.185042950921,19.7301034287197,38.7555678423087));
#49035=CARTESIAN_POINT('Ctrl Pts',(18.2018860133886,19.7334060511824,38.8004464683576));
#49036=CARTESIAN_POINT('Ctrl Pts',(18.2233426233009,19.7371362810372,38.8517245833627));
#49037=CARTESIAN_POINT('Ctrl Pts',(18.2263428677531,19.737648289919,38.8587764265059));
#49038=CARTESIAN_POINT('Ctrl Pts',(18.2312154145351,19.7384644687757,38.8700421451077));
#49039=CARTESIAN_POINT('Ctrl Pts',(18.2330609028965,19.738770177474,38.8742674235953));
#49040=CARTESIAN_POINT('Ctrl Pts',(18.2363643522775,19.7393113239191,38.8817574061843));
#49041=CARTESIAN_POINT('Ctrl Pts',(18.2378162608873,19.739547121543,38.8850247196504));
#49042=CARTESIAN_POINT('Ctrl Pts',(18.2409294047999,19.7400483717136,38.8919782478189));
#49043=CARTESIAN_POINT('Ctrl Pts',(18.2425931447712,19.7403136693292,38.8956632766784));
#49044=CARTESIAN_POINT('Ctrl Pts',(18.2471592623024,19.7410348582048,38.9056926077548));
#49045=CARTESIAN_POINT('Ctrl Pts',(18.2500845247922,19.7414893798912,38.9120265163091));
#49046=CARTESIAN_POINT('Ctrl Pts',(18.2654584674742,19.7438403373042,38.9448459440278));
#49047=CARTESIAN_POINT('Ctrl Pts',(18.2784750561068,19.7457042208986,38.9710631953126));
#49048=CARTESIAN_POINT('Ctrl Pts',(18.319441590841,19.7512370663827,39.0490668617792));
#49049=CARTESIAN_POINT('Ctrl Pts',(18.3491702436532,19.7548246984331,39.0998833324394));
#49050=CARTESIAN_POINT('Ctrl Pts',(18.4344010093902,19.7642704127695,39.2313787042275));
#49051=CARTESIAN_POINT('Ctrl Pts',(18.4937949076322,19.7700488225071,39.309324021222));
#49052=CARTESIAN_POINT('Ctrl Pts',(18.622213014459,19.781706017784,39.4536364447325));
#49053=CARTESIAN_POINT('Ctrl Pts',(18.6907615680156,19.7875628712116,39.5200421428112));
#49054=CARTESIAN_POINT('Ctrl Pts',(18.774362896092,19.7945163249079,39.5898123688211));
#49055=CARTESIAN_POINT('Ctrl Pts',(18.7848870767143,19.7953883147591,39.598408413382));
#49056=CARTESIAN_POINT('Ctrl Pts',(18.8019339523593,19.7967959128715,39.6120344328661));
#49057=CARTESIAN_POINT('Ctrl Pts',(18.8083997034176,19.7973287066942,39.6171351655042));
#49058=CARTESIAN_POINT('Ctrl Pts',(18.8199563959602,19.7982791709333,39.6261326118605));
#49059=CARTESIAN_POINT('Ctrl Pts',(18.8250345054307,19.7986961905141,39.6300456664229));
#49060=CARTESIAN_POINT('Ctrl Pts',(18.835677278457,19.799568944179,39.6381624729912));
#49061=CARTESIAN_POINT('Ctrl Pts',(18.8412454124866,19.800024854218,39.6423615001005));
#49062=CARTESIAN_POINT('Ctrl Pts',(18.8558202165034,19.801216472131,39.6532291426539));
#49063=CARTESIAN_POINT('Ctrl Pts',(18.8648623394408,19.8019540254815,39.6598495533795));
#49064=CARTESIAN_POINT('Ctrl Pts',(18.9051018102497,19.8052292014499,39.6887766880532));
#49065=CARTESIAN_POINT('Ctrl Pts',(18.9369007395075,19.8077989400824,39.7102276291891));
#49066=CARTESIAN_POINT('Ctrl Pts',(19.0245657006077,19.8148399622077,39.765635747505));
#49067=CARTESIAN_POINT('Ctrl Pts',(19.0815490398656,19.8193724898872,39.7977222544556));
#49068=CARTESIAN_POINT('Ctrl Pts',(19.2617839279286,19.8335409247069,39.8874772958144));
#49069=CARTESIAN_POINT('Ctrl Pts',(19.3895845625096,19.8433853497653,39.9350556206581));
#49070=CARTESIAN_POINT('Ctrl Pts',(19.5659714343517,19.8561071876829,39.9802356389194));
#49071=CARTESIAN_POINT('Ctrl Pts',(19.6110199764226,19.8592805851452,39.9900693603643));
#49072=CARTESIAN_POINT('Ctrl Pts',(19.6638448671375,19.8628825252023,39.9996314934443));
#49073=CARTESIAN_POINT('Ctrl Pts',(19.6713163084197,19.8633892156679,40.0009384839476));
#49074=CARTESIAN_POINT('Ctrl Pts',(19.6833189167202,19.8641985625954,40.0029652371825));
#49075=CARTESIAN_POINT('Ctrl Pts',(19.6878451888825,19.8645027181646,40.0037129451171));
#49076=CARTESIAN_POINT('Ctrl Pts',(19.6959009548881,19.865042120699,40.0050141969574));
#49077=CARTESIAN_POINT('Ctrl Pts',(19.6994293656359,19.8652777191444,40.0055740905056));
#49078=CARTESIAN_POINT('Ctrl Pts',(19.706968132521,19.865779676766,40.0067488932045));
#49079=CARTESIAN_POINT('Ctrl Pts',(19.7109788724427,19.8660458751868,40.0073609531684));
#49080=CARTESIAN_POINT('Ctrl Pts',(19.721954165511,19.8667720685376,40.0090004270416));
#49081=CARTESIAN_POINT('Ctrl Pts',(19.7289225441078,19.8672306616814,40.010002390879));
#49082=CARTESIAN_POINT('Ctrl Pts',(19.765725932666,19.8696403904388,40.0150887749485));
#49083=CARTESIAN_POINT('Ctrl Pts',(19.7956499520157,19.8715570059891,40.018512615742));
#49084=CARTESIAN_POINT('Ctrl Pts',(19.9869626806524,19.8836089350197,40.0358746570323));
#49085=CARTESIAN_POINT('Ctrl Pts',(20.1494994290245,19.8929832748013,40.0301406576609));
#49086=CARTESIAN_POINT('Ctrl Pts',(20.3977273971722,19.9081959553671,39.9898040293313));
#49087=CARTESIAN_POINT('Ctrl Pts',(20.4849169449891,19.9137085849372,39.9693311039662));
#49088=CARTESIAN_POINT('Ctrl Pts',(20.5832092666239,19.9202802811138,39.9389100845173));
#49089=CARTESIAN_POINT('Ctrl Pts',(20.5960118125928,19.9211432375117,39.9348006028424));
#49090=CARTESIAN_POINT('Ctrl Pts',(20.6165449315399,19.9225390460061,39.9279721107334));
#49091=CARTESIAN_POINT('Ctrl Pts',(20.624303111645,19.923069159575,39.9253370405521));
#49092=CARTESIAN_POINT('Ctrl Pts',(20.6380955101542,19.9240165587032,39.920554228504));
#49093=CARTESIAN_POINT('Ctrl Pts',(20.6441362981052,19.9244332082163,39.9184256946104));
#49094=CARTESIAN_POINT('Ctrl Pts',(20.6567515355234,19.9253069475784,39.9139098377531));
#49095=CARTESIAN_POINT('Ctrl Pts',(20.6633238139053,19.9257642221371,39.9115167663185));
#49096=CARTESIAN_POINT('Ctrl Pts',(20.6804791100472,19.9269633364443,39.9051643729277));
#49097=CARTESIAN_POINT('Ctrl Pts',(20.6910404864623,19.9277070649088,39.9011477644518));
#49098=CARTESIAN_POINT('Ctrl Pts',(20.7381502318148,19.9310497413131,39.8827560705485));
#49099=CARTESIAN_POINT('Ctrl Pts',(20.7742875464824,19.9336824605317,39.8673605705435));
#49100=CARTESIAN_POINT('Ctrl Pts',(20.9586846468133,19.947486442863,39.7820612650716));
#49101=CARTESIAN_POINT('Ctrl Pts',(21.098046650583,19.9592630111454,39.6945789253741));
#49102=CARTESIAN_POINT('Ctrl Pts',(21.2872933814515,19.9766579990536,39.5390943181407));
#49103=CARTESIAN_POINT('Ctrl Pts',(21.3466424930026,19.9823494276627,39.4837174323383));
#49104=CARTESIAN_POINT('Ctrl Pts',(21.4087448344611,19.9884273640325,39.4179786229729));
#49105=CARTESIAN_POINT('Ctrl Pts',(21.415104696274,19.9890513113821,39.4111477286774));
#49106=CARTESIAN_POINT('Ctrl Pts',(21.4244834570584,19.9899733372056,39.4009266071075));
#49107=CARTESIAN_POINT('Ctrl Pts',(21.4275402531487,19.9902741559051,39.3975715715132));
#49108=CARTESIAN_POINT('Ctrl Pts',(21.4329734857427,19.9908093357816,39.391565801319));
#49109=CARTESIAN_POINT('Ctrl Pts',(21.4353544462621,19.9910440322346,39.3889192543719));
#49110=CARTESIAN_POINT('Ctrl Pts',(21.4404879009132,19.9915504073736,39.3831813185249));
#49111=CARTESIAN_POINT('Ctrl Pts',(21.443237770038,19.9918218920406,39.3800876645061));
#49112=CARTESIAN_POINT('Ctrl Pts',(21.4508849322831,19.9925775974396,39.3714284987859));
#49113=CARTESIAN_POINT('Ctrl Pts',(21.4557601979659,19.9930602198377,39.365843499257));
#49114=CARTESIAN_POINT('Ctrl Pts',(21.4839493924061,19.9958566650691,39.3331723083263));
#49115=CARTESIAN_POINT('Ctrl Pts',(21.5065409697201,19.9981214768895,39.3054685569875));
#49116=CARTESIAN_POINT('Ctrl Pts',(21.5782443308917,20.0054503343531,39.2123726570944));
#49117=CARTESIAN_POINT('Ctrl Pts',(21.623972727932,20.0103583263228,39.1444821263853));
#49118=CARTESIAN_POINT('Ctrl Pts',(21.7421847579459,20.024357512336,38.9423508726343));
#49119=CARTESIAN_POINT('Ctrl Pts',(21.803247398264,20.0333955004431,38.8021789440624));
#49120=CARTESIAN_POINT('Ctrl Pts',(21.853459103103,20.0444291324234,38.6354490173847));
#49121=CARTESIAN_POINT('Ctrl Pts',(21.8593821209898,20.045818910604,38.6145039983423));
#49122=CARTESIAN_POINT('Ctrl Pts',(21.8670944600564,20.0477599354255,38.5853567367578));
#49123=CARTESIAN_POINT('Ctrl Pts',(21.8691866933235,20.0483014836361,38.5772357766965));
#49124=CARTESIAN_POINT('Ctrl Pts',(21.8726968802224,20.049236598572,38.5632337919081));
#49125=CARTESIAN_POINT('Ctrl Pts',(21.8741402553103,20.0496293479759,38.5573592168126));
#49126=CARTESIAN_POINT('Ctrl Pts',(21.8770639289843,20.0504422681274,38.5452135230475));
#49127=CARTESIAN_POINT('Ctrl Pts',(21.8785404849612,20.0508625526628,38.5389415898211));
#49128=CARTESIAN_POINT('Ctrl Pts',(21.8819128338881,20.0518457017517,38.5242882093645));
#49129=CARTESIAN_POINT('Ctrl Pts',(21.8837840890325,20.0524093391408,38.5159013114189));
#49130=CARTESIAN_POINT('Ctrl Pts',(21.8896380575043,20.0542329007129,38.4888137629913));
#49131=CARTESIAN_POINT('Ctrl Pts',(21.8933987025167,20.0554998165771,38.4700668040557));
#49132=CARTESIAN_POINT('Ctrl Pts',(21.911171544734,20.0620125854446,38.3740916890476));
#49133=CARTESIAN_POINT('Ctrl Pts',(21.9207381032398,20.0673959068206,38.2961255799988));
#49134=CARTESIAN_POINT('Ctrl Pts',(21.9306229199611,20.0787271659919,38.1345535081039));
#49135=CARTESIAN_POINT('Ctrl Pts',(21.9303115787479,20.084678053253,38.051066871815));
#49136=CARTESIAN_POINT('Ctrl Pts',(21.917104114957,20.0984356395888,37.8586905182416));
#49137=CARTESIAN_POINT('Ctrl Pts',(21.9003312084986,20.1062212347068,37.7503350490334));
#49138=CARTESIAN_POINT('Ctrl Pts',(21.8722890258634,20.114191667664,37.6350694819463));
#49139=CARTESIAN_POINT('Ctrl Pts',(21.8700586465307,20.1148043648038,37.6261780401029));
#49140=CARTESIAN_POINT('Ctrl Pts',(21.8666375294097,20.1157130354577,37.6129402583701));
#49141=CARTESIAN_POINT('Ctrl Pts',(21.8654948446682,20.1160116370992,37.6085818036971));
#49142=CARTESIAN_POINT('Ctrl Pts',(21.8634226611789,20.1165444256061,37.6007894254387));
#49143=CARTESIAN_POINT('Ctrl Pts',(21.8624989279312,20.1167789354115,37.5973540449845));
#49144=CARTESIAN_POINT('Ctrl Pts',(21.8604735363488,20.117286685113,37.5899038236642));
#49145=CARTESIAN_POINT('Ctrl Pts',(21.859368385821,20.1175597214878,37.5858899969992));
#49146=CARTESIAN_POINT('Ctrl Pts',(21.8562295404201,20.1183241383047,37.5746324558864));
#49147=CARTESIAN_POINT('Ctrl Pts',(21.8541664229512,20.1188138602521,37.56739691733));
#49148=CARTESIAN_POINT('Ctrl Pts',(21.8415293831332,20.121739770149,37.524041194732));
#49149=CARTESIAN_POINT('Ctrl Pts',(21.8299418049666,20.1241214935229,37.4882218869513));
#49150=CARTESIAN_POINT('Ctrl Pts',(21.7619906241205,20.1367294843981,37.2974288475974));
#49151=CARTESIAN_POINT('Ctrl Pts',(21.6869784015494,20.1462552807949,37.1498179120137));
#49152=CARTESIAN_POINT('Ctrl Pts',(21.5497478396496,20.1610698670012,36.9484684581051));
#49153=CARTESIAN_POINT('Ctrl Pts',(21.5014625468668,20.1659470288155,36.886183209152));
#49154=CARTESIAN_POINT('Ctrl Pts',(21.4408447232797,20.1718167945172,36.8171588075002));
#49155=CARTESIAN_POINT('Ctrl Pts',(21.4320780642923,20.1726599602635,36.8073796203603));
#49156=CARTESIAN_POINT('Ctrl Pts',(21.4176844586401,20.1740355706943,36.7916497462919));
#49157=CARTESIAN_POINT('Ctrl Pts',(21.4121181715104,20.1745654737412,36.7856439306882));
#49158=CARTESIAN_POINT('Ctrl Pts',(21.4021428979645,20.1755115474532,36.7750174954372));
#49159=CARTESIAN_POINT('Ctrl Pts',(21.3977488590059,20.1759270782182,36.7703829614419));
#49160=CARTESIAN_POINT('Ctrl Pts',(21.3884439932401,20.1768045315955,36.7606659184575));
#49161=CARTESIAN_POINT('Ctrl Pts',(21.3835280970315,20.1772666693066,36.7555884161321));
#49162=CARTESIAN_POINT('Ctrl Pts',(21.3704497934732,20.1784924544795,36.7422278713968));
#49163=CARTESIAN_POINT('Ctrl Pts',(21.3622402999766,20.1792581474768,36.7339915283004));
#49164=CARTESIAN_POINT('Ctrl Pts',(21.3235123683717,20.1828534046414,36.6958332537641));
#49165=CARTESIAN_POINT('Ctrl Pts',(21.2920815265358,20.1857233329509,36.6668586671162));
#49166=CARTESIAN_POINT('Ctrl Pts',(21.133459230111,20.1999916283318,36.5300942851992));
#49167=CARTESIAN_POINT('Ctrl Pts',(20.9936366308077,20.2120039634669,36.4380727606343));
#49168=CARTESIAN_POINT('Ctrl Pts',(20.7769844192553,20.2290775021017,36.3326989191347));
#49169=CARTESIAN_POINT('Ctrl Pts',(20.7083709819766,20.2342724132195,36.3040960237335));
#49170=CARTESIAN_POINT('Ctrl Pts',(20.6295203537795,20.2398875366485,36.2764505278996));
#49171=CARTESIAN_POINT('Ctrl Pts',(20.6207469974858,20.2405074612004,36.2734453945825));
#49172=CARTESIAN_POINT('Ctrl Pts',(20.6076589673942,20.2414247152248,36.2690675519348));
#49173=CARTESIAN_POINT('Ctrl Pts',(20.60336073944,20.2417247445791,36.2676466309217));
#49174=CARTESIAN_POINT('Ctrl Pts',(20.5956744667335,20.2422590697356,36.2651356581803));
#49175=CARTESIAN_POINT('Ctrl Pts',(20.5922883800514,20.242493696438,36.264039842817));
#49176=CARTESIAN_POINT('Ctrl Pts',(20.5849497045539,20.2430005455212,36.2616872949759));
#49177=CARTESIAN_POINT('Ctrl Pts',(20.5809960986943,20.2432725705557,36.2604339391005));
#49178=CARTESIAN_POINT('Ctrl Pts',(20.5699277126936,20.2440313183915,36.2569643275209));
#49179=CARTESIAN_POINT('Ctrl Pts',(20.5628039929789,20.2445164219025,36.2547765019864));
#49180=CARTESIAN_POINT('Ctrl Pts',(20.520821252716,20.2473573086006,36.2421485771388));
#49181=CARTESIAN_POINT('Ctrl Pts',(20.4856825200526,20.2496622418272,36.232654399755));
#49182=CARTESIAN_POINT('Ctrl Pts',(20.3682236419186,20.2571912186197,36.204458520344));
#49183=CARTESIAN_POINT('Ctrl Pts',(20.2849421147792,20.2622493213279,36.1901632192109));
#49184=CARTESIAN_POINT('Ctrl Pts',(20.0530552173636,20.2761827986977,36.165871940095));
#49185=CARTESIAN_POINT('Ctrl Pts',(19.9038480656321,20.2850209714909,36.1675366158263));
#49186=CARTESIAN_POINT('Ctrl Pts',(19.734535230508,20.2958340683796,36.1890962103837));
#49187=CARTESIAN_POINT('Ctrl Pts',(19.7127999590524,20.2972361284344,36.1922419149831));
#49188=CARTESIAN_POINT('Ctrl Pts',(19.6828156951633,20.2991915729042,36.1971054904579));
#49189=CARTESIAN_POINT('Ctrl Pts',(19.6745166013135,20.2997350659232,36.1985074411959));
#49190=CARTESIAN_POINT('Ctrl Pts',(19.6602611282363,20.3006726387018,36.2010116518228));
#49191=CARTESIAN_POINT('Ctrl Pts',(19.6543002290282,20.3010658911029,36.2020877484819));
#49192=CARTESIAN_POINT('Ctrl Pts',(19.642013522804,20.3018790097305,36.2043656210585));
#49193=CARTESIAN_POINT('Ctrl Pts',(19.6356884742876,20.302298986016,36.205571028771));
#49194=CARTESIAN_POINT('Ctrl Pts',(19.620964322683,20.303279957875,36.2084535772744));
#49195=CARTESIAN_POINT('Ctrl Pts',(19.612570171059,20.3038417160265,36.2101550228484));
#49196=CARTESIAN_POINT('Ctrl Pts',(19.585626616049,20.3056530926891,36.2158033776958));
#49197=CARTESIAN_POINT('Ctrl Pts',(19.567124463433,20.3069095730287,36.2199678355833));
#49198=CARTESIAN_POINT('Ctrl Pts',(19.4965550129601,20.3117518853395,36.2369485162783));
#49199=CARTESIAN_POINT('Ctrl Pts',(19.4449830273365,20.3153962277656,36.2516573096051));
#49200=CARTESIAN_POINT('Ctrl Pts',(19.3941039696621,20.3190989370965,36.2684889961235));
#49201=CARTESIAN_POINT('Origin',(20.,-1.3495818343519,38.1));
#49202=CARTESIAN_POINT('',(19.3941043260691,21.2861174117667,36.2684888782178));
#49203=CARTESIAN_POINT('',(19.3941040087494,21.1141809091495,36.2684889831927));
#49204=CARTESIAN_POINT('',(19.3941040087494,-1.3495818343519,36.2684889831927));
#49205=CARTESIAN_POINT('Ctrl Pts',(19.3941043260691,21.2861174117667,36.2684888782178));
#49206=CARTESIAN_POINT('Ctrl Pts',(19.4530786536075,21.2817380599914,36.2489791468798));
#49207=CARTESIAN_POINT('Ctrl Pts',(19.513005684334,21.2773036111486,36.2323143814167));
#49208=CARTESIAN_POINT('Ctrl Pts',(19.6542575541718,21.2669641769365,36.2003077326673));
#49209=CARTESIAN_POINT('Ctrl Pts',(19.7359292577877,21.2610689936283,36.1872436377992));
#49210=CARTESIAN_POINT('Ctrl Pts',(19.8540254899233,21.2528461851445,36.1760640370774));
#49211=CARTESIAN_POINT('Ctrl Pts',(19.8899504322543,21.2503850532323,36.1736750926777));
#49212=CARTESIAN_POINT('Ctrl Pts',(19.9333558357535,21.2474758123637,36.1720071504368));
#49213=CARTESIAN_POINT('Ctrl Pts',(19.9407895419167,21.2469798467427,36.1717645375422));
#49214=CARTESIAN_POINT('Ctrl Pts',(19.9523714299181,21.2462108574831,36.1714535824357));
#49215=CARTESIAN_POINT('Ctrl Pts',(19.9565186440202,21.2459362457946,36.171355621719));
#49216=CARTESIAN_POINT('Ctrl Pts',(19.9642163443898,21.2454279595525,36.1711986375657));
#49217=CARTESIAN_POINT('Ctrl Pts',(19.9677666707605,21.2451940943045,36.1711360393342));
#49218=CARTESIAN_POINT('Ctrl Pts',(19.9758248462538,21.2446645706607,36.171016215258));
#49219=CARTESIAN_POINT('Ctrl Pts',(19.9803327248656,21.2443692489433,36.1709649875726));
#49220=CARTESIAN_POINT('Ctrl Pts',(19.9940939636114,21.2434703599312,36.1708568477203));
#49221=CARTESIAN_POINT('Ctrl Pts',(20.0033477575419,21.2428695451387,36.1708507097407));
#49222=CARTESIAN_POINT('Ctrl Pts',(20.0885530179799,21.2373680965722,36.1714072993462));
#49223=CARTESIAN_POINT('Ctrl Pts',(20.1644192405313,21.2326925888865,36.1763886224085));
#49224=CARTESIAN_POINT('Ctrl Pts',(20.4053846792953,21.2180052321809,36.2065762507952));
#49225=CARTESIAN_POINT('Ctrl Pts',(20.5675666773086,21.2083026314686,36.248714299268));
#49226=CARTESIAN_POINT('Ctrl Pts',(20.7604899077144,21.1953394782839,36.3266152572359));
#49227=CARTESIAN_POINT('Ctrl Pts',(20.7981684855944,21.1927393247003,36.3432515763493));
#49228=CARTESIAN_POINT('Ctrl Pts',(20.8455913928736,21.1893644891853,36.366030994445));
#49229=CARTESIAN_POINT('Ctrl Pts',(20.85585449596,21.1886278783365,36.3710736312747));
#49230=CARTESIAN_POINT('Ctrl Pts',(20.8723214668155,21.1874356206372,36.379347004679));
#49231=CARTESIAN_POINT('Ctrl Pts',(20.8785537583876,21.1869819647847,36.3825208114063));
#49232=CARTESIAN_POINT('Ctrl Pts',(20.8904101581071,21.1861142288381,36.3886401276433));
#49233=CARTESIAN_POINT('Ctrl Pts',(20.8960372648553,21.1857003635763,36.3915796533806));
#49234=CARTESIAN_POINT('Ctrl Pts',(20.9088810185705,21.1847510057067,36.3983699700053));
#49235=CARTESIAN_POINT('Ctrl Pts',(20.9160878491944,21.1842148737211,36.4022389703014));
#49236=CARTESIAN_POINT('Ctrl Pts',(20.9348584711648,21.1828093685556,36.4124703278089));
#49237=CARTESIAN_POINT('Ctrl Pts',(20.9463817963244,21.181937409327,36.4189056431971));
#49238=CARTESIAN_POINT('Ctrl Pts',(21.0298614889384,21.1755526819184,36.4666560392451));
#49239=CARTESIAN_POINT('Ctrl Pts',(21.0991419192553,21.169877751565,36.5124513219875));
#49240=CARTESIAN_POINT('Ctrl Pts',(21.2943721212357,21.1527427812399,36.6604194150749));
#49241=CARTESIAN_POINT('Ctrl Pts',(21.4106373212665,21.1409379368308,36.7741462546931));
#49242=CARTESIAN_POINT('Ctrl Pts',(21.5345450015419,21.1270994775988,36.9303372496378));
#49243=CARTESIAN_POINT('Ctrl Pts',(21.5569184125529,21.1245415249144,36.9602873934727));
#49244=CARTESIAN_POINT('Ctrl Pts',(21.5827031305217,21.1215376499932,36.9969818056244));
#49245=CARTESIAN_POINT('Ctrl Pts',(21.5869616573707,21.1210396066896,37.003117581942));
#49246=CARTESIAN_POINT('Ctrl Pts',(21.5935202523732,21.1202697330977,37.0126854970061));
#49247=CARTESIAN_POINT('Ctrl Pts',(21.5958450526281,21.119996276264,37.0161004696246));
#49248=CARTESIAN_POINT('Ctrl Pts',(21.6001464149953,21.119489313078,37.0224627152164));
#49249=CARTESIAN_POINT('Ctrl Pts',(21.602125792458,21.1192556226636,37.0254079402611));
#49250=CARTESIAN_POINT('Ctrl Pts',(21.6065987840943,21.1187265911647,37.032103382718));
#49251=CARTESIAN_POINT('Ctrl Pts',(21.6090874019486,21.1184315850437,37.0358568836092));
#49252=CARTESIAN_POINT('Ctrl Pts',(21.6165931069662,21.1175396846526,37.0472640258523));
#49253=CARTESIAN_POINT('Ctrl Pts',(21.6215689879624,21.1169454480223,37.0549448196159));
#49254=CARTESIAN_POINT('Ctrl Pts',(21.6857361985965,21.1092394010588,37.1555554463062));
#49255=CARTESIAN_POINT('Ctrl Pts',(21.7369247673846,21.1026029143702,37.253370230959));
#49256=CARTESIAN_POINT('Ctrl Pts',(21.812183949424,21.0909436145242,37.4331404862799));
#49257=CARTESIAN_POINT('Ctrl Pts',(21.8397040202578,21.0859163435093,37.5133136160916));
#49258=CARTESIAN_POINT('Ctrl Pts',(21.8820351897066,21.0761070359057,37.6693931048017));
#49259=CARTESIAN_POINT('Ctrl Pts',(21.897727972401,21.0713530011949,37.7448869903914));
#49260=CARTESIAN_POINT('Ctrl Pts',(21.9116047707611,21.065249769927,37.8398672342602));
#49261=CARTESIAN_POINT('Ctrl Pts',(21.9140683977022,21.0640364059259,37.8586620963925));
#49262=CARTESIAN_POINT('Ctrl Pts',(21.9172437241738,21.062261568147,37.8860079486286));
#49263=CARTESIAN_POINT('Ctrl Pts',(21.918176017861,21.0617069651693,37.8945325900674));
#49264=CARTESIAN_POINT('Ctrl Pts',(21.9197101998067,21.0607319086572,37.9094824209609));
#49265=CARTESIAN_POINT('Ctrl Pts',(21.9203367476118,21.0603122293246,37.9159049885079));
#49266=CARTESIAN_POINT('Ctrl Pts',(21.921490574949,21.0594954809485,37.9283799656088));
#49267=CARTESIAN_POINT('Ctrl Pts',(21.9220215115702,21.0590985309182,37.9344319672444));
#49268=CARTESIAN_POINT('Ctrl Pts',(21.9232224994058,21.0581473643596,37.9489067617029));
#49269=CARTESIAN_POINT('Ctrl Pts',(21.9238658138255,21.0575923236917,37.9573315891652));
#49270=CARTESIAN_POINT('Ctrl Pts',(21.92599124032,21.0555795844935,37.9878015899245));
#49271=CARTESIAN_POINT('Ctrl Pts',(21.9271498894069,21.0541119290967,38.0098668963292));
#49272=CARTESIAN_POINT('Ctrl Pts',(21.9330165595865,21.0429770023299,38.1760673539951));
#49273=CARTESIAN_POINT('Ctrl Pts',(21.921926607354,21.0328099751706,38.3202776090934));
#49274=CARTESIAN_POINT('Ctrl Pts',(21.8785680200289,21.0163278764021,38.5473149834864));
#49275=CARTESIAN_POINT('Ctrl Pts',(21.856490665271,21.0101155227914,38.6315568006907));
#49276=CARTESIAN_POINT('Ctrl Pts',(21.817019995336,21.0015161281742,38.7491155977939));
#49277=CARTESIAN_POINT('Ctrl Pts',(21.8042297042457,20.9989842712054,38.7838628045715));
#49278=CARTESIAN_POINT('Ctrl Pts',(21.7876508626281,20.9960021214082,38.8251919269138));
#49279=CARTESIAN_POINT('Ctrl Pts',(21.7848146217099,20.9955014613372,38.8321445951326));
#49280=CARTESIAN_POINT('Ctrl Pts',(21.7803401539089,20.9947264001822,38.8429326236933));
#49281=CARTESIAN_POINT('Ctrl Pts',(21.7787300017751,20.9944503818302,38.8467794376971));
#49282=CARTESIAN_POINT('Ctrl Pts',(21.775719304002,20.9939396379641,38.8539073129886));
#49283=CARTESIAN_POINT('Ctrl Pts',(21.7743221400591,20.9937047214475,38.8571896901662));
#49284=CARTESIAN_POINT('Ctrl Pts',(21.7711313980161,20.9931729638317,38.8646284189198));
#49285=CARTESIAN_POINT('Ctrl Pts',(21.7693322946587,20.9928764594571,38.8687823360134));
#49286=CARTESIAN_POINT('Ctrl Pts',(21.7646305596737,20.9921100416799,38.8795341564602));
#49287=CARTESIAN_POINT('Ctrl Pts',(21.7617055088434,20.9916414441549,38.8861222661129));
#49288=CARTESIAN_POINT('Ctrl Pts',(21.7428801021627,20.9886761357281,38.9278900409968));
#49289=CARTESIAN_POINT('Ctrl Pts',(21.7259624042659,20.9862365757345,38.9626049113432));
#49290=CARTESIAN_POINT('Ctrl Pts',(21.7024018777434,20.9830862984951,39.0074778724268));
#49291=CARTESIAN_POINT('Ctrl Pts',(21.6966906319288,20.9823399963124,39.0181117321505));
#49292=CARTESIAN_POINT('Ctrl Pts',(21.6251243888338,20.9731897381084,39.1484132593932));
#49293=CARTESIAN_POINT('Ctrl Pts',(21.5468367123748,20.9652128951141,39.2608189840831));
#49294=CARTESIAN_POINT('Ctrl Pts',(21.4018331783591,20.9518403516606,39.4279982559164));
#49295=CARTESIAN_POINT('Ctrl Pts',(21.342192640408,20.9466366368227,39.4882478086865));
#49296=CARTESIAN_POINT('Ctrl Pts',(21.2638892331462,20.9399937019944,39.5575742638341));
#49297=CARTESIAN_POINT('Ctrl Pts',(21.24878380741,20.938720486148,39.5705365291897));
#49298=CARTESIAN_POINT('Ctrl Pts',(21.2267643605746,20.9368747640557,39.588847900649));
#49299=CARTESIAN_POINT('Ctrl Pts',(21.2200099939171,20.9363099568753,39.5943876599692));
#49300=CARTESIAN_POINT('Ctrl Pts',(21.2081887341865,20.9353236785883,39.6039495960522));
#49301=CARTESIAN_POINT('Ctrl Pts',(21.2031387634259,20.9349030447146,39.6079925461116));
#49302=CARTESIAN_POINT('Ctrl Pts',(21.1933540759508,20.9340893271147,39.6157456211735));
#49303=CARTESIAN_POINT('Ctrl Pts',(21.1886221472469,20.9336963850587,39.6194591565408));
#49304=CARTESIAN_POINT('Ctrl Pts',(21.177361187723,20.9327625844666,39.6282117689243));
#49305=CARTESIAN_POINT('Ctrl Pts',(21.1708170993336,20.9322209636444,39.6332311937149));
#49306=CARTESIAN_POINT('Ctrl Pts',(21.1475714980462,20.9303005457373,39.6508253532704));
#49307=CARTESIAN_POINT('Ctrl Pts',(21.1306984734675,20.9289129084639,39.6631700238439));
#49308=CARTESIAN_POINT('Ctrl Pts',(20.9797784232138,20.9165518939551,39.7698643380567));
#49309=CARTESIAN_POINT('Ctrl Pts',(20.8344380519894,20.9049100657465,39.8470271596253));
#49310=CARTESIAN_POINT('Ctrl Pts',(20.6118752125089,20.8879419200109,39.9310193124834));
#49311=CARTESIAN_POINT('Ctrl Pts',(20.5411611809335,20.8826798684249,39.9531511186928));
#49312=CARTESIAN_POINT('Ctrl Pts',(20.4366324219033,20.8752250306513,39.9793701553393));
#49313=CARTESIAN_POINT('Ctrl Pts',(20.4037069540682,20.8729227015064,39.9867170135623));
#49314=CARTESIAN_POINT('Ctrl Pts',(20.3634514272122,20.870176555391,39.9945972469143));
#49315=CARTESIAN_POINT('Ctrl Pts',(20.3562914207787,20.869690742674,39.9959567757769));
#49316=CARTESIAN_POINT('Ctrl Pts',(20.345080360158,20.8689343483586,39.9980197587123));
#49317=CARTESIAN_POINT('Ctrl Pts',(20.3410345626943,20.8686622552477,39.998750875513));
#49318=CARTESIAN_POINT('Ctrl Pts',(20.333479800961,20.8681558365528,40.0000911721797));
#49319=CARTESIAN_POINT('Ctrl Pts',(20.3299715217119,20.8679213391175,40.0007035632666));
#49320=CARTESIAN_POINT('Ctrl Pts',(20.3219533526429,20.8673869135395,40.0020803132277));
#49321=CARTESIAN_POINT('Ctrl Pts',(20.3174424333628,20.8670873437189,40.0028383488388));
#49322=CARTESIAN_POINT('Ctrl Pts',(20.3056453041331,20.8663066465731,40.0047776741459));
#49323=CARTESIAN_POINT('Ctrl Pts',(20.298354851389,20.865826924639,40.0059332167614));
#49324=CARTESIAN_POINT('Ctrl Pts',(20.2494790731442,20.8626280621921,40.0133927483809));
#49325=CARTESIAN_POINT('Ctrl Pts',(20.2077002527982,20.8599770802714,40.0183776573052));
#49326=CARTESIAN_POINT('Ctrl Pts',(20.1583209762786,20.8569066141167,40.0226370438984));
#49327=CARTESIAN_POINT('Ctrl Pts',(20.150849784348,20.8564437345537,40.0232376554204));
#49328=CARTESIAN_POINT('Ctrl Pts',(20.1298918897804,20.8551495544537,40.0247995904074));
#49329=CARTESIAN_POINT('Ctrl Pts',(20.1163981485239,20.8543212503624,40.02566270417));
#49330=CARTESIAN_POINT('Ctrl Pts',(19.9847847460247,20.8462812323355,40.032692726101));
#49331=CARTESIAN_POINT('Ctrl Pts',(19.8663397391472,20.8393363118176,40.0281260326375));
#49332=CARTESIAN_POINT('Ctrl Pts',(19.6835322088371,20.8282215762719,40.0041422777983));
#49333=CARTESIAN_POINT('Ctrl Pts',(19.6184994585567,20.8241906396675,39.9921854860312));
#49334=CARTESIAN_POINT('Ctrl Pts',(19.5166213884595,20.8176514627929,39.9679883405995));
#49335=CARTESIAN_POINT('Ctrl Pts',(19.4793097206715,20.8152080408505,39.9579334304749));
#49336=CARTESIAN_POINT('Ctrl Pts',(19.4315771843869,20.8120079228133,39.9435195022696));
#49337=CARTESIAN_POINT('Ctrl Pts',(19.4208561228392,20.8112842695956,39.9401796144482));
#49338=CARTESIAN_POINT('Ctrl Pts',(19.4035241307728,20.8101061885651,39.9346137859423));
#49339=CARTESIAN_POINT('Ctrl Pts',(19.396894937397,20.8096536355749,39.9324452208689));
#49340=CARTESIAN_POINT('Ctrl Pts',(19.3842030378788,20.8087833761557,39.9282170701286));
#49341=CARTESIAN_POINT('Ctrl Pts',(19.3781385294055,20.8083658604063,39.9261631536649));
#49342=CARTESIAN_POINT('Ctrl Pts',(19.3643186995108,20.8074105187375,39.9214058564097));
#49343=CARTESIAN_POINT('Ctrl Pts',(19.3565702337417,20.8068720606466,39.9186830790249));
#49344=CARTESIAN_POINT('Ctrl Pts',(19.3361085881551,20.8054425384426,39.9113458163529));
#49345=CARTESIAN_POINT('Ctrl Pts',(19.3234263284071,20.8045487069609,39.9066470392066));
#49346=CARTESIAN_POINT('Ctrl Pts',(19.2240385739183,20.7974810827014,39.8686306263865));
#49347=CARTESIAN_POINT('Ctrl Pts',(19.1398058304123,20.7911035751112,39.8292286529764));
#49348=CARTESIAN_POINT('Ctrl Pts',(18.9193057411064,20.7733565314104,39.7059769132127));
#49349=CARTESIAN_POINT('Ctrl Pts',(18.7900926816148,20.7617248975331,39.6110208129822));
#49350=CARTESIAN_POINT('Ctrl Pts',(18.6529510204969,20.7487191795197,39.4812481908839));
#49351=CARTESIAN_POINT('Ctrl Pts',(18.6322900881075,20.7467412802435,39.4607929087645));
#49352=CARTESIAN_POINT('Ctrl Pts',(18.6072660011793,20.74433095791,39.4348718915644));
#49353=CARTESIAN_POINT('Ctrl Pts',(18.6024609566081,20.7438674411294,39.4298404356177));
#49354=CARTESIAN_POINT('Ctrl Pts',(18.5949112795147,20.7431382195105,39.4218489083909));
#49355=CARTESIAN_POINT('Ctrl Pts',(18.592148595844,20.7428711701187,39.4189060897612));
#49356=CARTESIAN_POINT('Ctrl Pts',(18.5869563238376,20.7423689236967,39.4133403626425));
#49357=CARTESIAN_POINT('Ctrl Pts',(18.5845248198157,20.7421335856978,39.4107194029951));
#49358=CARTESIAN_POINT('Ctrl Pts',(18.5789708506079,20.7415956851671,39.4046992056137));
#49359=CARTESIAN_POINT('Ctrl Pts',(18.5758532885409,20.741293492685,39.4012955105899));
#49360=CARTESIAN_POINT('Ctrl Pts',(18.5675814949199,20.7404908946309,39.3921991927915));
#49361=CARTESIAN_POINT('Ctrl Pts',(18.562448923044,20.7399920615767,39.3864868570794));
#49362=CARTESIAN_POINT('Ctrl Pts',(18.5252953457473,20.7363737080218,39.344636500091));
#49363=CARTESIAN_POINT('Ctrl Pts',(18.4946039320468,20.7333441227353,39.3073348356099));
#49364=CARTESIAN_POINT('Ctrl Pts',(18.4569991913185,20.7295200251917,39.257964005415));
#49365=CARTESIAN_POINT('Ctrl Pts',(18.4487736885712,20.7286761324003,39.2469215657361));
#49366=CARTESIAN_POINT('Ctrl Pts',(18.3686241837584,20.7203688115048,39.1368839964109));
#49367=CARTESIAN_POINT('Ctrl Pts',(18.306153006079,20.7131922398046,39.031343336422));
#49368=CARTESIAN_POINT('Ctrl Pts',(18.2270148952385,20.7019606705466,38.8629681662927));
#49369=CARTESIAN_POINT('Ctrl Pts',(18.2028024607114,20.6980703894045,38.8040430365984));
#49370=CARTESIAN_POINT('Ctrl Pts',(18.1689728312178,20.6917369514213,38.708523675981));
#49371=CARTESIAN_POINT('Ctrl Pts',(18.1574404500939,20.6893533089713,38.6726565824612));
#49372=CARTESIAN_POINT('Ctrl Pts',(18.1438681532177,20.686220444831,38.6257767673026));
#49373=CARTESIAN_POINT('Ctrl Pts',(18.140863176003,20.6855024856943,38.6150503886727));
#49374=CARTESIAN_POINT('Ctrl Pts',(18.1361316589063,20.6843310145616,38.5975799608769));
#49375=CARTESIAN_POINT('Ctrl Pts',(18.1343484026852,20.6838793316209,38.5908514293874));
#49376=CARTESIAN_POINT('Ctrl Pts',(18.1309909504513,20.6830089112049,38.5779005381241));
#49377=CARTESIAN_POINT('Ctrl Pts',(18.1294113132571,20.6825903547232,38.5716796741426));
#49378=CARTESIAN_POINT('Ctrl Pts',(18.1258668752172,20.6816300446292,38.5574232369915));
#49379=CARTESIAN_POINT('Ctrl Pts',(18.1239226685804,20.6810876408784,38.5493827211766));
#49380=CARTESIAN_POINT('Ctrl Pts',(18.1188942129158,20.6796419680049,38.5279853848949));
#49381=CARTESIAN_POINT('Ctrl Pts',(18.1159005632451,20.6787358388782,38.5146079689316));
#49382=CARTESIAN_POINT('Ctrl Pts',(18.0848801270923,20.668826538751,38.3687106412563));
#49383=CARTESIAN_POINT('Ctrl Pts',(18.0707478826055,20.659371969667,38.2336496127508));
#49384=CARTESIAN_POINT('Ctrl Pts',(18.0709928462404,20.6401631583163,37.9637962455339));
#49385=CARTESIAN_POINT('Ctrl Pts',(18.0851705182672,20.6304706736182,37.8297155384801));
#49386=CARTESIAN_POINT('Ctrl Pts',(18.1161120013264,20.620408379265,37.6844198972611));
#49387=CARTESIAN_POINT('Ctrl Pts',(18.11919551829,20.6194616306672,37.6706803717333));
#49388=CARTESIAN_POINT('Ctrl Pts',(18.1236983313918,20.6181544599231,37.6515971218349));
#49389=CARTESIAN_POINT('Ctrl Pts',(18.1249904825226,20.61778729405,37.646224280073));
#49390=CARTESIAN_POINT('Ctrl Pts',(18.1271039921872,20.6171993621344,37.6375993618584));
#49391=CARTESIAN_POINT('Ctrl Pts',(18.127910764255,20.6169777789537,37.6343437962699));
#49392=CARTESIAN_POINT('Ctrl Pts',(18.1296179757692,20.6165148013958,37.6275308414398));
#49393=CARTESIAN_POINT('Ctrl Pts',(18.1305200792661,20.6162735090259,37.6239738992171));
#49394=CARTESIAN_POINT('Ctrl Pts',(18.1327397539886,20.6156878057185,37.6153254811324));
#49395=CARTESIAN_POINT('Ctrl Pts',(18.1340680199539,20.6153440032017,37.6102367275803));
#49396=CARTESIAN_POINT('Ctrl Pts',(18.1388622324917,20.6141262696561,37.5921721260313));
#49397=CARTESIAN_POINT('Ctrl Pts',(18.1424429528276,20.6132586438342,37.579226747897));
#49398=CARTESIAN_POINT('Ctrl Pts',(18.1653294684156,20.6079553450875,37.4997260748553));
#49399=CARTESIAN_POINT('Ctrl Pts',(18.1880768118965,20.6036922667605,37.434206287396));
#49400=CARTESIAN_POINT('Ctrl Pts',(18.2668309394992,20.5910952720247,37.2415489187266));
#49401=CARTESIAN_POINT('Ctrl Pts',(18.3330727075436,20.5829761589737,37.1190985668106));
#49402=CARTESIAN_POINT('Ctrl Pts',(18.4489458117829,20.5704728911086,36.951072028565));
#49403=CARTESIAN_POINT('Ctrl Pts',(18.4887088310256,20.5664027502613,36.8992493226898));
#49404=CARTESIAN_POINT('Ctrl Pts',(18.5391303563616,20.5614281283557,36.8400162540496));
#49405=CARTESIAN_POINT('Ctrl Pts',(18.5473342185821,20.5606242115891,36.8305665549551));
#49406=CARTESIAN_POINT('Ctrl Pts',(18.560932907847,20.5593001394236,36.8152072255856));
#49407=CARTESIAN_POINT('Ctrl Pts',(18.5662736787097,20.5587822174707,36.8092500624174));
#49408=CARTESIAN_POINT('Ctrl Pts',(18.57593029567,20.557849406416,36.7986128318426));
#49409=CARTESIAN_POINT('Ctrl Pts',(18.5802325671074,20.5574350900605,36.7939205540572));
#49410=CARTESIAN_POINT('Ctrl Pts',(18.5894346797119,20.5565515557838,36.783983453731));
#49411=CARTESIAN_POINT('Ctrl Pts',(18.5943407126723,20.5560820787099,36.7787445218794));
#49412=CARTESIAN_POINT('Ctrl Pts',(18.6076141547584,20.5548160105801,36.7647280152689));
#49413=CARTESIAN_POINT('Ctrl Pts',(18.6160351717435,20.5540171277593,36.7560018757322));
#49414=CARTESIAN_POINT('Ctrl Pts',(18.6586246307406,20.5499976713498,36.71269396313));
#49415=CARTESIAN_POINT('Ctrl Pts',(18.6940067056829,20.5467242182585,36.6793358170251));
#49416=CARTESIAN_POINT('Ctrl Pts',(18.8552168211107,20.5320756402526,36.5384628965962));
#49417=CARTESIAN_POINT('Ctrl Pts',(18.9933083352661,20.5201252832972,36.4460705891164));
#49418=CARTESIAN_POINT('Ctrl Pts',(19.2030934478916,20.5035569674476,36.341813392907));
#49419=CARTESIAN_POINT('Ctrl Pts',(19.2663346837732,20.4987558837779,36.3144979396941));
#49420=CARTESIAN_POINT('Ctrl Pts',(19.3395314034464,20.4935121198439,36.2874304622701));
#49421=CARTESIAN_POINT('Ctrl Pts',(19.3481780820398,20.4928975294562,36.2843030837612));
#49422=CARTESIAN_POINT('Ctrl Pts',(19.3610999829948,20.4919866217655,36.2797336252887));
#49423=CARTESIAN_POINT('Ctrl Pts',(19.3653582839632,20.4916876572992,36.2782445828467));
#49424=CARTESIAN_POINT('Ctrl Pts',(19.3729840108008,20.4911544984062,36.2756080021452));
#49425=CARTESIAN_POINT('Ctrl Pts',(19.3763494125397,20.4909199788694,36.2744548326584));
#49426=CARTESIAN_POINT('Ctrl Pts',(19.3836555889905,20.4904125306446,36.2719739018155));
#49427=CARTESIAN_POINT('Ctrl Pts',(19.3875974635277,20.4901398037333,36.2706495735492));
#49428=CARTESIAN_POINT('Ctrl Pts',(19.3923968938888,20.4898089912107,36.2690543888959));
#49429=CARTESIAN_POINT('Ctrl Pts',(19.3932503519079,20.489750212374,36.2687713878594));
#49430=CARTESIAN_POINT('Ctrl Pts',(19.3941040087494,20.489691467393,36.2684889831927));
#49431=CARTESIAN_POINT('',(18.0708703408215,20.4785431656481,38.1011467247646));
#49432=CARTESIAN_POINT('Ctrl Pts',(19.3941039696621,20.3190989370965,36.2684889961235));
#49433=CARTESIAN_POINT('Ctrl Pts',(19.3716471618326,20.3207332250667,36.2759181028497));
#49434=CARTESIAN_POINT('Ctrl Pts',(19.3493253354268,20.3223787230364,36.2837607820347));
#49435=CARTESIAN_POINT('Ctrl Pts',(19.2482078801407,20.3299262073019,36.3213920884692));
#49436=CARTESIAN_POINT('Ctrl Pts',(19.1712792221264,20.3359349437724,36.3559077664399));
#49437=CARTESIAN_POINT('Ctrl Pts',(18.9996103855285,20.3497960266246,36.44685915099));
#49438=CARTESIAN_POINT('Ctrl Pts',(18.906938389977,20.3576277663694,36.5066148479924));
#49439=CARTESIAN_POINT('Ctrl Pts',(18.8126148015479,20.3656391045745,36.579558341963));
#49440=CARTESIAN_POINT('Ctrl Pts',(18.8054093265105,20.3662512927585,36.5852130262149));
#49441=CARTESIAN_POINT('Ctrl Pts',(18.7947208197537,20.3671593554595,36.5937248120561));
#49442=CARTESIAN_POINT('Ctrl Pts',(18.7912072068778,20.3674578531395,36.5965430406995));
#49443=CARTESIAN_POINT('Ctrl Pts',(18.7849363823635,20.3679905251424,36.6016089910456));
#49444=CARTESIAN_POINT('Ctrl Pts',(18.7821754976225,20.3682250218602,36.6038520485203));
#49445=CARTESIAN_POINT('Ctrl Pts',(18.7794083306838,20.3684600241805,36.6061129447132));
#49446=CARTESIAN_POINT('Ctrl Pts',(18.7793959008334,20.3684610797881,36.6061231007023));
#49447=CARTESIAN_POINT('Ctrl Pts',(18.7793712052984,20.3684631770605,36.6061432790605));
#49448=CARTESIAN_POINT('Ctrl Pts',(18.7793589399764,20.3684642186945,36.6061533011265));
#49449=CARTESIAN_POINT('Ctrl Pts',(18.7793345722372,20.368466288127,36.6061732126485));
#49450=CARTESIAN_POINT('Ctrl Pts',(18.7793224691425,20.3684673159829,36.6061831026515));
#49451=CARTESIAN_POINT('Ctrl Pts',(18.7792984214893,20.3684693582303,36.6062027535976));
#49452=CARTESIAN_POINT('Ctrl Pts',(18.7792864772904,20.3684703725911,36.6062125142405));
#49453=CARTESIAN_POINT('Ctrl Pts',(18.7760953336031,20.3687413802891,36.6088203388873));
#49454=CARTESIAN_POINT('Ctrl Pts',(18.7729243998563,20.3690106410012,36.6114285752936));
#49455=CARTESIAN_POINT('Ctrl Pts',(18.7642122353526,20.3697504291266,36.6186414799745));
#49456=CARTESIAN_POINT('Ctrl Pts',(18.7586883654837,20.3702194765097,36.6232671554728));
#49457=CARTESIAN_POINT('Ctrl Pts',(18.7462596930017,20.3712751518598,36.6337939116918));
#49458=CARTESIAN_POINT('Ctrl Pts',(18.7393703388348,20.3718605519273,36.6397130708068));
#49459=CARTESIAN_POINT('Ctrl Pts',(18.7179033888305,20.3736862990958,36.6584220775019));
#49460=CARTESIAN_POINT('Ctrl Pts',(18.7034762268257,20.3749157545948,36.6713836081802));
#49461=CARTESIAN_POINT('Ctrl Pts',(18.6463164774943,20.3798084642916,36.7243158425823));
#49462=CARTESIAN_POINT('Ctrl Pts',(18.6052139254752,20.3833769835044,36.7660064240685));
#49463=CARTESIAN_POINT('Ctrl Pts',(18.5004791923888,20.3928162290999,36.8823822660866));
#49464=CARTESIAN_POINT('Ctrl Pts',(18.4405422746111,20.3986055688392,36.9601545623183));
#49465=CARTESIAN_POINT('Ctrl Pts',(18.3343681786917,20.4102884422177,37.1220697728059));
#49466=CARTESIAN_POINT('Ctrl Pts',(18.28797799341,20.4161601134303,37.2057663187303));
#49467=CARTESIAN_POINT('Ctrl Pts',(18.2422929310617,20.4231300315013,37.3048942077643));
#49468=CARTESIAN_POINT('Ctrl Pts',(18.2367337285371,20.4240023854527,37.3172999285764));
#49469=CARTESIAN_POINT('Ctrl Pts',(18.2280173795923,20.4254104578191,37.3373152674415));
#49470=CARTESIAN_POINT('Ctrl Pts',(18.2247769903029,20.4259433586893,37.3448883058201));
#49471=CARTESIAN_POINT('Ctrl Pts',(18.2191009991907,20.4268939445154,37.3583920117446));
#49472=CARTESIAN_POINT('Ctrl Pts',(18.216646259645,20.4273109780362,37.3643145410993));
#49473=CARTESIAN_POINT('Ctrl Pts',(18.2115833163227,20.4281836901362,37.3767041082259));
#49474=CARTESIAN_POINT('Ctrl Pts',(18.2089805679969,20.428639544319,37.3831732611315));
#49475=CARTESIAN_POINT('Ctrl Pts',(18.2022878343676,20.4298308594311,37.4000721234502));
#49476=CARTESIAN_POINT('Ctrl Pts',(18.1982535743931,20.4305681641121,37.4105234799487));
#49477=CARTESIAN_POINT('Ctrl Pts',(18.180824924404,20.4338406673716,37.4568727496232));
#49478=CARTESIAN_POINT('Ctrl Pts',(18.1684115238389,20.4364079173706,37.4931277598327));
#49479=CARTESIAN_POINT('Ctrl Pts',(18.1377917785253,20.4434401539474,37.5920794319352));
#49480=CARTESIAN_POINT('Ctrl Pts',(18.121675866749,20.447966194841,37.6553656297573));
#49481=CARTESIAN_POINT('Ctrl Pts',(18.0835039116005,20.4615782357669,37.8450128468811));
#49482=CARTESIAN_POINT('Ctrl Pts',(18.0708001340919,20.4708402101582,37.9728809532063));
#49483=CARTESIAN_POINT('Ctrl Pts',(18.0708702889621,20.4798373080997,38.1010558838905));
#49484=CARTESIAN_POINT('Ctrl Pts',(18.0708703408215,20.4785431656481,38.1011467247647));
#49485=CARTESIAN_POINT('Ctrl Pts',(18.0709111555238,20.483059702729,38.1698091058912));
#49486=CARTESIAN_POINT('Ctrl Pts',(18.0746175415454,20.4875762398099,38.2383609278836));
#49487=CARTESIAN_POINT('Ctrl Pts',(18.0819556351502,20.4920927768908,38.3065148211825));
#49488=CARTESIAN_POINT('Ctrl Pts',(18.0891992046318,20.4965511351406,38.37379080431));
#49489=CARTESIAN_POINT('Ctrl Pts',(18.100000955713,20.5010094933905,38.4408181004181));
#49490=CARTESIAN_POINT('Ctrl Pts',(18.1143335343437,20.5054678516404,38.507191032808));
#49491=CARTESIAN_POINT('Ctrl Pts',(18.12938235242,20.5101490066474,38.5768808081418));
#49492=CARTESIAN_POINT('Ctrl Pts',(18.1483241750998,20.5148301616545,38.6458485571126));
#49493=CARTESIAN_POINT('Ctrl Pts',(18.1710655625826,20.5195113166616,38.7136296770274));
#49494=CARTESIAN_POINT('Ctrl Pts',(18.1926658517794,20.5239575845951,38.7780097327012));
#49495=CARTESIAN_POINT('Ctrl Pts',(18.2176934096763,20.5284038525285,38.8413188378757));
#49496=CARTESIAN_POINT('Ctrl Pts',(18.2460161837978,20.532850120462,38.903170797154));
#49497=CARTESIAN_POINT('Ctrl Pts',(18.2743218618263,20.5372937045549,38.9649854215706));
#49498=CARTESIAN_POINT('Ctrl Pts',(18.3059186054943,20.5417372886478,39.0253441974552));
#49499=CARTESIAN_POINT('Ctrl Pts',(18.3406260642371,20.5461808727408,39.0838804288178));
#49500=CARTESIAN_POINT('Ctrl Pts',(18.3753245338612,20.5506233059599,39.1424014994872));
#49501=CARTESIAN_POINT('Ctrl Pts',(18.4131318675803,20.555065739179,39.1991005388149));
#49502=CARTESIAN_POINT('Ctrl Pts',(18.4538224294339,20.5595081723981,39.2536366313438));
#49503=CARTESIAN_POINT('Ctrl Pts',(18.4945164748564,20.5639509859394,39.3081773927745));
#49504=CARTESIAN_POINT('Ctrl Pts',(18.5380939413293,20.5683937994806,39.3605544462424));
#49505=CARTESIAN_POINT('Ctrl Pts',(18.5842877530733,20.5728366130219,39.410458465882));
#49506=CARTESIAN_POINT('Ctrl Pts',(18.6305313534035,20.5772842151138,39.4604162730418));
#49507=CARTESIAN_POINT('Ctrl Pts',(18.6793965899742,20.5817318172057,39.5078953655218));
#49508=CARTESIAN_POINT('Ctrl Pts',(18.7305789504475,20.5861794192976,39.5526227162801));
#49509=CARTESIAN_POINT('Ctrl Pts',(18.781793310398,20.5906298020533,39.5973780308101));
#49510=CARTESIAN_POINT('Ctrl Pts',(18.8353272890455,20.5950801848091,39.6393778759309));
#49511=CARTESIAN_POINT('Ctrl Pts',(18.8908448890875,20.5995305675649,39.6783907934465));
#49512=CARTESIAN_POINT('Ctrl Pts',(18.9464563730737,20.6039884762131,39.7174696843934));
#49513=CARTESIAN_POINT('Ctrl Pts',(19.004057754121,20.6084463848613,39.7535513079927));
#49514=CARTESIAN_POINT('Ctrl Pts',(19.063286648776,20.6129042935095,39.7864491259859));
#49515=CARTESIAN_POINT('Ctrl Pts',(19.0850374747073,20.6145413862763,39.7985303021899));
#49516=CARTESIAN_POINT('Ctrl Pts',(19.1070075813411,20.6161784790431,39.8101825734671));
#49517=CARTESIAN_POINT('Ctrl Pts',(19.129178373231,20.6178155718099,39.821398341829));
#49518=CARTESIAN_POINT('Ctrl Pts',(19.1895549429292,20.622273781784,39.851941663131));
#49519=CARTESIAN_POINT('Ctrl Pts',(19.25165968076,20.626731991758,39.8793650048683));
#49520=CARTESIAN_POINT('Ctrl Pts',(19.3151374153393,20.6311902017321,39.9034704868758));
#49521=CARTESIAN_POINT('Ctrl Pts',(19.3817897922614,20.6358713752737,39.9287815299257));
#49522=CARTESIAN_POINT('Ctrl Pts',(19.4499556611319,20.6405525488152,39.9504338143543));
#49523=CARTESIAN_POINT('Ctrl Pts',(19.5191943989729,20.6452337223567,39.9682528016628));
#49524=CARTESIAN_POINT('Ctrl Pts',(19.5849564745287,20.6496798416496,39.9851770499413));
#49525=CARTESIAN_POINT('Ctrl Pts',(19.6516857260476,20.6541259609425,39.998643539088));
#49526=CARTESIAN_POINT('Ctrl Pts',(19.7189863291311,20.6585720802353,40.008552821822));
#49527=CARTESIAN_POINT('Ctrl Pts',(19.7862463109997,20.663015515945,40.0184561235234));
#49528=CARTESIAN_POINT('Ctrl Pts',(19.8540764734469,20.6674589516547,40.024806406256));
#49529=CARTESIAN_POINT('Ctrl Pts',(19.9220710582345,20.6719023873644,40.0275553524958));
#49530=CARTESIAN_POINT('Ctrl Pts',(19.9900480394356,20.6763446726824,40.030303587042));
#49531=CARTESIAN_POINT('Ctrl Pts',(20.0581888658978,20.6807869580004,40.0294523163286));
#49532=CARTESIAN_POINT('Ctrl Pts',(20.1260847549693,20.6852292433183,40.0250052445291));
#49533=CARTESIAN_POINT('Ctrl Pts',(20.193986467695,20.6896719096658,40.0205577912895));
#49534=CARTESIAN_POINT('Ctrl Pts',(20.2616427094173,20.6941145760132,40.0125139596816));
#49535=CARTESIAN_POINT('Ctrl Pts',(20.3286486398796,20.6985572423607,40.0009294117366));
#49536=CARTESIAN_POINT('Ctrl Pts',(20.3957268230535,20.7030046992496,39.9893323721361));
#49537=CARTESIAN_POINT('Ctrl Pts',(20.4621528090275,20.7074521561386,39.9741870825268));
#49538=CARTESIAN_POINT('Ctrl Pts',(20.5275318296978,20.7118996130275,39.9556003679553));
#49539=CARTESIAN_POINT('Ctrl Pts',(20.5929517413555,20.7163498515565,39.9370020284144));
#49540=CARTESIAN_POINT('Ctrl Pts',(20.6573229182579,20.7208000900855,39.9149581406292));
#49541=CARTESIAN_POINT('Ctrl Pts',(20.7202683257296,20.7252503286145,39.8896245684083));
#49542=CARTESIAN_POINT('Ctrl Pts',(20.7833202210014,20.7297080958279,39.8642481381541));
#49543=CARTESIAN_POINT('Ctrl Pts',(20.8449410876416,20.7341658630414,39.8355711269434));
#49544=CARTESIAN_POINT('Ctrl Pts',(20.9047772110109,20.7386236302549,39.8037959840707));
#49545=CARTESIAN_POINT('Ctrl Pts',(20.9267672016582,20.7402618757462,39.792118504728));
#49546=CARTESIAN_POINT('Ctrl Pts',(20.9485164242748,20.7419001212376,39.7800230214307));
#49547=CARTESIAN_POINT('Ctrl Pts',(20.9700083480463,20.743538366729,39.7675210228421));
#49548=CARTESIAN_POINT('Ctrl Pts',(21.0284978130772,20.7479967904327,39.733497302256));
#49549=CARTESIAN_POINT('Ctrl Pts',(21.0853105251314,20.7524552141363,39.6963253160254));
#49550=CARTESIAN_POINT('Ctrl Pts',(21.1400871365967,20.75691363784,39.6561953212456));
#49551=CARTESIAN_POINT('Ctrl Pts',(21.1976001452084,20.7615947846653,39.6140606094842));
#49552=CARTESIAN_POINT('Ctrl Pts',(21.2528677787936,20.7662759314907,39.5686647970493));
#49553=CARTESIAN_POINT('Ctrl Pts',(21.3055038160382,20.770957078316,39.5202824871164));
#49554=CARTESIAN_POINT('Ctrl Pts',(21.3554995186628,20.7754034089456,39.4743271358719));
#49555=CARTESIAN_POINT('Ctrl Pts',(21.4031208630278,20.7798497395752,39.4256780713646));
#49556=CARTESIAN_POINT('Ctrl Pts',(21.4480689460585,20.7842960702048,39.3746132293213));
#49557=CARTESIAN_POINT('Ctrl Pts',(21.4929898863324,20.7887397158329,39.3235792237564));
#49558=CARTESIAN_POINT('Ctrl Pts',(21.5352404424524,20.793183361461,39.2701327039082));
#49559=CARTESIAN_POINT('Ctrl Pts',(21.574559195328,20.7976270070891,39.2145877701231));
#49560=CARTESIAN_POINT('Ctrl Pts',(21.6138677539025,20.8020695005987,39.159057237654));
#49561=CARTESIAN_POINT('Ctrl Pts',(21.6502457336331,20.8065119941083,39.1014297737565));
#49562=CARTESIAN_POINT('Ctrl Pts',(21.683473708243,20.8109544876179,39.0420503333446));
#49563=CARTESIAN_POINT('Ctrl Pts',(21.7167045175562,20.8153973601199,38.9826658272283));
#49564=CARTESIAN_POINT('Ctrl Pts',(21.7467845498965,20.8198402326219,38.9215294795391));
#49565=CARTESIAN_POINT('Ctrl Pts',(21.773540110251,20.824283105124,38.859011221413));
#49566=CARTESIAN_POINT('Ctrl Pts',(21.8003244937898,20.8287307638361,38.7964256137247));
#49567=CARTESIAN_POINT('Ctrl Pts',(21.8237770651948,20.8331784225482,38.7324555793768));
#49568=CARTESIAN_POINT('Ctrl Pts',(21.8437725306241,20.8376260812604,38.6674904512114));
#49569=CARTESIAN_POINT('Ctrl Pts',(21.8637804913952,20.8420765193535,38.6024847257673));
#49570=CARTESIAN_POINT('Ctrl Pts',(21.8803269274325,20.8465269574466,38.5364831473164));
#49571=CARTESIAN_POINT('Ctrl Pts',(21.8933373342609,20.8509773955397,38.4698868686421));
#49572=CARTESIAN_POINT('Ctrl Pts',(21.9063697352151,20.8554353571097,38.403178008789));
#49573=CARTESIAN_POINT('Ctrl Pts',(21.9158541111529,20.8598933186797,38.3358729304174));
#49574=CARTESIAN_POINT('Ctrl Pts',(21.9217677302915,20.8643512802497,38.2683785844767));
#49575=CARTESIAN_POINT('Ctrl Pts',(21.9239387650532,20.8659879073825,38.2435997531337));
#49576=CARTESIAN_POINT('Ctrl Pts',(21.9256290393793,20.8676245345153,38.2187954115716));
#49577=CARTESIAN_POINT('Ctrl Pts',(21.926839188957,20.8692611616481,38.1939856201742));
#49578=CARTESIAN_POINT('Ctrl Pts',(21.9301359006187,20.8737196912827,38.1263983316863));
#49579=CARTESIAN_POINT('Ctrl Pts',(21.9298786981062,20.8781782209172,38.0585039674556));
#49580=CARTESIAN_POINT('Ctrl Pts',(21.9260315986928,20.8826367505517,37.990707558648));
#49581=CARTESIAN_POINT('Ctrl Pts',(21.9219924226099,20.8873178841357,37.9195262338265));
#49582=CARTESIAN_POINT('Ctrl Pts',(21.9139953705416,20.8919990177197,37.8484534371793));
#49583=CARTESIAN_POINT('Ctrl Pts',(21.902060588042,20.8966801513037,37.777962616584));
#49584=CARTESIAN_POINT('Ctrl Pts',(21.8907241608886,20.9011265942843,37.711005882962));
#49585=CARTESIAN_POINT('Ctrl Pts',(21.8758354328192,20.9055730372648,37.6445747319696));
#49586=CARTESIAN_POINT('Ctrl Pts',(21.8574648725121,20.9100194802454,37.5790712099684));
#49587=CARTESIAN_POINT('Ctrl Pts',(21.8391053969685,20.9144632402502,37.5136072126764));
#49588=CARTESIAN_POINT('Ctrl Pts',(21.8172683897229,20.9189070002549,37.4490702078103));
#49589=CARTESIAN_POINT('Ctrl Pts',(21.792075060108,20.9233507602597,37.3858504807543));
#49590=CARTESIAN_POINT('Ctrl Pts',(21.7668882518946,20.9277933699781,37.322647118396));
#49591=CARTESIAN_POINT('Ctrl Pts',(21.7383470287057,20.9322359796965,37.2607608147207));
#49592=CARTESIAN_POINT('Ctrl Pts',(21.7066213401951,20.9366785894149,37.2005634218631));
#49593=CARTESIAN_POINT('Ctrl Pts',(21.6748929334973,20.9411215797663,37.1403608714253));
#49594=CARTESIAN_POINT('Ctrl Pts',(21.6399797521761,20.9455645701177,37.0818479539657));
#49595=CARTESIAN_POINT('Ctrl Pts',(21.6020975899296,20.9500075604692,37.0253717530039));
#49596=CARTESIAN_POINT('Ctrl Pts',(21.5641746049835,20.9544553386904,36.9688346919739));
#49597=CARTESIAN_POINT('Ctrl Pts',(21.5232765305345,20.9589031169116,36.914339136874));
#49598=CARTESIAN_POINT('Ctrl Pts',(21.4796617814511,20.9633508951328,36.8622021290158));
#49599=CARTESIAN_POINT('Ctrl Pts',(21.4360197670868,20.9678014538337,36.8100325282804));
#49600=CARTESIAN_POINT('Ctrl Pts',(21.3896580345579,20.9722520125346,36.7602247695383));
#49601=CARTESIAN_POINT('Ctrl Pts',(21.3408725598251,20.9767025712355,36.7130597218308));
#49602=CARTESIAN_POINT('Ctrl Pts',(21.2920046098859,20.9811606539125,36.6658149383605));
#49603=CARTESIAN_POINT('Ctrl Pts',(21.2407051137358,20.9856187365895,36.6212221032468));
#49604=CARTESIAN_POINT('Ctrl Pts',(21.1873030923581,20.9900768192665,36.5795218108185));
#49605=CARTESIAN_POINT('Ctrl Pts',(21.167709388815,20.9917125317001,36.5642215816057));
#49606=CARTESIAN_POINT('Ctrl Pts',(21.147832913589,20.9933482441336,36.5493103278902));
#49607=CARTESIAN_POINT('Ctrl Pts',(21.1276908112208,20.9949839565672,36.5347984183536));
#49608=CARTESIAN_POINT('Ctrl Pts',(21.0727993548713,20.9994416162496,36.4952504191275));
#49609=CARTESIAN_POINT('Ctrl Pts',(21.0157162941417,21.003899275932,36.4585151822182));
#49610=CARTESIAN_POINT('Ctrl Pts',(20.9567616502993,21.0083569356144,36.4248433800338));
#49611=CARTESIAN_POINT('Ctrl Pts',(20.8979095980615,21.0128068381733,36.3912301727961));
#49612=CARTESIAN_POINT('Ctrl Pts',(20.8371928576362,21.0172567407321,36.3606700527017));
#49613=CARTESIAN_POINT('Ctrl Pts',(20.7749613541135,21.0217066432909,36.3333711605064));
#49614=CARTESIAN_POINT('Ctrl Pts',(20.7127908879904,21.0261521813323,36.3060990433896));
#49615=CARTESIAN_POINT('Ctrl Pts',(20.6491090545898,21.0305977193737,36.2820820077792));
#49616=CARTESIAN_POINT('Ctrl Pts',(20.5842901976383,21.0350432574151,36.2614822487004));
#49617=CARTESIAN_POINT('Ctrl Pts',(20.519512553486,21.0394859689169,36.2408955872566));
#49618=CARTESIAN_POINT('Ctrl Pts',(20.4535997892027,21.0439286804187,36.2237220405848));
#49619=CARTESIAN_POINT('Ctrl Pts',(20.3869443306759,21.0483713919205,36.2100749639582));
#49620=CARTESIAN_POINT('Ctrl Pts',(20.3203082581246,21.0528128113106,36.1964318564272));
#49621=CARTESIAN_POINT('Ctrl Pts',(20.2529304033284,21.0572542307007,36.1863132808701));
#49622=CARTESIAN_POINT('Ctrl Pts',(20.1852145989036,21.0616956500908,36.1797817547859));
#49623=CARTESIAN_POINT('Ctrl Pts',(20.1174534960788,21.0661400405627,36.1732458594458));
#49624=CARTESIAN_POINT('Ctrl Pts',(20.0493544834623,21.0705844310346,36.1703018605945));
#49625=CARTESIAN_POINT('Ctrl Pts',(19.9813266676957,21.0750288215065,36.1709603779184));
#49626=CARTESIAN_POINT('Ctrl Pts',(19.9132787554393,21.0794745249214,36.1716190897788));
#49627=CARTESIAN_POINT('Ctrl Pts',(19.845302575557,21.0839202283363,36.1758824135838));
#49628=CARTESIAN_POINT('Ctrl Pts',(19.7778046531292,21.0883659317512,36.1837088465661));
#49629=CARTESIAN_POINT('Ctrl Pts',(19.7101977872644,21.0928188106494,36.1915479116188));
#49630=CARTESIAN_POINT('Ctrl Pts',(19.6430712100821,21.0972716895475,36.2029614995978));
#49631=CARTESIAN_POINT('Ctrl Pts',(19.5768230943422,21.1017245684457,36.2178565773518));
#49632=CARTESIAN_POINT('Ctrl Pts',(19.5150496424909,21.1058766820136,36.2317455817134));
#49633=CARTESIAN_POINT('Ctrl Pts',(19.4540401875754,21.1100287955816,36.2486610432304));
#49634=CARTESIAN_POINT('Ctrl Pts',(19.3941040087494,21.1141809091495,36.2684889831927));
#49635=CARTESIAN_POINT('Origin',(20.,-0.075,38.1));
#49636=CARTESIAN_POINT('',(17.6365301745119,0.384026849772126,38.099091756019));
#49637=CARTESIAN_POINT('',(21.0904144288932,0.125000000000002,36.00310066666));
#49638=CARTESIAN_POINT('Ctrl Pts',(17.6365301745122,0.384026849728286,38.0990917552036));
#49639=CARTESIAN_POINT('Ctrl Pts',(17.6365466202516,0.381726187737689,38.056296014461));
#49640=CARTESIAN_POINT('Ctrl Pts',(17.6377253551942,0.379425525747093,38.0135219170556));
#49641=CARTESIAN_POINT('Ctrl Pts',(17.6400633130001,0.377124863756497,37.9708130259966));
#49642=CARTESIAN_POINT('Ctrl Pts',(17.6443776509738,0.372879349416942,37.8920004015614));
#49643=CARTESIAN_POINT('Ctrl Pts',(17.6526523098677,0.368633835077388,37.8132585686871));
#49644=CARTESIAN_POINT('Ctrl Pts',(17.6648817042177,0.364388320737833,37.7350164584497));
#49645=CARTESIAN_POINT('Ctrl Pts',(17.6770934799562,0.360148922814607,37.6568870698479));
#49646=CARTESIAN_POINT('Ctrl Pts',(17.6932486037894,0.355909524891381,37.5792564315695));
#49647=CARTESIAN_POINT('Ctrl Pts',(17.7132895602032,0.351670126968155,37.5025505833759));
#49648=CARTESIAN_POINT('Ctrl Pts',(17.7333070781187,0.34743568714769,37.4259344449676));
#49649=CARTESIAN_POINT('Ctrl Pts',(17.7572012787173,0.343201247327225,37.3502413964795));
#49650=CARTESIAN_POINT('Ctrl Pts',(17.7848634742222,0.33896680750676,37.2758879851228));
#49651=CARTESIAN_POINT('Ctrl Pts',(17.8125079350198,0.334735082458186,37.2015822430116));
#49652=CARTESIAN_POINT('Ctrl Pts',(17.8439154327941,0.330503357409613,37.1286148695029));
#49653=CARTESIAN_POINT('Ctrl Pts',(17.8789276000118,0.32627163236104,37.0573867855681));
#49654=CARTESIAN_POINT('Ctrl Pts',(17.9139281139794,0.322041315775697,36.9861824087825));
#49655=CARTESIAN_POINT('Ctrl Pts',(17.952530708808,0.317810999190353,36.9167165905492));
#49656=CARTESIAN_POINT('Ctrl Pts',(17.9945296831701,0.31358068260501,36.8493684598515));
#49657=CARTESIAN_POINT('Ctrl Pts',(18.0365276259034,0.309350469929734,36.7820219834388));
#49658=CARTESIAN_POINT('Ctrl Pts',(18.081921534115,0.305120257254458,36.7167934865995));
#49659=CARTESIAN_POINT('Ctrl Pts',(18.1304614998172,0.300890044579181,36.6540344965268));
#49660=CARTESIAN_POINT('Ctrl Pts',(18.1790478208794,0.296655792077581,36.591215572016));
#49661=CARTESIAN_POINT('Ctrl Pts',(18.2307859149217,0.292421539575981,36.5308712355465));
#49662=CARTESIAN_POINT('Ctrl Pts',(18.28538492457,0.28818728707438,36.4733206880248));
#49663=CARTESIAN_POINT('Ctrl Pts',(18.3400093704208,0.283951061949012,36.4157433292588));
#49664=CARTESIAN_POINT('Ctrl Pts',(18.3974970493029,0.279714836823644,36.3609626755641));
#49665=CARTESIAN_POINT('Ctrl Pts',(18.4575213005469,0.275478611698276,36.3092599567125));
#49666=CARTESIAN_POINT('Ctrl Pts',(18.5176502304147,0.271234998855322,36.2574670714806));
#49667=CARTESIAN_POINT('Ctrl Pts',(18.5803242023937,0.266991386012368,36.2087631341215));
#49668=CARTESIAN_POINT('Ctrl Pts',(18.645184842545,0.262747773169415,36.1633879247433));
#49669=CARTESIAN_POINT('Ctrl Pts',(18.7029885484259,0.258965871725414,36.1229496057401));
#49670=CARTESIAN_POINT('Ctrl Pts',(18.7625283691001,0.255183970281414,36.0851545808996));
#49671=CARTESIAN_POINT('Ctrl Pts',(18.8235345245485,0.251402068837414,36.0501416083128));
#49672=CARTESIAN_POINT('Ctrl Pts',(18.8919721557191,0.247159474393527,36.0108635242166));
#49673=CARTESIAN_POINT('Ctrl Pts',(18.962503989743,0.242916879949641,35.9749447688772));
#49674=CARTESIAN_POINT('Ctrl Pts',(19.0347671401997,0.238674285505754,35.9426136258746));
#49675=CARTESIAN_POINT('Ctrl Pts',(19.1069281207725,0.234437689490933,35.91032819454));
#49676=CARTESIAN_POINT('Ctrl Pts',(19.1808151329091,0.230201093476113,35.8816204907315));
#49677=CARTESIAN_POINT('Ctrl Pts',(19.2560395078073,0.225964497461293,35.8566736245129));
#49678=CARTESIAN_POINT('Ctrl Pts',(19.3311791878672,0.221732671413845,35.8317548458762));
#49679=CARTESIAN_POINT('Ctrl Pts',(19.4076527967903,0.217500845366396,35.8105886361722));
#49680=CARTESIAN_POINT('Ctrl Pts',(19.4850518236164,0.213269019318948,35.7933099868992));
#49681=CARTESIAN_POINT('Ctrl Pts',(19.5624033121621,0.209039792448016,35.7760419501274));
#49682=CARTESIAN_POINT('Ctrl Pts',(19.6406786352875,0.204810565577084,35.7626568355487));
#49683=CARTESIAN_POINT('Ctrl Pts',(19.7194554280259,0.200581338706152,35.7532394276288));
#49684=CARTESIAN_POINT('Ctrl Pts',(19.7982081837649,0.19635340229044,35.7438248932231));
#49685=CARTESIAN_POINT('Ctrl Pts',(19.8774616414621,0.192125465874728,35.7383757165539));
#49686=CARTESIAN_POINT('Ctrl Pts',(19.9567860404826,0.187897529459016,35.7369250975471));
#49687=CARTESIAN_POINT('Ctrl Pts',(20.036110751376,0.183669576420693,35.735474472837));
#49688=CARTESIAN_POINT('Ctrl Pts',(20.1155059368129,0.179441623382369,35.7380224440605));
#49689=CARTESIAN_POINT('Ctrl Pts',(20.1945410240051,0.175213670344046,35.7445501001127));
#49690=CARTESIAN_POINT('Ctrl Pts',(20.2736554109043,0.170981475196947,35.7510843056764));
#49691=CARTESIAN_POINT('Ctrl Pts',(20.3524085109971,0.166749280049848,35.7616061333742));
#49692=CARTESIAN_POINT('Ctrl Pts',(20.4303746581921,0.162517084902749,35.7760447305325));
#49693=CARTESIAN_POINT('Ctrl Pts',(20.5083791304018,0.158282809379141,35.7904904251229));
#49694=CARTESIAN_POINT('Ctrl Pts',(20.5855954237906,0.154048533855532,35.808856616531));
#49695=CARTESIAN_POINT('Ctrl Pts',(20.6616103489271,0.149814258331924,35.8310217746544));
#49696=CARTESIAN_POINT('Ctrl Pts',(20.7377615202967,0.145572393455453,35.8532266607561));
#49697=CARTESIAN_POINT('Ctrl Pts',(20.8127065783469,0.141330528578983,35.8792439652926));
#49698=CARTESIAN_POINT('Ctrl Pts',(20.8860499319902,0.137088663702512,35.908903023844));
#49699=CARTESIAN_POINT('Ctrl Pts',(20.951807402204,0.133285533774455,35.9354944539106));
#49700=CARTESIAN_POINT('Ctrl Pts',(21.0162774292693,0.129482403846397,35.9650124980401));
#49701=CARTESIAN_POINT('Ctrl Pts',(21.0791925799285,0.125679273918339,35.9973032039005));
#49702=CARTESIAN_POINT('Ctrl Pts',(21.0829383210873,0.125452849278894,35.9992256760669));
#49703=CARTESIAN_POINT('Ctrl Pts',(21.0866789488293,0.125226424639448,36.0011581693281));
#49704=CARTESIAN_POINT('Ctrl Pts',(21.0904144288932,0.125000000000002,36.0031006666601));
#49705=CARTESIAN_POINT('',(18.9094067387628,0.125,36.0031936714508));
#49706=CARTESIAN_POINT('Origin',(20.,0.125,38.1));
#49707=CARTESIAN_POINT('',(17.6361271868254,0.262848150271721,38.0978834451601));
#49708=CARTESIAN_POINT('Ctrl Pts',(18.9094067387628,0.124999999999998,36.0031936714508));
#49709=CARTESIAN_POINT('Ctrl Pts',(18.2138265225729,0.166907598306358,36.3649796342733));
#49710=CARTESIAN_POINT('Ctrl Pts',(17.6705484964577,0.212856981730266,37.1675355659372));
#49711=CARTESIAN_POINT('Ctrl Pts',(17.6334287363114,0.258806365154173,38.0226003826317));
#49712=CARTESIAN_POINT('Ctrl Pts',(17.6339392807276,0.262848150271721,38.0978814861616));
#49713=CARTESIAN_POINT('',(17.6365302632328,1.05659815022249,38.098884524413));
#49714=CARTESIAN_POINT('Ctrl Pts',(17.6365309473941,0.262848150271721,38.0978838066776));
#49715=CARTESIAN_POINT('Ctrl Pts',(17.6364618825206,0.26699404237924,38.175018863043));
#49716=CARTESIAN_POINT('Ctrl Pts',(17.6401730751359,0.271139934486759,38.2523306584864));
#49717=CARTESIAN_POINT('Ctrl Pts',(17.647689911148,0.275285826594278,38.3294072509425));
#49718=CARTESIAN_POINT('Ctrl Pts',(17.6553320274445,0.279500816729439,38.4077684500353));
#49719=CARTESIAN_POINT('Ctrl Pts',(17.6669078983962,0.283715806864601,38.4858860293951));
#49720=CARTESIAN_POINT('Ctrl Pts',(17.682388929481,0.287930796999763,38.5633242565501));
#49721=CARTESIAN_POINT('Ctrl Pts',(17.6975783227697,0.292066383481074,38.6393036717064));
#49722=CARTESIAN_POINT('Ctrl Pts',(17.7165269305249,0.296201969962385,38.7146286024622));
#49723=CARTESIAN_POINT('Ctrl Pts',(17.7391554804501,0.300337556443697,38.7888922262019));
#49724=CARTESIAN_POINT('Ctrl Pts',(17.7617717581082,0.304470900049416,38.8631155741379));
#49725=CARTESIAN_POINT('Ctrl Pts',(17.7880638787022,0.308604243655135,38.9362782884214));
#49726=CARTESIAN_POINT('Ctrl Pts',(17.8179020386913,0.312737587260854,39.0079861938116));
#49727=CARTESIAN_POINT('Ctrl Pts',(17.8477341671462,0.316870095345768,39.0796796040492));
#49728=CARTESIAN_POINT('Ctrl Pts',(17.8811107239061,0.321002603430683,39.1499183368414));
#49729=CARTESIAN_POINT('Ctrl Pts',(17.9178534771978,0.325135111515597,39.2183274558388));
#49730=CARTESIAN_POINT('Ctrl Pts',(17.955870911315,0.329410984709144,39.2891098262793));
#49731=CARTESIAN_POINT('Ctrl Pts',(17.9974921636746,0.333686857902691,39.3579327945156));
#49732=CARTESIAN_POINT('Ctrl Pts',(18.0424687398505,0.337962731096238,39.4244099842713));
#49733=CARTESIAN_POINT('Ctrl Pts',(18.085990774814,0.342100322670602,39.4887373035743));
#49734=CARTESIAN_POINT('Ctrl Pts',(18.1326540628943,0.346237914244966,39.5508678940322));
#49735=CARTESIAN_POINT('Ctrl Pts',(18.1821914387838,0.350375505819329,39.6104841858388));
#49736=CARTESIAN_POINT('Ctrl Pts',(18.234212182748,0.354720519822468,39.6730891138649));
#49737=CARTESIAN_POINT('Ctrl Pts',(18.2894023108564,0.359065533825606,39.7329205901025));
#49738=CARTESIAN_POINT('Ctrl Pts',(18.3474095171519,0.363410547828744,39.7896553307997));
#49739=CARTESIAN_POINT('Ctrl Pts',(18.4054167234473,0.367755561831882,39.8463900714969));
#49740=CARTESIAN_POINT('Ctrl Pts',(18.466240487423,0.372100575835021,39.9000277367094));
#49741=CARTESIAN_POINT('Ctrl Pts',(18.5294918301591,0.376445589838159,39.9502962366419));
#49742=CARTESIAN_POINT('Ctrl Pts',(18.5912586311502,0.380688624114211,39.9993849088683));
#49743=CARTESIAN_POINT('Ctrl Pts',(18.6556004960446,0.384931658390263,40.0454682312156));
#49744=CARTESIAN_POINT('Ctrl Pts',(18.7221932971537,0.389174692666315,40.0882656942826));
#49745=CARTESIAN_POINT('Ctrl Pts',(18.788690404912,0.39341162973425,40.1310016577194));
#49746=CARTESIAN_POINT('Ctrl Pts',(18.857431634827,0.397648566802186,40.1704608889279));
#49747=CARTESIAN_POINT('Ctrl Pts',(18.9280605298275,0.401885503870121,40.2064036206735));
#49748=CARTESIAN_POINT('Ctrl Pts',(18.9986074118953,0.406117521087132,40.2423046164009));
#49749=CARTESIAN_POINT('Ctrl Pts',(19.0710371882806,0.410349538304143,40.2746970170407));
#49750=CARTESIAN_POINT('Ctrl Pts',(19.1449665116178,0.414581555521154,40.3033856164196));
#49751=CARTESIAN_POINT('Ctrl Pts',(19.2188488338598,0.418810882203,40.3320559768166));
#49752=CARTESIAN_POINT('Ctrl Pts',(19.2942283760049,0.423040208884845,40.3570270416089));
#49753=CARTESIAN_POINT('Ctrl Pts',(19.3707004875316,0.427269535566691,40.3781511285486));
#49754=CARTESIAN_POINT('Ctrl Pts',(19.4471476170331,0.431497480605695,40.3992683146395));
#49755=CARTESIAN_POINT('Ctrl Pts',(19.5246861569039,0.435725425644699,40.416540894387));
#49756=CARTESIAN_POINT('Ctrl Pts',(19.6028963277898,0.439953370683703,40.4298710510278));
#49757=CARTESIAN_POINT('Ctrl Pts',(19.6811051208929,0.444181241241473,40.443200972839));
#49758=CARTESIAN_POINT('Ctrl Pts',(19.7599850605302,0.448409111799243,40.4525885324591));
#49759=CARTESIAN_POINT('Ctrl Pts',(19.8391076657526,0.452636982357013,40.457987298032));
#49760=CARTESIAN_POINT('Ctrl Pts',(19.9183070009431,0.456868952936158,40.4633912991139));
#49761=CARTESIAN_POINT('Ctrl Pts',(19.9977490044459,0.461100923515304,40.4647987472846));
#49762=CARTESIAN_POINT('Ctrl Pts',(20.077002187465,0.465332894094449,40.4622152958665));
#49763=CARTESIAN_POINT('Ctrl Pts',(20.1562928650638,0.469566866813471,40.4596306222208));
#49764=CARTESIAN_POINT('Ctrl Pts',(20.2353940777908,0.473800839532493,40.4530513257599));
#49765=CARTESIAN_POINT('Ctrl Pts',(20.3138789833638,0.478034812251516,40.4425350423638));
#49766=CARTESIAN_POINT('Ctrl Pts',(20.3925021979024,0.482276246231814,40.4320002267893));
#49767=CARTESIAN_POINT('Ctrl Pts',(20.4705064744765,0.486517680212112,40.4175146466936));
#49768=CARTESIAN_POINT('Ctrl Pts',(20.5474749282159,0.49075911419241,40.3991871702571));
#49769=CARTESIAN_POINT('Ctrl Pts',(20.616488844873,0.494562204380686,40.382753802171));
#49770=CARTESIAN_POINT('Ctrl Pts',(20.6846699260661,0.498365294568962,40.3632323758914));
#49771=CARTESIAN_POINT('Ctrl Pts',(20.7517303997312,0.502168384757237,40.3407346668046));
#49772=CARTESIAN_POINT('Ctrl Pts',(20.826578481796,0.506413120753787,40.3156243404981));
#49773=CARTESIAN_POINT('Ctrl Pts',(20.9003021434443,0.510657856750337,40.286714333335));
#49774=CARTESIAN_POINT('Ctrl Pts',(20.9724895378996,0.514902592746886,40.2541250055593));
#49775=CARTESIAN_POINT('Ctrl Pts',(21.0445757922291,0.51914138153983,40.2215813379537));
#49776=CARTESIAN_POINT('Ctrl Pts',(21.1151296321602,0.523380170332774,40.1853687790023));
#49777=CARTESIAN_POINT('Ctrl Pts',(21.1837559386883,0.527618959125719,40.1456569405744));
#49778=CARTESIAN_POINT('Ctrl Pts',(21.2523061311334,0.531853046638082,40.1059891469206));
#49779=CARTESIAN_POINT('Ctrl Pts',(21.3189326366379,0.536087134150445,40.0628300196778));
#49780=CARTESIAN_POINT('Ctrl Pts',(21.3832631957482,0.540321221662809,40.0163959330442));
#49781=CARTESIAN_POINT('Ctrl Pts',(21.4475548872188,0.544552750997682,39.9699899012477));
#49782=CARTESIAN_POINT('Ctrl Pts',(21.5095530083465,0.548784280332555,39.9203131106354));
#49783=CARTESIAN_POINT('Ctrl Pts',(21.5689136943686,0.553015809667429,39.8676255996456));
#49784=CARTESIAN_POINT('Ctrl Pts',(21.6282568153375,0.557246086876645,39.8149536790911));
#49785=CARTESIAN_POINT('Ctrl Pts',(21.6849637021973,0.561476364085862,39.7592731172668));
#49786=CARTESIAN_POINT('Ctrl Pts',(21.738724193471,0.565706641295079,39.7008836996918));
#49787=CARTESIAN_POINT('Ctrl Pts',(21.7924853496532,0.569936970824267,39.6424935599577));
#49788=CARTESIAN_POINT('Ctrl Pts',(21.8432997227037,0.574167300353455,39.5813948424348));
#49789=CARTESIAN_POINT('Ctrl Pts',(21.8908956101143,0.578397629882643,39.5179225058339));
#49790=CARTESIAN_POINT('Ctrl Pts',(21.9385396920706,0.582632242950196,39.4543858985452));
#49791=CARTESIAN_POINT('Ctrl Pts',(21.982958498106,0.586866856017749,39.3884712458543));
#49792=CARTESIAN_POINT('Ctrl Pts',(22.0239224456132,0.591101469085302,39.3205442945847));
#49793=CARTESIAN_POINT('Ctrl Pts',(22.0649067739001,0.595338188998541,39.2525835476406));
#49794=CARTESIAN_POINT('Ctrl Pts',(22.1024325983729,0.59957490891178,39.1826089195754));
#49795=CARTESIAN_POINT('Ctrl Pts',(22.1363165313248,0.603811628825019,39.1110104445001));
#49796=CARTESIAN_POINT('Ctrl Pts',(22.1702613067429,0.608055956252082,39.0392834061967));
#49797=CARTESIAN_POINT('Ctrl Pts',(22.2005509456261,0.612300283679145,38.9659271274026));
#49798=CARTESIAN_POINT('Ctrl Pts',(22.2270504962148,0.616544611106208,38.8913510777206));
#49799=CARTESIAN_POINT('Ctrl Pts',(22.250664678752,0.620326800629578,38.8248951412623));
#49800=CARTESIAN_POINT('Ctrl Pts',(22.2712698413409,0.624108990152948,38.7574710555183));
#49801=CARTESIAN_POINT('Ctrl Pts',(22.2888046377453,0.627891179676317,38.6893757469861));
#49802=CARTESIAN_POINT('Ctrl Pts',(22.3084266942537,0.632123583340497,38.6131746916016));
#49803=CARTESIAN_POINT('Ctrl Pts',(22.324276863283,0.636355987004676,38.5358461616176));
#49804=CARTESIAN_POINT('Ctrl Pts',(22.3362300683726,0.640588390668856,38.4577981393634));
#49805=CARTESIAN_POINT('Ctrl Pts',(22.348165852922,0.644814626049535,38.3798638638985));
#49806=CARTESIAN_POINT('Ctrl Pts',(22.3562158807938,0.649040861430213,38.3012126390911));
#49807=CARTESIAN_POINT('Ctrl Pts',(22.3603053973195,0.653267096810892,38.2222655809483));
#49808=CARTESIAN_POINT('Ctrl Pts',(22.3643901000154,0.657488357428077,38.1434114525425));
#49809=CARTESIAN_POINT('Ctrl Pts',(22.364523531154,0.661709618045262,38.0642626498012));
#49810=CARTESIAN_POINT('Ctrl Pts',(22.3606825622673,0.665930878662447,37.9852468688568));
#49811=CARTESIAN_POINT('Ctrl Pts',(22.3568440671912,0.670149420538699,37.906281978738));
#49812=CARTESIAN_POINT('Ctrl Pts',(22.349036275205,0.674367962414951,37.8274504086583));
#49813=CARTESIAN_POINT('Ctrl Pts',(22.3372881366587,0.678586504291203,37.7491800930187));
#49814=CARTESIAN_POINT('Ctrl Pts',(22.3255438813021,0.682803651785012,37.6709356485823));
#49815=CARTESIAN_POINT('Ctrl Pts',(22.309861935233,0.68702079927882,37.5932525547799));
#49816=CARTESIAN_POINT('Ctrl Pts',(22.2903229652327,0.691237946772629,37.5165523538245));
#49817=CARTESIAN_POINT('Ctrl Pts',(22.2707843277844,0.695455022490872,37.4398534583013));
#49818=CARTESIAN_POINT('Ctrl Pts',(22.2473889142856,0.699672098209116,37.3641378776005));
#49819=CARTESIAN_POINT('Ctrl Pts',(22.2202678816469,0.703889173927359,37.289814234495));
#49820=CARTESIAN_POINT('Ctrl Pts',(22.1931199610293,0.708110430483589,37.2154169064164));
#49821=CARTESIAN_POINT('Ctrl Pts',(22.1622392046997,0.71233168703982,37.1424147151563));
#49822=CARTESIAN_POINT('Ctrl Pts',(22.1278055815535,0.71655294359605,37.0711978576958));
#49823=CARTESIAN_POINT('Ctrl Pts',(22.0933554042309,0.720776229547382,36.9999467622923));
#49824=CARTESIAN_POINT('Ctrl Pts',(22.0553491836034,0.724999515498714,36.9304831233829));
#49825=CARTESIAN_POINT('Ctrl Pts',(22.0140124684469,0.729222801450046,36.8631717104463));
#49826=CARTESIAN_POINT('Ctrl Pts',(21.9726010402798,0.733453720673798,36.7957386371821));
#49827=CARTESIAN_POINT('Ctrl Pts',(21.9278473563894,0.737684639897551,36.7304659510557));
#49828=CARTESIAN_POINT('Ctrl Pts',(21.8800196967714,0.741915559121303,36.6676884484681));
#49829=CARTESIAN_POINT('Ctrl Pts',(21.8359388242095,0.745815030946001,36.6098288936955));
#49830=CARTESIAN_POINT('Ctrl Pts',(21.7892473922436,0.749714502770699,36.5540887381423));
#49831=CARTESIAN_POINT('Ctrl Pts',(21.7401831006425,0.753613974595397,36.5007022737657));
#49832=CARTESIAN_POINT('Ctrl Pts',(21.6868504876868,0.757852678849993,36.4426714829653));
#49833=CARTESIAN_POINT('Ctrl Pts',(21.6305121517996,0.762091383104589,36.3872028090615));
#49834=CARTESIAN_POINT('Ctrl Pts',(21.5714438914437,0.766330087359185,36.3346234008167));
#49835=CARTESIAN_POINT('Ctrl Pts',(21.5124604928476,0.770562701982907,36.2821195319746));
#49836=CARTESIAN_POINT('Ctrl Pts',(21.4507553057172,0.774795316606628,36.2324969942412));
#49837=CARTESIAN_POINT('Ctrl Pts',(21.3866424318643,0.779027931230349,36.1860477521491));
#49838=CARTESIAN_POINT('Ctrl Pts',(21.3226035729714,0.783255659521835,36.1396521332779));
#49839=CARTESIAN_POINT('Ctrl Pts',(21.2561629285916,0.787483387813321,36.096422803308));
#49840=CARTESIAN_POINT('Ctrl Pts',(21.1876681226633,0.791711116104807,36.0566119136812));
#49841=CARTESIAN_POINT('Ctrl Pts',(21.1192165382217,0.79593617662171,36.0168261454606));
#49842=CARTESIAN_POINT('Ctrl Pts',(21.0487137691173,0.800161237138613,35.980454770714));
#49843=CARTESIAN_POINT('Ctrl Pts',(20.9765358888945,0.804386297655516,35.9477063168329));
#49844=CARTESIAN_POINT('Ctrl Pts',(20.9043811128216,0.808610005729933,35.9149683457366));
#49845=CARTESIAN_POINT('Ctrl Pts',(20.8305527167774,0.81283371380435,35.8858511859687));
#49846=CARTESIAN_POINT('Ctrl Pts',(20.7554494762376,0.817057421878768,35.8605164591468));
#49847=CARTESIAN_POINT('Ctrl Pts',(20.6803469258958,0.82128109113735,35.8351819651508));
#49848=CARTESIAN_POINT('Ctrl Pts',(20.603969998732,0.825504760395932,35.8136299833845));
#49849=CARTESIAN_POINT('Ctrl Pts',(20.5267340449842,0.829728429654514,35.7959727243901));
#49850=CARTESIAN_POINT('Ctrl Pts',(20.4494215288891,0.833956285746006,35.7782979621328));
#49851=CARTESIAN_POINT('Ctrl Pts',(20.3712487430369,0.838184141837497,35.7645257392072));
#49852=CARTESIAN_POINT('Ctrl Pts',(20.292642094316,0.842411997928989,35.7547172781231));
#49853=CARTESIAN_POINT('Ctrl Pts',(20.2139974548782,0.846641897349977,35.7449040765943));
#49854=CARTESIAN_POINT('Ctrl Pts',(20.1349190026683,0.850871796770964,35.7390584878856));
#49855=CARTESIAN_POINT('Ctrl Pts',(20.0558365932587,0.855101696191952,35.7371896572612));
#49856=CARTESIAN_POINT('Ctrl Pts',(19.9766124765105,0.85933917514667,35.7353174778894));
#49857=CARTESIAN_POINT('Ctrl Pts',(19.8973848578431,0.863576654101389,35.7374362824276));
#49858=CARTESIAN_POINT('Ctrl Pts',(19.8185816833028,0.867814133056107,35.7435030585068));
#49859=CARTESIAN_POINT('Ctrl Pts',(19.7471539671461,0.871655011875563,35.749002024282));
#49860=CARTESIAN_POINT('Ctrl Pts',(19.6760751522037,0.87549589069502,35.7577438284633));
#49861=CARTESIAN_POINT('Ctrl Pts',(19.6056561338333,0.879336769514476,35.7696602487799));
#49862=CARTESIAN_POINT('Ctrl Pts',(19.5279481238012,0.883575213286357,35.7828101240683));
#49863=CARTESIAN_POINT('Ctrl Pts',(19.450753377928,0.887813657058239,35.7998757220939));
#49864=CARTESIAN_POINT('Ctrl Pts',(19.3744964180902,0.89205210083012,35.8208037140435));
#49865=CARTESIAN_POINT('Ctrl Pts',(19.2983487787586,0.896284468450797,35.8417017040277));
#49866=CARTESIAN_POINT('Ctrl Pts',(19.223136703738,0.900516836071473,35.8664509687147));
#49867=CARTESIAN_POINT('Ctrl Pts',(19.1492760415994,0.904749203692149,35.8949468968972));
#49868=CARTESIAN_POINT('Ctrl Pts',(19.0755002743758,0.908976706659862,35.9234100720644));
#49869=CARTESIAN_POINT('Ctrl Pts',(19.003073268172,0.913204209627575,35.9556111849861));
#49870=CARTESIAN_POINT('Ctrl Pts',(18.9323957143926,0.917431712595288,35.9913958336728));
#49871=CARTESIAN_POINT('Ctrl Pts',(18.8617625388377,0.92165656112653,36.0271580132855));
#49872=CARTESIAN_POINT('Ctrl Pts',(18.7928770522779,0.925881409657772,36.0664990513099));
#49873=CARTESIAN_POINT('Ctrl Pts',(18.7261188279924,0.930106258189014,36.1092169378598));
#49874=CARTESIAN_POINT('Ctrl Pts',(18.6593817580276,0.93432976795186,36.151921287982));
#49875=CARTESIAN_POINT('Ctrl Pts',(18.5947710061138,0.938553277714706,36.1980001093094));
#49876=CARTESIAN_POINT('Ctrl Pts',(18.532639145738,0.942776787477552,36.2472068209648));
#49877=CARTESIAN_POINT('Ctrl Pts',(18.4705076500873,0.947000272447639,36.296413243768));
#49878=CARTESIAN_POINT('Ctrl Pts',(18.4108553834613,0.951223757417726,36.3487472283445));
#49879=CARTESIAN_POINT('Ctrl Pts',(18.354002482924,0.955447242387812,36.4039214007954));
#49880=CARTESIAN_POINT('Ctrl Pts',(18.2970929061349,0.959674937720001,36.4591505759862));
#49881=CARTESIAN_POINT('Ctrl Pts',(18.2429886068065,0.96390263305219,36.5172252675961));
#49882=CARTESIAN_POINT('Ctrl Pts',(18.1919729611805,0.968130328384379,36.5778210789143));
#49883=CARTESIAN_POINT('Ctrl Pts',(18.1409325062355,0.97236007967883,36.6384463584632));
#49884=CARTESIAN_POINT('Ctrl Pts',(18.0929839809455,0.976589830973282,36.7015948264862));
#49885=CARTESIAN_POINT('Ctrl Pts',(18.0483689442624,0.980819582267733,36.7669108570016));
#49886=CARTESIAN_POINT('Ctrl Pts',(18.0036737137948,0.985056936374789,36.8323442905284));
#49887=CARTESIAN_POINT('Ctrl Pts',(17.9623241892086,0.989294290481844,36.8999526706709));
#49888=CARTESIAN_POINT('Ctrl Pts',(17.9245171304773,0.9935316445889,36.969353592312));
#49889=CARTESIAN_POINT('Ctrl Pts',(17.8902318405216,0.997374284537119,37.0322897423725));
#49890=CARTESIAN_POINT('Ctrl Pts',(17.8588592969497,1.00121692448534,37.0966994897598));
#49891=CARTESIAN_POINT('Ctrl Pts',(17.830511574449,1.00505956443356,37.1622844715479));
#49892=CARTESIAN_POINT('Ctrl Pts',(17.7960497203405,1.00973099781886,37.2420150415799));
#49893=CARTESIAN_POINT('Ctrl Pts',(17.7659475077993,1.01440243120416,37.3237385639075));
#49894=CARTESIAN_POINT('Ctrl Pts',(17.7404156919232,1.01907386458946,37.4069854290183));
#49895=CARTESIAN_POINT('Ctrl Pts',(17.7149582744737,1.02373168565296,37.4899897169534));
#49896=CARTESIAN_POINT('Ctrl Pts',(17.6940448157563,1.02838950671645,37.5745082191302));
#49897=CARTESIAN_POINT('Ctrl Pts',(17.6778379434104,1.03304732777995,37.6600524760432));
#49898=CARTESIAN_POINT('Ctrl Pts',(17.6617109571308,1.03768218975585,37.7451750726861));
#49899=CARTESIAN_POINT('Ctrl Pts',(17.6502443976019,1.04231705173175,37.8313130549651));
#49900=CARTESIAN_POINT('Ctrl Pts',(17.6435505015056,1.04695191370765,37.9179664812586));
#49901=CARTESIAN_POINT('Ctrl Pts',(17.6389066447746,1.05016732587926,37.9780818596809));
#49902=CARTESIAN_POINT('Ctrl Pts',(17.6365587886261,1.05338273805088,38.0384449196041));
#49903=CARTESIAN_POINT('Ctrl Pts',(17.6365302632328,1.05659815022249,38.098884524413));
#49904=CARTESIAN_POINT('',(17.6365309191062,1.85034815030119,38.102084360615));
#49905=CARTESIAN_POINT('Ctrl Pts',(17.6365302632324,1.05659815027172,38.0988845253384));
#49906=CARTESIAN_POINT('Ctrl Pts',(17.6364922090284,1.06088766352129,38.1795138418281));
#49907=CARTESIAN_POINT('Ctrl Pts',(17.6405844802438,1.06517717677086,38.2601328060387));
#49908=CARTESIAN_POINT('Ctrl Pts',(17.6487775398017,1.06946669002043,38.3402985300805));
#49909=CARTESIAN_POINT('Ctrl Pts',(17.656974087378,1.07375802943784,38.4204983829519));
#49910=CARTESIAN_POINT('Ctrl Pts',(17.6692748484675,1.07804936885525,38.5002441667311));
#49911=CARTESIAN_POINT('Ctrl Pts',(17.6855986141635,1.08234070827266,38.5790998498624));
#49912=CARTESIAN_POINT('Ctrl Pts',(17.7019469595511,1.08663850942208,38.6580742708148));
#49913=CARTESIAN_POINT('Ctrl Pts',(17.7223303146537,1.0909363105715,38.7361554754159));
#49914=CARTESIAN_POINT('Ctrl Pts',(17.7466167131606,1.09523411172092,38.8129194929954));
#49915=CARTESIAN_POINT('Ctrl Pts',(17.770922240334,1.09953529794223,38.8897439721246));
#49916=CARTESIAN_POINT('Ctrl Pts',(17.7991367774029,1.10383648416353,38.9652487783743));
#49917=CARTESIAN_POINT('Ctrl Pts',(17.8310799063504,1.10813767038484,39.0390293223658));
#49918=CARTESIAN_POINT('Ctrl Pts',(17.8630887408235,1.1124477039455,39.1129616294936));
#49919=CARTESIAN_POINT('Ctrl Pts',(17.8988412914902,1.11675773750616,39.1851621864708));
#49920=CARTESIAN_POINT('Ctrl Pts',(17.9381108110437,1.12106777106683,39.2552503682601));
#49921=CARTESIAN_POINT('Ctrl Pts',(17.967614619562,1.1243059671621,39.3079087230966));
#49922=CARTESIAN_POINT('Ctrl Pts',(17.999102709071,1.12754416325737,39.359375209935));
#49923=CARTESIAN_POINT('Ctrl Pts',(18.0324634928686,1.13078235935264,39.4095001084404));
#49924=CARTESIAN_POINT('Ctrl Pts',(18.0761228872686,1.135020199846,39.4750987684232));
#49925=CARTESIAN_POINT('Ctrl Pts',(18.1231484012448,1.13925804033936,39.5386346470832));
#49926=CARTESIAN_POINT('Ctrl Pts',(18.173318584529,1.14349588083273,39.5997417935341));
#49927=CARTESIAN_POINT('Ctrl Pts',(18.2234166423239,1.14772762893617,39.6607610913357));
#49928=CARTESIAN_POINT('Ctrl Pts',(18.2766500964784,1.15195937703962,39.7193582316383));
#49929=CARTESIAN_POINT('Ctrl Pts',(18.3327541842083,1.15619112514307,39.7751960573691));
#49930=CARTESIAN_POINT('Ctrl Pts',(18.3887934905289,1.16041798699639,39.8309694091341));
#49931=CARTESIAN_POINT('Ctrl Pts',(18.44769651288,1.16464484884972,39.8839894489175));
#49932=CARTESIAN_POINT('Ctrl Pts',(18.5091591799931,1.16887171070304,39.9339531319805));
#49933=CARTESIAN_POINT('Ctrl Pts',(18.5705830619685,1.17309590525559,39.9838852861754));
#49934=CARTESIAN_POINT('Ctrl Pts',(18.6345630198887,1.17732009980815,40.0307646169701));
#49935=CARTESIAN_POINT('Ctrl Pts',(18.7007600941331,1.1815442943607,40.0743267480088));
#49936=CARTESIAN_POINT('Ctrl Pts',(18.7669360012338,1.18576713818689,40.117874949642));
#49937=CARTESIAN_POINT('Ctrl Pts',(18.8353272255652,1.18998998201307,40.1581078004002));
#49938=CARTESIAN_POINT('Ctrl Pts',(18.9055650888976,1.19421282583926,40.1948037297705));
#49939=CARTESIAN_POINT('Ctrl Pts',(18.9758023558371,1.19843563380909,40.2314993475539));
#49940=CARTESIAN_POINT('Ctrl Pts',(19.0478858144988,1.20265844177892,40.2646578878824));
#49941=CARTESIAN_POINT('Ctrl Pts',(19.1214227338433,1.20688124974875,40.294104014921));
#49942=CARTESIAN_POINT('Ctrl Pts',(19.1950327513745,1.21110825533262,40.3235794124066));
#49943=CARTESIAN_POINT('Ctrl Pts',(19.2700986794169,1.2153352609165,40.3493348506362));
#49944=CARTESIAN_POINT('Ctrl Pts',(19.346208941088,1.21956226650037,40.3712436443911));
#49945=CARTESIAN_POINT('Ctrl Pts',(19.4223560763857,1.22379131996875,40.3931630524397));
#49946=CARTESIAN_POINT('Ctrl Pts',(19.4995480962676,1.22802037343713,40.4112319965042));
#49947=CARTESIAN_POINT('Ctrl Pts',(19.5773619293001,1.23224942690551,40.4253747014396));
#49948=CARTESIAN_POINT('Ctrl Pts',(19.6553155498996,1.23648607759758,40.4395428128385));
#49949=CARTESIAN_POINT('Ctrl Pts',(19.7338927497158,1.24072272828964,40.4497705314025));
#49950=CARTESIAN_POINT('Ctrl Pts',(19.8126642430962,1.24495937898171,40.4560339036366));
#49951=CARTESIAN_POINT('Ctrl Pts',(19.8842206074614,1.24880797074504,40.4617235779911));
#49952=CARTESIAN_POINT('Ctrl Pts',(19.9559370023904,1.25265656250838,40.4641425402918));
#49953=CARTESIAN_POINT('Ctrl Pts',(20.0274937259456,1.25650515427172,40.4633100803605));
#49954=CARTESIAN_POINT('Ctrl Pts',(20.1062856091861,1.26074288034121,40.462393449715));
#49955=CARTESIAN_POINT('Ctrl Pts',(20.1851794264319,1.2649806064107,40.4575304519096));
#49956=CARTESIAN_POINT('Ctrl Pts',(20.2637476697309,1.26921833248019,40.4487076462624));
#49957=CARTESIAN_POINT('Ctrl Pts',(20.3422029700115,1.27344996675542,40.4398975235296));
#49958=CARTESIAN_POINT('Ctrl Pts',(20.4203331638077,1.27768160103065,40.4271389491961));
#49959=CARTESIAN_POINT('Ctrl Pts',(20.4977113197383,1.28191323530589,40.410470489555));
#49960=CARTESIAN_POINT('Ctrl Pts',(20.5750001542058,1.28613998479471,40.3938212711478));
#49961=CARTESIAN_POINT('Ctrl Pts',(20.6515382200484,1.29036673428353,40.3732712348634));
#49962=CARTESIAN_POINT('Ctrl Pts',(20.7269058037042,1.29459348377236,40.3489104903133));
#49963=CARTESIAN_POINT('Ctrl Pts',(20.8022258433493,1.29881756690765,40.3245651132122));
#49964=CARTESIAN_POINT('Ctrl Pts',(20.8763764215342,1.30304165004293,40.2964139431262));
#49965=CARTESIAN_POINT('Ctrl Pts',(20.9489512710763,1.30726573317822,40.264597405067));
#49966=CARTESIAN_POINT('Ctrl Pts',(21.0215029325541,1.31148846669568,40.232791032567));
#49967=CARTESIAN_POINT('Ctrl Pts',(21.0924794361512,1.31571120021313,40.1973218057531));
#49968=CARTESIAN_POINT('Ctrl Pts',(21.1614942462938,1.31993393373059,40.1583783803583));
#49969=CARTESIAN_POINT('Ctrl Pts',(21.2305084911823,1.32415663266246,40.119435273923));
#49970=CARTESIAN_POINT('Ctrl Pts',(21.2975606670246,1.32837933159433,40.0770182570923));
#49971=CARTESIAN_POINT('Ctrl Pts',(21.362289930623,1.3326020305262,40.0313613296903));
#49972=CARTESIAN_POINT('Ctrl Pts',(21.4270835816442,1.33682892985657,39.9856589864791));
#49973=CARTESIAN_POINT('Ctrl Pts',(21.4895493209607,1.34105582918694,39.9367105659571));
#49974=CARTESIAN_POINT('Ctrl Pts',(21.5493568587223,1.34528272851731,39.884792359136));
#49975=CARTESIAN_POINT('Ctrl Pts',(21.6091933917337,1.34951167708774,39.832848981886));
#49976=CARTESIAN_POINT('Ctrl Pts',(21.6663688174055,1.35374062565816,39.777933275252));
#49977=CARTESIAN_POINT('Ctrl Pts',(21.7205892967737,1.35796957422859,39.720358883929));
#49978=CARTESIAN_POINT('Ctrl Pts',(21.7749072275994,1.36220612356548,39.6626810131014));
#49979=CARTESIAN_POINT('Ctrl Pts',(21.8262592957658,1.36644267290238,39.6023352675118));
#49980=CARTESIAN_POINT('Ctrl Pts',(21.8743917519422,1.37067922223927,39.5396687122915));
#49981=CARTESIAN_POINT('Ctrl Pts',(21.9181277069757,1.37452879788978,39.4827262277615));
#49982=CARTESIAN_POINT('Ctrl Pts',(21.9592057467301,1.37837837354028,39.4238681546416));
#49983=CARTESIAN_POINT('Ctrl Pts',(21.9974679156332,1.38222794919079,39.3633734075545));
#49984=CARTESIAN_POINT('Ctrl Pts',(22.0395862130507,1.38646549182956,39.2967818937159));
#49985=CARTESIAN_POINT('Ctrl Pts',(22.0784499280056,1.39070303446833,39.2279568106674));
#49986=CARTESIAN_POINT('Ctrl Pts',(22.1138150633832,1.3949405771071,39.1572494117824));
#49987=CARTESIAN_POINT('Ctrl Pts',(22.1491293279213,1.39917202426938,39.0866437216765));
#49988=CARTESIAN_POINT('Ctrl Pts',(22.1809547990065,1.40340347143165,39.0141615086005));
#49989=CARTESIAN_POINT('Ctrl Pts',(22.209091417091,1.40763491859393,38.9401818564066));
#49990=CARTESIAN_POINT('Ctrl Pts',(22.2371955231821,1.41186147629926,38.8662876880461));
#49991=CARTESIAN_POINT('Ctrl Pts',(22.2616190810898,1.41608803400459,38.7908999550597));
#49992=CARTESIAN_POINT('Ctrl Pts',(22.2822091960486,1.42031459170992,38.714419747706));
#49993=CARTESIAN_POINT('Ctrl Pts',(22.3027863081582,1.42453848030471,38.6379878383152));
#49994=CARTESIAN_POINT('Ctrl Pts',(22.3195346608879,1.4287623688995,38.5604652754409));
#49995=CARTESIAN_POINT('Ctrl Pts',(22.3323508852338,1.43298625749429,38.4822692624957));
#49996=CARTESIAN_POINT('Ctrl Pts',(22.3451630069937,1.43720879398521,38.4040982807816));
#49997=CARTESIAN_POINT('Ctrl Pts',(22.3540454241433,1.44143133047612,38.3252547393824));
#49998=CARTESIAN_POINT('Ctrl Pts',(22.3589459666818,1.44565386696704,38.2461655471566));
#49999=CARTESIAN_POINT('Ctrl Pts',(22.3638464665078,1.4498763666548,38.1670770442634));
#50000=CARTESIAN_POINT('Ctrl Pts',(22.3647651331607,1.45409886634255,38.0877433627901));
#50001=CARTESIAN_POINT('Ctrl Pts',(22.3617018193823,1.45832136603031,38.0085945448767));
#50002=CARTESIAN_POINT('Ctrl Pts',(22.3586354598535,1.46254806400814,37.9293670319435));
#50003=CARTESIAN_POINT('Ctrl Pts',(22.3515792296434,1.46677476198598,37.8503252192567));
#50004=CARTESIAN_POINT('Ctrl Pts',(22.3405850896208,1.47100145996381,37.7718965420103));
#50005=CARTESIAN_POINT('Ctrl Pts',(22.3295856231211,1.47523020570618,37.6934298673803));
#50006=CARTESIAN_POINT('Ctrl Pts',(22.31464453462,1.47945895144855,37.6155773809426));
#50007=CARTESIAN_POINT('Ctrl Pts',(22.2958649617504,1.48368769719093,37.5387562754857));
#50008=CARTESIAN_POINT('Ctrl Pts',(22.2770516350047,1.48792404356196,37.4617970939344));
#50009=CARTESIAN_POINT('Ctrl Pts',(22.2543861730742,1.492160389933,37.3858734476615));
#50010=CARTESIAN_POINT('Ctrl Pts',(22.228021571741,1.49639673630403,37.3113870932095));
#50011=CARTESIAN_POINT('Ctrl Pts',(22.2040530555621,1.50024807223931,37.2436702569397));
#50012=CARTESIAN_POINT('Ctrl Pts',(22.1770279440483,1.50409940817459,37.1771413418693));
#50013=CARTESIAN_POINT('Ctrl Pts',(22.1470944454545,1.50795074410987,37.1120850830167));
#50014=CARTESIAN_POINT('Ctrl Pts',(22.1141582190445,1.51218842023544,37.0405028166052));
#50015=CARTESIAN_POINT('Ctrl Pts',(22.0775765256762,1.51642609636102,36.9704351006756));
#50016=CARTESIAN_POINT('Ctrl Pts',(22.0375112375595,1.52066377248659,36.9022778294952));
#50017=CARTESIAN_POINT('Ctrl Pts',(21.9975035613329,1.52489535504482,36.8342185650784));
#50018=CARTESIAN_POINT('Ctrl Pts',(21.9540224738326,1.52912693760305,36.76806469065));
#50019=CARTESIAN_POINT('Ctrl Pts',(21.9072771086963,1.53335852016128,36.7041903885046));
#50020=CARTESIAN_POINT('Ctrl Pts',(21.8605857316504,1.53758521549571,36.6403898573435));
#50021=CARTESIAN_POINT('Ctrl Pts',(21.8106378444394,1.54181191083013,36.5788640428588));
#50022=CARTESIAN_POINT('Ctrl Pts',(21.7576867131067,1.54603860616456,36.5199595386611));
#50023=CARTESIAN_POINT('Ctrl Pts',(21.7047690035798,1.55026263368459,36.4610922139315));
#50024=CARTESIAN_POINT('Ctrl Pts',(21.6488521250394,1.55448666120462,36.4048432631426));
#50025=CARTESIAN_POINT('Ctrl Pts',(21.5902298172869,1.55871068872465,36.3515265031715));
#50026=CARTESIAN_POINT('Ctrl Pts',(21.5316262591519,1.56293336524191,36.2982267959044));
#50027=CARTESIAN_POINT('Ctrl Pts',(21.4703193366545,1.56715604175917,36.2478577322939));
#50028=CARTESIAN_POINT('Ctrl Pts',(21.4066387990038,1.57137871827643,36.2006954614815));
#50029=CARTESIAN_POINT('Ctrl Pts',(21.3429588026859,1.57560135889775,36.153533591584));
#50030=CARTESIAN_POINT('Ctrl Pts',(21.2769056088874,1.57982399951907,36.109578738123));
#50031=CARTESIAN_POINT('Ctrl Pts',(21.2088399116202,1.58404664014039,36.0690651145411));
#50032=CARTESIAN_POINT('Ctrl Pts',(21.1407065340248,1.58827347949492,36.0285112067125));
#50033=CARTESIAN_POINT('Ctrl Pts',(21.0705570594829,1.59250031884945,35.9914056040329));
#50034=CARTESIAN_POINT('Ctrl Pts',(20.9987783582249,1.59672715820398,35.9579373883937));
#50035=CARTESIAN_POINT('Ctrl Pts',(20.9269648746004,1.6009560457911,35.9244529547995));
#50036=CARTESIAN_POINT('Ctrl Pts',(20.8535210263446,1.60518493337822,35.89460959624));
#50037=CARTESIAN_POINT('Ctrl Pts',(20.7788529481758,1.60941382096534,35.8685478884776));
#50038=CARTESIAN_POINT('Ctrl Pts',(20.704050683485,1.61365030831573,35.8424393450391));
#50039=CARTESIAN_POINT('Ctrl Pts',(20.6280202437852,1.61788679566611,35.8201261638457));
#50040=CARTESIAN_POINT('Ctrl Pts',(20.5511819536775,1.62212328301649,35.8016986936348));
#50041=CARTESIAN_POINT('Ctrl Pts',(20.4813519389428,1.62597336835398,35.7849519581914));
#50042=CARTESIAN_POINT('Ctrl Pts',(20.4108551177745,1.62982345369147,35.7714138383846));
#50043=CARTESIAN_POINT('Ctrl Pts',(20.340010694254,1.63367353902895,35.7611149731778));
#50044=CARTESIAN_POINT('Ctrl Pts',(20.2620347941965,1.63791118900294,35.7497793839507));
#50045=CARTESIAN_POINT('Ctrl Pts',(20.1833450394548,1.64214883897692,35.7423262308307));
#50046=CARTESIAN_POINT('Ctrl Pts',(20.1043616405112,1.64638648895091,35.7388352262305));
#50047=CARTESIAN_POINT('Ctrl Pts',(20.0254918181876,1.65061804526513,35.7353492416284));
#50048=CARTESIAN_POINT('Ctrl Pts',(19.9463296546664,1.65484960157934,35.7358141113773));
#50049=CARTESIAN_POINT('Ctrl Pts',(19.8673028734806,1.65908115789356,35.7402580832825));
#50050=CARTESIAN_POINT('Ctrl Pts',(19.7883673642613,1.66330782697259,35.7446969226232));
#50051=CARTESIAN_POINT('Ctrl Pts',(19.7095673923144,1.66753449605162,35.7531057051948));
#50052=CARTESIAN_POINT('Ctrl Pts',(19.6313315611324,1.67176116513065,35.7654606400656));
#50053=CARTESIAN_POINT('Ctrl Pts',(19.553145111207,1.67598516640098,35.7778077766911));
#50054=CARTESIAN_POINT('Ctrl Pts',(19.4755225570951,1.68020916767132,35.7940960488192));
#50055=CARTESIAN_POINT('Ctrl Pts',(19.3988870385322,1.68443316894165,35.8142498718243));
#50056=CARTESIAN_POINT('Ctrl Pts',(19.3222760302581,1.68865581925237,35.834397249045));
#50057=CARTESIAN_POINT('Ctrl Pts',(19.2466518836787,1.69287846956309,35.8584076029226));
#50058=CARTESIAN_POINT('Ctrl Pts',(19.172425741671,1.69710111987381,35.8861546377736));
#50059=CARTESIAN_POINT('Ctrl Pts',(19.098200229228,1.70132373436923,35.9139014372824));
#50060=CARTESIAN_POINT('Ctrl Pts',(19.0253731363741,1.70554634886465,35.945384689268));
#50061=CARTESIAN_POINT('Ctrl Pts',(18.9543372719364,1.70976896336007,35.980429312328));
#50062=CARTESIAN_POINT('Ctrl Pts',(18.8832307681291,1.71399577690097,36.0155087844053));
#50063=CARTESIAN_POINT('Ctrl Pts',(18.8139194721272,1.71822259044188,36.054156493825));
#50064=CARTESIAN_POINT('Ctrl Pts',(18.7467725820626,1.72244940398278,36.0961508340621));
#50065=CARTESIAN_POINT('Ctrl Pts',(18.6795931518429,1.72667826588613,36.1381655252394));
#50066=CARTESIAN_POINT('Ctrl Pts',(18.614580602009,1.73090712778948,36.1835298094884));
#50067=CARTESIAN_POINT('Ctrl Pts',(18.552073926742,1.73513598969284,36.2319795163651));
#50068=CARTESIAN_POINT('Ctrl Pts',(18.489454911885,1.73937245188225,36.280516299065));
#50069=CARTESIAN_POINT('Ctrl Pts',(18.4293511267712,1.74360891407166,36.3321492781482));
#50070=CARTESIAN_POINT('Ctrl Pts',(18.3720671557503,1.74784537626107,36.3865750394274));
#50071=CARTESIAN_POINT('Ctrl Pts',(18.3200044757893,1.75169569549006,36.4360400283347));
#50072=CARTESIAN_POINT('Ctrl Pts',(18.2702707099253,1.75554601471904,36.4878112278055));
#50073=CARTESIAN_POINT('Ctrl Pts',(18.2230653501685,1.75939633394803,36.5416374968807));
#50074=CARTESIAN_POINT('Ctrl Pts',(18.1715836395797,1.76359545500637,36.6003399073884));
#50075=CARTESIAN_POINT('Ctrl Pts',(18.1229080755859,1.76779457606471,36.6617171330744));
#50076=CARTESIAN_POINT('Ctrl Pts',(18.0773323538624,1.77199369712305,36.7254675109712));
#50077=CARTESIAN_POINT('Ctrl Pts',(18.0318175156023,1.77618720868092,36.7891327263375));
#50078=CARTESIAN_POINT('Ctrl Pts',(17.989394580521,1.78038072023878,36.8551644206018));
#50079=CARTESIAN_POINT('Ctrl Pts',(17.9503186160587,1.78457423179664,36.923226162245));
#50080=CARTESIAN_POINT('Ctrl Pts',(17.911282140254,1.78876350555401,36.9912191233261));
#50081=CARTESIAN_POINT('Ctrl Pts',(17.8755861597843,1.79295277931138,37.0612376488103));
#50082=CARTESIAN_POINT('Ctrl Pts',(17.8434428890811,1.79714205306875,37.1329157905098));
#50083=CARTESIAN_POINT('Ctrl Pts',(17.8113216485129,1.80132845561033,37.204544805935));
#50084=CARTESIAN_POINT('Ctrl Pts',(17.7827484780239,1.80551485815192,37.27783074427));
#50085=CARTESIAN_POINT('Ctrl Pts',(17.7578892482021,1.80970126069351,37.3523839103041));
#50086=CARTESIAN_POINT('Ctrl Pts',(17.7330335636422,1.81388706619755,37.4269264440499));
#50087=CARTESIAN_POINT('Ctrl Pts',(17.7118909287193,1.8180728717016,37.5027353967955));
#50088=CARTESIAN_POINT('Ctrl Pts',(17.6945782475928,1.82225867720565,37.5794032420121));
#50089=CARTESIAN_POINT('Ctrl Pts',(17.6772666835378,1.82644421262763,37.6560661403648));
#50090=CARTESIAN_POINT('Ctrl Pts',(17.6637846795615,1.83062974804961,37.7335873531143));
#50091=CARTESIAN_POINT('Ctrl Pts',(17.6541982053108,1.8348152834716,37.8115483039864));
#50092=CARTESIAN_POINT('Ctrl Pts',(17.6446061767769,1.83900324394048,37.8895544244588));
#50093=CARTESIAN_POINT('Ctrl Pts',(17.638914228829,1.84319120440936,37.9680003158431));
#50094=CARTESIAN_POINT('Ctrl Pts',(17.6371364426992,1.84737916487824,38.0464626253931));
#50095=CARTESIAN_POINT('Ctrl Pts',(17.636716331996,1.84836882667607,38.0650041448052));
#50096=CARTESIAN_POINT('Ctrl Pts',(17.6365145705078,1.84935848847389,38.0835465812456));
#50097=CARTESIAN_POINT('Ctrl Pts',(17.6365309191057,1.85034815027172,38.1020843600629));
#50098=CARTESIAN_POINT('',(17.6365300584559,2.64409815030312,38.0994743406844));
#50099=CARTESIAN_POINT('Ctrl Pts',(17.6365309191062,1.85034815030119,38.102084360615));
#50100=CARTESIAN_POINT('Ctrl Pts',(17.6366171557615,1.8555684817835,38.1998686244756));
#50101=CARTESIAN_POINT('Ctrl Pts',(17.6427755898215,1.86078881326582,38.2973860103044));
#50102=CARTESIAN_POINT('Ctrl Pts',(17.6548850483977,1.86600914474813,38.3939835108835));
#50103=CARTESIAN_POINT('Ctrl Pts',(17.6672029815152,1.87131934863924,38.4922440188962));
#50104=CARTESIAN_POINT('Ctrl Pts',(17.6856785644927,1.87662955253035,38.5895528165203));
#50105=CARTESIAN_POINT('Ctrl Pts',(17.7101357563283,1.88193975642146,38.6852454070336));
#50106=CARTESIAN_POINT('Ctrl Pts',(17.7150168320469,1.88299954723668,38.704343379652));
#50107=CARTESIAN_POINT('Ctrl Pts',(17.7201360078384,1.8840593380519,38.7233770457282));
#50108=CARTESIAN_POINT('Ctrl Pts',(17.7254916586676,1.88511912886712,38.7423412224896));
#50109=CARTESIAN_POINT('Ctrl Pts',(17.7469066035976,1.88935677666546,38.8181708114481));
#50110=CARTESIAN_POINT('Ctrl Pts',(17.7721580043752,1.8935944244638,38.8930706393473));
#50111=CARTESIAN_POINT('Ctrl Pts',(17.8011474670498,1.89783207226214,38.9666244741747));
#50112=CARTESIAN_POINT('Ctrl Pts',(17.8300952422087,1.90206362622524,39.0400725368917));
#50113=CARTESIAN_POINT('Ctrl Pts',(17.8627702337122,1.90629518018834,39.1121780178797));
#50114=CARTESIAN_POINT('Ctrl Pts',(17.899023986667,1.91052673415144,39.1825387902054));
#50115=CARTESIAN_POINT('Ctrl Pts',(17.9352358661502,1.91475340062454,39.2528182950881));
#50116=CARTESIAN_POINT('Ctrl Pts',(17.9750180791399,1.91898006709764,39.3213566813332));
#50117=CARTESIAN_POINT('Ctrl Pts',(18.018174287773,1.92320673357075,39.3877722187002));
#50118=CARTESIAN_POINT('Ctrl Pts',(18.0613032552779,1.92743073208096,39.4541458331499));
#50119=CARTESIAN_POINT('Ctrl Pts',(18.1078017363803,1.93165473059118,39.5183988664016));
#50120=CARTESIAN_POINT('Ctrl Pts',(18.1574283184202,1.93587872910139,39.580175678472));
#50121=CARTESIAN_POINT('Ctrl Pts',(18.2070390266422,1.94010137650138,39.6419327302885));
#50122=CARTESIAN_POINT('Ctrl Pts',(18.2597755554984,1.94432402390136,39.7012147685995));
#50123=CARTESIAN_POINT('Ctrl Pts',(18.3153550678058,1.94854667130134,39.7576977689955));
#50124=CARTESIAN_POINT('Ctrl Pts',(18.3709341067662,1.95276928273883,39.8141802883497));
#50125=CARTESIAN_POINT('Ctrl Pts',(18.4293557512288,1.95699189417632,39.8678634840564));
#50126=CARTESIAN_POINT('Ctrl Pts',(18.49030007955,1.9612145056138,39.9184599503682));
#50127=CARTESIAN_POINT('Ctrl Pts',(18.5513050090197,1.96544131588506,39.9691067282359));
#50128=CARTESIAN_POINT('Ctrl Pts',(18.6148372715323,1.96966812615631,40.0166603455416));
#50129=CARTESIAN_POINT('Ctrl Pts',(18.6805440751784,1.97389493642756,40.0608739131707));
#50130=CARTESIAN_POINT('Ctrl Pts',(18.7462827192386,1.97812379494011,40.1051089059524));
#50131=CARTESIAN_POINT('Ctrl Pts',(18.814197601508,1.98235265345266,40.146000382642));
#50132=CARTESIAN_POINT('Ctrl Pts',(18.8839093634339,1.98658151196521,40.1833463782745));
#50133=CARTESIAN_POINT('Ctrl Pts',(18.9537464115799,1.99081797059693,40.2207594922598));
#50134=CARTESIAN_POINT('Ctrl Pts',(19.0253863671182,1.99505442922866,40.2546141926485));
#50135=CARTESIAN_POINT('Ctrl Pts',(19.0984280504848,1.99929088786038,40.2847559270425));
#50136=CARTESIAN_POINT('Ctrl Pts',(19.164812672012,2.00314123316898,40.3121505260946));
#50137=CARTESIAN_POINT('Ctrl Pts',(19.2323546680652,2.00699157847758,40.336478654606));
#50138=CARTESIAN_POINT('Ctrl Pts',(19.3007434046261,2.01084192378618,40.3576604383136));
#50139=CARTESIAN_POINT('Ctrl Pts',(19.3760112099709,2.01507956664628,40.3809728498762));
#50140=CARTESIAN_POINT('Ctrl Pts',(19.4525873877916,2.01931720950637,40.400560891116));
#50141=CARTESIAN_POINT('Ctrl Pts',(19.5300692163137,2.02355485236646,40.4162805312492));
#50142=CARTESIAN_POINT('Ctrl Pts',(19.607439623386,2.02778640135498,40.4319775660164));
#50143=CARTESIAN_POINT('Ctrl Pts',(19.6857126391836,2.03201795034351,40.4438171546242));
#50144=CARTESIAN_POINT('Ctrl Pts',(19.764470124179,2.03624949933204,40.4517049386553));
#50145=CARTESIAN_POINT('Ctrl Pts',(19.8431366427601,2.04047616079987,40.4595836121437));
#50146=CARTESIAN_POINT('Ctrl Pts',(19.9222860544513,2.0447028222677,40.4635195052084));
#50147=CARTESIAN_POINT('Ctrl Pts',(20.0014912653639,2.04892948373553,40.4634695295323));
#50148=CARTESIAN_POINT('Ctrl Pts',(20.0806464798769,2.05315347722415,40.4634195854022));
#50149=CARTESIAN_POINT('Ctrl Pts',(20.159856956153,2.05737747071278,40.4593887667777));
#50150=CARTESIAN_POINT('Ctrl Pts',(20.2386929506919,2.0616014642014,40.4513859989781));
#50151=CARTESIAN_POINT('Ctrl Pts',(20.317503728136,2.0658241065706,40.443385791006));
#50152=CARTESIAN_POINT('Ctrl Pts',(20.3959397956713,2.07004674893979,40.4314162041263));
#50153=CARTESIAN_POINT('Ctrl Pts',(20.4735753821855,2.07426939130899,40.4155381228319));
#50154=CARTESIAN_POINT('Ctrl Pts',(20.5512103074713,2.0784919977136,40.3996601767723));
#50155=CARTESIAN_POINT('Ctrl Pts',(20.6280443063126,2.08271460411822,40.3798738978164));
#50156=CARTESIAN_POINT('Ctrl Pts',(20.7036621393815,2.08693721052283,40.3562912122554));
#50157=CARTESIAN_POINT('Ctrl Pts',(20.7793551651435,2.09116401579344,40.3326850765959));
#50158=CARTESIAN_POINT('Ctrl Pts',(20.853829160939,2.09539082106404,40.3052751335167));
#50159=CARTESIAN_POINT('Ctrl Pts',(20.9266849830521,2.09961762633465,40.2742229377609));
#50160=CARTESIAN_POINT('Ctrl Pts',(20.999576110082,2.10384647985623,40.2431556945435));
#50161=CARTESIAN_POINT('Ctrl Pts',(21.0708470793397,2.10807533337781,40.2084428881213));
#50162=CARTESIAN_POINT('Ctrl Pts',(21.1401219713545,2.11230418689939,40.1702928129458));
#50163=CARTESIAN_POINT('Ctrl Pts',(21.2095213658217,2.1165406406152,40.1320741735649));
#50164=CARTESIAN_POINT('Ctrl Pts',(21.2769171154113,2.120777094331,40.0904061692058));
#50165=CARTESIAN_POINT('Ctrl Pts',(21.3419611955674,2.12501354804681,40.0455412076055));
#50166=CARTESIAN_POINT('Ctrl Pts',(21.4010778782623,2.1288639382663,40.0047647419737));
#50167=CARTESIAN_POINT('Ctrl Pts',(21.458252154305,2.13271432848578,39.961348140781));
#50168=CARTESIAN_POINT('Ctrl Pts',(21.5132479222866,2.13656471870527,39.9155085146028));
#50169=CARTESIAN_POINT('Ctrl Pts',(21.5737748531757,2.14080235936861,39.8650585984093));
#50170=CARTESIAN_POINT('Ctrl Pts',(21.6318897287454,2.14504000003196,39.8114838263428));
#50171=CARTESIAN_POINT('Ctrl Pts',(21.6872525104689,2.1492776406953,39.755043626862));
#50172=CARTESIAN_POINT('Ctrl Pts',(21.7425356779164,2.15350918743267,39.6986845910344));
#50173=CARTESIAN_POINT('Ctrl Pts',(21.7950742854727,2.15774073417004,39.6394686428468));
#50174=CARTESIAN_POINT('Ctrl Pts',(21.8445615706559,2.16197228090742,39.5776951826948));
#50175=CARTESIAN_POINT('Ctrl Pts',(21.8939916962034,2.16619894005258,39.5159930731628));
#50176=CARTESIAN_POINT('Ctrl Pts',(21.940377211622,2.17042559919773,39.4517396860489));
#50177=CARTESIAN_POINT('Ctrl Pts',(21.9834494890326,2.17465225834289,39.3852698414561));
#50178=CARTESIAN_POINT('Ctrl Pts',(22.0264945776475,2.17887624946633,39.3188419550583));
#50179=CARTESIAN_POINT('Ctrl Pts',(22.0662303252704,2.18310024058977,39.2502007806291));
#50180=CARTESIAN_POINT('Ctrl Pts',(22.1024302942585,2.18732423171321,39.1797116738668));
#50181=CARTESIAN_POINT('Ctrl Pts',(22.1386186837,2.19154687167797,39.1092451149662));
#50182=CARTESIAN_POINT('Ctrl Pts',(22.171273326482,2.19576951164274,39.0369322142614));
#50183=CARTESIAN_POINT('Ctrl Pts',(22.2002135341123,2.19999215160751,38.9631632784179));
#50184=CARTESIAN_POINT('Ctrl Pts',(22.2291534950096,2.20421475557169,38.8893949714997));
#50185=CARTESIAN_POINT('Ctrl Pts',(22.2543789138503,2.20843735953587,38.8141710910394));
#50186=CARTESIAN_POINT('Ctrl Pts',(22.2757576522585,2.21265996350005,38.7379008928407));
#50187=CARTESIAN_POINT('Ctrl Pts',(22.2971576490197,2.21688676629038,38.6615548539273));
#50188=CARTESIAN_POINT('Ctrl Pts',(22.3147031980385,2.22111356908071,38.5841608714462));
#50189=CARTESIAN_POINT('Ctrl Pts',(22.3283125540416,2.22534037187103,38.5061417136818));
#50190=CARTESIAN_POINT('Ctrl Pts',(22.34192850487,2.22956922288656,38.4280847493735));
#50191=CARTESIAN_POINT('Ctrl Pts',(22.3516044056267,2.23379807390209,38.349402472139));
#50192=CARTESIAN_POINT('Ctrl Pts',(22.3573103612433,2.23802692491762,38.2705236103154));
#50193=CARTESIAN_POINT('Ctrl Pts',(22.3630265717229,2.24226337611281,38.1915029857483));
#50194=CARTESIAN_POINT('Ctrl Pts',(22.3647585706317,2.24649982730801,38.1122855404265));
#50195=CARTESIAN_POINT('Ctrl Pts',(22.3625286523006,2.2507362785032,38.0333006150055));
#50196=CARTESIAN_POINT('Ctrl Pts',(22.3605019315261,2.25458669021025,37.9615130580364));
#50197=CARTESIAN_POINT('Ctrl Pts',(22.3552031283345,2.2584371019173,37.8899178042344));
#50198=CARTESIAN_POINT('Ctrl Pts',(22.3466858523132,2.26228751362435,37.8188310979975));
#50199=CARTESIAN_POINT('Ctrl Pts',(22.3373120035765,2.26652515683622,37.740595282958));
#50200=CARTESIAN_POINT('Ctrl Pts',(22.324003842043,2.27076280004809,37.6626818952908));
#50201=CARTESIAN_POINT('Ctrl Pts',(22.3067938993386,2.27500044325996,37.5855173988616));
#50202=CARTESIAN_POINT('Ctrl Pts',(22.2896087051605,2.27923199258609,37.5084638677971));
#50203=CARTESIAN_POINT('Ctrl Pts',(22.2685329737471,2.28346354191222,37.4321575430333));
#50204=CARTESIAN_POINT('Ctrl Pts',(22.2436508812131,2.28769509123835,37.3570187323144));
#50205=CARTESIAN_POINT('Ctrl Pts',(22.2187975281099,2.29192175302061,37.2819667087757));
#50206=CARTESIAN_POINT('Ctrl Pts',(22.1901466973382,2.29614841480287,37.2080799622139));
#50207=CARTESIAN_POINT('Ctrl Pts',(22.1578330354633,2.30037507658513,37.1357660906381));
#50208=CARTESIAN_POINT('Ctrl Pts',(22.1255397709241,2.30459907037389,37.0634978657096));
#50209=CARTESIAN_POINT('Ctrl Pts',(22.0895884552659,2.30882306416266,36.9928009719466));
#50210=CARTESIAN_POINT('Ctrl Pts',(22.0501623160007,2.31304705795142,36.9240642368945));
#50211=CARTESIAN_POINT('Ctrl Pts',(22.0107487880241,2.31726970060601,36.8553494887479));
#50212=CARTESIAN_POINT('Ctrl Pts',(21.9678628767205,2.32149234326059,36.7885940605554));
#50213=CARTESIAN_POINT('Ctrl Pts',(21.9217336430263,2.32571498591517,36.7241619840399));
#50214=CARTESIAN_POINT('Ctrl Pts',(21.8756048023846,2.32993759258995,36.6597304565298));
#50215=CARTESIAN_POINT('Ctrl Pts',(21.8262329683468,2.33416019926473,36.5976226216611));
#50216=CARTESIAN_POINT('Ctrl Pts',(21.7738895251984,2.33838280593951,36.5381720986961));
#50217=CARTESIAN_POINT('Ctrl Pts',(21.7214940332192,2.34260961145423,36.4786624598224));
#50218=CARTESIAN_POINT('Ctrl Pts',(21.6661213402309,2.34683641696896,36.4218157636223));
#50219=CARTESIAN_POINT('Ctrl Pts',(21.6080815964379,2.35106322248368,36.3679307115194));
#50220=CARTESIAN_POINT('Ctrl Pts',(21.5500137275854,2.35529207623551,36.314019547649));
#50221=CARTESIAN_POINT('Ctrl Pts',(21.4892765929159,2.35952092998734,36.2630731885298));
#50222=CARTESIAN_POINT('Ctrl Pts',(21.4262135662216,2.36374978373917,36.2153500843856));
#50223=CARTESIAN_POINT('Ctrl Pts',(21.3630372015836,2.36798623765886,36.1675412114672));
#50224=CARTESIAN_POINT('Ctrl Pts',(21.297526981097,2.37222269157856,36.1229674326072));
#50225=CARTESIAN_POINT('Ctrl Pts',(21.2300552007382,2.37645914549825,36.0818437513322));
#50226=CARTESIAN_POINT('Ctrl Pts',(21.1687320949326,2.38030953317998,36.0444676535839));
#50227=CARTESIAN_POINT('Ctrl Pts',(21.1057892168215,2.3841599208617,36.0099410418537));
#50228=CARTESIAN_POINT('Ctrl Pts',(21.0415210293745,2.38801030854343,35.9783910854565));
#50229=CARTESIAN_POINT('Ctrl Pts',(20.970789036555,2.39224795090858,35.9436679762793));
#50230=CARTESIAN_POINT('Ctrl Pts',(20.8981859316676,2.39648559327372,35.9124207415185));
#50231=CARTESIAN_POINT('Ctrl Pts',(20.8240871693434,2.40072323563887,35.8848542309312));
#50232=CARTESIAN_POINT('Ctrl Pts',(20.7500949639096,2.40495478411016,35.8573273620538));
#50233=CARTESIAN_POINT('Ctrl Pts',(20.6746118080797,2.40918633258145,35.8334708679945));
#50234=CARTESIAN_POINT('Ctrl Pts',(20.5980361042617,2.41341788105274,35.8134429246355));
#50235=CARTESIAN_POINT('Ctrl Pts',(20.5215488474356,2.41764454197204,35.7934381140883));
#50236=CARTESIAN_POINT('Ctrl Pts',(20.4439720016012,2.42187120289134,35.7772531844735));
#50237=CARTESIAN_POINT('Ctrl Pts',(20.3657207802558,2.42609786381065,35.7649970552933));
#50238=CARTESIAN_POINT('Ctrl Pts',(20.2875189534818,2.43032185673192,35.7527486625578));
#50239=CARTESIAN_POINT('Ctrl Pts',(20.2086440580531,2.43454584965319,35.7444242201197));
#50240=CARTESIAN_POINT('Ctrl Pts',(20.1295220058824,2.43876984257446,35.7400816770718));
#50241=CARTESIAN_POINT('Ctrl Pts',(20.0504252626488,2.44299248435824,35.7357405230824));
#50242=CARTESIAN_POINT('Ctrl Pts',(19.9710819873992,2.44721512614202,35.7353787648406));
#50243=CARTESIAN_POINT('Ctrl Pts',(19.8919222404062,2.4514377679258,35.7390024060196));
#50244=CARTESIAN_POINT('Ctrl Pts',(19.8127631679478,2.45566037372769,35.7426260163209));
#50245=CARTESIAN_POINT('Ctrl Pts',(19.7337880888534,2.45988297952957,35.7502349356552));
#50246=CARTESIAN_POINT('Ctrl Pts',(19.6554245894791,2.46410558533146,35.7617831094263));
#50247=CARTESIAN_POINT('Ctrl Pts',(19.5769831676012,2.46833238997615,35.773342766383));
#50248=CARTESIAN_POINT('Ctrl Pts',(19.4991550050446,2.47255919462084,35.7888494336711));
#50249=CARTESIAN_POINT('Ctrl Pts',(19.4223594983946,2.47678599926553,35.8082055302002));
#50250=CARTESIAN_POINT('Ctrl Pts',(19.3455267779548,2.4810148521475,35.8275710063628));
#50251=CARTESIAN_POINT('Ctrl Pts',(19.2697281590817,2.48524370502947,35.8507894903244));
#50252=CARTESIAN_POINT('Ctrl Pts',(19.1953673577147,2.48947255791144,35.8777136206445));
#50253=CARTESIAN_POINT('Ctrl Pts',(19.1208729136391,2.49370901097178,35.9046861395462));
#50254=CARTESIAN_POINT('Ctrl Pts',(19.0478218835058,2.49794546403211,35.9353774298504));
#50255=CARTESIAN_POINT('Ctrl Pts',(18.9765972806018,2.50218191709245,35.9695922186519));
#50256=CARTESIAN_POINT('Ctrl Pts',(18.911863201522,2.50603231254914,36.0006890974505));
#50257=CARTESIAN_POINT('Ctrl Pts',(18.8486377701117,2.50988270800582,36.03469583917));
#50258=CARTESIAN_POINT('Ctrl Pts',(18.7871879528988,2.51373310346251,36.0714346499789));
#50259=CARTESIAN_POINT('Ctrl Pts',(18.7195579291215,2.51797074562482,36.1118684016359));
#50260=CARTESIAN_POINT('Ctrl Pts',(18.6538251905401,2.52220838778714,36.155763810211));
#50261=CARTESIAN_POINT('Ctrl Pts',(18.590365952264,2.52644602994945,36.2029174260556));
#50262=CARTESIAN_POINT('Ctrl Pts',(18.5269979709271,2.53067757821175,36.2500032331026));
#50263=CARTESIAN_POINT('Ctrl Pts',(18.4658973703607,2.53490912647406,36.3003376653042));
#50264=CARTESIAN_POINT('Ctrl Pts',(18.4074137037711,2.53914067473636,36.353672616614));
#50265=CARTESIAN_POINT('Ctrl Pts',(18.3489975875033,2.54336733543837,36.4069459645166));
#50266=CARTESIAN_POINT('Ctrl Pts',(18.2931927430933,2.54759399614038,36.4632126300605));
#50267=CARTESIAN_POINT('Ctrl Pts',(18.2403165550457,2.55182065684239,36.5221835929191));
#50268=CARTESIAN_POINT('Ctrl Pts',(18.187473744134,2.5560446495414,36.5811173314256));
#50269=CARTESIAN_POINT('Ctrl Pts',(18.1375562323235,2.56026864224041,36.6427516308589));
#50270=CARTESIAN_POINT('Ctrl Pts',(18.0908444702271,2.56449263493942,36.7067607513289));
#50271=CARTESIAN_POINT('Ctrl Pts',(18.0441476499725,2.56871527649628,36.7707493969954));
#50272=CARTESIAN_POINT('Ctrl Pts',(18.0006548192613,2.57293791805314,36.8371109768091));
#50273=CARTESIAN_POINT('Ctrl Pts',(17.9606051114807,2.57716055961,36.9054879952125));
#50274=CARTESIAN_POINT('Ctrl Pts',(17.9205557450123,2.58138316518061,36.9738644308923));
#50275=CARTESIAN_POINT('Ctrl Pts',(17.8839496788187,2.58560577075122,37.0442558657929));
#50276=CARTESIAN_POINT('Ctrl Pts',(17.8509810296547,2.58982837632183,37.1162785424746));
#50277=CARTESIAN_POINT('Ctrl Pts',(17.8179795974141,2.59405518072996,37.1883728364345));
#50278=CARTESIAN_POINT('Ctrl Pts',(17.7886230026289,2.5982819851381,37.2621011850176));
#50279=CARTESIAN_POINT('Ctrl Pts',(17.7630576801667,2.60250878954623,37.3370586532119));
#50280=CARTESIAN_POINT('Ctrl Pts',(17.7374799692052,2.60673764218838,37.4120524444582));
#50281=CARTESIAN_POINT('Ctrl Pts',(17.7156973194211,2.61096649483052,37.4882760905327));
#50282=CARTESIAN_POINT('Ctrl Pts',(17.6978058710282,2.61519534747267,37.5653107131916));
#50283=CARTESIAN_POINT('Ctrl Pts',(17.6798822677788,2.61943180029042,37.6424837839614));
#50284=CARTESIAN_POINT('Ctrl Pts',(17.665863922428,2.62366825310818,37.720470281074));
#50285=CARTESIAN_POINT('Ctrl Pts',(17.655795514626,2.62790470592593,37.7988426131532));
#50286=CARTESIAN_POINT('Ctrl Pts',(17.6466446108514,2.63175510341115,37.8700731079398));
#50287=CARTESIAN_POINT('Ctrl Pts',(17.6407559108034,2.63560550089637,37.941621989365));
#50288=CARTESIAN_POINT('Ctrl Pts',(17.6381255883642,2.63945589838159,38.0131685278254));
#50289=CARTESIAN_POINT('Ctrl Pts',(17.6370685010235,2.6410033156783,38.0419220140714));
#50290=CARTESIAN_POINT('Ctrl Pts',(17.6365364592934,2.64255073297501,38.0706949209532));
#50291=CARTESIAN_POINT('Ctrl Pts',(17.6365300584561,2.64409815027172,38.0994743401003));
#50292=CARTESIAN_POINT('',(17.6365305931584,3.43784812059947,38.0983255377209));
#50293=CARTESIAN_POINT('Ctrl Pts',(17.6365300584559,2.64409815030312,38.0994743406844));
#50294=CARTESIAN_POINT('Ctrl Pts',(17.6365126342479,2.64831049778694,38.1778170825479));
#50295=CARTESIAN_POINT('Ctrl Pts',(17.640394763803,2.65252284527075,38.2563144725919));
#50296=CARTESIAN_POINT('Ctrl Pts',(17.6481964798018,2.65673519275457,38.3345434784501));
#50297=CARTESIAN_POINT('Ctrl Pts',(17.6559871178273,2.66094155895511,38.4126614037658));
#50298=CARTESIAN_POINT('Ctrl Pts',(17.6676862462287,2.66514792515566,38.4905112328437));
#50299=CARTESIAN_POINT('Ctrl Pts',(17.6832618833385,2.66935429135621,38.5676696908159));
#50300=CARTESIAN_POINT('Ctrl Pts',(17.698820203847,2.67355598102465,38.6447423659561));
#50301=CARTESIAN_POINT('Ctrl Pts',(17.7182463777624,2.67775767069309,38.7211247337187));
#50302=CARTESIAN_POINT('Ctrl Pts',(17.7414567754773,2.68195936036154,38.7963999884138));
#50303=CARTESIAN_POINT('Ctrl Pts',(17.7646533659365,2.68615855055519,38.8716304638376));
#50304=CARTESIAN_POINT('Ctrl Pts',(17.7916295736728,2.69035774074883,38.9457546802339));
#50305=CARTESIAN_POINT('Ctrl Pts',(17.8222512861565,2.69455693094248,39.0183686516063));
#50306=CARTESIAN_POINT('Ctrl Pts',(17.8528646098222,2.698754970768,39.0909627303815));
#50307=CARTESIAN_POINT('Ctrl Pts',(17.8871212708334,2.70295301059351,39.1620469482083));
#50308=CARTESIAN_POINT('Ctrl Pts',(17.9248387147748,2.70715105041902,39.2312365275231));
#50309=CARTESIAN_POINT('Ctrl Pts',(17.9625579303584,2.71134928743246,39.3004293567713));
#50310=CARTESIAN_POINT('Ctrl Pts',(18.0037380224241,2.7155475244459,39.3677269548083));
#50311=CARTESIAN_POINT('Ctrl Pts',(18.0481508620189,2.71974576145934,39.4327698163834));
#50312=CARTESIAN_POINT('Ctrl Pts',(18.0926089584444,2.7239482764902,39.4978789568498));
#50313=CARTESIAN_POINT('Ctrl Pts',(18.1403061098576,2.72815079152106,39.5607283814506));
#50314=CARTESIAN_POINT('Ctrl Pts',(18.1909717149057,2.73235330655192,39.6209888574966));
#50315=CARTESIAN_POINT('Ctrl Pts',(18.2416652800875,2.7365581407672,39.6812825886664));
#50316=CARTESIAN_POINT('Ctrl Pts',(18.2953302355493,2.74076297498247,39.7389841801321));
#50317=CARTESIAN_POINT('Ctrl Pts',(18.3516584349362,2.74496780919775,39.793800615711));
#50318=CARTESIAN_POINT('Ctrl Pts',(18.4080820901582,2.74917976907949,39.8487099452346));
#50319=CARTESIAN_POINT('Ctrl Pts',(18.4671776426322,2.75339172896124,39.9007240446893));
#50320=CARTESIAN_POINT('Ctrl Pts',(18.5286035805689,2.75760368884298,39.9495899593654));
#50321=CARTESIAN_POINT('Ctrl Pts',(18.5654274319154,2.76012869032888,39.9788842809239));
#50322=CARTESIAN_POINT('Ctrl Pts',(18.6030881936985,2.76265369181477,40.0070480259098));
#50323=CARTESIAN_POINT('Ctrl Pts',(18.6415077282651,2.76517869330067,40.0340344331311));
#50324=CARTESIAN_POINT('Ctrl Pts',(18.7059862041131,2.76941633566571,40.0793249975762));
#50325=CARTESIAN_POINT('Ctrl Pts',(18.7728530917134,2.77365397803075,40.1214725932932));
#50326=CARTESIAN_POINT('Ctrl Pts',(18.8417693212833,2.77789162039579,40.160216526431));
#50327=CARTESIAN_POINT('Ctrl Pts',(18.9105864466124,2.78212316886492,40.1989047442735));
#50328=CARTESIAN_POINT('Ctrl Pts',(18.9814466561246,2.78635471733404,40.2341987919326));
#50329=CARTESIAN_POINT('Ctrl Pts',(19.0539809595455,2.79058626580317,40.2658805174796));
#50330=CARTESIAN_POINT('Ctrl Pts',(19.1264314838471,2.79481292671721,40.2975256497605));
#50331=CARTESIAN_POINT('Ctrl Pts',(19.2005518320499,2.79903958763125,40.3255665647168));
#50332=CARTESIAN_POINT('Ctrl Pts',(19.2759487543359,2.80326624854529,40.3498311568987));
#50333=CARTESIAN_POINT('Ctrl Pts',(19.3512980837379,2.8074902414594,40.3740804325149));
#50334=CARTESIAN_POINT('Ctrl Pts',(19.427921942706,2.81171423437352,40.394557973569));
#50335=CARTESIAN_POINT('Ctrl Pts',(19.5054085940351,2.81593822728763,40.4111403639861));
#50336=CARTESIAN_POINT('Ctrl Pts',(19.5828704595116,2.82016086906237,40.4277174501517));
#50337=CARTESIAN_POINT('Ctrl Pts',(19.6611941112365,2.82438351083711,40.4404017618673));
#50338=CARTESIAN_POINT('Ctrl Pts',(19.739955643659,2.82860615261186,40.4491205532359));
#50339=CARTESIAN_POINT('Ctrl Pts',(19.818716504905,2.83282875840281,40.4578392703061));
#50340=CARTESIAN_POINT('Ctrl Pts',(19.8979147733456,2.83705136419377,40.4625924840629));
#50341=CARTESIAN_POINT('Ctrl Pts',(19.9771208994181,2.84127396998473,40.4633592591175));
#50342=CARTESIAN_POINT('Ctrl Pts',(20.0564057858247,2.84550077461559,40.4641267966317));
#50343=CARTESIAN_POINT('Ctrl Pts',(20.1356980756293,2.84972757924645,40.4608999727833));
#50344=CARTESIAN_POINT('Ctrl Pts',(20.2145683043251,2.8539543838773,40.4537100254023));
#50345=CARTESIAN_POINT('Ctrl Pts',(20.2934767521556,2.85818323674383,40.4465165938983));
#50346=CARTESIAN_POINT('Ctrl Pts',(20.3719622667441,2.86241208961035,40.435356279158));
#50347=CARTESIAN_POINT('Ctrl Pts',(20.4496031398418,2.86664094247688,40.420311931087));
#50348=CARTESIAN_POINT('Ctrl Pts',(20.5273835506115,2.87087739551919,40.4052405450239));
#50349=CARTESIAN_POINT('Ctrl Pts',(20.6043158305455,2.87511384856151,40.3862712904857));
#50350=CARTESIAN_POINT('Ctrl Pts',(20.6799912790346,2.87935030160383,40.3635375634915));
#50351=CARTESIAN_POINT('Ctrl Pts',(20.7487706107861,2.88320069714247,40.3428755048965));
#50352=CARTESIAN_POINT('Ctrl Pts',(20.8165116962031,2.88705109268111,40.3191045291742));
#50353=CARTESIAN_POINT('Ctrl Pts',(20.882923187911,2.89090148821975,40.2923587948028));
#50354=CARTESIAN_POINT('Ctrl Pts',(20.956013899517,2.89513913057119,40.2629231548652));
#50355=CARTESIAN_POINT('Ctrl Pts',(21.0277681739357,2.89937677292263,40.2297731241964));
#50356=CARTESIAN_POINT('Ctrl Pts',(21.0977827558158,2.90361441527406,40.1930512325152));
#50357=CARTESIAN_POINT('Ctrl Pts',(21.1676966539706,2.90784596372896,40.1563821483601));
#50358=CARTESIAN_POINT('Ctrl Pts',(21.235875416115,2.91207751218385,40.1161516196961));
#50359=CARTESIAN_POINT('Ctrl Pts',(21.30193518715,2.91630906063874,40.0725504326533));
#50360=CARTESIAN_POINT('Ctrl Pts',(21.3679186573145,2.92053572153763,40.0289996061926));
#50361=CARTESIAN_POINT('Ctrl Pts',(21.4317876108973,2.92476238243652,39.9820861150492));
#50362=CARTESIAN_POINT('Ctrl Pts',(21.4931836143664,2.92898904333542,39.9320461606324));
#50363=CARTESIAN_POINT('Ctrl Pts',(21.554540862759,2.93321303623384,39.8820377929988));
#50364=CARTESIAN_POINT('Ctrl Pts',(21.6134278970377,2.93743702913226,39.8289071746988));
#50365=CARTESIAN_POINT('Ctrl Pts',(21.6695170642665,2.94166102203068,39.7729325189687));
#50366=CARTESIAN_POINT('Ctrl Pts',(21.7255882901034,2.9458836637892,39.7169757680014));
#50367=CARTESIAN_POINT('Ctrl Pts',(21.7788630945344,2.95010630554772,39.658177117043));
#50368=CARTESIAN_POINT('Ctrl Pts',(21.8290497065301,2.95432894730624,39.5968525685391));
#50369=CARTESIAN_POINT('Ctrl Pts',(21.8792358908482,2.95855155308047,39.5355285426276));
#50370=CARTESIAN_POINT('Ctrl Pts',(21.926333639276,2.96277415885471,39.4716790256496));
#50371=CARTESIAN_POINT('Ctrl Pts',(21.9700915707039,2.96699676462894,39.4056529569305));
#50372=CARTESIAN_POINT('Ctrl Pts',(22.0138930137757,2.97122356924239,39.3395612337644));
#50373=CARTESIAN_POINT('Ctrl Pts',(22.0543477465301,2.97545037385585,39.2712890273145));
#50374=CARTESIAN_POINT('Ctrl Pts',(22.0912482005776,2.9796771784693,39.2012136052923));
#50375=CARTESIAN_POINT('Ctrl Pts',(22.128166535937,2.98390603131803,39.1311042259516));
#50376=CARTESIAN_POINT('Ctrl Pts',(22.1615269639637,2.98813488416676,39.0591903161031));
#50377=CARTESIAN_POINT('Ctrl Pts',(22.1911694339725,2.99236373701548,38.9858707312722));
#50378=CARTESIAN_POINT('Ctrl Pts',(22.220865177996,2.99660019003953,38.9124193750795));
#50379=CARTESIAN_POINT('Ctrl Pts',(22.2468294587741,3.00083664306357,38.8375577400424));
#50380=CARTESIAN_POINT('Ctrl Pts',(22.268951707638,3.00507309608762,38.7617012840448));
#50381=CARTESIAN_POINT('Ctrl Pts',(22.289058011439,3.00892349177136,38.6927574366568));
#50382=CARTESIAN_POINT('Ctrl Pts',(22.3059911908141,3.01277388745509,38.6229922463347));
#50383=CARTESIAN_POINT('Ctrl Pts',(22.3197051962276,3.01662428313883,38.5527231422126));
#50384=CARTESIAN_POINT('Ctrl Pts',(22.3347984633941,3.02086192553427,38.4753868476661));
#50385=CARTESIAN_POINT('Ctrl Pts',(22.3460483782244,3.02509956792971,38.3971497721236));
#50386=CARTESIAN_POINT('Ctrl Pts',(22.3533549980713,3.02933721032515,38.3184277774291));
#50387=CARTESIAN_POINT('Ctrl Pts',(22.3606511107127,3.03356875882481,38.2398189880471));
#50388=CARTESIAN_POINT('Ctrl Pts',(22.3640151467171,3.03780030732446,38.160727127262));
#50389=CARTESIAN_POINT('Ctrl Pts',(22.3633982044233,3.04203185582412,38.0815780503533));
#50390=CARTESIAN_POINT('Ctrl Pts',(22.3627819747148,3.04625851676872,38.0025203928082));
#50391=CARTESIAN_POINT('Ctrl Pts',(22.3581939080036,3.05048517771332,37.9234061168559));
#50392=CARTESIAN_POINT('Ctrl Pts',(22.3496370378967,3.05471183865792,37.8446644735964));
#50393=CARTESIAN_POINT('Ctrl Pts',(22.3410855691526,3.0589358316026,37.7659725345124));
#50394=CARTESIAN_POINT('Ctrl Pts',(22.3285703201331,3.06315982454729,37.6876532260512));
#50395=CARTESIAN_POINT('Ctrl Pts',(22.3121463217775,3.06738381749197,37.6101328469975));
#50396=CARTESIAN_POINT('Ctrl Pts',(22.2957275770082,3.07160645929725,37.5326372645854));
#50397=CARTESIAN_POINT('Ctrl Pts',(22.2754026628456,3.07582910110253,37.455940562361));
#50398=CARTESIAN_POINT('Ctrl Pts',(22.2512778421683,3.0800517429078,37.3804595089489));
#50399=CARTESIAN_POINT('Ctrl Pts',(22.2271532270742,3.08427434872922,37.3049790987599));
#50400=CARTESIAN_POINT('Ctrl Pts',(22.1992289139255,3.08849695455063,37.2307147628709));
#50401=CARTESIAN_POINT('Ctrl Pts',(22.1676607809497,3.09271956037204,37.1580673168254));
#50402=CARTESIAN_POINT('Ctrl Pts',(22.1360612575172,3.09694636503301,37.0853476322185));
#50403=CARTESIAN_POINT('Ctrl Pts',(22.1008108639355,3.10117316969397,37.0142484799576));
#50404=CARTESIAN_POINT('Ctrl Pts',(22.0621130910175,3.10539997435494,36.9451493426618));
#50405=CARTESIAN_POINT('Ctrl Pts',(22.0233965658362,3.10962882725143,36.876016721134));
#50406=CARTESIAN_POINT('Ctrl Pts',(21.9812295830714,3.11385768014793,36.8088864427421));
#50407=CARTESIAN_POINT('Ctrl Pts',(21.9358596084275,3.11808653304443,36.744109880057));
#50408=CARTESIAN_POINT('Ctrl Pts',(21.8904080939984,3.12232298611613,36.6792168996961));
#50409=CARTESIAN_POINT('Ctrl Pts',(21.8417423742846,3.12655943918783,36.6166864580939));
#50410=CARTESIAN_POINT('Ctrl Pts',(21.7901507769903,3.13079589225953,36.556837456215));
#50411=CARTESIAN_POINT('Ctrl Pts',(21.7432605981942,3.13464628752565,36.5024423503053));
#50412=CARTESIAN_POINT('Ctrl Pts',(21.6939541776096,3.13849668279178,36.4502619890175));
#50413=CARTESIAN_POINT('Ctrl Pts',(21.642472729767,3.14234707805791,36.4005077896996));
#50414=CARTESIAN_POINT('Ctrl Pts',(21.5858136208204,3.14658472043226,36.3457496444291));
#50415=CARTESIAN_POINT('Ctrl Pts',(21.5263068026791,3.1508223628066,36.2937252357204));
#50416=CARTESIAN_POINT('Ctrl Pts',(21.4642467260256,3.15506000518095,36.244744770598));
#50417=CARTESIAN_POINT('Ctrl Pts',(21.402275894198,3.15929155365925,36.1958347413069));
#50418=CARTESIAN_POINT('Ctrl Pts',(21.3377594604198,3.16352310213755,36.1499602506902));
#50419=CARTESIAN_POINT('Ctrl Pts',(21.2710280419653,3.16775465061585,36.1073941289262));
#50420=CARTESIAN_POINT('Ctrl Pts',(21.2043737001417,3.17198131153881,36.0648771722082));
#50421=CARTESIAN_POINT('Ctrl Pts',(21.135509850979,3.17620797246177,36.0256612413644));
#50422=CARTESIAN_POINT('Ctrl Pts',(21.0647982306072,3.18043463338473,35.9899774482258));
#50423=CARTESIAN_POINT('Ctrl Pts',(20.9941312456137,3.18465862630761,35.9543161798094));
#50424=CARTESIAN_POINT('Ctrl Pts',(20.9216192219379,3.18888261923048,35.9221828342385));
#50425=CARTESIAN_POINT('Ctrl Pts',(20.8476497231039,3.19310661215335,35.8937632974176));
#50426=CARTESIAN_POINT('Ctrl Pts',(20.773703885085,3.19732925393668,35.8653528512274));
#50427=CARTESIAN_POINT('Ctrl Pts',(20.6983019349738,3.20155189572001,35.8406540227646));
#50428=CARTESIAN_POINT('Ctrl Pts',(20.6218513291174,3.20577453750334,35.8198045335158));
#50429=CARTESIAN_POINT('Ctrl Pts',(20.545401374748,3.2099971433027,35.7989552219395));
#50430=CARTESIAN_POINT('Ctrl Pts',(20.4679032350335,3.21421974910206,35.7819553063147));
#50431=CARTESIAN_POINT('Ctrl Pts',(20.3897779911959,3.21844235490142,35.7688922035909));
#50432=CARTESIAN_POINT('Ctrl Pts',(20.3115750618297,3.22266915954033,35.7558161112879));
#50433=CARTESIAN_POINT('Ctrl Pts',(20.2327442461769,3.22689596417925,35.7466847289162));
#50434=CARTESIAN_POINT('Ctrl Pts',(20.1537146471826,3.23112276881816,35.7415339205022));
#50435=CARTESIAN_POINT('Ctrl Pts',(20.0746467518291,3.23535162169255,35.7363806160967));
#50436=CARTESIAN_POINT('Ctrl Pts',(19.9953803505619,3.23958047456695,35.7352117351967));
#50437=CARTESIAN_POINT('Ctrl Pts',(19.9163449028138,3.24380932744135,35.7380109514194));
#50438=CARTESIAN_POINT('Ctrl Pts',(19.8371674110449,3.24804578049114,35.7408151984471));
#50439=CARTESIAN_POINT('Ctrl Pts',(19.7582221703125,3.25228223354094,35.747601751861));
#50440=CARTESIAN_POINT('Ctrl Pts',(19.6799336433097,3.25651868659074,35.7583023320217));
#50441=CARTESIAN_POINT('Ctrl Pts',(19.6087793579768,3.26036908205282,35.7680277945273));
#50442=CARTESIAN_POINT('Ctrl Pts',(19.5381677039131,3.26421947751491,35.7809857284757));
#50443=CARTESIAN_POINT('Ctrl Pts',(19.4684073339674,3.26806987297699,35.7970888687749));
#50444=CARTESIAN_POINT('Ctrl Pts',(19.3916309345943,3.27230751535147,35.8148115547604));
#50445=CARTESIAN_POINT('Ctrl Pts',(19.3155976689195,3.27654515772595,35.836411161631));
#50446=CARTESIAN_POINT('Ctrl Pts',(19.2407280395302,3.28078280010044,35.8618095409585));
#50447=CARTESIAN_POINT('Ctrl Pts',(19.1659660756073,3.28501434857882,35.8871713964195));
#50448=CARTESIAN_POINT('Ctrl Pts',(19.0923648651002,3.2892458970572,35.9163210264038));
#50449=CARTESIAN_POINT('Ctrl Pts',(19.020333243132,3.29347744553558,35.9491295979563));
#50450=CARTESIAN_POINT('Ctrl Pts',(18.9483848196777,3.29770410645853,35.981900274702));
#50451=CARTESIAN_POINT('Ctrl Pts',(18.8780028064846,3.30193076738147,36.018321301211));
#50452=CARTESIAN_POINT('Ctrl Pts',(18.8095779816057,3.30615742830442,36.05821503115));
#50453=CARTESIAN_POINT('Ctrl Pts',(18.7411963486092,3.31038142122723,36.0980835789229));
#50454=CARTESIAN_POINT('Ctrl Pts',(18.6747698556288,3.31460541415005,36.1414202435998));
#50455=CARTESIAN_POINT('Ctrl Pts',(18.6106654009218,3.31882940707286,36.1880010950044));
#50456=CARTESIAN_POINT('Ctrl Pts',(18.5465814514735,3.32305204885607,36.234567046471));
#50457=CARTESIAN_POINT('Ctrl Pts',(18.4848184442857,3.32727469063928,36.2843748485822));
#50458=CARTESIAN_POINT('Ctrl Pts',(18.4257137024169,3.33149733242249,36.3371576661136));
#50459=CARTESIAN_POINT('Ctrl Pts',(18.3666094642199,3.33571993822169,36.3899400338466));
#50460=CARTESIAN_POINT('Ctrl Pts',(18.3101637949927,3.33994254402088,36.4456970532807));
#50461=CARTESIAN_POINT('Ctrl Pts',(18.2566792354514,3.34416514982008,36.5041230771787));
#50462=CARTESIAN_POINT('Ctrl Pts',(18.2031414923808,3.34839195445873,36.562607198258));
#50463=CARTESIAN_POINT('Ctrl Pts',(18.1525710577994,3.35261875909739,36.623765278567));
#50464=CARTESIAN_POINT('Ctrl Pts',(18.1052315928562,3.35684556373604,36.687256879617));
#50465=CARTESIAN_POINT('Ctrl Pts',(18.0578691880381,3.36107441661013,36.7507792475839));
#50466=CARTESIAN_POINT('Ctrl Pts',(18.0137411331327,3.36530326948422,36.8166369990124));
#50467=CARTESIAN_POINT('Ctrl Pts',(17.9730675024953,3.36953212235831,36.8844609872738));
#50468=CARTESIAN_POINT('Ctrl Pts',(17.9323207724304,3.37376857540772,36.9524068701051));
#50469=CARTESIAN_POINT('Ctrl Pts',(17.8950410926088,3.37800502845714,37.0223256359311));
#50470=CARTESIAN_POINT('Ctrl Pts',(17.8614022355798,3.38224148150655,37.0938240497224));
#50471=CARTESIAN_POINT('Ctrl Pts',(17.83082880517,3.38609187696972,37.1588069882503));
#50472=CARTESIAN_POINT('Ctrl Pts',(17.8032623637644,3.3899422724329,37.2250942800547));
#50473=CARTESIAN_POINT('Ctrl Pts',(17.7787977182185,3.39379266789607,37.2923795047743));
#50474=CARTESIAN_POINT('Ctrl Pts',(17.747710668165,3.398685337862,37.3778783584077));
#50475=CARTESIAN_POINT('Ctrl Pts',(17.7215354524299,3.40357800782793,37.4652526455507));
#50476=CARTESIAN_POINT('Ctrl Pts',(17.7004693699155,3.40847067779385,37.5539694860147));
#50477=CARTESIAN_POINT('Ctrl Pts',(17.6793879141012,3.41336691826146,37.6427510689668));
#50478=CARTESIAN_POINT('Ctrl Pts',(17.6634232143288,3.41826315872906,37.7328770278252));
#50479=CARTESIAN_POINT('Ctrl Pts',(17.6527251187551,3.42315939919666,37.823791613493));
#50480=CARTESIAN_POINT('Ctrl Pts',(17.6420270231814,3.42805563966427,37.9147061991608));
#50481=CARTESIAN_POINT('Ctrl Pts',(17.6365957136741,3.43295188013187,38.0064092559421));
#50482=CARTESIAN_POINT('Ctrl Pts',(17.6365305931584,3.43784812059947,38.0983255377209));
#50483=CARTESIAN_POINT('',(17.6387453353606,4.23159815027171,38.101781203975));
#50484=CARTESIAN_POINT('Ctrl Pts',(17.6390002039829,3.43784815027172,38.0983278438321));
#50485=CARTESIAN_POINT('Ctrl Pts',(17.6423555560034,3.4650705877862,38.6088386346336));
#50486=CARTESIAN_POINT('Ctrl Pts',(18.0552834653053,3.53420062360702,39.910202051485));
#50487=CARTESIAN_POINT('Ctrl Pts',(20.1976448724621,3.64523825773423,40.8842741316918));
#50488=CARTESIAN_POINT('Ctrl Pts',(22.4432224513611,3.77096105265329,39.4497814596623));
#50489=CARTESIAN_POINT('Ctrl Pts',(22.4622207069824,3.89668384757238,36.7851938828303));
#50490=CARTESIAN_POINT('Ctrl Pts',(20.2373259792565,4.02240664249146,35.3188271691023));
#50491=CARTESIAN_POINT('Ctrl Pts',(18.0696336552147,4.13404474339124,36.2673539383482));
#50492=CARTESIAN_POINT('Ctrl Pts',(17.6424244891864,4.20377524598466,37.5801514847896));
#50493=CARTESIAN_POINT('Ctrl Pts',(17.6387453353606,4.23159815027171,38.101781203975));
#50494=CARTESIAN_POINT('',(17.6327380335352,5.02534815027172,38.1003247073934));
#50495=CARTESIAN_POINT('Ctrl Pts',(17.6387453353606,4.23159815027171,38.101781203975));
#50496=CARTESIAN_POINT('Ctrl Pts',(17.6368828498576,4.24568284429102,38.3658440390514));
#50497=CARTESIAN_POINT('Ctrl Pts',(17.7993870304845,4.30167513661668,39.4133737818963));
#50498=CARTESIAN_POINT('Ctrl Pts',(19.3334665954578,4.3995750272487,40.8105311576044));
#50499=CARTESIAN_POINT('Ctrl Pts',(21.9109589195357,4.52529782216778,40.1345716855284));
#50500=CARTESIAN_POINT('Ctrl Pts',(22.7469390798614,4.65102061708686,37.60444815888));
#50501=CARTESIAN_POINT('Ctrl Pts',(21.0795541642787,4.77674341200594,35.5259353655944));
#50502=CARTESIAN_POINT('Ctrl Pts',(18.4483093765511,4.9015192564009,35.791228794861));
#50503=CARTESIAN_POINT('Ctrl Pts',(17.6342141099641,4.98438750248949,37.3374076479298));
#50504=CARTESIAN_POINT('Ctrl Pts',(17.6327380335352,5.02534815027172,38.1003247073934));
#50505=CARTESIAN_POINT('',(17.6378382696348,5.81909815027172,38.0979654557371));
#50506=CARTESIAN_POINT('Ctrl Pts',(17.6327380335352,5.02534815027172,38.1003247073934));
#50507=CARTESIAN_POINT('Ctrl Pts',(17.6327039087979,5.02629510079585,38.1179622387422));
#50508=CARTESIAN_POINT('Ctrl Pts',(17.6408568301016,5.06914964962618,38.9161219948285));
#50509=CARTESIAN_POINT('Ctrl Pts',(18.5336418898511,5.15391179676333,40.4750873307105));
#50510=CARTESIAN_POINT('Ctrl Pts',(21.1941929599868,5.27963459168218,40.6229247135073));
#50511=CARTESIAN_POINT('Ctrl Pts',(22.7664414274776,5.40535738660137,38.4715477951031));
#50512=CARTESIAN_POINT('Ctrl Pts',(21.8175517653059,5.5310801815204,35.9815686189682));
#50513=CARTESIAN_POINT('Ctrl Pts',(19.2122745821007,5.65680297643949,35.4221772646974));
#50514=CARTESIAN_POINT('Ctrl Pts',(17.7709947773869,5.75280896602327,36.8585589655981));
#50515=CARTESIAN_POINT('Ctrl Pts',(17.6359459392263,5.80690735730068,37.8696316425113));
#50516=CARTESIAN_POINT('Ctrl Pts',(17.6378382696348,5.81909815027172,38.0979654557371));
#50517=CARTESIAN_POINT('',(17.6396768404944,6.61284815027172,38.1012519486375));
#50518=CARTESIAN_POINT('Ctrl Pts',(17.6378382696348,5.81909815027172,38.0979654557371));
#50519=CARTESIAN_POINT('Ctrl Pts',(17.6424510962582,5.84881495560703,38.654561855595));
#50520=CARTESIAN_POINT('Ctrl Pts',(18.1165213946417,5.9204393592487,40.0031607324733));
#50521=CARTESIAN_POINT('Ctrl Pts',(20.3621280800665,6.03397136119673,40.8676902264046));
#50522=CARTESIAN_POINT('Ctrl Pts',(22.5188448048673,6.15969415611581,39.3027746192458));
#50523=CARTESIAN_POINT('Ctrl Pts',(22.3800653672784,6.28541695103489,36.6417356950161));
#50524=CARTESIAN_POINT('Ctrl Pts',(20.0722634848505,6.41113974595397,35.3096552319713));
#50525=CARTESIAN_POINT('Ctrl Pts',(18.0116199776956,6.52028347903291,36.3608230696746));
#50526=CARTESIAN_POINT('Ctrl Pts',(17.641972639838,6.5875196138055,37.6259160691615));
#50527=CARTESIAN_POINT('Ctrl Pts',(17.6396768404944,6.61284815027172,38.1012519486375));
#50528=CARTESIAN_POINT('',(17.6333442921061,7.40659815027172,38.1011170196962));
#50529=CARTESIAN_POINT('Ctrl Pts',(17.6396768404944,6.61284815027172,38.1012519486375));
#50530=CARTESIAN_POINT('Ctrl Pts',(17.6381741007155,6.62942721211186,38.4123880836123));
#50531=CARTESIAN_POINT('Ctrl Pts',(17.8398734532478,6.68791387225836,39.5081257521821));
#50532=CARTESIAN_POINT('Ctrl Pts',(19.4950998583179,6.7883081307112,40.845236197969));
#50533=CARTESIAN_POINT('Ctrl Pts',(22.0280545809553,6.91403092563029,40.0178739667594));
#50534=CARTESIAN_POINT('Ctrl Pts',(22.7127844750115,7.03975372054937,37.4426976891526));
#50535=CARTESIAN_POINT('Ctrl Pts',(20.9252753729429,7.16547651546845,35.4665400287961));
#50536=CARTESIAN_POINT('Ctrl Pts',(18.3665453557022,7.28775799204257,35.8787305372433));
#50537=CARTESIAN_POINT('Ctrl Pts',(17.6375482172936,7.36813187031033,37.3841700502603));
#50538=CARTESIAN_POINT('Ctrl Pts',(17.6333442921061,7.40659815027172,38.1011170196962));
#50539=CARTESIAN_POINT('',(17.6364827852058,8.20034815027172,38.0978694718631));
#50540=CARTESIAN_POINT('Ctrl Pts',(17.6333442921061,7.40659815027172,38.1011170196962));
#50541=CARTESIAN_POINT('Ctrl Pts',(17.6329681953044,7.41003946861669,38.1652574242468));
#50542=CARTESIAN_POINT('Ctrl Pts',(17.6643665387496,7.45538838526801,39.010111409356));
#50543=CARTESIAN_POINT('Ctrl Pts',(18.6768195719384,7.54264490022567,40.5577305569364));
#50544=CARTESIAN_POINT('Ctrl Pts',(21.3414563833941,7.66836769514478,40.5478032411045));
#50545=CARTESIAN_POINT('Ctrl Pts',(22.7835851728612,7.79409049006385,38.3071219957784));
#50546=CARTESIAN_POINT('Ctrl Pts',(21.6889522413839,7.91981328498292,35.8776844818901));
#50547=CARTESIAN_POINT('Ctrl Pts',(19.0551282565062,8.04553607990202,35.4735074102416));
#50548=CARTESIAN_POINT('Ctrl Pts',(17.7365819503052,8.13904770166493,36.9532235056783));
#50549=CARTESIAN_POINT('Ctrl Pts',(17.6348288095622,8.19065172512151,37.9165204024922));
#50550=CARTESIAN_POINT('Ctrl Pts',(17.6364827852058,8.20034815027172,38.0978694718631));
#50551=CARTESIAN_POINT('',(17.6402258042432,8.99409815027172,38.1005671551939));
#50552=CARTESIAN_POINT('Ctrl Pts',(17.6364827852058,8.20034815027172,38.0978694718631));
#50553=CARTESIAN_POINT('Ctrl Pts',(17.6419772323887,8.23255932342787,38.700304512068));
#50554=CARTESIAN_POINT('Ctrl Pts',(18.1821171684312,8.30667809489039,40.0952851716237));
#50555=CARTESIAN_POINT('Ctrl Pts',(20.5253410324787,8.42270446465923,40.8413979527426));
#50556=CARTESIAN_POINT('Ctrl Pts',(22.5856316777532,8.54842725957834,39.1515487448081));
#50557=CARTESIAN_POINT('Ctrl Pts',(22.2895613506621,8.67415005449739,36.5033927354347));
#50558=CARTESIAN_POINT('Ctrl Pts',(19.9069475081291,8.79987284941649,35.3102711297575));
#50559=CARTESIAN_POINT('Ctrl Pts',(17.9577366623079,8.90652221467458,36.4548168564723));
#50560=CARTESIAN_POINT('Ctrl Pts',(17.6411507209954,8.97126398162633,37.6717931370567));
#50561=CARTESIAN_POINT('Ctrl Pts',(17.6402258042432,8.99409815027172,38.1005671551939));
#50562=CARTESIAN_POINT('',(17.6365306272256,9.78784815027173,38.1017218761687));
#50563=CARTESIAN_POINT('Ctrl Pts',(17.6402258042432,8.99409815027172,38.1005671551939));
#50564=CARTESIAN_POINT('Ctrl Pts',(17.6394532193119,9.0131715799327,38.4587230049819));
#50565=CARTESIAN_POINT('Ctrl Pts',(17.8840036200799,9.07415260790002,39.6028076270516));
#50566=CARTESIAN_POINT('Ctrl Pts',(19.6585041852042,9.17704123417373,40.8703116330452));
#50567=CARTESIAN_POINT('Ctrl Pts',(22.1380363316913,9.3027640290928,39.8944488234764));
#50568=CARTESIAN_POINT('Ctrl Pts',(22.6691140974391,9.42848682401188,37.2832528723284));
#50569=CARTESIAN_POINT('Ctrl Pts',(20.7677509459015,9.55420961893096,35.4163822141042));
#50570=CARTESIAN_POINT('Ctrl Pts',(18.2895222809352,9.67399640298303,35.9678425920262));
#50571=CARTESIAN_POINT('Ctrl Pts',(17.6399433145644,9.75187558872876,37.4304476506293));
#50572=CARTESIAN_POINT('Ctrl Pts',(17.6344290770428,9.78784717616812,38.1017052298117));
#50573=CARTESIAN_POINT('',(17.6365307901728,10.5815981503084,38.0980673595779));
#50574=CARTESIAN_POINT('Ctrl Pts',(17.6365306272256,9.78784815027173,38.1017218761687));
#50575=CARTESIAN_POINT('Ctrl Pts',(17.6366112510818,9.79378383643753,38.2123872180115));
#50576=CARTESIAN_POINT('Ctrl Pts',(17.6444651929882,9.79971952260332,38.3227723948623));
#50577=CARTESIAN_POINT('Ctrl Pts',(17.6599710750915,9.80565520876911,38.432046791118));
#50578=CARTESIAN_POINT('Ctrl Pts',(17.6710411319083,9.8098928511466,38.5100606549601));
#50579=CARTESIAN_POINT('Ctrl Pts',(17.6860375731455,9.81413049352408,38.5876667582401));
#50580=CARTESIAN_POINT('Ctrl Pts',(17.7049186169119,9.81836813590157,38.6644394439639));
#50581=CARTESIAN_POINT('Ctrl Pts',(17.7237725089964,9.82259968438302,38.7411017275527));
#50582=CARTESIAN_POINT('Ctrl Pts',(17.746499798886,9.82683123286447,38.8169325222216));
#50583=CARTESIAN_POINT('Ctrl Pts',(17.7730072060122,9.83106278134592,38.8915134467756));
#50584=CARTESIAN_POINT('Ctrl Pts',(17.7994839963513,9.83528944227202,38.9660082283023));
#50585=CARTESIAN_POINT('Ctrl Pts',(17.8297320711137,9.83951610319812,39.0392555691103));
#50586=CARTESIAN_POINT('Ctrl Pts',(17.8636079670862,9.84374276412422,39.1108508903901));
#50587=CARTESIAN_POINT('Ctrl Pts',(17.8974624795375,9.84796675705023,39.1824010184721));
#50588=CARTESIAN_POINT('Ctrl Pts',(17.9349400678453,9.85219074997625,39.2523007742551));
#50589=CARTESIAN_POINT('Ctrl Pts',(17.9758491067801,9.85641474290226,39.3201653995984));
#50590=CARTESIAN_POINT('Ctrl Pts',(18.0167450600346,9.86063738468872,39.3880083169082));
#50591=CARTESIAN_POINT('Ctrl Pts',(18.0610700424113,9.86486002647517,39.4538169953179));
#50592=CARTESIAN_POINT('Ctrl Pts',(18.1085871443441,9.86908266826163,39.5172324616518));
#50593=CARTESIAN_POINT('Ctrl Pts',(18.1561038413518,9.87330527406412,39.5806473875799));
#50594=CARTESIAN_POINT('Ctrl Pts',(18.2068123215903,9.8775278798666,39.6416687676949));
#50595=CARTESIAN_POINT('Ctrl Pts',(18.2604340223364,9.88175048566909,39.6999689529036));
#50596=CARTESIAN_POINT('Ctrl Pts',(18.3141090429816,9.88597729031107,39.7583271101636));
#50597=CARTESIAN_POINT('Ctrl Pts',(18.3707027524758,9.89020409495305,39.8139583216821));
#50598=CARTESIAN_POINT('Ctrl Pts',(18.4298985893385,9.89443089959503,39.8665706895392));
#50599=CARTESIAN_POINT('Ctrl Pts',(18.4891231114666,9.89865975247248,39.9192085524278));
#50600=CARTESIAN_POINT('Ctrl Pts',(18.5509519068367,9.90288860534993,39.9688243636632));
#50601=CARTESIAN_POINT('Ctrl Pts',(18.6150360720197,9.90711745822738,40.0151671882876));
#50602=CARTESIAN_POINT('Ctrl Pts',(18.6792354104909,9.91135391128016,40.0615933011234));
#50603=CARTESIAN_POINT('Ctrl Pts',(18.7456978237154,9.91559036433293,40.1047344181595));
#50604=CARTESIAN_POINT('Ctrl Pts',(18.8140464360769,9.91982681738571,40.1443836687662));
#50605=CARTESIAN_POINT('Ctrl Pts',(18.8761666063443,9.92367721281988,40.1804197800137));
#50606=CARTESIAN_POINT('Ctrl Pts',(18.9398443143707,9.92752760825404,40.2135719016388));
#50607=CARTESIAN_POINT('Ctrl Pts',(19.0047824039744,9.93137800368821,40.2437192860683));
#50608=CARTESIAN_POINT('Ctrl Pts',(19.0762515310092,9.93561564606571,40.2768986921873));
#50609=CARTESIAN_POINT('Ctrl Pts',(19.1495158714723,9.93985328844322,40.3065624231164));
#50610=CARTESIAN_POINT('Ctrl Pts',(19.2241956121396,9.94409093082072,40.3325138281042));
#50611=CARTESIAN_POINT('Ctrl Pts',(19.2987679604092,9.94832247930218,40.3584279139532));
#50612=CARTESIAN_POINT('Ctrl Pts',(19.3747512276241,9.95255402778364,40.380640122966));
#50613=CARTESIAN_POINT('Ctrl Pts',(19.4517436714328,9.95678557626511,40.3990009654383));
#50614=CARTESIAN_POINT('Ctrl Pts',(19.5286471868427,9.96101223719122,40.4173406006304));
#50615=CARTESIAN_POINT('Ctrl Pts',(19.6065571087742,9.96523889811733,40.4318376012495));
#50616=CARTESIAN_POINT('Ctrl Pts',(19.6850559570527,9.96946555904344,40.4423920873142));
#50617=CARTESIAN_POINT('Ctrl Pts',(19.7635052544119,9.97368955196946,40.4529399110583));
#50618=CARTESIAN_POINT('Ctrl Pts',(19.8425422768608,9.97791354489548,40.4595500976168));
#50619=CARTESIAN_POINT('Ctrl Pts',(19.9217399548449,9.98213753782151,40.4621739576569));
#50620=CARTESIAN_POINT('Ctrl Pts',(20.0009122996626,9.98636017960797,40.4647969783961));
#50621=CARTESIAN_POINT('Ctrl Pts',(20.0802447297881,9.99058282139444,40.4634361892354));
#50622=CARTESIAN_POINT('Ctrl Pts',(20.159307155965,9.9948054631809,40.4580949240771));
#50623=CARTESIAN_POINT('Ctrl Pts',(20.2383689083978,9.99902806898339,40.4527537044354));
#50624=CARTESIAN_POINT('Ctrl Pts',(20.3171601938467,10.0032506747859,40.4434321092631));
#50625=CARTESIAN_POINT('Ctrl Pts',(20.3952545265196,10.0074732805884,40.4301854647572));
#50626=CARTESIAN_POINT('Ctrl Pts',(20.4734265139831,10.0117000852304,40.4169256481635));
#50627=CARTESIAN_POINT('Ctrl Pts',(20.5508997010936,10.0159268898723,40.3997330646378));
#50628=CARTESIAN_POINT('Ctrl Pts',(20.6272569084859,10.0201536945143,40.3787143769364));
#50629=CARTESIAN_POINT('Ctrl Pts',(20.703651117243,10.0243825473918,40.3576855039472));
#50630=CARTESIAN_POINT('Ctrl Pts',(20.7789278232766,10.0286114002692,40.3328269804548));
#50631=CARTESIAN_POINT('Ctrl Pts',(20.8526866048507,10.0328402531467,40.3042948974237));
#50632=CARTESIAN_POINT('Ctrl Pts',(20.9265779471188,10.0370767061995,40.2757115359869));
#50633=CARTESIAN_POINT('Ctrl Pts',(20.9989454848812,10.0413131592523,40.2434416145585));
#50634=CARTESIAN_POINT('Ctrl Pts',(21.069410534283,10.0455496123051,40.2076886748437));
#50635=CARTESIAN_POINT('Ctrl Pts',(21.1334542758511,10.0494000077391,40.1751938131949));
#50636=CARTESIAN_POINT('Ctrl Pts',(21.1959265551441,10.0532504031732,40.1398225255816));
#50637=CARTESIAN_POINT('Ctrl Pts',(21.2565643282684,10.0571007986073,40.1017583594988));
#50638=CARTESIAN_POINT('Ctrl Pts',(21.3233006418414,10.0613384409847,40.0598659549346));
#50639=CARTESIAN_POINT('Ctrl Pts',(21.3880649679024,10.0655760833622,40.0145538970917));
#50640=CARTESIAN_POINT('Ctrl Pts',(21.4504855966769,10.0698137257397,39.9660337549821));
#50641=CARTESIAN_POINT('Ctrl Pts',(21.5128164621377,10.0740452742212,39.917583386741));
#50642=CARTESIAN_POINT('Ctrl Pts',(21.5728099564192,10.0782768227026,39.8659343812352));
#50643=CARTESIAN_POINT('Ctrl Pts',(21.6301219948177,10.0825083711841,39.8113423745445));
#50644=CARTESIAN_POINT('Ctrl Pts',(21.6873678362291,10.0867350321102,39.7568134231291));
#50645=CARTESIAN_POINT('Ctrl Pts',(21.7419380388731,10.0909616930363,39.6993485473729));
#50646=CARTESIAN_POINT('Ctrl Pts',(21.7935215673784,10.0951883539624,39.6392435896402));
#50647=CARTESIAN_POINT('Ctrl Pts',(21.845072534753,10.0994123468884,39.5791765720298));
#50648=CARTESIAN_POINT('Ctrl Pts',(21.8936402655684,10.1036363398144,39.5164731350639));
#50649=CARTESIAN_POINT('Ctrl Pts',(21.9389514467888,10.1078603327404,39.4514650302156));
#50650=CARTESIAN_POINT('Ctrl Pts',(21.9842481342043,10.1120829745269,39.3864777196782));
#50651=CARTESIAN_POINT('Ctrl Pts',(22.0262900727396,10.1163056163134,39.3191875894887));
#50652=CARTESIAN_POINT('Ctrl Pts',(22.0648459462335,10.1205282580998,39.2499572423455));
#50653=CARTESIAN_POINT('Ctrl Pts',(22.1034014911669,10.1247508639023,39.1807274851607));
#50654=CARTESIAN_POINT('Ctrl Pts',(22.1384708032911,10.1289734697048,39.1095579541354));
#50655=CARTESIAN_POINT('Ctrl Pts',(22.1698681425892,10.1331960755073,39.0368365303919));
#50656=CARTESIAN_POINT('Ctrl Pts',(22.2012967025113,10.1374228801492,38.9640427945263));
#50657=CARTESIAN_POINT('Ctrl Pts',(22.2290458098626,10.1416496847912,38.889694514852));
#50658=CARTESIAN_POINT('Ctrl Pts',(22.2529778550209,10.1458764894332,38.8141997099449));
#50659=CARTESIAN_POINT('Ctrl Pts',(22.2769214972289,10.1501053423107,38.7386683215783));
#50660=CARTESIAN_POINT('Ctrl Pts',(22.2970442733188,10.1543341951881,38.6619897551865));
#50661=CARTESIAN_POINT('Ctrl Pts',(22.3132591591634,10.1585630480656,38.5845848774434));
#50662=CARTESIAN_POINT('Ctrl Pts',(22.3295031867111,10.1627995011183,38.5070408861726));
#50663=CARTESIAN_POINT('Ctrl Pts',(22.3418252176368,10.1670359541711,38.4287684395224));
#50664=CARTESIAN_POINT('Ctrl Pts',(22.3501898654027,10.1712724072239,38.3501959980866));
#50665=CARTESIAN_POINT('Ctrl Pts',(22.3577922632494,10.175122802658,38.2787836713156));
#50666=CARTESIAN_POINT('Ctrl Pts',(22.3621263178339,10.1789731980922,38.2071238524588));
#50667=CARTESIAN_POINT('Ctrl Pts',(22.3632028170632,10.1828235935264,38.1355371119357));
#50668=CARTESIAN_POINT('Ctrl Pts',(22.3643875833634,10.1870612359039,38.0567506572731));
#50669=CARTESIAN_POINT('Ctrl Pts',(22.3616302904976,10.1912988782814,37.9777570002356));
#50670=CARTESIAN_POINT('Ctrl Pts',(22.3549060820149,10.1955365206589,37.8989831206356));
#50671=CARTESIAN_POINT('Ctrl Pts',(22.3481915432079,10.1997680691403,37.8203225209658));
#50672=CARTESIAN_POINT('Ctrl Pts',(22.3375214570927,10.2039996176218,37.7418815343062));
#50673=CARTESIAN_POINT('Ctrl Pts',(22.3229229709614,10.2082311661032,37.6640879539632));
#50674=CARTESIAN_POINT('Ctrl Pts',(22.3083413464846,10.2124578270293,37.5863842273538));
#50675=CARTESIAN_POINT('Ctrl Pts',(22.2898404249894,10.2166844879554,37.509326879449));
#50676=CARTESIAN_POINT('Ctrl Pts',(22.2674990714423,10.2209111488815,37.4333378652509));
#50677=CARTESIAN_POINT('Ctrl Pts',(22.2451718204538,10.2251351418075,37.3573968176866));
#50678=CARTESIAN_POINT('Ctrl Pts',(22.2190090810641,10.2293591347336,37.2825232138497));
#50679=CARTESIAN_POINT('Ctrl Pts',(22.189140374835,10.2335831276596,37.2091269113014));
#50680=CARTESIAN_POINT('Ctrl Pts',(22.1592812227863,10.237805769446,37.1357540862185));
#50681=CARTESIAN_POINT('Ctrl Pts',(22.1257186345117,10.2420284112325,37.0638580579205));
#50682=CARTESIAN_POINT('Ctrl Pts',(22.0886308720566,10.246251053019,36.9938302475696));
#50683=CARTESIAN_POINT('Ctrl Pts',(22.0515434256514,10.2504736588214,36.9238030339729));
#50684=CARTESIAN_POINT('Ctrl Pts',(22.0109310854571,10.2546962646239,36.8556444202606));
#50685=CARTESIAN_POINT('Ctrl Pts',(21.9670181274846,10.2589188704264,36.7897213551894));
#50686=CARTESIAN_POINT('Ctrl Pts',(21.9230615037117,10.2631456750684,36.7237327380911));
#50687=CARTESIAN_POINT('Ctrl Pts',(21.8757979667557,10.2673724797104,36.6599845010665));
#50688=CARTESIAN_POINT('Ctrl Pts',(21.8254948843686,10.2715992843524,36.5988141793755));
#50689=CARTESIAN_POINT('Ctrl Pts',(21.7751674259893,10.2758281372298,36.5376142156185));
#50690=CARTESIAN_POINT('Ctrl Pts',(21.7217978039609,10.2800569901073,36.4789950028464));
#50691=CARTESIAN_POINT('Ctrl Pts',(21.6656916993704,10.2842858429847,36.4232586354633));
#50692=CARTESIAN_POINT('Ctrl Pts',(21.609484759815,10.2885222960375,36.367422097614));
#50693=CARTESIAN_POINT('Ctrl Pts',(21.5505318605398,10.2927587490903,36.314479071465));
#50694=CARTESIAN_POINT('Ctrl Pts',(21.4891731611,10.296995202143,36.2646924679609));
#50695=CARTESIAN_POINT('Ctrl Pts',(21.4334059300638,10.3008455975772,36.2194427960241));
#50696=CARTESIAN_POINT('Ctrl Pts',(21.3756520105745,10.3046959930113,36.1768001125802));
#50697=CARTESIAN_POINT('Ctrl Pts',(21.3161861910076,10.3085463884455,36.1369298658731));
#50698=CARTESIAN_POINT('Ctrl Pts',(21.2507396982202,10.312784030823,36.0930497372118));
#50699=CARTESIAN_POINT('Ctrl Pts',(21.1829735872081,10.3170216732005,36.0523636865999));
#50700=CARTESIAN_POINT('Ctrl Pts',(21.1132325072472,10.3212593155779,36.0151249855907));
#50701=CARTESIAN_POINT('Ctrl Pts',(21.0435917176962,10.3254908640594,35.977939835295));
#50702=CARTESIAN_POINT('Ctrl Pts',(20.9719820094379,10.3297224125409,35.9441924085928));
#50703=CARTESIAN_POINT('Ctrl Pts',(20.8987770216472,10.3339539610223,35.9140927955975));
#50704=CARTESIAN_POINT('Ctrl Pts',(20.825656587639,10.3381806219484,35.8840279484863));
#50705=CARTESIAN_POINT('Ctrl Pts',(20.7509449671529,10.3424072828745,35.8576027195065));
#50706=CARTESIAN_POINT('Ctrl Pts',(20.6750390535672,10.3466339438006,35.8349806364936));
#50707=CARTESIAN_POINT('Ctrl Pts',(20.5991810541596,10.3508579367267,35.8123728332445));
#50708=CARTESIAN_POINT('Ctrl Pts',(20.5221307060824,10.3550819296527,35.7935635444467));
#50709=CARTESIAN_POINT('Ctrl Pts',(20.4443023287473,10.3593059225787,35.7786672186932));
#50710=CARTESIAN_POINT('Ctrl Pts',(20.3664988465768,10.3635285643652,35.763775657866));
#50711=CARTESIAN_POINT('Ctrl Pts',(20.2879182894395,10.3677512061516,35.7527946626141));
#50712=CARTESIAN_POINT('Ctrl Pts',(20.2089860422268,10.3719738479381,35.7457877591317));
#50713=CARTESIAN_POINT('Ctrl Pts',(20.1300544676489,10.3761964537406,35.7387809153597));
#50714=CARTESIAN_POINT('Ctrl Pts',(20.0507716760174,10.380419059543,35.735748136048));
#50715=CARTESIAN_POINT('Ctrl Pts',(19.9715675701519,10.3846416653455,35.7367010265663));
#50716=CARTESIAN_POINT('Ctrl Pts',(19.892284705969,10.3888684699875,35.7376548646119));
#50717=CARTESIAN_POINT('Ctrl Pts',(19.8130811536719,10.3930952746295,35.7426022834191));
#50718=CARTESIAN_POINT('Ctrl Pts',(19.734385598417,10.3973220792715,35.7515027292816));
#50719=CARTESIAN_POINT('Ctrl Pts',(19.655651908675,10.4015509321489,35.7604074881442));
#50720=CARTESIAN_POINT('Ctrl Pts',(19.5774271695223,10.4057797850264,35.7732690139461));
#50721=CARTESIAN_POINT('Ctrl Pts',(19.5001311912394,10.4100086379038,35.7899953214488));
#50722=CARTESIAN_POINT('Ctrl Pts',(19.422696295145,10.4142450909566,35.8067516897916));
#50723=CARTESIAN_POINT('Ctrl Pts',(19.3461939487898,10.4184815440094,35.8273865959679));
#50724=CARTESIAN_POINT('Ctrl Pts',(19.2710298605755,10.4227179970622,35.8517578029208));
#50725=CARTESIAN_POINT('Ctrl Pts',(19.2027152921228,10.4265683924963,35.8739081213137));
#50726=CARTESIAN_POINT('Ctrl Pts',(19.1355062167052,10.4304187879304,35.8991440847221));
#50727=CARTESIAN_POINT('Ctrl Pts',(19.0696910005683,10.4342691833645,35.9273252414417));
#50728=CARTESIAN_POINT('Ctrl Pts',(18.9972565314969,10.438506825742,35.9583406698581));
#50729=CARTESIAN_POINT('Ctrl Pts',(18.9262388203568,10.4427444681195,35.9930406009896));
#50730=CARTESIAN_POINT('Ctrl Pts',(18.8570379332917,10.446982110497,36.031273784435));
#50731=CARTESIAN_POINT('Ctrl Pts',(18.7879365598179,10.4512136589785,36.0694519870622));
#50732=CARTESIAN_POINT('Ctrl Pts',(18.7206472288333,10.4554452074599,36.1111531268728));
#50733=CARTESIAN_POINT('Ctrl Pts',(18.655549563203,10.4596767559414,36.1561781295869));
#50734=CARTESIAN_POINT('Ctrl Pts',(18.5905270871742,10.4639034168675,36.2011511271795));
#50735=CARTESIAN_POINT('Ctrl Pts',(18.5276916294922,10.4681300777936,36.2494400930017));
#50736=CARTESIAN_POINT('Ctrl Pts',(18.4673964115256,10.4723567387197,36.3008011000739));
#50737=CARTESIAN_POINT('Ctrl Pts',(18.4071392537795,10.4765807316457,36.352129686478));
#50738=CARTESIAN_POINT('Ctrl Pts',(18.3494195089428,10.4808047245717,36.4065261619143));
#50739=CARTESIAN_POINT('Ctrl Pts',(18.2945587130075,10.4850287174977,36.4637052656928));
#50740=CARTESIAN_POINT('Ctrl Pts',(18.2397154655372,10.4892513592842,36.5208660794433));
#50741=CARTESIAN_POINT('Ctrl Pts',(18.1877296752638,10.4934740010706,36.5808074159847));
#50742=CARTESIAN_POINT('Ctrl Pts',(18.1388861843631,10.4976966428571,36.6432070132838));
#50743=CARTESIAN_POINT('Ctrl Pts',(18.0900431096907,10.5019192486596,36.7056060788339));
#50744=CARTESIAN_POINT('Ctrl Pts',(18.0443425689648,10.5061418544621,36.7704629934736));
#50745=CARTESIAN_POINT('Ctrl Pts',(18.0020283089336,10.5103644602645,36.8374234428768));
#50746=CARTESIAN_POINT('Ctrl Pts',(17.9596719728017,10.5145912649065,36.9044504758526));
#50747=CARTESIAN_POINT('Ctrl Pts',(17.9207088944077,10.5188180695485,36.9735848245615));
#50748=CARTESIAN_POINT('Ctrl Pts',(17.885338403124,10.5230448741905,37.044444804097));
#50749=CARTESIAN_POINT('Ctrl Pts',(17.84995077192,10.5272737270679,37.1153391211369));
#50750=CARTESIAN_POINT('Ctrl Pts',(17.8181593841433,10.5315025799454,37.1879603048555));
#50751=CARTESIAN_POINT('Ctrl Pts',(17.7901155940106,10.5357314328228,37.2619061191818));
#50752=CARTESIAN_POINT('Ctrl Pts',(17.7620214030416,10.5399678858756,37.3359848303409));
#50753=CARTESIAN_POINT('Ctrl Pts',(17.7376884117068,10.5442043389284,37.4113924816997));
#50754=CARTESIAN_POINT('Ctrl Pts',(17.7172181434474,10.5484407919811,37.4877113129461));
#50755=CARTESIAN_POINT('Ctrl Pts',(17.6986132807333,10.5522911874153,37.5570753955191));
#50756=CARTESIAN_POINT('Ctrl Pts',(17.6831986247484,10.5561415828494,37.6271917420335));
#50757=CARTESIAN_POINT('Ctrl Pts',(17.6710133231036,10.5599919782835,37.6977419985394));
#50758=CARTESIAN_POINT('Ctrl Pts',(17.6502336907217,10.5665580694628,37.8180515680009));
#50759=CARTESIAN_POINT('Ctrl Pts',(17.6387726117503,10.573124160642,37.9400146317809));
#50760=CARTESIAN_POINT('Ctrl Pts',(17.6368279557372,10.5796902518213,38.0624722753877));
#50761=CARTESIAN_POINT('Ctrl Pts',(17.6366396038906,10.5803262179714,38.0743330482635));
#50762=CARTESIAN_POINT('Ctrl Pts',(17.6365404955559,10.5809621841216,38.0861984337401));
#50763=CARTESIAN_POINT('Ctrl Pts',(17.6365307901734,10.5815981502717,38.0980673588938));
#50764=CARTESIAN_POINT('',(17.6365300074329,11.3753481502331,38.0998125575523));
#50765=CARTESIAN_POINT('Ctrl Pts',(17.6365307901728,10.5815981503084,38.0980673595779));
#50766=CARTESIAN_POINT('Ctrl Pts',(17.6364645857,10.585936342929,38.1790302905545));
#50767=CARTESIAN_POINT('Ctrl Pts',(17.640563531315,10.5902745355496,38.2601393309714));
#50768=CARTESIAN_POINT('Ctrl Pts',(17.6488415013264,10.5946127281702,38.3409235459956));
#50769=CARTESIAN_POINT('Ctrl Pts',(17.656787108768,10.5987767412702,38.4184642545474));
#50770=CARTESIAN_POINT('Ctrl Pts',(17.6685825490526,10.6029407543702,38.4957051822));
#50771=CARTESIAN_POINT('Ctrl Pts',(17.6841870367672,10.6071047674702,38.5722295630548));
#50772=CARTESIAN_POINT('Ctrl Pts',(17.6997824680218,10.6112663638797,38.6487095310455));
#50773=CARTESIAN_POINT('Ctrl Pts',(17.7191824658297,10.6154279602891,38.7244733038589));
#50774=CARTESIAN_POINT('Ctrl Pts',(17.7422947371148,10.6195895566986,38.7991118557431));
#50775=CARTESIAN_POINT('Ctrl Pts',(17.7654012946875,10.6237501242968,38.873731955818));
#50776=CARTESIAN_POINT('Ctrl Pts',(17.7922181608439,10.627910691895,38.9472269249856));
#50777=CARTESIAN_POINT('Ctrl Pts',(17.822602968645,10.6320712594932,39.0192021588021));
#50778=CARTESIAN_POINT('Ctrl Pts',(17.8529903875591,10.636232184629,39.0911835777974));
#50779=CARTESIAN_POINT('Ctrl Pts',(17.8869461655744,10.6403931097648,39.1616445575498));
#50780=CARTESIAN_POINT('Ctrl Pts',(17.9242801823507,10.6445540349007,39.230211342855));
#50781=CARTESIAN_POINT('Ctrl Pts',(17.9616524192876,10.6487192197235,39.2988483224164));
#50782=CARTESIAN_POINT('Ctrl Pts',(18.0024095615276,10.6528844045463,39.3655868139426));
#50783=CARTESIAN_POINT('Ctrl Pts',(18.0463164606769,10.6570495893692,39.4300793469105));
#50784=CARTESIAN_POINT('Ctrl Pts',(18.0902500971362,10.6612173106007,39.4946111529058));
#50785=CARTESIAN_POINT('Ctrl Pts',(18.1373370118005,10.6653850318321,39.5568938960868));
#50786=CARTESIAN_POINT('Ctrl Pts',(18.1873014405384,10.6695527530636,39.6166127961434));
#50787=CARTESIAN_POINT('Ctrl Pts',(18.2373451387713,10.6737270864623,39.6764264413451));
#50788=CARTESIAN_POINT('Ctrl Pts',(18.2902751262759,10.677901419861,39.7336677789488));
#50789=CARTESIAN_POINT('Ctrl Pts',(18.3457791175477,10.6820757532597,39.7880591556456));
#50790=CARTESIAN_POINT('Ctrl Pts',(18.3619078509177,10.6832887599073,39.8038645777831));
#50791=CARTESIAN_POINT('Ctrl Pts',(18.3782537283861,10.684501766555,39.8194296123154));
#50792=CARTESIAN_POINT('Ctrl Pts',(18.3948086017898,10.6857147732027,39.8347481131311));
#50793=CARTESIAN_POINT('Ctrl Pts',(18.4526431018926,10.6899524155802,39.8882633418736));
#50794=CARTESIAN_POINT('Ctrl Pts',(18.5132652934297,10.6941900579577,39.9389836574223));
#50795=CARTESIAN_POINT('Ctrl Pts',(18.5763740608301,10.6984277003352,39.9866053180839));
#50796=CARTESIAN_POINT('Ctrl Pts',(18.6393920753463,10.7026592488166,40.0341584969287));
#50797=CARTESIAN_POINT('Ctrl Pts',(18.7048891934309,10.7068907972981,40.0786215900338));
#50798=CARTESIAN_POINT('Ctrl Pts',(18.7725289528581,10.7111223457796,40.1197290088842));
#50799=CARTESIAN_POINT('Ctrl Pts',(18.8400905864953,10.7153490067057,40.1607889475307));
#50800=CARTESIAN_POINT('Ctrl Pts',(18.9097895448374,10.7195756676318,40.1985006720779));
#50801=CARTESIAN_POINT('Ctrl Pts',(18.9812591597996,10.7238023285579,40.2326409780851));
#50802=CARTESIAN_POINT('Ctrl Pts',(19.0526836609138,10.7280263214839,40.2667597336673));
#50803=CARTESIAN_POINT('Ctrl Pts',(19.1258761782657,10.7322503144099,40.2973113438965));
#50804=CARTESIAN_POINT('Ctrl Pts',(19.2004452042721,10.7364743073359,40.3241183802866));
#50805=CARTESIAN_POINT('Ctrl Pts',(19.274990377691,10.7406969491224,40.3509168418405));
#50806=CARTESIAN_POINT('Ctrl Pts',(19.3509107445848,10.7449195909088,40.3739729496525));
#50807=CARTESIAN_POINT('Ctrl Pts',(19.4277959548363,10.7491422326953,40.3931578601567));
#50808=CARTESIAN_POINT('Ctrl Pts',(19.5046805098969,10.7533648384978,40.4123426071733));
#50809=CARTESIAN_POINT('Ctrl Pts',(19.5825294367942,10.7575874443003,40.42765611037));
#50810=CARTESIAN_POINT('Ctrl Pts',(19.6609198558077,10.7618100501027,40.4390201146451));
#50811=CARTESIAN_POINT('Ctrl Pts',(19.7393882240316,10.7660368547447,40.4503954189639));
#50812=CARTESIAN_POINT('Ctrl Pts',(19.8183986949142,10.7702636593867,40.4578133122121));
#50813=CARTESIAN_POINT('Ctrl Pts',(19.8975214880639,10.7744904640287,40.4612472542052));
#50814=CARTESIAN_POINT('Ctrl Pts',(19.9766826227329,10.7787193169061,40.4646828602263));
#50815=CARTESIAN_POINT('Ctrl Pts',(20.0559557187369,10.7829481697836,40.4641306723745));
#50816=CARTESIAN_POINT('Ctrl Pts',(20.1349117722814,10.7871770226611,40.459616336314));
#50817=CARTESIAN_POINT('Ctrl Pts',(20.2140097271565,10.7914134757138,40.4550938870023));
#50818=CARTESIAN_POINT('Ctrl Pts',(20.2927890338919,10.7956499287666,40.4465951117349));
#50819=CARTESIAN_POINT('Ctrl Pts',(20.3708268121079,10.7998863818194,40.4341974887147));
#50820=CARTESIAN_POINT('Ctrl Pts',(20.4417531982116,10.8037367772535,40.4229296307976));
#50821=CARTESIAN_POINT('Ctrl Pts',(20.5120669072558,10.8075871726876,40.408441843249));
#50822=CARTESIAN_POINT('Ctrl Pts',(20.5814612535748,10.8114375681218,40.3908280711331));
#50823=CARTESIAN_POINT('Ctrl Pts',(20.6578348177323,10.8156752104993,40.3714428239752));
#50824=CARTESIAN_POINT('Ctrl Pts',(20.733381259297,10.8199128528767,40.3481977022715));
#50825=CARTESIAN_POINT('Ctrl Pts',(20.8076818713031,10.8241504952542,40.3211799647188));
#50826=CARTESIAN_POINT('Ctrl Pts',(20.8818756361132,10.8283820437357,40.294201079733));
#50827=CARTESIAN_POINT('Ctrl Pts',(20.9548266923092,10.8326135922171,40.2634605116557));
#50828=CARTESIAN_POINT('Ctrl Pts',(21.0261290979499,10.8368451406986,40.2290959384773));
#50829=CARTESIAN_POINT('Ctrl Pts',(21.0973491473432,10.8410718016247,40.1947710573298));
#50830=CARTESIAN_POINT('Ctrl Pts',(21.1669239102289,10.8452984625508,40.1568306918639));
#50831=CARTESIAN_POINT('Ctrl Pts',(21.2344665571698,10.8495251234769,40.1154609299437));
#50832=CARTESIAN_POINT('Ctrl Pts',(21.3019665690871,10.8537491164029,40.0741172819064));
#50833=CARTESIAN_POINT('Ctrl Pts',(21.3674366124437,10.8579731093289,40.0293487783934));
#50834=CARTESIAN_POINT('Ctrl Pts',(21.4305147367452,10.8621971022549,39.9813872617977));
#50835=CARTESIAN_POINT('Ctrl Pts',(21.4935726840838,10.8664197440414,39.9334410867765));
#50836=CARTESIAN_POINT('Ctrl Pts',(21.5542398588359,10.8706423858279,39.8823042104119));
#50837=CARTESIAN_POINT('Ctrl Pts',(21.6121848101614,10.8748650276143,39.8282507279862));
#50838=CARTESIAN_POINT('Ctrl Pts',(21.6701292676988,10.8790876334168,39.7741977061867));
#50839=CARTESIAN_POINT('Ctrl Pts',(21.7253512061264,10.8833102392193,39.7172284485515));
#50840=CARTESIAN_POINT('Ctrl Pts',(21.7775547913187,10.8875328450218,39.6576550981395));
#50841=CARTESIAN_POINT('Ctrl Pts',(21.8298102862763,10.8917596496637,39.5980225096765));
#50842=CARTESIAN_POINT('Ctrl Pts',(21.8790411230933,10.8959864543057,39.5357810094083));
#50843=CARTESIAN_POINT('Ctrl Pts',(21.9249910933316,10.9002132589477,39.4712766794101));
#50844=CARTESIAN_POINT('Ctrl Pts',(21.9709633301203,10.9044421118252,39.4067410917438));
#50845=CARTESIAN_POINT('Ctrl Pts',(22.0136512804146,10.9086709647026,39.3399408854482));
#50846=CARTESIAN_POINT('Ctrl Pts',(22.0528429355228,10.9128998175801,39.2712498977478));
#50847=CARTESIAN_POINT('Ctrl Pts',(22.0921050266236,10.9171362706328,39.2024354572896));
#50848=CARTESIAN_POINT('Ctrl Pts',(22.1278580552572,10.9213727236856,39.1317238649282));
#50849=CARTESIAN_POINT('Ctrl Pts',(22.1599368265607,10.9256091767384,39.0595120354465));
#50850=CARTESIAN_POINT('Ctrl Pts',(22.1890923377918,10.9294595721726,38.993880693599));
#50851=CARTESIAN_POINT('Ctrl Pts',(22.2152132525274,10.9333099676067,38.9270105845734));
#50852=CARTESIAN_POINT('Ctrl Pts',(22.2382114383322,10.9371603630409,38.8592101146711));
#50853=CARTESIAN_POINT('Ctrl Pts',(22.2635226273876,10.9413980054184,38.7845907283287));
#50854=CARTESIAN_POINT('Ctrl Pts',(22.2851456605777,10.9456356477959,38.7085641214613));
#50855=CARTESIAN_POINT('Ctrl Pts',(22.3029258193166,10.9498732901734,38.6315290317802));
#50856=CARTESIAN_POINT('Ctrl Pts',(22.3206804094894,10.9541048386548,38.5546047215811));
#50857=CARTESIAN_POINT('Ctrl Pts',(22.3346029951879,10.9583363871363,38.4766752615975));
#50858=CARTESIAN_POINT('Ctrl Pts',(22.3445881013937,10.9625679356177,38.3981561263885));
#50859=CARTESIAN_POINT('Ctrl Pts',(22.3545616745261,10.9667945965438,38.319727682949));
#50860=CARTESIAN_POINT('Ctrl Pts',(22.360606747145,10.9710212574699,38.2407113804582));
#50861=CARTESIAN_POINT('Ctrl Pts',(22.3626688573211,10.975247918396,38.1615330118293));
#50862=CARTESIAN_POINT('Ctrl Pts',(22.3647296658291,10.9794719113221,38.0824046230541));
#50863=CARTESIAN_POINT('Ctrl Pts',(22.3628124900714,10.9836959042481,38.0031148385859));
#50864=CARTESIAN_POINT('Ctrl Pts',(22.3569147926027,10.9879198971741,37.9240934870149));
#50865=CARTESIAN_POINT('Ctrl Pts',(22.3510189816458,10.9921425389605,37.8450974122081));
#50866=CARTESIAN_POINT('Ctrl Pts',(22.3411452122845,10.996365180747,37.766370066925));
#50867=CARTESIAN_POINT('Ctrl Pts',(22.3273429936983,11.0005878225335,37.6883386943332));
#50868=CARTESIAN_POINT('Ctrl Pts',(22.3135408927301,11.004810428336,37.6103079866992));
#50869=CARTESIAN_POINT('Ctrl Pts',(22.2958104921561,11.0090330341384,37.5329737013224));
#50870=CARTESIAN_POINT('Ctrl Pts',(22.2742526056455,11.0132556399409,37.4567539144196));
#50871=CARTESIAN_POINT('Ctrl Pts',(22.2526732825838,11.0174824445829,37.3804583367218));
#50872=CARTESIAN_POINT('Ctrl Pts',(22.2272589990749,11.0217092492249,37.3052799233104));
#50873=CARTESIAN_POINT('Ctrl Pts',(22.1981606087981,11.0259360538669,37.23162198391));
#50874=CARTESIAN_POINT('Ctrl Pts',(22.1690481179513,11.0301649067443,37.1579283511628));
#50875=CARTESIAN_POINT('Ctrl Pts',(22.1362481581054,11.0343937596218,37.0857570875216));
#50876=CARTESIAN_POINT('Ctrl Pts',(22.0999589253276,11.0386226124992,37.0154895330901));
#50877=CARTESIAN_POINT('Ctrl Pts',(22.063604472846,11.042859065552,36.945095692465));
#50878=CARTESIAN_POINT('Ctrl Pts',(22.0237484537432,11.0470955186048,36.8766128034194));
#50879=CARTESIAN_POINT('Ctrl Pts',(21.9806339055323,11.0513319716575,36.8103954973885));
#50880=CARTESIAN_POINT('Ctrl Pts',(21.9414482807872,11.0551823670917,36.7502124127122));
#50881=CARTESIAN_POINT('Ctrl Pts',(21.8995716557137,11.0590327625258,36.6919006476892));
#50882=CARTESIAN_POINT('Ctrl Pts',(21.8552147687459,11.0628831579599,36.6357020102701));
#50883=CARTESIAN_POINT('Ctrl Pts',(21.8063967636439,11.0671208003374,36.5738512908939));
#50884=CARTESIAN_POINT('Ctrl Pts',(21.754390692574,11.0713584427149,36.5143284458008));
#50885=CARTESIAN_POINT('Ctrl Pts',(21.6994468248549,11.0755960850924,36.4574803105014));
#50886=CARTESIAN_POINT('Ctrl Pts',(21.6445819685736,11.0798276335739,36.4007139250514));
#50887=CARTESIAN_POINT('Ctrl Pts',(21.5867880285279,11.0840591820553,36.3466149452102));
#50888=CARTESIAN_POINT('Ctrl Pts',(21.5263561190588,11.0882907305368,36.2954980081164));
#50889=CARTESIAN_POINT('Ctrl Pts',(21.465994010114,11.0925173914629,36.2444401124967));
#50890=CARTESIAN_POINT('Ctrl Pts',(21.4030003428528,11.096744052389,36.196357716058));
#50891=CARTESIAN_POINT('Ctrl Pts',(21.3377026555861,11.1009707133151,36.151528279359));
#50892=CARTESIAN_POINT('Ctrl Pts',(21.2724461862546,11.1051947062411,36.1067271403975));
#50893=CARTESIAN_POINT('Ctrl Pts',(21.204888969131,11.1094186991671,36.0651751500913));
#50894=CARTESIAN_POINT('Ctrl Pts',(21.1353901922661,11.1136426920931,36.0271084079948));
#50895=CARTESIAN_POINT('Ctrl Pts',(21.065913646155,11.1178653338796,35.9890538424057));
#50896=CARTESIAN_POINT('Ctrl Pts',(20.994497184432,11.122087975666,35.9544825362157));
#50897=CARTESIAN_POINT('Ctrl Pts',(20.921526157148,11.1263106174525,35.9235855214155));
#50898=CARTESIAN_POINT('Ctrl Pts',(20.8485557516991,11.130533223255,35.8926887699096));
#50899=CARTESIAN_POINT('Ctrl Pts',(20.7740312392585,11.1347558290575,35.8654664289973));
#50900=CARTESIAN_POINT('Ctrl Pts',(20.6983582068759,11.13897843486,35.8420615030987));
#50901=CARTESIAN_POINT('Ctrl Pts',(20.6226099273753,11.1432052395019,35.8186333040053));
#50902=CARTESIAN_POINT('Ctrl Pts',(20.5457112955545,11.1474320441439,35.7990302411467));
#50903=CARTESIAN_POINT('Ctrl Pts',(20.4680827498871,11.1516588487859,35.7833453040735));
#50904=CARTESIAN_POINT('Ctrl Pts',(20.3904165867866,11.1558877016634,35.7676527663548));
#50905=CARTESIAN_POINT('Ctrl Pts',(20.3120202693913,11.1601165545408,35.7558822064558));
#50906=CARTESIAN_POINT('Ctrl Pts',(20.2333215767156,11.1643454074183,35.7480749410879));
#50907=CARTESIAN_POINT('Ctrl Pts',(20.1544814452432,11.1685818604711,35.7402536443531));
#50908=CARTESIAN_POINT('Ctrl Pts',(20.0753383219877,11.1728183135238,35.7364098972061));
#50909=CARTESIAN_POINT('Ctrl Pts',(19.9963219897195,11.1770547665766,35.7365328618446));
#50910=CARTESIAN_POINT('Ctrl Pts',(19.9245062228041,11.1809051620107,35.736644621016));
#50911=CARTESIAN_POINT('Ctrl Pts',(19.8527954382003,11.1847555574448,35.7400323989185));
#50912=CARTESIAN_POINT('Ctrl Pts',(19.781507193178,11.188605952879,35.7466510385693));
#50913=CARTESIAN_POINT('Ctrl Pts',(19.7030492546903,11.1928435952564,35.7539353365967));
#50914=CARTESIAN_POINT('Ctrl Pts',(19.6248087169068,11.1970812376339,35.765161144516));
#50915=CARTESIAN_POINT('Ctrl Pts',(19.547212759378,11.2013188800114,35.7803073143992));
#50916=CARTESIAN_POINT('Ctrl Pts',(19.4697283878813,11.2055504284929,35.7954317034957));
#50917=CARTESIAN_POINT('Ctrl Pts',(19.3928872121281,11.2097819769743,35.814465169672));
#50918=CARTESIAN_POINT('Ctrl Pts',(19.3171116348953,11.2140135254558,35.8373347747171));
#50919=CARTESIAN_POINT('Ctrl Pts',(19.2414235805467,11.2182401863819,35.8601779647368));
#50920=CARTESIAN_POINT('Ctrl Pts',(19.1667991253259,11.222466847308,35.8868483536596));
#50921=CARTESIAN_POINT('Ctrl Pts',(19.093649312643,11.2266935082341,35.9172222118531));
#50922=CARTESIAN_POINT('Ctrl Pts',(19.0205456744013,11.2309175011601,35.9475768971209));
#50923=CARTESIAN_POINT('Ctrl Pts',(18.9489152628844,11.2351414940861,35.9816302321969));
#50924=CARTESIAN_POINT('Ctrl Pts',(18.879151653174,11.2393654870121,36.0192094232438));
#50925=CARTESIAN_POINT('Ctrl Pts',(18.8094103589302,11.2435881287986,36.0567765937375));
#50926=CARTESIAN_POINT('Ctrl Pts',(18.7415350931024,11.247810770585,36.0978671584149));
#50927=CARTESIAN_POINT('Ctrl Pts',(18.6758958659601,11.2520334123715,36.1422618451084));
#50928=CARTESIAN_POINT('Ctrl Pts',(18.6102571981736,11.256256018174,36.186656153485));
#50929=CARTESIAN_POINT('Ctrl Pts',(18.5468549186846,11.2604786239765,36.2343542640857));
#50930=CARTESIAN_POINT('Ctrl Pts',(18.4860297647078,11.264701229779,36.2850937854674));
#50931=CARTESIAN_POINT('Ctrl Pts',(18.4251441279225,11.268928034421,36.3358837607904));
#50932=CARTESIAN_POINT('Ctrl Pts',(18.3668410963031,11.273154839063,36.3897208869518));
#50933=CARTESIAN_POINT('Ctrl Pts',(18.3114275353693,11.2773816437049,36.44630308926));
#50934=CARTESIAN_POINT('Ctrl Pts',(18.2559871219948,11.2816104965824,36.5029127103121));
#50935=CARTESIAN_POINT('Ctrl Pts',(18.2034392797682,11.2858393494599,36.5622697060143));
#50936=CARTESIAN_POINT('Ctrl Pts',(18.154051523256,11.2900682023373,36.6240377165705));
#50937=CARTESIAN_POINT('Ctrl Pts',(18.1045750061226,11.2943046553901,36.6859167377775));
#50938=CARTESIAN_POINT('Ctrl Pts',(18.0582701972243,11.2985411084429,36.7502150505365));
#50939=CARTESIAN_POINT('Ctrl Pts',(18.0153619511129,11.3027775614956,36.8165662246109));
#50940=CARTESIAN_POINT('Ctrl Pts',(17.9763638286608,11.3066279569298,36.876870978263));
#50941=CARTESIAN_POINT('Ctrl Pts',(17.9401709977417,11.3104783523639,36.9388709190513));
#50942=CARTESIAN_POINT('Ctrl Pts',(17.9069184353317,11.3143287477981,37.0022750779245));
#50943=CARTESIAN_POINT('Ctrl Pts',(17.8681932052737,11.3188128367884,37.076114218762));
#50944=CARTESIAN_POINT('Ctrl Pts',(17.8333244380349,11.3232969257787,37.1521088126688));
#50945=CARTESIAN_POINT('Ctrl Pts',(17.8025426710631,11.3277810147689,37.2298438482654));
#50946=CARTESIAN_POINT('Ctrl Pts',(17.7718532744003,11.3322516478492,37.3073456156009));
#50947=CARTESIAN_POINT('Ctrl Pts',(17.7452265869857,11.3367222809295,37.3865770613249));
#50948=CARTESIAN_POINT('Ctrl Pts',(17.7228462170966,11.3411929140099,37.4671010428919));
#50949=CARTESIAN_POINT('Ctrl Pts',(17.7005069260382,11.3456553413107,37.5474772239072));
#50950=CARTESIAN_POINT('Ctrl Pts',(17.6823985487696,11.3501177686115,37.6291408496797));
#50951=CARTESIAN_POINT('Ctrl Pts',(17.6686561326386,11.3545801959123,37.711636493712));
#50952=CARTESIAN_POINT('Ctrl Pts',(17.6549469886206,11.359031819117,37.7939324054432));
#50953=CARTESIAN_POINT('Ctrl Pts',(17.6455828135995,11.3634834423216,37.8770559423081));
#50954=CARTESIAN_POINT('Ctrl Pts',(17.6406481221886,11.3679350655263,37.9605397634879));
#50955=CARTESIAN_POINT('Ctrl Pts',(17.6379089501496,11.3704060937619,38.006880361034));
#50956=CARTESIAN_POINT('Ctrl Pts',(17.6365336937416,11.3728771219975,38.0533317298038));
#50957=CARTESIAN_POINT('Ctrl Pts',(17.6365300074329,11.3753481502331,38.0998125575523));
#50958=CARTESIAN_POINT('',(17.636530903764,12.1690981502314,38.10206689074));
#50959=CARTESIAN_POINT('Ctrl Pts',(17.6365300074328,11.3753481502717,38.0998125582779));
#50960=CARTESIAN_POINT('Ctrl Pts',(17.6365234494525,11.3797441513659,38.1825027382993));
#50961=CARTESIAN_POINT('Ctrl Pts',(17.6408608001244,11.3841401524601,38.2651212912942));
#50962=CARTESIAN_POINT('Ctrl Pts',(17.6494937094782,11.3885361535542,38.3472056211282));
#50963=CARTESIAN_POINT('Ctrl Pts',(17.6581476503877,11.3929428642178,38.4294899253955));
#50964=CARTESIAN_POINT('Ctrl Pts',(17.6711180189738,11.3973495748814,38.5112369962023));
#50965=CARTESIAN_POINT('Ctrl Pts',(17.688304818639,11.401756285545,38.5919916964463));
#50966=CARTESIAN_POINT('Ctrl Pts',(17.7055127065732,11.4061684032594,38.6728454830171));
#50967=CARTESIAN_POINT('Ctrl Pts',(17.7269472330067,11.4105805209739,38.7527040752355));
#50968=CARTESIAN_POINT('Ctrl Pts',(17.7524584399641,11.4149926386884,38.8311274696054));
#50969=CARTESIAN_POINT('Ctrl Pts',(17.7780370260216,11.4194164094979,38.9097579924635));
#50970=CARTESIAN_POINT('Ctrl Pts',(17.8077136725913,11.4238401803075,38.9869453542417));
#50971=CARTESIAN_POINT('Ctrl Pts',(17.8412898630427,11.428263951117,39.0622686659649));
#50972=CARTESIAN_POINT('Ctrl Pts',(17.8711122655108,11.4321931483171,39.1291708989829));
#50973=CARTESIAN_POINT('Ctrl Pts',(17.9040102459344,11.4361223455171,39.1946027443427));
#50974=CARTESIAN_POINT('Ctrl Pts',(17.9398154781111,11.4400515427171,39.2582876053336));
#50975=CARTESIAN_POINT('Ctrl Pts',(17.9784314501492,11.4442891850946,39.3269717797339));
#50976=CARTESIAN_POINT('Ctrl Pts',(18.0205584409762,11.4485268274721,39.3938516508459));
#50977=CARTESIAN_POINT('Ctrl Pts',(18.0660031052796,11.4527644698496,39.4585457121908));
#50978=CARTESIAN_POINT('Ctrl Pts',(18.1113824183724,11.456996018331,39.5231467409367));
#50979=CARTESIAN_POINT('Ctrl Pts',(18.1600696630579,11.4612275668125,39.585567821757));
#50980=CARTESIAN_POINT('Ctrl Pts',(18.2118261425487,11.465459115294,39.6454529098059));
#50981=CARTESIAN_POINT('Ctrl Pts',(18.2635228418764,11.4696857762201,39.7052688289244));
#50982=CARTESIAN_POINT('Ctrl Pts',(18.3182814261258,11.4739124371462,39.7625542233394));
#50983=CARTESIAN_POINT('Ctrl Pts',(18.3758214409796,11.4781390980723,39.816984114463));
#50984=CARTESIAN_POINT('Ctrl Pts',(18.4333251347829,11.4823630909983,39.8713796477432));
#50985=CARTESIAN_POINT('Ctrl Pts',(18.4936064346114,11.4865870839243,39.9229229341624));
#50986=CARTESIAN_POINT('Ctrl Pts',(18.5563471947755,11.4908110768503,39.9713249367407));
#50987=CARTESIAN_POINT('Ctrl Pts',(18.6190678858902,11.4950337186368,40.019711456845));
#50988=CARTESIAN_POINT('Ctrl Pts',(18.6842461041889,11.4992563604232,40.0649584023344));
#50989=CARTESIAN_POINT('Ctrl Pts',(18.7515308578564,11.5034790022097,40.1068171919772));
#50990=CARTESIAN_POINT('Ctrl Pts',(18.8188150381452,11.5077016080122,40.1486756249131));
#50991=CARTESIAN_POINT('Ctrl Pts',(18.8882053193212,11.5119242138147,40.1871457130015));
#50992=CARTESIAN_POINT('Ctrl Pts',(18.9593232566276,11.5161468196172,40.2220231753456));
#50993=CARTESIAN_POINT('Ctrl Pts',(19.0305119115947,11.5203736242591,40.2569353188495));
#50994=CARTESIAN_POINT('Ctrl Pts',(19.1034312324066,11.5246004289011,40.2882474938245));
#50995=CARTESIAN_POINT('Ctrl Pts',(19.1776803327944,11.5288272335431,40.3158025195913));
#50996=CARTESIAN_POINT('Ctrl Pts',(19.2519654129954,11.5330560864206,40.3433708980406));
#50997=CARTESIAN_POINT('Ctrl Pts',(19.3275811087614,11.537284939298,40.3671783593769));
#50998=CARTESIAN_POINT('Ctrl Pts',(19.4041112544086,11.5415137921755,40.387117627884));
#50999=CARTESIAN_POINT('Ctrl Pts',(19.4807789414983,11.5457502452283,40.407092731626));
#51000=CARTESIAN_POINT('Ctrl Pts',(19.5583639021829,11.549986698281,40.4231856563543));
#51001=CARTESIAN_POINT('Ctrl Pts',(19.6364398885131,11.5542231513338,40.4353403362756));
#51002=CARTESIAN_POINT('Ctrl Pts',(19.7074010009196,11.558073546768,40.446387389905));
#51003=CARTESIAN_POINT('Ctrl Pts',(19.7787673752423,11.5619239422021,40.4541818933362));
#51004=CARTESIAN_POINT('Ctrl Pts',(19.8502182944387,11.5657743376363,40.4587191188395));
#51005=CARTESIAN_POINT('Ctrl Pts',(19.9288552677771,11.5700119800138,40.4637126680471));
#51006=CARTESIAN_POINT('Ctrl Pts',(20.0078898418441,11.5742496223913,40.4647787910041));
#51007=CARTESIAN_POINT('Ctrl Pts',(20.0868967384967,11.5784872647688,40.461872011295));
#51008=CARTESIAN_POINT('Ctrl Pts',(20.1657900201316,11.5827188132502,40.4589694116492));
#51009=CARTESIAN_POINT('Ctrl Pts',(20.2446552388075,11.5869503617317,40.4521052722963));
#51010=CARTESIAN_POINT('Ctrl Pts',(20.3230637889011,11.5911819102132,40.4412860203745));
#51011=CARTESIAN_POINT('Ctrl Pts',(20.4013817749539,11.5954085711393,40.4304792649874));
#51012=CARTESIAN_POINT('Ctrl Pts',(20.4792436786066,11.5996352320654,40.4157265390742));
#51013=CARTESIAN_POINT('Ctrl Pts',(20.5562242246053,11.6038618929915,40.3970862092795));
#51014=CARTESIAN_POINT('Ctrl Pts',(20.6331561780845,11.6080858859175,40.3784576458419));
#51015=CARTESIAN_POINT('Ctrl Pts',(20.7092074237692,11.6123098788435,40.355946459429));
#51016=CARTESIAN_POINT('Ctrl Pts',(20.7839623199025,11.6165338717695,40.3296621990501));
#51017=CARTESIAN_POINT('Ctrl Pts',(20.8586933039937,11.620756513556,40.3033863462857));
#51018=CARTESIAN_POINT('Ctrl Pts',(20.9321283200646,11.6249791553424,40.2733399716059));
#51019=CARTESIAN_POINT('Ctrl Pts',(21.0038677840611,11.6292017971289,40.2396821990717));
#51020=CARTESIAN_POINT('Ctrl Pts',(21.0756066367174,11.6334244029314,40.206024713358));
#51021=CARTESIAN_POINT('Ctrl Pts',(21.1456495422488,11.6376470087339,40.1687560913823));
#51022=CARTESIAN_POINT('Ctrl Pts',(21.2136191351045,11.6418696145364,40.1280826008347));
#51023=CARTESIAN_POINT('Ctrl Pts',(21.2816563149963,11.6460964191784,40.0873686657211));
#51024=CARTESIAN_POINT('Ctrl Pts',(21.3476156608831,11.6503232238203,40.0432433403453));
#51025=CARTESIAN_POINT('Ctrl Pts',(21.4111471023474,11.6545500284623,39.9959573561757));
#51026=CARTESIAN_POINT('Ctrl Pts',(21.474709330035,11.6587788813398,39.9486484580467));
#51027=CARTESIAN_POINT('Ctrl Pts',(21.5358409475857,11.6630077342172,39.8981761488354));
#51028=CARTESIAN_POINT('Ctrl Pts',(21.5942254311096,11.6672365870947,39.8448311424615));
#51029=CARTESIAN_POINT('Ctrl Pts',(21.6527148443447,11.6714730401474,39.7913902634212));
#51030=CARTESIAN_POINT('Ctrl Pts',(21.708446928044,11.6757094932002,39.7350667053189));
#51031=CARTESIAN_POINT('Ctrl Pts',(21.7611426285269,11.679945946253,39.6761875151407));
#51032=CARTESIAN_POINT('Ctrl Pts',(21.8090362985402,11.6837963416871,39.6226738417441));
#51033=CARTESIAN_POINT('Ctrl Pts',(21.8544221080747,11.6876467371212,39.567049728623));
#51034=CARTESIAN_POINT('Ctrl Pts',(21.8971215135095,11.6914971325553,39.5095816414381));
#51035=CARTESIAN_POINT('Ctrl Pts',(21.944115338705,11.6957347749328,39.446333799554));
#51036=CARTESIAN_POINT('Ctrl Pts',(21.9880310015187,11.6999724173103,39.3806145856531));
#51037=CARTESIAN_POINT('Ctrl Pts',(22.0285988592561,11.7042100596878,39.3127559973569));
#51038=CARTESIAN_POINT('Ctrl Pts',(22.069108378822,11.7084416081693,39.2449949923734));
#51039=CARTESIAN_POINT('Ctrl Pts',(22.106279415464,11.7126731566507,39.1751011216777));
#51040=CARTESIAN_POINT('Ctrl Pts',(22.1398840554303,11.7169047051322,39.1034374271548));
#51041=CARTESIAN_POINT('Ctrl Pts',(22.1734498811094,11.7211313660583,39.0318565061783));
#51042=CARTESIAN_POINT('Ctrl Pts',(22.2034572981561,11.7253580269844,38.9585102459841));
#51043=CARTESIAN_POINT('Ctrl Pts',(22.2297237760258,11.7295846879105,38.883787167237));
#51044=CARTESIAN_POINT('Ctrl Pts',(22.255973673676,11.7338086808365,38.8091112560258));
#51045=CARTESIAN_POINT('Ctrl Pts',(22.2784871642117,11.7380326737625,38.7330606924001));
#51046=CARTESIAN_POINT('Ctrl Pts',(22.2971298961696,11.7422566666885,38.6560437761758));
#51047=CARTESIAN_POINT('Ctrl Pts',(22.3157666648286,11.746479308475,38.5790514955519));
#51048=CARTESIAN_POINT('Ctrl Pts',(22.3305350234233,11.7507019502615,38.5010939314472));
#51049=CARTESIAN_POINT('Ctrl Pts',(22.3413509481727,11.7549245920479,38.4225928988535));
#51050=CARTESIAN_POINT('Ctrl Pts',(22.3521667807523,11.7591471978504,38.34409253522));
#51051=CARTESIAN_POINT('Ctrl Pts',(22.3590301838881,11.7633698036529,38.2650491768866));
#51052=CARTESIAN_POINT('Ctrl Pts',(22.3619087753822,11.7675924094553,38.1858916624153));
#51053=CARTESIAN_POINT('Ctrl Pts',(22.3647902292661,11.7718192140973,38.1066554359555));
#51054=CARTESIAN_POINT('Ctrl Pts',(22.3636789395533,11.7760460187393,38.0273052961667));
#51055=CARTESIAN_POINT('Ctrl Pts',(22.3585946809799,11.7802728233813,37.9482713878224));
#51056=CARTESIAN_POINT('Ctrl Pts',(22.3535079586638,11.7845016762587,37.8691991810309));
#51057=CARTESIAN_POINT('Ctrl Pts',(22.3444444858648,11.7887305291362,37.7904439772517));
#51058=CARTESIAN_POINT('Ctrl Pts',(22.3314758378677,11.7929593820136,37.7124295440325));
#51059=CARTESIAN_POINT('Ctrl Pts',(22.3184838823684,11.7971958350664,37.6342749017808));
#51060=CARTESIAN_POINT('Ctrl Pts',(22.3015728284014,11.8014322881192,37.5568641492687));
#51061=CARTESIAN_POINT('Ctrl Pts',(22.2808651262499,11.805668741172,37.4806093988788));
#51062=CARTESIAN_POINT('Ctrl Pts',(22.2620444664143,11.8095191366061,37.4113035576305));
#51063=CARTESIAN_POINT('Ctrl Pts',(22.2400883095329,11.8133695320402,37.3429526919254));
#51064=CARTESIAN_POINT('Ctrl Pts',(22.2151229973752,11.8172199274744,37.2758516229467));
#51065=CARTESIAN_POINT('Ctrl Pts',(22.1876468415941,11.8214575698519,37.2020019785807));
#51066=CARTESIAN_POINT('Ctrl Pts',(22.1564219787768,11.8256952122293,37.1293892492687));
#51067=CARTESIAN_POINT('Ctrl Pts',(22.1215801348679,11.8299328546068,37.0584203476288));
#51068=CARTESIAN_POINT('Ctrl Pts',(22.0867883948979,11.8341644030883,36.9875535020545));
#51069=CARTESIAN_POINT('Ctrl Pts',(22.0483902081382,11.8383959515697,36.9183262070084));
#51070=CARTESIAN_POINT('Ctrl Pts',(22.0065660571066,11.8426275000512,36.8511272685467));
#51071=CARTESIAN_POINT('Ctrl Pts',(21.9647902141243,11.8468541609773,36.7840059467146));
#51072=CARTESIAN_POINT('Ctrl Pts',(21.9195965170393,11.8510808219034,36.7189087216886));
#51073=CARTESIAN_POINT('Ctrl Pts',(21.8712115253835,11.8553074828295,36.6562001980289));
#51074=CARTESIAN_POINT('Ctrl Pts',(21.8228570758423,11.8595314757555,36.5935312579434));
#51075=CARTESIAN_POINT('Ctrl Pts',(21.7713156157961,11.8637554686815,36.5332483965298));
#51076=CARTESIAN_POINT('Ctrl Pts',(21.7168565224518,11.8679794616076,36.475686568973));
#51077=CARTESIAN_POINT('Ctrl Pts',(21.6624148490787,11.872202103394,36.418143153867));
#51078=CARTESIAN_POINT('Ctrl Pts',(21.6050577176351,11.8764247451805,36.3633193844847));
#51079=CARTESIAN_POINT('Ctrl Pts',(21.5450932379161,11.8806473869669,36.3115153545401));
#51080=CARTESIAN_POINT('Ctrl Pts',(21.485129269195,11.8848699927694,36.2597117660526));
#51081=CARTESIAN_POINT('Ctrl Pts',(21.4225583520407,11.8890925985719,36.2109281712106));
#51082=CARTESIAN_POINT('Ctrl Pts',(21.3577225984424,11.8933152043744,36.1654251664568));
#51083=CARTESIAN_POINT('Ctrl Pts',(21.2928223740089,11.8975420090164,36.1198769148051));
#51084=CARTESIAN_POINT('Ctrl Pts',(21.2256531991711,11.9017688136584,36.0776160392707));
#51085=CARTESIAN_POINT('Ctrl Pts',(21.156586672529,11.9059956183003,36.0388600945524));
#51086=CARTESIAN_POINT('Ctrl Pts',(21.0874866774581,11.9102244711778,36.0000853693824));
#51087=CARTESIAN_POINT('Ctrl Pts',(21.0164879193549,11.9144533240553,35.9648191673006));
#51088=CARTESIAN_POINT('Ctrl Pts',(20.9439848440504,11.9186821769327,35.9332321178532));
#51089=CARTESIAN_POINT('Ctrl Pts',(20.8713514648315,11.9229186299855,35.901588299556));
#51090=CARTESIAN_POINT('Ctrl Pts',(20.7972088060598,11.9271550830383,35.8736370115531));
#51091=CARTESIAN_POINT('Ctrl Pts',(20.7219692294953,11.931391536091,35.8494998616836));
#51092=CARTESIAN_POINT('Ctrl Pts',(20.6535860517611,11.9352419315252,35.8275622713238));
#51093=CARTESIAN_POINT('Ctrl Pts',(20.5842972096088,11.9390923269593,35.8087747749266));
#51094=CARTESIAN_POINT('Ctrl Pts',(20.5144187912874,11.9429427223935,35.7931918701222));
#51095=CARTESIAN_POINT('Ctrl Pts',(20.437512470413,11.947180364771,35.7760417412865));
#51096=CARTESIAN_POINT('Ctrl Pts',(20.3596032030523,11.9514180071485,35.7627095780923));
#51097=CARTESIAN_POINT('Ctrl Pts',(20.2811040381236,11.955655649526,35.7533063769102));
#51098=CARTESIAN_POINT('Ctrl Pts',(20.2027177580751,11.9598871980074,35.7439166979004));
#51099=CARTESIAN_POINT('Ctrl Pts',(20.1237437266959,11.9641187464889,35.7384448158167));
#51100=CARTESIAN_POINT('Ctrl Pts',(20.0446063438319,11.9683502949703,35.7369509706758));
#51101=CARTESIAN_POINT('Ctrl Pts',(19.9655603668302,11.9725769558964,35.7354588509674));
#51102=CARTESIAN_POINT('Ctrl Pts',(19.886351879607,11.9768036168225,35.7379356460951));
#51103=CARTESIAN_POINT('Ctrl Pts',(19.8074100615131,11.9810302777486,35.7443897698274));
#51104=CARTESIAN_POINT('Ctrl Pts',(19.7285180739549,11.9852542706746,35.7508398195158));
#51105=CARTESIAN_POINT('Ctrl Pts',(19.6498928874021,11.9894782636006,35.7612621764191));
#51106=CARTESIAN_POINT('Ctrl Pts',(19.5719621164874,11.9937022565267,35.7756131967381));
#51107=CARTESIAN_POINT('Ctrl Pts',(19.4940562734901,11.9979248983131,35.7899596265591));
#51108=CARTESIAN_POINT('Ctrl Pts',(19.4168448657247,12.0021475400996,35.8082321394577));
#51109=CARTESIAN_POINT('Ctrl Pts',(19.3407473471902,12.0063701818861,35.8303356237842));
#51110=CARTESIAN_POINT('Ctrl Pts',(19.2646504771337,12.0105927876886,35.852438919752));
#51111=CARTESIAN_POINT('Ctrl Pts',(19.1896679272032,12.0148153934911,35.8783729901076));
#51112=CARTESIAN_POINT('Ctrl Pts',(19.116204527019,12.0190379992936,35.9079927000947));
#51113=CARTESIAN_POINT('Ctrl Pts',(19.0426680769127,12.0232648039355,35.9376418630814));
#51114=CARTESIAN_POINT('Ctrl Pts',(18.9706542297579,12.0274916085775,35.9709838106444));
#51115=CARTESIAN_POINT('Ctrl Pts',(18.9005477594611,12.0317184132195,36.0078252435148));
#51116=CARTESIAN_POINT('Ctrl Pts',(18.8304073167971,12.035947266097,36.044684529098));
#51117=CARTESIAN_POINT('Ctrl Pts',(18.7621764962502,12.0401761189744,36.0850464392235));
#51118=CARTESIAN_POINT('Ctrl Pts',(18.696213144297,12.0444049718519,36.1286729657928));
#51119=CARTESIAN_POINT('Ctrl Pts',(18.6301312417454,12.0486414249047,36.1723778987906));
#51120=CARTESIAN_POINT('Ctrl Pts',(18.5663253286885,12.0528778779574,36.2193588929237));
#51121=CARTESIAN_POINT('Ctrl Pts',(18.5051218811585,12.0571143310102,36.2693362267448));
#51122=CARTESIAN_POINT('Ctrl Pts',(18.4494957543052,12.0609647264443,36.3147592482104));
#51123=CARTESIAN_POINT('Ctrl Pts',(18.3960191538544,12.0648151218784,36.3626567102708));
#51124=CARTESIAN_POINT('Ctrl Pts',(18.344909854166,12.0686655173126,36.4127931217355));
#51125=CARTESIAN_POINT('Ctrl Pts',(18.2893631618179,12.0728502103508,36.4672824581194));
#51126=CARTESIAN_POINT('Ctrl Pts',(18.2363912731082,12.0770349033891,36.5246348089381));
#51127=CARTESIAN_POINT('Ctrl Pts',(18.1863097270532,12.0812195964274,36.5845733159542));
#51128=CARTESIAN_POINT('Ctrl Pts',(18.1364025412697,12.0853897203425,36.6443031454198));
#51129=CARTESIAN_POINT('Ctrl Pts',(18.089365962541,12.0895598442576,36.7066008259692));
#51130=CARTESIAN_POINT('Ctrl Pts',(18.0454776458662,12.0937299681727,36.7711535799457));
#51131=CARTESIAN_POINT('Ctrl Pts',(18.0016311623586,12.0978961172374,36.8356448039671));
#51132=CARTESIAN_POINT('Ctrl Pts',(17.9609272596224,12.1020622663021,36.9023864408502));
#51133=CARTESIAN_POINT('Ctrl Pts',(17.9236031437762,12.1062284153669,36.971032978177));
#51134=CARTESIAN_POINT('Ctrl Pts',(17.8863021886088,12.1103919792172,37.0396369183689));
#51135=CARTESIAN_POINT('Ctrl Pts',(17.8523770889213,12.1145555430676,37.1101429896707));
#51136=CARTESIAN_POINT('Ctrl Pts',(17.8220206330937,12.118719106918,37.1821784932622));
#51137=CARTESIAN_POINT('Ctrl Pts',(17.7914112549676,12.1229173605274,37.2548141784179));
#51138=CARTESIAN_POINT('Ctrl Pts',(17.7644305105462,12.1271156141369,37.3290044660351));
#51139=CARTESIAN_POINT('Ctrl Pts',(17.7412271533729,12.1313138677463,37.4043451515011));
#51140=CARTESIAN_POINT('Ctrl Pts',(17.7182126026396,12.1354779600354,37.479072787463));
#51141=CARTESIAN_POINT('Ctrl Pts',(17.6989142830347,12.1396420523245,37.5549316847391));
#51142=CARTESIAN_POINT('Ctrl Pts',(17.6834270820676,12.1438061446135,37.6315126930192));
#51143=CARTESIAN_POINT('Ctrl Pts',(17.6677493005859,12.1480214788832,37.7090360825593));
#51144=CARTESIAN_POINT('Ctrl Pts',(17.6559771855541,12.1522368131528,37.7872989801367));
#51145=CARTESIAN_POINT('Ctrl Pts',(17.648155372092,12.1564521474225,37.8658690813235));
#51146=CARTESIAN_POINT('Ctrl Pts',(17.6403335586299,12.1606674816921,37.9444391825103));
#51147=CARTESIAN_POINT('Ctrl Pts',(17.6364620348551,12.1648828159617,38.02331597533));
#51148=CARTESIAN_POINT('Ctrl Pts',(17.636530903764,12.1690981502314,38.10206689074));
#51149=CARTESIAN_POINT('',(17.6365304462654,12.9628481502994,38.0985475986668));
#51150=CARTESIAN_POINT('Ctrl Pts',(17.6365309037646,12.1690981502717,38.1020668914937));
#51151=CARTESIAN_POINT('Ctrl Pts',(17.6366294876699,12.175132280472,38.21479656999));
#51152=CARTESIAN_POINT('Ctrl Pts',(17.6447967865786,12.1811664106723,38.3271841533755));
#51153=CARTESIAN_POINT('Ctrl Pts',(17.660866537229,12.1872005408726,38.4382973311233));
#51154=CARTESIAN_POINT('Ctrl Pts',(17.6672472245105,12.1895964646589,38.4824161513517));
#51155=CARTESIAN_POINT('Ctrl Pts',(17.6748733071161,12.1919923884453,38.5263343998155));
#51156=CARTESIAN_POINT('Ctrl Pts',(17.6837324628504,12.1943883122316,38.5699948268302));
#51157=CARTESIAN_POINT('Ctrl Pts',(17.6994015479786,12.1986259546091,38.6472165134263));
#51158=CARTESIAN_POINT('Ctrl Pts',(17.7189659915919,12.2028635969866,38.7237987115027));
#51159=CARTESIAN_POINT('Ctrl Pts',(17.7423588860591,12.2071012393641,38.7993189841149));
#51160=CARTESIAN_POINT('Ctrl Pts',(17.765718140626,12.2113327878455,38.8747306556113));
#51161=CARTESIAN_POINT('Ctrl Pts',(17.7928947751503,12.215564336327,38.9490829902201));
#51162=CARTESIAN_POINT('Ctrl Pts',(17.8237709043756,12.2197958848084,39.0219638627723));
#51163=CARTESIAN_POINT('Ctrl Pts',(17.8546113708191,12.2240225457345,39.0947605559041));
#51164=CARTESIAN_POINT('Ctrl Pts',(17.8891426584629,12.2282492066606,39.1660887350197));
#51165=CARTESIAN_POINT('Ctrl Pts',(17.9271976045251,12.2324758675867,39.2355530239552));
#51166=CARTESIAN_POINT('Ctrl Pts',(17.9652285291196,12.2366998605127,39.3049734648668));
#51167=CARTESIAN_POINT('Ctrl Pts',(18.0067784726181,12.2409238534387,39.3725319408648));
#51168=CARTESIAN_POINT('Ctrl Pts',(18.0516333680824,12.2451478463648,39.4378557128965));
#51169=CARTESIAN_POINT('Ctrl Pts',(18.096473915695,12.2493704881512,39.5031585896441));
#51170=CARTESIAN_POINT('Ctrl Pts',(18.1446170507948,12.2535931299377,39.5662277957552));
#51171=CARTESIAN_POINT('Ctrl Pts',(18.1958050280076,12.2578157717241,39.6267190127648));
#51172=CARTESIAN_POINT('Ctrl Pts',(18.2469925690134,12.2620383775266,39.6872097142881));
#51173=CARTESIAN_POINT('Ctrl Pts',(18.3012245966393,12.2662609833291,39.7451221134685));
#51174=CARTESIAN_POINT('Ctrl Pts',(18.3582036398034,12.2704835891316,39.8001456268641));
#51175=CARTESIAN_POINT('Ctrl Pts',(18.4152393413126,12.2747103937736,39.8552238540815));
#51176=CARTESIAN_POINT('Ctrl Pts',(18.4750271766593,12.2789371984156,39.9074071310377));
#51177=CARTESIAN_POINT('Ctrl Pts',(18.5372338591295,12.2831640030576,39.9564228122986));
#51178=CARTESIAN_POINT('Ctrl Pts',(18.599470685868,12.287392855935,40.0054622456999));
#51179=CARTESIAN_POINT('Ctrl Pts',(18.6641283119256,12.2916217088125,40.0513307540042));
#51180=CARTESIAN_POINT('Ctrl Pts',(18.7308435903827,12.2958505616899,40.0937984975487));
#51181=CARTESIAN_POINT('Ctrl Pts',(18.7976787708152,12.3000870147427,40.1363425649347));
#51182=CARTESIAN_POINT('Ctrl Pts',(18.8665785841266,12.3043234677955,40.1754734233001));
#51183=CARTESIAN_POINT('Ctrl Pts',(18.937154568891,12.3085599208483,40.2110068759885));
#51184=CARTESIAN_POINT('Ctrl Pts',(19.0012991365544,12.3124103162824,40.2433022519283));
#51185=CARTESIAN_POINT('Ctrl Pts',(19.0668277772106,12.3162607117166,40.2726264897086));
#51186=CARTESIAN_POINT('Ctrl Pts',(19.133436707561,12.3201111071507,40.2988766452662));
#51187=CARTESIAN_POINT('Ctrl Pts',(19.2067447172969,12.3243487495282,40.3277668653774));
#51188=CARTESIAN_POINT('Ctrl Pts',(19.2816366628692,12.3285863919057,40.3530412991894));
#51189=CARTESIAN_POINT('Ctrl Pts',(19.3577217554161,12.3328240342832,40.3745261259072));
#51190=CARTESIAN_POINT('Ctrl Pts',(19.4336974346141,12.3370555827646,40.3959800566009));
#51191=CARTESIAN_POINT('Ctrl Pts',(19.5108624059776,12.3412871312461,40.4136550762709));
#51192=CARTESIAN_POINT('Ctrl Pts',(19.5888067819264,12.3455186797276,40.4274257406651));
#51193=CARTESIAN_POINT('Ctrl Pts',(19.6666611299686,12.3497453406537,40.4411804995616));
#51194=CARTESIAN_POINT('Ctrl Pts',(19.7452926343172,12.3539720015798,40.4510397838242));
#51195=CARTESIAN_POINT('Ctrl Pts',(19.8242786340817,12.3581986625059,40.4569286035983));
#51196=CARTESIAN_POINT('Ctrl Pts',(19.9032147754217,12.3624226554319,40.4628137061659));
#51197=CARTESIAN_POINT('Ctrl Pts',(19.9825045017686,12.3666466483579,40.4647332841742));
#51198=CARTESIAN_POINT('Ctrl Pts',(20.0617186101721,12.3708706412839,40.4626640163295));
#51199=CARTESIAN_POINT('Ctrl Pts',(20.1409073801535,12.3750932830704,40.460595410387));
#51200=CARTESIAN_POINT('Ctrl Pts',(20.2200201119486,12.3793159248569,40.4545405045538));
#51201=CARTESIAN_POINT('Ctrl Pts',(20.2986276679923,12.3835385666433,40.4445280882961));
#51202=CARTESIAN_POINT('Ctrl Pts',(20.3772345541679,12.3877611724458,40.434515757361));
#51203=CARTESIAN_POINT('Ctrl Pts',(20.4553358083166,12.3919837782483,40.4205460437042));
#51204=CARTESIAN_POINT('Ctrl Pts',(20.5325089679762,12.3962063840508,40.4026994245722));
#51205=CARTESIAN_POINT('Ctrl Pts',(20.6097588664379,12.4004331886928,40.3848350592681));
#51206=CARTESIAN_POINT('Ctrl Pts',(20.68607836919,12.4046599933347,40.3630861938033));
#51207=CARTESIAN_POINT('Ctrl Pts',(20.7610573430146,12.4088867979767,40.3375840010028));
#51208=CARTESIAN_POINT('Ctrl Pts',(20.8360726503362,12.4131156508542,40.3120694502865));
#51209=CARTESIAN_POINT('Ctrl Pts',(20.9097456984525,12.4173445037316,40.2827981222891));
#51210=CARTESIAN_POINT('Ctrl Pts',(20.9816860085487,12.4215733566091,40.2499495392961));
#51211=CARTESIAN_POINT('Ctrl Pts',(21.0537556111472,12.4258098096619,40.2170419202012));
#51212=CARTESIAN_POINT('Ctrl Pts',(21.1240858363615,12.4300462627146,40.1805444165595));
#51213=CARTESIAN_POINT('Ctrl Pts',(21.1923107142304,12.4342827157674,40.1406826312858));
#51214=CARTESIAN_POINT('Ctrl Pts',(21.2543184256263,12.4381331112015,40.104453353137));
#51215=CARTESIAN_POINT('Ctrl Pts',(21.3145871456284,12.4419835066356,40.0654457249484));
#51216=CARTESIAN_POINT('Ctrl Pts',(21.3728651577554,12.4458339020698,40.0238585445716));
#51217=CARTESIAN_POINT('Ctrl Pts',(21.4370043813992,12.4500715444472,39.9780888045694));
#51218=CARTESIAN_POINT('Ctrl Pts',(21.4989726316662,12.4543091868247,39.9290221511788));
#51219=CARTESIAN_POINT('Ctrl Pts',(21.5584113756626,12.4585468292022,39.8768917876746));
#51220=CARTESIAN_POINT('Ctrl Pts',(21.6177646444126,12.4627783776837,39.8248363896789));
#51221=CARTESIAN_POINT('Ctrl Pts',(21.6745952811693,12.4670099261651,39.7697263374953));
#51222=CARTESIAN_POINT('Ctrl Pts',(21.7285749384423,12.4712414746466,39.7118371887661));
#51223=CARTESIAN_POINT('Ctrl Pts',(21.7824922477204,12.4754681355727,39.6540149036023));
#51224=CARTESIAN_POINT('Ctrl Pts',(21.8335648033793,12.4796947964988,39.5934202419499));
#51225=CARTESIAN_POINT('Ctrl Pts',(21.8814996295203,12.4839214574249,39.5303669406887));
#51226=CARTESIAN_POINT('Ctrl Pts',(21.9294041977053,12.4881454503509,39.467353440636));
#51227=CARTESIAN_POINT('Ctrl Pts',(21.974174684751,12.4923694432769,39.4018847536659));
#51228=CARTESIAN_POINT('Ctrl Pts',(22.0155578967642,12.496593436203,39.3343082296134));
#51229=CARTESIAN_POINT('Ctrl Pts',(22.0569278714223,12.5008160779894,39.2667533214386));
#51230=CARTESIAN_POINT('Ctrl Pts',(22.09491247802,12.5050387197759,39.1970923145672));
#51231=CARTESIAN_POINT('Ctrl Pts',(22.1293022722832,12.5092613615623,39.1257008697226));
#51232=CARTESIAN_POINT('Ctrl Pts',(22.1636917734877,12.5134839673648,39.0543100332526));
#51233=CARTESIAN_POINT('Ctrl Pts',(22.1944863211164,12.5177065731673,38.9811892110775));
#51234=CARTESIAN_POINT('Ctrl Pts',(22.2215234635945,12.5219291789698,38.9067365998882));
#51235=CARTESIAN_POINT('Ctrl Pts',(22.2485874910406,12.5261559836118,38.8322099551331));
#51236=CARTESIAN_POINT('Ctrl Pts',(22.2718864897644,12.5303827882538,38.7563493177261));
#51237=CARTESIAN_POINT('Ctrl Pts',(22.2913072463144,12.5346095928957,38.6795701371597));
#51238=CARTESIAN_POINT('Ctrl Pts',(22.3107374138227,12.5388384457732,38.6027537507478));
#51239=CARTESIAN_POINT('Ctrl Pts',(22.3262855032581,12.5430672986506,38.5250183947225));
#51240=CARTESIAN_POINT('Ctrl Pts',(22.3378895585545,12.5472961515281,38.446789349464));
#51241=CARTESIAN_POINT('Ctrl Pts',(22.3495144688812,12.5515326045809,38.3684197094681));
#51242=CARTESIAN_POINT('Ctrl Pts',(22.357181136506,12.5557690576337,38.2895550750729));
#51243=CARTESIAN_POINT('Ctrl Pts',(22.3608796019484,12.5600055106864,38.2106252502993));
#51244=CARTESIAN_POINT('Ctrl Pts',(22.3642410352691,12.5638559061206,38.1388881076613));
#51245=CARTESIAN_POINT('Ctrl Pts',(22.3643252059902,12.5677063015547,38.0670973938957));
#51246=CARTESIAN_POINT('Ctrl Pts',(22.3611618609618,12.5715566969889,37.995572478534));
#51247=CARTESIAN_POINT('Ctrl Pts',(22.3576803679109,12.5757943393664,37.9168540669924));
#51248=CARTESIAN_POINT('Ctrl Pts',(22.3502514631331,12.5800319817439,37.8381621875518));
#51249=CARTESIAN_POINT('Ctrl Pts',(22.3388756111042,12.5842696241213,37.7599245426642));
#51250=CARTESIAN_POINT('Ctrl Pts',(22.3275161179968,12.5885011726028,37.6817994065802));
#51251=CARTESIAN_POINT('Ctrl Pts',(22.3122210162743,12.5927327210843,37.604127667903));
#51252=CARTESIAN_POINT('Ctrl Pts',(22.2930427311057,12.5969642695657,37.5273347625153));
#51253=CARTESIAN_POINT('Ctrl Pts',(22.273886597386,12.6011909304918,37.4506305550539));
#51254=CARTESIAN_POINT('Ctrl Pts',(22.2508563064176,12.6054175914179,37.374803616172));
#51255=CARTESIAN_POINT('Ctrl Pts',(22.2240555647086,12.609644252344,37.3002704919858));
#51256=CARTESIAN_POINT('Ctrl Pts',(22.197271740463,12.61386824527,37.2257844154303));
#51257=CARTESIAN_POINT('Ctrl Pts',(22.1667223477699,12.618092238196,37.1525909724864));
#51258=CARTESIAN_POINT('Ctrl Pts',(22.1325609447152,12.6223162311221,37.0810916341616));
#51259=CARTESIAN_POINT('Ctrl Pts',(22.098410468957,12.6265388729085,37.0096151665153));
#51260=CARTESIAN_POINT('Ctrl Pts',(22.0606504791455,12.630761514695,36.939832150056));
#51261=CARTESIAN_POINT('Ctrl Pts',(22.0194820969255,12.6349841564814,36.8721227662762));
#51262=CARTESIAN_POINT('Ctrl Pts',(21.9783140655291,12.6392067622839,36.8044139594937));
#51263=CARTESIAN_POINT('Ctrl Pts',(21.9337379442344,12.6434293680864,36.7387791500589));
#51264=CARTESIAN_POINT('Ctrl Pts',(21.8859993391751,12.6476519738889,36.6755713659396));
#51265=CARTESIAN_POINT('Ctrl Pts',(21.8382132642003,12.6518787785308,36.6123007297917));
#51266=CARTESIAN_POINT('Ctrl Pts',(21.7872587071196,12.6561055831728,36.5514623146082));
#51267=CARTESIAN_POINT('Ctrl Pts',(21.7334225489425,12.6603323878148,36.4933772354042));
#51268=CARTESIAN_POINT('Ctrl Pts',(21.6795603027065,12.6645612406922,36.4352640091885));
#51269=CARTESIAN_POINT('Ctrl Pts',(21.6228140096196,12.6687900935697,36.3799071046296));
#51270=CARTESIAN_POINT('Ctrl Pts',(21.5635066987201,12.6730189464471,36.3275899898846));
#51271=CARTESIAN_POINT('Ctrl Pts',(21.5040927995864,12.6772553994999,36.2751788498197));
#51272=CARTESIAN_POINT('Ctrl Pts',(21.442109053553,12.6814918525527,36.2258187082233));
#51273=CARTESIAN_POINT('Ctrl Pts',(21.3779105879832,12.6857283056055,36.1797518773805));
#51274=CARTESIAN_POINT('Ctrl Pts',(21.3195623717677,12.6895787010396,36.1378830043082));
#51275=CARTESIAN_POINT('Ctrl Pts',(21.2593852859931,12.6934290964738,36.0987341599395));
#51276=CARTESIAN_POINT('Ctrl Pts',(21.1976634316755,12.697279491908,36.0624542347895));
#51277=CARTESIAN_POINT('Ctrl Pts',(21.1297340072963,12.7015171342855,36.0225255181428));
#51278=CARTESIAN_POINT('Ctrl Pts',(21.0596781233794,12.705754776663,35.9859225996151));
#51279=CARTESIAN_POINT('Ctrl Pts',(20.9878548184795,12.7099924190405,35.952877903214));
#51280=CARTESIAN_POINT('Ctrl Pts',(20.9161347983107,12.7142239675219,35.9198807263831));
#51281=CARTESIAN_POINT('Ctrl Pts',(20.8426528269265,12.7184555160034,35.8904318043761));
#51282=CARTESIAN_POINT('Ctrl Pts',(20.767794325582,12.7226870644849,35.8647187392849));
#51283=CARTESIAN_POINT('Ctrl Pts',(20.6930222878737,12.726913725411,35.839035373494));
#51284=CARTESIAN_POINT('Ctrl Pts',(20.6168773209006,12.7311403863371,35.8170794411071));
#51285=CARTESIAN_POINT('Ctrl Pts',(20.5397653028354,12.7353670472632,35.7989906869474));
#51286=CARTESIAN_POINT('Ctrl Pts',(20.462701960279,12.7395910401892,35.7809133509729));
#51287=CARTESIAN_POINT('Ctrl Pts',(20.3846732334631,12.7438150331153,35.766698454722));
#51288=CARTESIAN_POINT('Ctrl Pts',(20.3060994905254,12.7480390260413,35.7564357182275));
#51289=CARTESIAN_POINT('Ctrl Pts',(20.2275508811745,12.7522616678277,35.746176264501));
#51290=CARTESIAN_POINT('Ctrl Pts',(20.1484580663881,12.7564843096142,35.7398665207724));
#51291=CARTESIAN_POINT('Ctrl Pts',(20.0692494457552,12.7607069514007,35.7375447189073));
#51292=CARTESIAN_POINT('Ctrl Pts',(19.9900415001122,12.7649295572032,35.7352229368279));
#51293=CARTESIAN_POINT('Ctrl Pts',(19.910718219198,12.7691521630057,35.7368890413476));
#51294=CARTESIAN_POINT('Ctrl Pts',(19.8317094388776,12.7733747688082,35.7425291671079));
#51295=CARTESIAN_POINT('Ctrl Pts',(19.7526220944659,12.7776015734501,35.7481749012493));
#51296=CARTESIAN_POINT('Ctrl Pts',(19.6738503439991,12.7818283780921,35.7578025166216));
#51297=CARTESIAN_POINT('Ctrl Pts',(19.5958197199819,12.7860551827341,35.7713461523566));
#51298=CARTESIAN_POINT('Ctrl Pts',(19.5177512836915,12.7902840356116,35.7848963511001));
#51299=CARTESIAN_POINT('Ctrl Pts',(19.4404251471274,12.794512888489,35.8023662470807));
#51300=CARTESIAN_POINT('Ctrl Pts',(19.3642549387221,12.7987417413665,35.8236391634979));
#51301=CARTESIAN_POINT('Ctrl Pts',(19.2879478357604,12.8029781944193,35.8449503120076));
#51302=CARTESIAN_POINT('Ctrl Pts',(19.2128012575486,12.8072146474721,35.8700779886578));
#51303=CARTESIAN_POINT('Ctrl Pts',(19.1392117804505,12.8114511005249,35.8988561878003));
#51304=CARTESIAN_POINT('Ctrl Pts',(19.0723283326503,12.8153014959589,35.9250118999488));
#51305=CARTESIAN_POINT('Ctrl Pts',(19.0067311100855,12.819151891393,35.9541823997606));
#51306=CARTESIAN_POINT('Ctrl Pts',(18.9426996584608,12.8230022868271,35.9862104104994));
#51307=CARTESIAN_POINT('Ctrl Pts',(18.8722283529694,12.8272399292046,36.0214595837071));
#51308=CARTESIAN_POINT('Ctrl Pts',(18.8033894442427,12.831477571582,36.060302924982));
#51309=CARTESIAN_POINT('Ctrl Pts',(18.7365733426896,12.8357152139595,36.1025657651633));
#51310=CARTESIAN_POINT('Ctrl Pts',(18.6698533253128,12.839946762441,36.1447678297219));
#51311=CARTESIAN_POINT('Ctrl Pts',(18.6051507312514,12.8441783109224,36.1903793792192));
#51312=CARTESIAN_POINT('Ctrl Pts',(18.5428327323031,12.8484098594038,36.2391792147408));
#51313=CARTESIAN_POINT('Ctrl Pts',(18.4805867123643,12.8526365203299,36.2879226851049));
#51314=CARTESIAN_POINT('Ctrl Pts',(18.4207201813142,12.856863181256,36.33984683577));
#51315=CARTESIAN_POINT('Ctrl Pts',(18.3635713004658,12.8610898421821,36.3946872567647));
#51316=CARTESIAN_POINT('Ctrl Pts',(18.3064584937719,12.8653138351081,36.4494930607767));
#51317=CARTESIAN_POINT('Ctrl Pts',(18.252060269619,12.8695378280341,36.5072111575306));
#51318=CARTESIAN_POINT('Ctrl Pts',(18.2006807125478,12.8737618209602,36.5675377516224));
#51319=CARTESIAN_POINT('Ctrl Pts',(18.1493175903886,12.8779844627466,36.6278450488903));
#51320=CARTESIAN_POINT('Ctrl Pts',(18.1009715215737,12.8822071045331,36.690758829947));
#51321=CARTESIAN_POINT('Ctrl Pts',(18.0559077706933,12.8864297463195,36.7559405352257));
#51322=CARTESIAN_POINT('Ctrl Pts',(18.0108444038316,12.890652352122,36.8211216850471));
#51323=CARTESIAN_POINT('Ctrl Pts',(17.9690635646959,12.8948749579245,36.8885703342577));
#51324=CARTESIAN_POINT('Ctrl Pts',(17.9307875970201,12.8990975637269,36.9579183600749));
#51325=CARTESIAN_POINT('Ctrl Pts',(17.8924735688071,12.9033243683689,37.0273353436029));
#51326=CARTESIAN_POINT('Ctrl Pts',(17.857671600695,12.9075511730109,37.0986550650328));
#51327=CARTESIAN_POINT('Ctrl Pts',(17.8265580765977,12.9117779776529,37.171484708528));
#51328=CARTESIAN_POINT('Ctrl Pts',(17.7954294754318,12.9160068305303,37.2443496439924));
#51329=CARTESIAN_POINT('Ctrl Pts',(17.7679930413479,12.9202356834078,37.3187255187517));
#51330=CARTESIAN_POINT('Ctrl Pts',(17.7443760506119,12.9244645362852,37.3942018419924));
#51331=CARTESIAN_POINT('Ctrl Pts',(17.7207166149682,12.928700989338,37.4698138127258));
#51332=CARTESIAN_POINT('Ctrl Pts',(17.7008904559355,12.9329374423907,37.5465297287325));
#51333=CARTESIAN_POINT('Ctrl Pts',(17.6849741873614,12.9371738954435,37.6239265521821));
#51334=CARTESIAN_POINT('Ctrl Pts',(17.6705083294649,12.9410242908777,37.6942703921629));
#51335=CARTESIAN_POINT('Ctrl Pts',(17.6592716173198,12.9448746863119,37.7651763155258));
#51336=CARTESIAN_POINT('Ctrl Pts',(17.6512842832292,12.9487250817461,37.8363242091241));
#51337=CARTESIAN_POINT('Ctrl Pts',(17.6415185618787,12.9534327712546,37.9233132464774));
#51338=CARTESIAN_POINT('Ctrl Pts',(17.6365843354261,12.9581404607632,38.0108546571211));
#51339=CARTESIAN_POINT('Ctrl Pts',(17.6365304462657,12.9628481502717,38.0985475981509));
#51340=CARTESIAN_POINT('',(17.6365301790272,13.7565981502284,38.0990800810601));
#51341=CARTESIAN_POINT('Ctrl Pts',(17.6365304462654,12.9628481502994,38.0985475986668));
#51342=CARTESIAN_POINT('Ctrl Pts',(17.6364826128399,12.9670268198915,38.1763861701059));
#51343=CARTESIAN_POINT('Ctrl Pts',(17.640284307832,12.9712054894835,38.2543759824577));
#51344=CARTESIAN_POINT('Ctrl Pts',(17.6479539514616,12.9753841590756,38.3320987428979));
#51345=CARTESIAN_POINT('Ctrl Pts',(17.6556128976047,12.9795570003315,38.4097130969743));
#51346=CARTESIAN_POINT('Ctrl Pts',(17.6671290306768,12.9837298415874,38.4870606623887));
#51347=CARTESIAN_POINT('Ctrl Pts',(17.6824687502264,12.9879026828433,38.5637233520351));
#51348=CARTESIAN_POINT('Ctrl Pts',(17.6977966391079,12.99207230582,38.6403269160354));
#51349=CARTESIAN_POINT('Ctrl Pts',(17.7169421724458,12.9962419287968,38.7162461806144));
#51350=CARTESIAN_POINT('Ctrl Pts',(17.7398201132759,13.0004115517735,38.7910696929744));
#51351=CARTESIAN_POINT('Ctrl Pts',(17.7626879857003,13.0045793397313,38.8658602760824));
#51352=CARTESIAN_POINT('Ctrl Pts',(17.7892848659156,13.008747127689,38.9395556029792));
#51353=CARTESIAN_POINT('Ctrl Pts',(17.8194751502271,13.0129149156468,39.0117575447579));
#51354=CARTESIAN_POINT('Ctrl Pts',(17.8496621445242,13.017082249416,39.0839516182627));
#51355=CARTESIAN_POINT('Ctrl Pts',(17.8834415781697,13.0212495831852,39.1546521852162));
#51356=CARTESIAN_POINT('Ctrl Pts',(17.9206296373,13.0254169169544,39.2234809013174));
#51357=CARTESIAN_POINT('Ctrl Pts',(17.9578512201433,13.0295880074267,39.2923716640587));
#51358=CARTESIAN_POINT('Ctrl Pts',(17.9984873370944,13.0337590978991,39.3593867795776));
#51359=CARTESIAN_POINT('Ctrl Pts',(18.0423084863937,13.0379301883715,39.4241730923312));
#51360=CARTESIAN_POINT('Ctrl Pts',(18.0861484987403,13.042103074312,39.4889872926984));
#51361=CARTESIAN_POINT('Ctrl Pts',(18.133175982708,13.0462759602526,39.5515703941878));
#51362=CARTESIAN_POINT('Ctrl Pts',(18.183120018302,13.0504488461931,39.6116009966275));
#51363=CARTESIAN_POINT('Ctrl Pts',(18.2331526724192,13.0546291363208,39.6717381147556));
#51364=CARTESIAN_POINT('Ctrl Pts',(18.2861118880157,13.0588094264485,39.7293133313685));
#51365=CARTESIAN_POINT('Ctrl Pts',(18.3416889378209,13.0629897165762,39.7840412292917));
#51366=CARTESIAN_POINT('Ctrl Pts',(18.3924677685148,13.0668091032726,39.8340442192421));
#51367=CARTESIAN_POINT('Ctrl Pts',(18.4454312783559,13.0706284899689,39.8816705988585));
#51368=CARTESIAN_POINT('Ctrl Pts',(18.5003215091152,13.0744478766652,39.9267333863697));
#51369=CARTESIAN_POINT('Ctrl Pts',(18.5612226920721,13.0786855190427,39.9767309365493));
#51370=CARTESIAN_POINT('Ctrl Pts',(18.6247412175117,13.0829231614202,40.0237734433076));
#51371=CARTESIAN_POINT('Ctrl Pts',(18.6905585163841,13.0871608037977,40.0675755238074));
#51372=CARTESIAN_POINT('Ctrl Pts',(18.756281167398,13.0913923522792,40.1113146151965));
#51373=CARTESIAN_POINT('Ctrl Pts',(18.8242956399514,13.0956239007607,40.1518222768073));
#51374=CARTESIAN_POINT('Ctrl Pts',(18.8942503390128,13.0998554492421,40.1888533045972));
#51375=CARTESIAN_POINT('Ctrl Pts',(18.9641242384648,13.1040821101682,40.2258415605273));
#51376=CARTESIAN_POINT('Ctrl Pts',(19.0359334987553,13.1083087710944,40.2593609444544));
#51377=CARTESIAN_POINT('Ctrl Pts',(19.1092988811206,13.1125354320205,40.2892103502695));
#51378=CARTESIAN_POINT('Ctrl Pts',(19.1826179529704,13.1167594249465,40.3190409142095));
#51379=CARTESIAN_POINT('Ctrl Pts',(19.2574907641177,13.1209834178725,40.3452059220412));
#51380=CARTESIAN_POINT('Ctrl Pts',(19.3335159898157,13.1252074107985,40.3675514338309));
#51381=CARTESIAN_POINT('Ctrl Pts',(19.409516897128,13.129430052585,40.3898897979039));
#51382=CARTESIAN_POINT('Ctrl Pts',(19.4866690375485,13.1336526943715,40.4084109599972));
#51383=CARTESIAN_POINT('Ctrl Pts',(19.5645551530859,13.1378753361579,40.4230105953689));
#51384=CARTESIAN_POINT('Ctrl Pts',(19.6424406049032,13.1420979419604,40.4376101063272));
#51385=CARTESIAN_POINT('Ctrl Pts',(19.7210595583898,13.1463205477629,40.4482880720475));
#51386=CARTESIAN_POINT('Ctrl Pts',(19.7999852427785,13.1505431535654,40.4549914092823));
#51387=CARTESIAN_POINT('Ctrl Pts',(19.8789894086302,13.1547699582074,40.4617014121257));
#51388=CARTESIAN_POINT('Ctrl Pts',(19.9583004464542,13.1589967628494,40.4644288520671));
#51389=CARTESIAN_POINT('Ctrl Pts',(20.0374877584534,13.1632235674913,40.4631726785968));
#51390=CARTESIAN_POINT('Ctrl Pts',(20.1167134432364,13.1674524203688,40.4619158964067));
#51391=CARTESIAN_POINT('Ctrl Pts',(20.1958148144115,13.1716812732463,40.4566716862937));
#51392=CARTESIAN_POINT('Ctrl Pts',(20.2743651388343,13.1759101261237,40.4474910460942));
#51393=CARTESIAN_POINT('Ctrl Pts',(20.3530566354036,13.1801465791765,40.4382939062724));
#51394=CARTESIAN_POINT('Ctrl Pts',(20.4311946430298,13.1843830322293,40.4251462785399));
#51395=CARTESIAN_POINT('Ctrl Pts',(20.5083616097451,13.1886194852821,40.408150539856));
#51396=CARTESIAN_POINT('Ctrl Pts',(20.5784965392721,13.1924698807161,40.3927035813244));
#51397=CARTESIAN_POINT('Ctrl Pts',(20.6478292455125,13.1963202761502,40.3740786111803));
#51398=CARTESIAN_POINT('Ctrl Pts',(20.7160591422646,13.2001706715843,40.3523875656022));
#51399=CARTESIAN_POINT('Ctrl Pts',(20.7911511443299,13.2044083139617,40.3285149801684));
#51400=CARTESIAN_POINT('Ctrl Pts',(20.8651889687577,13.2086459563392,40.3008382558305));
#51401=CARTESIAN_POINT('Ctrl Pts',(20.9377598086829,13.2128835987167,40.2694692858206));
#51402=CARTESIAN_POINT('Ctrl Pts',(21.0102262888923,13.2171151471982,40.2381454256207));
#51403=CARTESIAN_POINT('Ctrl Pts',(21.0812295472923,13.2213466956796,40.2031400485707));
#51404=CARTESIAN_POINT('Ctrl Pts',(21.1503725044909,13.225578244161,40.1646146230741));
#51405=CARTESIAN_POINT('Ctrl Pts',(21.2194355996647,13.2298049050871,40.1261336955077));
#51406=CARTESIAN_POINT('Ctrl Pts',(21.2866422562177,13.2340315660132,40.0841410261804));
#51407=CARTESIAN_POINT('Ctrl Pts',(21.35161733962,13.2382582269393,40.0388452769983));
#51408=CARTESIAN_POINT('Ctrl Pts',(21.4165514087248,13.2424822198654,39.9935781199046));
#51409=CARTESIAN_POINT('Ctrl Pts',(21.479256317124,13.2467062127914,39.9450122888448));
#51410=CARTESIAN_POINT('Ctrl Pts',(21.5393844742776,13.2509302057174,39.8934006471654));
#51411=CARTESIAN_POINT('Ctrl Pts',(21.5994933980818,13.2551528475038,39.8418055146355));
#51412=CARTESIAN_POINT('Ctrl Pts',(21.6570268519539,13.2593754892903,39.7871668112994));
#51413=CARTESIAN_POINT('Ctrl Pts',(21.711670192899,13.2635981310767,39.7297777736983));
#51414=CARTESIAN_POINT('Ctrl Pts',(21.7663130681914,13.2678207368792,39.6723892251479));
#51415=CARTESIAN_POINT('Ctrl Pts',(21.8180655573098,13.2720433426817,39.612250729413));
#51416=CARTESIAN_POINT('Ctrl Pts',(21.8666508239462,13.2762659484842,39.5496913955601));
#51417=CARTESIAN_POINT('Ctrl Pts',(21.9152844023945,13.2804927531261,39.4870698544791));
#51418=CARTESIAN_POINT('Ctrl Pts',(21.9607441792256,13.2847195577681,39.422023037956));
#51419=CARTESIAN_POINT('Ctrl Pts',(22.0027948835204,13.2889463624101,39.3549115886965));
#51420=CARTESIAN_POINT('Ctrl Pts',(22.0448659648496,13.2931752152875,39.2877676184046));
#51421=CARTESIAN_POINT('Ctrl Pts',(22.0835244538215,13.297404068165,39.2185574320744));
#51422=CARTESIAN_POINT('Ctrl Pts',(22.1185808448557,13.3016329210424,39.1476667622439));
#51423=CARTESIAN_POINT('Ctrl Pts',(22.1537002399067,13.3058693740952,39.0766486863448));
#51424=CARTESIAN_POINT('Ctrl Pts',(22.1852044149956,13.310105827148,39.0039445234467));
#51425=CARTESIAN_POINT('Ctrl Pts',(22.2129519624632,13.3143422802008,38.9299602717783));
#51426=CARTESIAN_POINT('Ctrl Pts',(22.2381709437073,13.318192675635,38.8627180242476));
#51427=CARTESIAN_POINT('Ctrl Pts',(22.2602873153771,13.3220430710692,38.7944188311924));
#51428=CARTESIAN_POINT('Ctrl Pts',(22.279231357355,13.3258934665034,38.7253757754739));
#51429=CARTESIAN_POINT('Ctrl Pts',(22.3000806639933,13.3301311088809,38.6493888323705));
#51430=CARTESIAN_POINT('Ctrl Pts',(22.3171649754614,13.3343687512583,38.5722154767498));
#51431=CARTESIAN_POINT('Ctrl Pts',(22.3303534499209,13.3386063936358,38.4942629063728));
#51432=CARTESIAN_POINT('Ctrl Pts',(22.3435229588367,13.3428379421173,38.4164224348513));
#51433=CARTESIAN_POINT('Ctrl Pts',(22.3528076789724,13.3470694905987,38.3378054322512));
#51434=CARTESIAN_POINT('Ctrl Pts',(22.3581269165168,13.3513010390802,38.2588328885931));
#51435=CARTESIAN_POINT('Ctrl Pts',(22.363440010195,13.3555277000063,38.1799515604037));
#51436=CARTESIAN_POINT('Ctrl Pts',(22.3647966920309,13.3597543609324,38.1007159725868));
#51437=CARTESIAN_POINT('Ctrl Pts',(22.3621678026812,13.3639810218585,38.0215543954304));
#51438=CARTESIAN_POINT('Ctrl Pts',(22.3595405727684,13.3682050147845,37.9424427875283));
#51439=CARTESIAN_POINT('Ctrl Pts',(22.3529327808065,13.3724290077105,37.8634055648463));
#51440=CARTESIAN_POINT('Ctrl Pts',(22.3423673397802,13.3766530006365,37.784871952326));
#51441=CARTESIAN_POINT('Ctrl Pts',(22.331805278349,13.380875642423,37.7063634605558));
#51442=CARTESIAN_POINT('Ctrl Pts',(22.3172881442246,13.3850982842095,37.6283587233051));
#51443=CARTESIAN_POINT('Ctrl Pts',(22.2988906526755,13.3893209259959,37.5512813034522));
#51444=CARTESIAN_POINT('Ctrl Pts',(22.2804933179039,13.3935435317984,37.4742045404281));
#51445=CARTESIAN_POINT('Ctrl Pts',(22.2582158016787,13.3977661376009,37.3980555347218));
#51446=CARTESIAN_POINT('Ctrl Pts',(22.2321834910903,13.4019887434034,37.3232456610973));
#51447=CARTESIAN_POINT('Ctrl Pts',(22.2061252947101,13.4062155480453,37.2483613986554));
#51448=CARTESIAN_POINT('Ctrl Pts',(22.1763050003823,13.4104423526873,37.1748193719255));
#51449=CARTESIAN_POINT('Ctrl Pts',(22.1428970732627,13.4146691573293,37.1030132526948));
#51450=CARTESIAN_POINT('Ctrl Pts',(22.1094729572469,13.4188980102067,37.0311723374768));
#51451=CARTESIAN_POINT('Ctrl Pts',(22.0724579642951,13.4231268630842,36.9610694205743));
#51452=CARTESIAN_POINT('Ctrl Pts',(22.0320725183102,13.4273557159616,36.8930734400021));
#51453=CARTESIAN_POINT('Ctrl Pts',(21.9916144908288,13.4315921690144,36.8249552557522));
#51454=CARTESIAN_POINT('Ctrl Pts',(21.9477741669369,13.4358286220672,36.7589519652903));
#51455=CARTESIAN_POINT('Ctrl Pts',(21.9008151521759,13.44006507512,36.6954031901793));
#51456=CARTESIAN_POINT('Ctrl Pts',(21.8581353977266,13.4439154705541,36.6376454597181));
#51457=CARTESIAN_POINT('Ctrl Pts',(21.8128801453055,13.4477658659883,36.5819150748636));
#51458=CARTESIAN_POINT('Ctrl Pts',(21.7652740788398,13.4516162614224,36.528440943688));
#51459=CARTESIAN_POINT('Ctrl Pts',(21.7128801135627,13.4558539037999,36.469588743117));
#51460=CARTESIAN_POINT('Ctrl Pts',(21.6574414846348,13.4600915461774,36.4132490684755));
#51461=CARTESIAN_POINT('Ctrl Pts',(21.5992285551981,13.4643291885549,36.3597533309502));
#51462=CARTESIAN_POINT('Ctrl Pts',(21.5410993382385,13.4685607370364,36.3063345223949));
#51463=CARTESIAN_POINT('Ctrl Pts',(21.4802040859639,13.4727922855178,36.255751843776));
#51464=CARTESIAN_POINT('Ctrl Pts',(21.4168520287486,13.4770238339993,36.2083021463429));
#51465=CARTESIAN_POINT('Ctrl Pts',(21.3535731449087,13.4812504949254,36.1609072546206));
#51466=CARTESIAN_POINT('Ctrl Pts',(21.2878434686099,13.4854771558515,36.1166384324546));
#51467=CARTESIAN_POINT('Ctrl Pts',(21.2200063894486,13.4897038167776,36.0757532634077));
#51468=CARTESIAN_POINT('Ctrl Pts',(21.1522121311656,13.4939278097036,36.0348939023535));
#51469=CARTESIAN_POINT('Ctrl Pts',(21.0823135108773,13.4981518026296,35.9974141963021));
#51470=CARTESIAN_POINT('Ctrl Pts',(21.0106830638267,13.5023757955557,35.9635285666797));
#51471=CARTESIAN_POINT('Ctrl Pts',(20.9390755293927,13.5065984373421,35.9296537761413));
#51472=CARTESIAN_POINT('Ctrl Pts',(20.8657376917039,13.5108210791286,35.8993709793767));
#51473=CARTESIAN_POINT('Ctrl Pts',(20.7910655341056,13.5150437209151,35.8728480604929));
#51474=CARTESIAN_POINT('Ctrl Pts',(20.7163940128394,13.5192663267175,35.8463253676289));
#51475=CARTESIAN_POINT('Ctrl Pts',(20.6403886364857,13.52348893252,35.8235626444933));
#51476=CARTESIAN_POINT('Ctrl Pts',(20.5634627466488,13.5277115383225,35.8046786338208));
#51477=CARTESIAN_POINT('Ctrl Pts',(20.4864603638877,13.5319383429645,35.7857758454233));
#51478=CARTESIAN_POINT('Ctrl Pts',(20.4085360955777,13.5361651476065,35.7707595856452));
#51479=CARTESIAN_POINT('Ctrl Pts',(20.3301151478045,13.5403919522485,35.7596977908633));
#51480=CARTESIAN_POINT('Ctrl Pts',(20.2516561986142,13.5446208051259,35.7486306357295));
#51481=CARTESIAN_POINT('Ctrl Pts',(20.1727005579758,13.5488496580034,35.7415218051048));
#51482=CARTESIAN_POINT('Ctrl Pts',(20.093677700594,13.5530785108808,35.7383872185916));
#51483=CARTESIAN_POINT('Ctrl Pts',(20.0145128218205,13.5573149639336,35.7352469985396));
#51484=CARTESIAN_POINT('Ctrl Pts',(19.9352809547857,13.5615514169864,35.7360952891515));
#51485=CARTESIAN_POINT('Ctrl Pts',(19.8564104868735,13.5657878700392,35.7408958283662));
#51486=CARTESIAN_POINT('Ctrl Pts',(19.7847272920522,13.5696382654733,35.7452589061681));
#51487=CARTESIAN_POINT('Ctrl Pts',(19.7133428366945,13.5734886609074,35.752886041988));
#51488=CARTESIAN_POINT('Ctrl Pts',(19.6425714478075,13.5773390563415,35.7637133585586));
#51489=CARTESIAN_POINT('Ctrl Pts',(19.5646823473772,13.581576698719,35.7756296139977));
#51490=CARTESIAN_POINT('Ctrl Pts',(19.4872436049088,13.5858143410965,35.7914675962248));
#51491=CARTESIAN_POINT('Ctrl Pts',(19.4106803987692,13.590051983474,35.8111809052472));
#51492=CARTESIAN_POINT('Ctrl Pts',(19.3342272935246,13.5942835319554,35.8308658657576));
#51493=CARTESIAN_POINT('Ctrl Pts',(19.2586476744575,13.5985150804369,35.8544149699349));
#51494=CARTESIAN_POINT('Ctrl Pts',(19.1843588855393,13.6027466289184,35.8817304011232));
#51495=CARTESIAN_POINT('Ctrl Pts',(19.1101559022238,13.6069732898445,35.9090142822341));
#51496=CARTESIAN_POINT('Ctrl Pts',(19.0372412239228,13.6111999507706,35.9400556844346));
#51497=CARTESIAN_POINT('Ctrl Pts',(18.9660178482963,13.6154266116967,35.9747067612073));
#51498=CARTESIAN_POINT('Ctrl Pts',(18.8948394310842,13.6196506046227,36.0093359651404));
#51499=CARTESIAN_POINT('Ctrl Pts',(18.825350617903,13.6238745975487,36.0475701164525));
#51500=CARTESIAN_POINT('Ctrl Pts',(18.7579340641067,13.6280985904747,36.0892134246038));
#51501=CARTESIAN_POINT('Ctrl Pts',(18.690539075018,13.6323212322612,36.1308434122023));
#51502=CARTESIAN_POINT('Ctrl Pts',(18.6252154275414,13.6365438740477,36.1758801449555));
#51503=CARTESIAN_POINT('Ctrl Pts',(18.5623195020174,13.6407665158341,36.2240828305545));
#51504=CARTESIAN_POINT('Ctrl Pts',(18.4994241124719,13.6449891216366,36.2722851053859));
#51505=CARTESIAN_POINT('Ctrl Pts',(18.4389567749458,13.6492117274391,36.3236529931348));
#51506=CARTESIAN_POINT('Ctrl Pts',(18.3812420953924,13.6534343332416,36.3779043908161));
#51507=CARTESIAN_POINT('Ctrl Pts',(18.3234700259979,13.6576611378836,36.4322097345491));
#51508=CARTESIAN_POINT('Ctrl Pts',(18.2684564244321,13.6618879425256,36.4894039938075));
#51509=CARTESIAN_POINT('Ctrl Pts',(18.2164897350997,13.6661147471676,36.5491674571717));
#51510=CARTESIAN_POINT('Ctrl Pts',(18.1644978636203,13.6703436000451,36.6089598808629));
#51511=CARTESIAN_POINT('Ctrl Pts',(18.1155561354708,13.6745724529225,36.6713236195836));
#51512=CARTESIAN_POINT('Ctrl Pts',(18.0699116834311,13.6788013058,36.7359070665294));
#51513=CARTESIAN_POINT('Ctrl Pts',(18.0241851983087,13.6830377588528,36.8006065840822));
#51514=CARTESIAN_POINT('Ctrl Pts',(17.9817680814153,13.6872742119055,36.867533383985));
#51515=CARTESIAN_POINT('Ctrl Pts',(17.9428631001573,13.6915106649583,36.9363083672185));
#51516=CARTESIAN_POINT('Ctrl Pts',(17.9075034348117,13.6953610603924,36.9988160542204));
#51517=CARTESIAN_POINT('Ctrl Pts',(17.8750444964466,13.6992114558265,37.0628498811227));
#51518=CARTESIAN_POINT('Ctrl Pts',(17.8456037998514,13.7030618512606,37.1281113985208));
#51519=CARTESIAN_POINT('Ctrl Pts',(17.8102375024772,13.7076872251708,37.2065082606305));
#51520=CARTESIAN_POINT('Ctrl Pts',(17.7791119595227,13.712312599081,37.2869312211764));
#51521=CARTESIAN_POINT('Ctrl Pts',(17.7524417551234,13.7169379729913,37.3689238228562));
#51522=CARTESIAN_POINT('Ctrl Pts',(17.7258416135051,13.7215511960175,37.4507010294978));
#51523=CARTESIAN_POINT('Ctrl Pts',(17.7036736021471,13.7261644190438,37.5340393592405));
#51524=CARTESIAN_POINT('Ctrl Pts',(17.6861045739136,13.73077764207,37.6184624645612));
#51525=CARTESIAN_POINT('Ctrl Pts',(17.6686127640987,13.7353705893142,37.7025145181311));
#51526=CARTESIAN_POINT('Ctrl Pts',(17.6556797311303,13.7399635365585,37.7876415314826));
#51527=CARTESIAN_POINT('Ctrl Pts',(17.6474222125353,13.7445564838027,37.8733544731799));
#51528=CARTESIAN_POINT('Ctrl Pts',(17.6402057652928,13.7485703726113,37.9482611070111));
#51529=CARTESIAN_POINT('Ctrl Pts',(17.636559551907,13.7525842614199,38.0236148285961));
#51530=CARTESIAN_POINT('Ctrl Pts',(17.6365301790272,13.7565981502284,38.0990800810601));
#51531=CARTESIAN_POINT('',(17.6365309503988,14.5503481503104,38.1021195464647));
#51532=CARTESIAN_POINT('Ctrl Pts',(17.6365301790269,13.7565981502717,38.0990800818733));
#51533=CARTESIAN_POINT('Ctrl Pts',(17.6364986455271,13.7609072978428,38.1800965038199));
#51534=CARTESIAN_POINT('Ctrl Pts',(17.6406371502407,13.765216445414,38.2610898530213));
#51535=CARTESIAN_POINT('Ctrl Pts',(17.6489123164394,13.7695255929851,38.34161362774));
#51536=CARTESIAN_POINT('Ctrl Pts',(17.6571923099408,13.7738372542894,38.4221843758518));
#51537=CARTESIAN_POINT('Ctrl Pts',(17.6696137192139,13.7781489155937,38.5022845658516));
#51538=CARTESIAN_POINT('Ctrl Pts',(17.6860915665036,13.782460576898,38.5814750276955));
#51539=CARTESIAN_POINT('Ctrl Pts',(17.7025966209716,13.7867793573445,38.6607962438168));
#51540=CARTESIAN_POINT('Ctrl Pts',(17.7231713963529,13.791098137791,38.7392042997413));
#51541=CARTESIAN_POINT('Ctrl Pts',(17.7476802625299,13.7954169182375,38.8162724628956));
#51542=CARTESIAN_POINT('Ctrl Pts',(17.7722111442425,13.7997395781072,38.893409853932));
#51543=CARTESIAN_POINT('Ctrl Pts',(17.8006830009683,13.8040622379769,38.9692045418666));
#51544=CARTESIAN_POINT('Ctrl Pts',(17.8329119001906,13.8083848978467,39.0432494943356));
#51545=CARTESIAN_POINT('Ctrl Pts',(17.8652070717965,13.812716446415,39.117446705666));
#51546=CARTESIAN_POINT('Ctrl Pts',(17.9012745212117,13.8170479949834,39.1898865993884));
#51547=CARTESIAN_POINT('Ctrl Pts',(17.9408842013788,13.8213795435518,39.2601864370733));
#51548=CARTESIAN_POINT('Ctrl Pts',(17.9634560939373,13.8238479110944,39.3002473609788));
#51549=CARTESIAN_POINT('Ctrl Pts',(17.9871774796518,13.826316278637,39.339613849284));
#51550=CARTESIAN_POINT('Ctrl Pts',(18.0119997541912,13.8287846461796,39.3782196460562));
#51551=CARTESIAN_POINT('Ctrl Pts',(18.0546141220591,13.8330222885571,39.4444972799964));
#51552=CARTESIAN_POINT('Ctrl Pts',(18.1006265355379,13.8372599309346,39.508765921821));
#51553=CARTESIAN_POINT('Ctrl Pts',(18.1498214031218,13.8414975733121,39.5706561802657));
#51554=CARTESIAN_POINT('Ctrl Pts',(18.1989455265555,13.8457291217936,39.63245743809));
#51555=CARTESIAN_POINT('Ctrl Pts',(18.2512427263197,13.849960670275,39.6918867408173));
#51556=CARTESIAN_POINT('Ctrl Pts',(18.3064536463111,13.8541922187565,39.7486027989807));
#51557=CARTESIAN_POINT('Ctrl Pts',(18.3616007961654,13.8584188796826,39.8052533485308));
#51558=CARTESIAN_POINT('Ctrl Pts',(18.4196546529653,13.8626455406087,39.8591965471098));
#51559=CARTESIAN_POINT('Ctrl Pts',(18.4803160154472,13.8668722015348,39.9101245890804));
#51560=CARTESIAN_POINT('Ctrl Pts',(18.5409390865866,13.8710961944608,39.9610204836839));
#51561=CARTESIAN_POINT('Ctrl Pts',(18.6041660383181,13.8753201873868,40.0089046988142));
#51562=CARTESIAN_POINT('Ctrl Pts',(18.6696621718654,13.8795441803128,40.0535075387452));
#51563=CARTESIAN_POINT('Ctrl Pts',(18.735137354995,13.8837668220993,40.0980961114502));
#51564=CARTESIAN_POINT('Ctrl Pts',(18.8028798913659,13.8879894638858,40.1394051296273));
#51565=CARTESIAN_POINT('Ctrl Pts',(18.8725246886765,13.8922121056722,40.1772072268447));
#51566=CARTESIAN_POINT('Ctrl Pts',(18.9421688924969,13.8964347114747,40.215009001925));
#51567=CARTESIAN_POINT('Ctrl Pts',(19.0137149123486,13.9006573172772,40.2493036930975));
#51568=CARTESIAN_POINT('Ctrl Pts',(19.0867728737301,13.9048799230797,40.2799097817903));
#51569=CARTESIAN_POINT('Ctrl Pts',(19.1599034818773,13.9091067277217,40.3105463043099));
#51570=CARTESIAN_POINT('Ctrl Pts',(19.234548601295,13.9133335323637,40.3374867162676));
#51571=CARTESIAN_POINT('Ctrl Pts',(19.3102987436765,13.9175603370057,40.3605978452449));
#51572=CARTESIAN_POINT('Ctrl Pts',(19.3860855932496,13.9217891898831,40.3837201734703));
#51573=CARTESIAN_POINT('Ctrl Pts',(19.4629780772484,13.9260180427606,40.4030094079282));
#51574=CARTESIAN_POINT('Ctrl Pts',(19.5405544091374,13.930246895638,40.4183830981822));
#51575=CARTESIAN_POINT('Ctrl Pts',(19.6182701626948,13.9344833486908,40.4337844183266));
#51576=CARTESIAN_POINT('Ctrl Pts',(19.6966717549177,13.9387198017436,40.445256065448));
#51577=CARTESIAN_POINT('Ctrl Pts',(19.7753303663308,13.9429562547963,40.4527673060902));
#51578=CARTESIAN_POINT('Ctrl Pts',(19.8468210106192,13.9468066502305,40.4595940657198));
#51579=CARTESIAN_POINT('Ctrl Pts',(19.9185236541111,13.9506570456646,40.4631499880943));
#51580=CARTESIAN_POINT('Ctrl Pts',(19.9901178623789,13.9545074410988,40.4634493403194));
#51581=CARTESIAN_POINT('Ctrl Pts',(20.0689125358425,13.9587450834763,40.4637787993832));
#51582=CARTESIAN_POINT('Ctrl Pts',(20.1478716078969,13.9629827258538,40.4601641823324));
#51583=CARTESIAN_POINT('Ctrl Pts',(20.2265678540668,13.9672203682312,40.4525852691037));
#51584=CARTESIAN_POINT('Ctrl Pts',(20.3051509319465,13.9714519167127,40.4450172546495));
#51585=CARTESIAN_POINT('Ctrl Pts',(20.3834714717638,13.9756834651942,40.4334963098714));
#51586=CARTESIAN_POINT('Ctrl Pts',(20.4611020001047,13.9799150136756,40.4180542242147));
#51587=CARTESIAN_POINT('Ctrl Pts',(20.5386428630417,13.9841416746017,40.4026299745933));
#51588=CARTESIAN_POINT('Ctrl Pts',(20.615494840868,13.9883683355278,40.3832936754001));
#51589=CARTESIAN_POINT('Ctrl Pts',(20.6912368595323,13.9925949964539,40.3601287673325));
#51590=CARTESIAN_POINT('Ctrl Pts',(20.7669310674742,13.99681898938,40.3369784816767));
#51591=CARTESIAN_POINT('Ctrl Pts',(20.841516259845,14.001042982306,40.3100045208452));
#51592=CARTESIAN_POINT('Ctrl Pts',(20.9145840092054,14.005266975232,40.2793408478267));
#51593=CARTESIAN_POINT('Ctrl Pts',(20.9876283861956,14.0094896170185,40.2486869832766));
#51594=CARTESIAN_POINT('Ctrl Pts',(21.0591558521197,14.0137122588049,40.2143459315276));
#51595=CARTESIAN_POINT('Ctrl Pts',(21.1287769439355,14.0179349005914,40.1765001930507));
#51596=CARTESIAN_POINT('Ctrl Pts',(21.198397442463,14.0221575063939,40.138654777083));
#51597=CARTESIAN_POINT('Ctrl Pts',(21.2661111880111,14.0263801121964,40.0973049589083));
#51598=CARTESIAN_POINT('Ctrl Pts',(21.3315536879893,14.0306027179988,40.0526789846009));
#51599=CARTESIAN_POINT('Ctrl Pts',(21.3970612621344,14.0348295226408,40.0080086354898));
#51600=CARTESIAN_POINT('Ctrl Pts',(21.4602926912241,14.0390563272828,39.9600558876579));
#51601=CARTESIAN_POINT('Ctrl Pts',(21.5209133621982,14.0432831319248,39.9090917570944));
#51602=CARTESIAN_POINT('Ctrl Pts',(21.5815634088872,14.0475119848022,39.8581029302063));
#51603=CARTESIAN_POINT('Ctrl Pts',(21.6395998335552,14.0517408376797,39.8041001333042));
#51604=CARTESIAN_POINT('Ctrl Pts',(21.6947238778059,14.0559696905572,39.7473923087396));
#51605=CARTESIAN_POINT('Ctrl Pts',(21.749946992044,14.0602061436099,39.6905825677875));
#51606=CARTESIAN_POINT('Ctrl Pts',(21.8022469573061,14.0644425966627,39.6310584383577));
#51607=CARTESIAN_POINT('Ctrl Pts',(21.8513645706152,14.0686790497155,39.5691629138971));
#51608=CARTESIAN_POINT('Ctrl Pts',(21.8960062157988,14.0725294451496,39.5129077773939));
#51609=CARTESIAN_POINT('Ctrl Pts',(21.9380194603227,14.0763798405837,39.454694368697));
#51610=CARTESIAN_POINT('Ctrl Pts',(21.9772418485556,14.0802302360178,39.3947992559546));
#51611=CARTESIAN_POINT('Ctrl Pts',(22.0204089614837,14.0844678783952,39.3288802945633));
#51612=CARTESIAN_POINT('Ctrl Pts',(22.0603570047894,14.0887055207727,39.2606765237577));
#51613=CARTESIAN_POINT('Ctrl Pts',(22.0968364630553,14.0929431631502,39.1905353218038));
#51614=CARTESIAN_POINT('Ctrl Pts',(22.1332634624287,14.0971747116316,39.1204949856508));
#51615=CARTESIAN_POINT('Ctrl Pts',(22.1662315678807,14.1014062601131,39.0485231637431));
#51616=CARTESIAN_POINT('Ctrl Pts',(22.1955347575789,14.1056378085945,38.9749957537971));
#51617=CARTESIAN_POINT('Ctrl Pts',(22.2248041012839,14.1098644695206,38.9015532700399));
#51618=CARTESIAN_POINT('Ctrl Pts',(22.2504167687586,14.1140911304467,38.8265592020938));
#51619=CARTESIAN_POINT('Ctrl Pts',(22.2722135501325,14.1183177913728,38.750412195069));
#51620=CARTESIAN_POINT('Ctrl Pts',(22.2939965726987,14.1225417842988,38.674313254408));
#51621=CARTESIAN_POINT('Ctrl Pts',(22.3119683615138,14.1267657772248,38.5970632687079));
#51622=CARTESIAN_POINT('Ctrl Pts',(22.3260189722204,14.1309897701509,38.5190777753241));
#51623=CARTESIAN_POINT('Ctrl Pts',(22.3400650885218,14.1352124119373,38.441117227362));
#51624=CARTESIAN_POINT('Ctrl Pts',(22.3501924344012,14.1394350537238,38.3624220999262));
#51625=CARTESIAN_POINT('Ctrl Pts',(22.3563421050171,14.1436576955102,38.2834184424301));
#51626=CARTESIAN_POINT('Ctrl Pts',(22.3624917232275,14.1478803013127,38.2044154581773));
#51627=CARTESIAN_POINT('Ctrl Pts',(22.3646636986166,14.1521029071152,38.1251044165617));
#51628=CARTESIAN_POINT('Ctrl Pts',(22.3628510931506,14.1563255129177,38.0459153210517));
#51629=CARTESIAN_POINT('Ctrl Pts',(22.3610366852811,14.1605523175597,37.9666474821502));
#51630=CARTESIAN_POINT('Ctrl Pts',(22.3552297928876,14.1647791222016,37.8875023013112));
#51631=CARTESIAN_POINT('Ctrl Pts',(22.3454756207214,14.1690059268436,37.8089079982177));
#51632=CARTESIAN_POINT('Ctrl Pts',(22.3357167218543,14.173234779721,37.7302756097021));
#51633=CARTESIAN_POINT('Ctrl Pts',(22.3220068139017,14.1774636325985,37.6521950930199));
#51634=CARTESIAN_POINT('Ctrl Pts',(22.3044424337787,14.1816924854759,37.5750852352049));
#51635=CARTESIAN_POINT('Ctrl Pts',(22.2868464866157,14.1859289385287,37.4978367940776));
#51636=CARTESIAN_POINT('Ctrl Pts',(22.2653823530887,14.1901653915815,37.4215629497883));
#51637=CARTESIAN_POINT('Ctrl Pts',(22.2401966658929,14.1944018446342,37.3466678428328));
#51638=CARTESIAN_POINT('Ctrl Pts',(22.2173060888518,14.1982522400685,37.2785977440324));
#51639=CARTESIAN_POINT('Ctrl Pts',(22.191342048871,14.2021026355027,37.2116665682194));
#51640=CARTESIAN_POINT('Ctrl Pts',(22.1624481196334,14.2059530309369,37.1461611400274));
#51641=CARTESIAN_POINT('Ctrl Pts',(22.1306482328213,14.2101906733143,37.0740676152958));
#51642=CARTESIAN_POINT('Ctrl Pts',(22.0951794394757,14.2144283156918,37.0034307607884));
#51643=CARTESIAN_POINT('Ctrl Pts',(22.0561973238576,14.2186659580693,36.9346489772344));
#51644=CARTESIAN_POINT('Ctrl Pts',(22.0172712660515,14.2228975065508,36.8659661045843));
#51645=CARTESIAN_POINT('Ctrl Pts',(21.9748421485907,14.2271290550322,36.7991334096114));
#51646=CARTESIAN_POINT('Ctrl Pts',(21.9291131548827,14.2313606035137,36.7345283318361));
#51647=CARTESIAN_POINT('Ctrl Pts',(21.8834369794253,14.2355872644398,36.6699978747097));
#51648=CARTESIAN_POINT('Ctrl Pts',(21.8344687714853,14.2398139253659,36.6076903023494));
#51649=CARTESIAN_POINT('Ctrl Pts',(21.7824562779356,14.244040586292,36.5479561674528));
#51650=CARTESIAN_POINT('Ctrl Pts',(21.7304766162926,14.248264579218,36.4882597386035));
#51651=CARTESIAN_POINT('Ctrl Pts',(21.6754567903276,14.252488572144,36.4311338755057));
#51652=CARTESIAN_POINT('Ctrl Pts',(21.6176855342393,14.25671256507,36.3768969986641));
#51653=CARTESIAN_POINT('Ctrl Pts',(21.5599327575922,14.2609352068565,36.3226774707126));
#51654=CARTESIAN_POINT('Ctrl Pts',(21.4994306400565,14.265157848643,36.2713454145448));
#51655=CARTESIAN_POINT('Ctrl Pts',(21.4365045166777,14.2693804904294,36.2231821573566));
#51656=CARTESIAN_POINT('Ctrl Pts',(21.3735789295349,14.2736030962319,36.1750193106));
#51657=CARTESIAN_POINT('Ctrl Pts',(21.3082297507391,14.2778257020344,36.1300254929143));
#51658=CARTESIAN_POINT('Ctrl Pts',(21.2408139196441,14.2820483078368,36.0884405905573));
#51659=CARTESIAN_POINT('Ctrl Pts',(21.1733310521579,14.2862751124788,36.0468143373523));
#51660=CARTESIAN_POINT('Ctrl Pts',(21.1037778273624,14.2905019171208,36.0086040171511));
#51661=CARTESIAN_POINT('Ctrl Pts',(21.0325380714226,14.2947287217628,35.9740048043415));
#51662=CARTESIAN_POINT('Ctrl Pts',(20.9612637939451,14.2989575746402,35.9393888253596));
#51663=CARTESIAN_POINT('Ctrl Pts',(20.8883017892339,14.3031864275177,35.9083876232862));
#51664=CARTESIAN_POINT('Ctrl Pts',(20.8140559126307,14.3074152803951,35.8811481770945));
#51665=CARTESIAN_POINT('Ctrl Pts',(20.7396765999173,14.3116517334479,35.8538597756489));
#51666=CARTESIAN_POINT('Ctrl Pts',(20.6640092536251,14.3158881865007,35.8303467780549));
#51667=CARTESIAN_POINT('Ctrl Pts',(20.5874727115031,14.3201246395535,35.8107061669285));
#51668=CARTESIAN_POINT('Ctrl Pts',(20.5179107575141,14.3239750349876,35.7928553567193));
#51669=CARTESIAN_POINT('Ctrl Pts',(20.4476312140241,14.3278254304218,35.7782027312014));
#51670=CARTESIAN_POINT('Ctrl Pts',(20.3769528411782,14.331675825856,35.7667839799051));
#51671=CARTESIAN_POINT('Ctrl Pts',(20.2991661117201,14.3359134682335,35.7542168072032));
#51672=CARTESIAN_POINT('Ctrl Pts',(20.2206042195142,14.340151110611,35.7455202786349));
#51673=CARTESIAN_POINT('Ctrl Pts',(20.1416860600604,14.3443887529885,35.7407807432787));
#51674=CARTESIAN_POINT('Ctrl Pts',(20.0628813880167,14.3486203014699,35.7360480235604));
#51675=CARTESIAN_POINT('Ctrl Pts',(19.9837219302221,14.3528518499514,35.7352610244925));
#51676=CARTESIAN_POINT('Ctrl Pts',(19.9046349084043,14.3570833984329,35.7384547558421));
#51677=CARTESIAN_POINT('Ctrl Pts',(19.8256392342808,14.361310059359,35.7416447983437));
#51678=CARTESIAN_POINT('Ctrl Pts',(19.7467162958905,14.3655367202851,35.748806415352));
#51679=CARTESIAN_POINT('Ctrl Pts',(19.668295017955,14.3697633812112,35.7599225983343));
#51680=CARTESIAN_POINT('Ctrl Pts',(19.589923241974,14.3739873741372,35.7710317644354));
#51681=CARTESIAN_POINT('Ctrl Pts',(19.5120529608245,14.3782113670632,35.7860904761207));
#51682=CARTESIAN_POINT('Ctrl Pts',(19.4351084554308,14.3824353599893,35.8050298512237));
#51683=CARTESIAN_POINT('Ctrl Pts',(19.3581885624752,14.3866580017757,35.8239631681398));
#51684=CARTESIAN_POINT('Ctrl Pts',(19.2821943120779,14.3908806435622,35.8467745715013));
#51685=CARTESIAN_POINT('Ctrl Pts',(19.2075387919301,14.3951032853487,35.8733442846717));
#51686=CARTESIAN_POINT('Ctrl Pts',(19.1328839079724,14.3993258911512,35.8999137714236));
#51687=CARTESIAN_POINT('Ctrl Pts',(19.0595681727386,14.4035484969537,35.9302413457806));
#51688=CARTESIAN_POINT('Ctrl Pts',(18.9879871138078,14.4077711027561,35.9641581615015));
#51689=CARTESIAN_POINT('Ctrl Pts',(18.9163348767012,14.4119979073981,35.9981087031424));
#51690=CARTESIAN_POINT('Ctrl Pts',(18.8464211860292,14.4162247120401,36.0356554141299));
#51691=CARTESIAN_POINT('Ctrl Pts',(18.7786186974788,14.4204515166821,36.0765825554889));
#51692=CARTESIAN_POINT('Ctrl Pts',(18.7107833530305,14.4246803695596,36.1175295294235));
#51693=CARTESIAN_POINT('Ctrl Pts',(18.6450616378687,14.4289092224371,36.1618599345387));
#51694=CARTESIAN_POINT('Ctrl Pts',(18.5817966807019,14.4331380753145,36.2093149955554));
#51695=CARTESIAN_POINT('Ctrl Pts',(18.5184180225433,14.4373745283673,36.2568553437159));
#51696=CARTESIAN_POINT('Ctrl Pts',(18.4575053058653,14.4416109814201,36.3075312679571));
#51697=CARTESIAN_POINT('Ctrl Pts',(18.3993678745093,14.4458474344729,36.3610442099504));
#51698=CARTESIAN_POINT('Ctrl Pts',(18.3465283652661,14.4496978299069,36.4096806482508));
#51699=CARTESIAN_POINT('Ctrl Pts',(18.2959811000384,14.453548225341,36.4606599346863));
#51700=CARTESIAN_POINT('Ctrl Pts',(18.2479295300893,14.4573986207751,36.513734098782));
#51701=CARTESIAN_POINT('Ctrl Pts',(18.1956152135631,14.4615905921446,36.5715165733777));
#51702=CARTESIAN_POINT('Ctrl Pts',(18.1460536011349,14.4657825635142,36.6320102148364));
#51703=CARTESIAN_POINT('Ctrl Pts',(18.0995425725386,14.4699745348837,36.694919216804));
#51704=CARTESIAN_POINT('Ctrl Pts',(18.0530930388454,14.4741609638071,36.7577450431658));
#51705=CARTESIAN_POINT('Ctrl Pts',(18.009686371673,14.4783473927304,36.8229795146034));
#51706=CARTESIAN_POINT('Ctrl Pts',(17.969582416137,14.4825338216538,36.8902914086276));
#51707=CARTESIAN_POINT('Ctrl Pts',(17.9295183415414,14.4867160874286,36.9575363650744));
#51708=CARTESIAN_POINT('Ctrl Pts',(17.8927507061616,14.4908983532035,37.0268542355731));
#51709=CARTESIAN_POINT('Ctrl Pts',(17.859496993302,14.4950806189784,37.0978835800083));
#51710=CARTESIAN_POINT('Ctrl Pts',(17.8262654562584,14.4992600957366,37.1688655572916));
#51711=CARTESIAN_POINT('Ctrl Pts',(17.7965433924196,14.5034395724949,37.2415563094894));
#51712=CARTESIAN_POINT('Ctrl Pts',(17.7705023263606,14.5076190492532,37.31556991125));
#51713=CARTESIAN_POINT('Ctrl Pts',(17.7444633363955,14.5117981928075,37.3895776123614));
#51714=CARTESIAN_POINT('Ctrl Pts',(17.7221049331247,14.5159773363619,37.4649075058114));
#51715=CARTESIAN_POINT('Ctrl Pts',(17.7035499709274,14.5201564799162,37.5411550260828));
#51716=CARTESIAN_POINT('Ctrl Pts',(17.6849958812562,14.524335426951,37.6173989609012));
#51717=CARTESIAN_POINT('Ctrl Pts',(17.6702449825026,14.5285143739858,37.6945599686642));
#51718=CARTESIAN_POINT('Ctrl Pts',(17.6593693564179,14.5326933210207,37.7722216736504));
#51719=CARTESIAN_POINT('Ctrl Pts',(17.6484862171153,14.536875155001,37.8499370297378));
#51720=CARTESIAN_POINT('Ctrl Pts',(17.6414837496195,14.5410569889813,37.928153296773));
#51721=CARTESIAN_POINT('Ctrl Pts',(17.6383822176429,14.5452388229617,38.0064484582978));
#51722=CARTESIAN_POINT('Ctrl Pts',(17.637119076311,14.546941932065,38.0383352340443));
#51723=CARTESIAN_POINT('Ctrl Pts',(17.6365023565896,14.5486450411684,38.0702350809376));
#51724=CARTESIAN_POINT('Ctrl Pts',(17.6365309503982,14.5503481502717,38.1021195457395));
#51725=CARTESIAN_POINT('',(17.6365301165987,15.3440981503131,38.0992576019166));
#51726=CARTESIAN_POINT('Ctrl Pts',(17.6365309503988,14.5503481503104,38.1021195464647));
#51727=CARTESIAN_POINT('Ctrl Pts',(17.6366226564826,14.5558103612077,38.2043793903881));
#51728=CARTESIAN_POINT('Ctrl Pts',(17.6433550821026,14.561272572105,38.3063458974693));
#51729=CARTESIAN_POINT('Ctrl Pts',(17.6565905908059,14.5667347830023,38.407282901901));
#51730=CARTESIAN_POINT('Ctrl Pts',(17.6698260995093,14.5721969938996,38.5082199063327));
#51731=CARTESIAN_POINT('Ctrl Pts',(17.6895645153101,14.5776592047969,38.6081277364946));
#51732=CARTESIAN_POINT('Ctrl Pts',(17.7156187406071,14.5831214156942,38.7062942376721));
#51733=CARTESIAN_POINT('Ctrl Pts',(17.7358318907963,14.5873590580717,38.7824528725667));
#51734=CARTESIAN_POINT('Ctrl Pts',(17.7598957095871,14.5915967004492,38.8577425341505));
#51735=CARTESIAN_POINT('Ctrl Pts',(17.787718398304,14.5958343428268,38.9317454873321));
#51736=CARTESIAN_POINT('Ctrl Pts',(17.8155010769026,14.6000658913082,39.0056420213629));
#51737=CARTESIAN_POINT('Ctrl Pts',(17.8470317271923,14.6042974397897,39.0782550864287));
#51738=CARTESIAN_POINT('Ctrl Pts',(17.8821682727408,14.6085289882712,39.1491802590186));
#51739=CARTESIAN_POINT('Ctrl Pts',(17.9172642346088,14.6127556491973,39.2200235110755));
#51740=CARTESIAN_POINT('Ctrl Pts',(17.9559576079721,14.6169823101235,39.2891823270005));
#51741=CARTESIAN_POINT('Ctrl Pts',(17.9980581168457,14.6212089710496,39.356271920156));
#51742=CARTESIAN_POINT('Ctrl Pts',(18.0401320505661,14.6254329639756,39.4233191642698));
#51743=CARTESIAN_POINT('Ctrl Pts',(18.0856086023958,14.6296569569017,39.4882993821646));
#51744=CARTESIAN_POINT('Ctrl Pts',(18.134252014581,14.6338809498277,39.5508531613519));
#51745=CARTESIAN_POINT('Ctrl Pts',(18.182879867072,14.6381035916142,39.6133869312999));
#51746=CARTESIAN_POINT('Ctrl Pts',(18.2346722807604,14.6423262334007,39.6734954340356));
#51747=CARTESIAN_POINT('Ctrl Pts',(18.2893515785705,14.6465488751871,39.7308502135882));
#51748=CARTESIAN_POINT('Ctrl Pts',(18.3440304104214,14.6507714809896,39.7882045043821));
#51749=CARTESIAN_POINT('Ctrl Pts',(18.4015957529806,14.6549940867921,39.842804780346));
#51750=CARTESIAN_POINT('Ctrl Pts',(18.4617322702618,14.6592166925946,39.894358613139));
#51751=CARTESIAN_POINT('Ctrl Pts',(18.5219285855909,14.6634434972366,39.9459637096018));
#51752=CARTESIAN_POINT('Ctrl Pts',(18.5847008259455,14.6676703018786,39.9945160060486));
#51753=CARTESIAN_POINT('Ctrl Pts',(18.6497001484648,14.6718971065206,40.0397630659037));
#51754=CARTESIAN_POINT('Ctrl Pts',(18.7147309685168,14.6761259593981,40.0850320516911));
#51755=CARTESIAN_POINT('Ctrl Pts',(18.7819906224036,14.6803548122755,40.1269923617539));
#51756=CARTESIAN_POINT('Ctrl Pts',(18.8511029935441,14.684583665153,40.1654360579443));
#51757=CARTESIAN_POINT('Ctrl Pts',(18.9203395747608,14.6888201182058,40.2039488458814));
#51758=CARTESIAN_POINT('Ctrl Pts',(18.9914351047638,14.6930565712586,40.2389321842645));
#51759=CARTESIAN_POINT('Ctrl Pts',(19.0639908989435,14.6972930243114,40.2702251965267));
#51760=CARTESIAN_POINT('Ctrl Pts',(19.1299348608219,14.7011434197453,40.2986665530167));
#51761=CARTESIAN_POINT('Ctrl Pts',(19.1970845759434,14.7049938151792,40.3240600448236));
#51762=CARTESIAN_POINT('Ctrl Pts',(19.2651306994886,14.7088442106131,40.3463208924964));
#51763=CARTESIAN_POINT('Ctrl Pts',(19.3400204456741,14.7130818529906,40.3708205868983));
#51764=CARTESIAN_POINT('Ctrl Pts',(19.4162772940511,14.7173194953681,40.3916170671704));
#51765=CARTESIAN_POINT('Ctrl Pts',(19.4935008509108,14.7215571377456,40.4085599521936));
#51766=CARTESIAN_POINT('Ctrl Pts',(19.5706133572652,14.725788686227,40.4254784726832));
#51767=CARTESIAN_POINT('Ctrl Pts',(19.6486893572643,14.7300202347085,40.4385543034406));
#51768=CARTESIAN_POINT('Ctrl Pts',(19.7273122558831,14.73425178319,40.4476864856936));
#51769=CARTESIAN_POINT('Ctrl Pts',(19.8058443428827,14.7384784441161,40.4568081200239));
#51770=CARTESIAN_POINT('Ctrl Pts',(19.8849216099028,14.7427051050422,40.4619951040148));
#51771=CARTESIAN_POINT('Ctrl Pts',(19.9641176979259,14.7469317659683,40.4631976009843));
#51772=CARTESIAN_POINT('Ctrl Pts',(20.0432637949103,14.7511557588943,40.4643993389002));
#51773=CARTESIAN_POINT('Ctrl Pts',(20.1225280965307,14.7553797518203,40.4616215749565));
#51774=CARTESIAN_POINT('Ctrl Pts',(20.2014807719779,14.7596037447464,40.4548664377037));
#51775=CARTESIAN_POINT('Ctrl Pts',(20.2804081926282,14.7638263865328,40.4481134612341));
#51776=CARTESIAN_POINT('Ctrl Pts',(20.3590237183212,14.7680490283193,40.437385677831));
#51777=CARTESIAN_POINT('Ctrl Pts',(20.4369006684905,14.7722716701057,40.422737231538));
#51778=CARTESIAN_POINT('Ctrl Pts',(20.5147769550178,14.7764942759082,40.4080889100742));
#51779=CARTESIAN_POINT('Ctrl Pts',(20.591914218106,14.7807168817107,40.3895200802112));
#51780=CARTESIAN_POINT('Ctrl Pts',(20.6678955005168,14.7849394875132,40.3671360879509));
#51781=CARTESIAN_POINT('Ctrl Pts',(20.7439523365607,14.7891662921552,40.3447298376834));
#51782=CARTESIAN_POINT('Ctrl Pts',(20.8188504451349,14.7933930967972,40.3185009798862));
#51783=CARTESIAN_POINT('Ctrl Pts',(20.892188177814,14.7976199014392,40.2886047373313));
#51784=CARTESIAN_POINT('Ctrl Pts',(20.9655614486734,14.8018487543166,40.2586940075811));
#51785=CARTESIAN_POINT('Ctrl Pts',(21.037372412157,14.8060776071941,40.2251125516116));
#51786=CARTESIAN_POINT('Ctrl Pts',(21.1072419020736,14.8103064600716,40.1880626933099));
#51787=CARTESIAN_POINT('Ctrl Pts',(21.1772369627748,14.8145429131244,40.1509462482937));
#51788=CARTESIAN_POINT('Ctrl Pts',(21.2452831745163,14.8187793661771,40.1103491865972));
#51789=CARTESIAN_POINT('Ctrl Pts',(21.3110285649619,14.8230158192299,40.0665183809855));
#51790=CARTESIAN_POINT('Ctrl Pts',(21.3707827385673,14.826866214664,40.0266817696272));
#51791=CARTESIAN_POINT('Ctrl Pts',(21.4286364916091,14.8307166100982,39.9841746299141));
#51792=CARTESIAN_POINT('Ctrl Pts',(21.4843503179773,14.8345670055323,39.9392103127214));
#51793=CARTESIAN_POINT('Ctrl Pts',(21.5456674672597,14.8388046479098,39.889723786137));
#51794=CARTESIAN_POINT('Ctrl Pts',(21.6046222725346,14.8430422902873,39.837074650806));
#51795=CARTESIAN_POINT('Ctrl Pts',(21.6608706354333,14.8472799326648,39.7815169262471));
#51796=CARTESIAN_POINT('Ctrl Pts',(21.7170381109788,14.8515114811462,39.7260390958763));
#51797=CARTESIAN_POINT('Ctrl Pts',(21.7705065424822,14.8557430296277,39.667661309361));
#51798=CARTESIAN_POINT('Ctrl Pts',(21.8209644714277,14.8599745781092,39.6066780793183));
#51799=CARTESIAN_POINT('Ctrl Pts',(21.8713641200717,14.8642012390353,39.5457652865903));
#51800=CARTESIAN_POINT('Ctrl Pts',(21.9187598789322,14.8684278999614,39.4822533900328));
#51801=CARTESIAN_POINT('Ctrl Pts',(21.9628778592699,14.8726545608875,39.4164729205297));
#51802=CARTESIAN_POINT('Ctrl Pts',(22.0069679909635,14.8768785538135,39.3507339737089));
#51803=CARTESIAN_POINT('Ctrl Pts',(22.0477841905145,14.8811025467395,39.2827296845934));
#51804=CARTESIAN_POINT('Ctrl Pts',(22.0850942713132,14.8853265396655,39.212821782963));
#51805=CARTESIAN_POINT('Ctrl Pts',(22.1223924176397,14.889549181452,39.1429362429542));
#51806=CARTESIAN_POINT('Ctrl Pts',(22.1561864517544,14.8937718232384,39.0711487128743));
#51807=CARTESIAN_POINT('Ctrl Pts',(22.1862895359481,14.8979944650249,38.9978465937474));
#51808=CARTESIAN_POINT('Ctrl Pts',(22.2163923636132,14.9022170708274,38.9245450992773));
#51809=CARTESIAN_POINT('Ctrl Pts',(22.2428041271381,14.9064396766298,38.8497294755966));
#51810=CARTESIAN_POINT('Ctrl Pts',(22.26538623323,14.9106622824323,38.7738068381903));
#51811=CARTESIAN_POINT('Ctrl Pts',(22.287990794328,14.9148890870743,38.6978087054656));
#51812=CARTESIAN_POINT('Ctrl Pts',(22.306757957336,14.9191158917163,38.6207018105602));
#51813=CARTESIAN_POINT('Ctrl Pts',(22.3215993020975,14.9233426963583,38.5429075765895));
#51814=CARTESIAN_POINT('Ctrl Pts',(22.3364478387147,14.9275715492357,38.4650756448961));
#51815=CARTESIAN_POINT('Ctrl Pts',(22.3473667026679,14.9318004021132,38.3865561755179));
#51816=CARTESIAN_POINT('Ctrl Pts',(22.3543192232785,14.9360292549906,38.3077773707634));
#51817=CARTESIAN_POINT('Ctrl Pts',(22.3612842390922,14.9402657080434,38.2288569832333));
#51818=CARTESIAN_POINT('Ctrl Pts',(22.3642686506542,14.9445021610962,38.1496767986011));
#51819=CARTESIAN_POINT('Ctrl Pts',(22.363287960477,14.9487386141489,38.0706664566691));
#51820=CARTESIAN_POINT('Ctrl Pts',(22.3623966382002,14.9525890095831,37.9988561342048));
#51821=CARTESIAN_POINT('Ctrl Pts',(22.3582306298081,14.9564394050172,37.9271863494851));
#51822=CARTESIAN_POINT('Ctrl Pts',(22.3508385367489,14.9602898004514,37.855974150885));
#51823=CARTESIAN_POINT('Ctrl Pts',(22.3427029965578,14.9645274428289,37.777599907059));
#51824=CARTESIAN_POINT('Ctrl Pts',(22.3306285386171,14.9687650852063,37.6994858367418));
#51825=CARTESIAN_POINT('Ctrl Pts',(22.3146409466993,14.9730027275838,37.6220588647513));
#51826=CARTESIAN_POINT('Ctrl Pts',(22.2986763455661,14.9772342760653,37.5447432357851));
#51827=CARTESIAN_POINT('Ctrl Pts',(22.278809879646,14.9814658245467,37.468113198217));
#51828=CARTESIAN_POINT('Ctrl Pts',(22.255119068091,14.9856973730282,37.3925903381828));
#51829=CARTESIAN_POINT('Ctrl Pts',(22.2314556200775,14.9899240339543,37.3171547091374));
#51830=CARTESIAN_POINT('Ctrl Pts',(22.2039767441644,14.9941506948804,37.2428241613066));
#51831=CARTESIAN_POINT('Ctrl Pts',(22.1728106246247,14.9983773558065,37.1700083707806));
#51832=CARTESIAN_POINT('Ctrl Pts',(22.1416641781108,15.0026013487325,37.0972385438506));
#51833=CARTESIAN_POINT('Ctrl Pts',(22.10683529178,15.0068253416585,37.0259820061797));
#51834=CARTESIAN_POINT('Ctrl Pts',(22.0685010215988,15.0110493345845,36.9566304339608));
#51835=CARTESIAN_POINT('Ctrl Pts',(22.0301790134999,15.015271976371,36.887301045409));
#51836=CARTESIAN_POINT('Ctrl Pts',(21.9883540747974,15.0194946181574,36.8198758222411));
#51837=CARTESIAN_POINT('Ctrl Pts',(21.9432494812504,15.0237172599439,36.7547223726977));
#51838=CARTESIAN_POINT('Ctrl Pts',(21.89814527207,15.0279398657464,36.6895694783708));
#51839=CARTESIAN_POINT('Ctrl Pts',(21.8497617316133,15.0321624715489,36.6266887037883));
#51840=CARTESIAN_POINT('Ctrl Pts',(21.7983649346115,15.0363850773513,36.5664179177952));
#51841=CARTESIAN_POINT('Ctrl Pts',(21.7469170300919,15.0406118819933,36.5060872002412));
#51842=CARTESIAN_POINT('Ctrl Pts',(21.6924501887901,15.0448386866353,36.4483720129164));
#51843=CARTESIAN_POINT('Ctrl Pts',(21.635269798666,15.0490654912773,36.3935759241997));
#51844=CARTESIAN_POINT('Ctrl Pts',(21.5780616999267,15.0532943441547,36.3387532822585));
#51845=CARTESIAN_POINT('Ctrl Pts',(21.518137787653,15.0575231970322,36.2868528641554));
#51846=CARTESIAN_POINT('Ctrl Pts',(21.4558373057294,15.0617520499096,36.2381385174652));
#51847=CARTESIAN_POINT('Ctrl Pts',(21.3934248561873,15.0659885029624,36.1893366204188));
#51848=CARTESIAN_POINT('Ctrl Pts',(21.3286276869489,15.0702249560152,36.1437325064659));
#51849=CARTESIAN_POINT('Ctrl Pts',(21.2618146474872,15.074461409068,36.1015470392609));
#51850=CARTESIAN_POINT('Ctrl Pts',(21.201090117112,15.0783118045021,36.0632058306388));
#51851=CARTESIAN_POINT('Ctrl Pts',(21.1387009512912,15.0821621999363,36.0276881497473));
#51852=CARTESIAN_POINT('Ctrl Pts',(21.0749395671253,15.0860125953705,35.9951258071019));
#51853=CARTESIAN_POINT('Ctrl Pts',(21.0047654906677,15.0902502377479,35.9592885624698));
#51854=CARTESIAN_POINT('Ctrl Pts',(20.9326655724501,15.0944878801254,35.9268971699541));
#51855=CARTESIAN_POINT('Ctrl Pts',(20.8590119808882,15.0987255225029,35.8981623907312));
#51856=CARTESIAN_POINT('Ctrl Pts',(20.7854643060815,15.1029570709844,35.8694689332485));
#51857=CARTESIAN_POINT('Ctrl Pts',(20.7103678280376,15.1071886194658,35.8444218154254));
#51858=CARTESIAN_POINT('Ctrl Pts',(20.63411839813,15.1114201679473,35.8231854932707));
#51859=CARTESIAN_POINT('Ctrl Pts',(20.5579570384195,15.1156468288734,35.8019736996545));
#51860=CARTESIAN_POINT('Ctrl Pts',(20.4806458225512,15.1198734897995,35.7845640798067));
#51861=CARTESIAN_POINT('Ctrl Pts',(20.4025981897729,15.1241001507256,35.7710721053473));
#51862=CARTESIAN_POINT('Ctrl Pts',(20.3245998230925,15.1283241436516,35.7575886474425));
#51863=CARTESIAN_POINT('Ctrl Pts',(20.2458664228906,15.1325481365776,35.7480180060565));
#51864=CARTESIAN_POINT('Ctrl Pts',(20.1668229314838,15.1367721295036,35.742424857946));
#51865=CARTESIAN_POINT('Ctrl Pts',(20.0878047239234,15.1409947712901,35.7368334989302));
#51866=CARTESIAN_POINT('Ctrl Pts',(20.0084770893962,15.1452174130766,35.7352171397353));
#51867=CARTESIAN_POINT('Ctrl Pts',(19.9292699394693,15.149440054863,35.7375885837904));
#51868=CARTESIAN_POINT('Ctrl Pts',(19.8500634645198,15.1536626606655,35.7399600076369));
#51869=CARTESIAN_POINT('Ctrl Pts',(19.7709779406491,15.157885266468,35.7463191517079));
#51870=CARTESIAN_POINT('Ctrl Pts',(19.69244162901,15.1621078722705,35.7566267285526));
#51871=CARTESIAN_POINT('Ctrl Pts',(19.6138272230891,15.1663346769124,35.7669445549595));
#51872=CARTESIAN_POINT('Ctrl Pts',(19.5357635861472,15.1705614815544,35.7812185956183));
#51873=CARTESIAN_POINT('Ctrl Pts',(19.4586716053749,15.1747882861964,35.7993579135223));
#51874=CARTESIAN_POINT('Ctrl Pts',(19.3815422671796,15.1790171390739,35.8175060214219));
#51875=CARTESIAN_POINT('Ctrl Pts',(19.305385974045,15.1832459919513,35.839523007534));
#51876=CARTESIAN_POINT('Ctrl Pts',(19.2306087216496,15.1874748448287,35.8652679127693));
#51877=CARTESIAN_POINT('Ctrl Pts',(19.1556970781451,15.1917112978815,35.891059087241));
#51878=CARTESIAN_POINT('Ctrl Pts',(19.0821698635692,15.1959477509343,35.9205913927295));
#51879=CARTESIAN_POINT('Ctrl Pts',(19.0104131311567,15.2001842039871,35.9536756373016));
#51880=CARTESIAN_POINT('Ctrl Pts',(18.9451954144938,15.2040345994212,35.9837449954783));
#51881=CARTESIAN_POINT('Ctrl Pts',(18.8814401435087,15.2078849948554,36.0167477088419));
#51882=CARTESIAN_POINT('Ctrl Pts',(18.8194170627884,15.2117353902896,36.0525102273113));
#51883=CARTESIAN_POINT('Ctrl Pts',(18.751156116676,15.2159730326671,36.0918694999842));
#51884=CARTESIAN_POINT('Ctrl Pts',(18.6847374801201,15.2202106750446,36.1347199986297));
#51885=CARTESIAN_POINT('Ctrl Pts',(18.6205405383324,15.2244483174221,36.1808642480231));
#51886=CARTESIAN_POINT('Ctrl Pts',(18.5564359142663,15.2286798659035,36.2269421401751));
#51887=CARTESIAN_POINT('Ctrl Pts',(18.4945470177231,15.232911414385,36.2763041053966));
#51888=CARTESIAN_POINT('Ctrl Pts',(18.4352272814854,15.2371429628664,36.3287075960496));
#51889=CARTESIAN_POINT('Ctrl Pts',(18.3759760611813,15.2413696237925,36.3810505592237));
#51890=CARTESIAN_POINT('Ctrl Pts',(18.3192884536529,15.2455962847187,36.4364277577356));
#51891=CARTESIAN_POINT('Ctrl Pts',(18.2654863739721,15.2498229456448,36.494555226106));
#51892=CARTESIAN_POINT('Ctrl Pts',(18.2117182558406,15.2540469385708,36.5526460026069));
#51893=CARTESIAN_POINT('Ctrl Pts',(18.1608323678019,15.2582709314968,36.6134832599616));
#51894=CARTESIAN_POINT('Ctrl Pts',(18.1131142762925,15.2624949244228,36.6767457336903));
#51895=CARTESIAN_POINT('Ctrl Pts',(18.0654114484926,15.2667175662093,36.7399879714877));
#51896=CARTESIAN_POINT('Ctrl Pts',(18.0208746871121,15.2709402079958,36.8056535111753));
#51897=CARTESIAN_POINT('Ctrl Pts',(17.9797487486737,15.2751628497822,36.8733886832356));
#51898=CARTESIAN_POINT('Ctrl Pts',(17.9386231606971,15.2793854555847,36.9411232780789));
#51899=CARTESIAN_POINT('Ctrl Pts',(17.9009085799361,15.2836080613872,37.0109270687873));
#51900=CARTESIAN_POINT('Ctrl Pts',(17.8668051671834,15.2878306671897,37.0824194154051));
#51901=CARTESIAN_POINT('Ctrl Pts',(17.8326678429639,15.2920574718317,37.1539828519856));
#51902=CARTESIAN_POINT('Ctrl Pts',(17.8021490617755,15.2962842764737,37.2272377743056));
#51903=CARTESIAN_POINT('Ctrl Pts',(17.775401643363,15.3005110811156,37.3017816134991));
#51904=CARTESIAN_POINT('Ctrl Pts',(17.7486412636203,15.3047399339931,37.3763615753309));
#51905=CARTESIAN_POINT('Ctrl Pts',(17.7256560234111,15.3089687868706,37.4522312490748));
#51906=CARTESIAN_POINT('Ctrl Pts',(17.7065486745972,15.313197639748,37.5289733290746));
#51907=CARTESIAN_POINT('Ctrl Pts',(17.6874069856903,15.3174340928008,37.6058533314093));
#51908=CARTESIAN_POINT('Ctrl Pts',(17.672157204191,15.3216705458536,37.6836084117256));
#51909=CARTESIAN_POINT('Ctrl Pts',(17.6608507656111,15.3259069989063,37.7618117385863));
#51910=CARTESIAN_POINT('Ctrl Pts',(17.6505746551618,15.3297573943404,37.8328885872905));
#51911=CARTESIAN_POINT('Ctrl Pts',(17.6435553024465,15.3336077897745,37.9043353671689));
#51912=CARTESIAN_POINT('Ctrl Pts',(17.6397939534902,15.3374581852086,37.9758313287551));
#51913=CARTESIAN_POINT('Ctrl Pts',(17.6376318183635,15.3396715068963,38.0169293315632));
#51914=CARTESIAN_POINT('Ctrl Pts',(17.6365430497082,15.341884828584,38.0580842963015));
#51915=CARTESIAN_POINT('Ctrl Pts',(17.6365301165989,15.3440981502717,38.0992576011458));
#51916=CARTESIAN_POINT('',(17.636530500807,16.137848150243,38.0984614018017));
#51917=CARTESIAN_POINT('Ctrl Pts',(17.6365301165987,15.3440981503131,38.0992576019166));
#51918=CARTESIAN_POINT('Ctrl Pts',(17.6365055556943,15.3483014116799,38.1774487489868));
#51919=CARTESIAN_POINT('Ctrl Pts',(17.6403654742914,15.3525046730467,38.2557956400634));
#51920=CARTESIAN_POINT('Ctrl Pts',(17.6481300745053,15.3567079344135,38.3338766650466));
#51921=CARTESIAN_POINT('Ctrl Pts',(17.6558838071005,15.3609053127418,38.4118484049693));
#51922=CARTESIAN_POINT('Ctrl Pts',(17.6675313256336,15.3651026910701,38.4895545467128));
#51923=CARTESIAN_POINT('Ctrl Pts',(17.6830408144045,15.3693000693984,38.566573223819));
#51924=CARTESIAN_POINT('Ctrl Pts',(17.6985335795304,15.3734929217578,38.6435088528609));
#51925=CARTESIAN_POINT('Ctrl Pts',(17.7178799495353,15.3776857741171,38.7197580242518));
#51926=CARTESIAN_POINT('Ctrl Pts',(17.7409964574754,15.3818786264764,38.7949053430225));
#51927=CARTESIAN_POINT('Ctrl Pts',(17.7640997835948,15.3860690879284,38.8700098102308));
#51928=CARTESIAN_POINT('Ctrl Pts',(17.7909688421192,15.3902595493804,38.9440132164779));
#51929=CARTESIAN_POINT('Ctrl Pts',(17.8214696921664,15.3944500108324,39.0165130325044));
#51930=CARTESIAN_POINT('Ctrl Pts',(17.8519630306406,15.3986394402817,39.0889949936954));
#51931=CARTESIAN_POINT('Ctrl Pts',(17.8860861997453,15.4028288697311,39.1599736603698));
#51932=CARTESIAN_POINT('Ctrl Pts',(17.9236568444375,15.4070182991805,39.2290657825161));
#51933=CARTESIAN_POINT('Ctrl Pts',(17.9612304077784,15.4112080540827,39.2981632720344));
#51934=CARTESIAN_POINT('Ctrl Pts',(18.0022517483518,15.4153978089849,39.3653735081291));
#51935=CARTESIAN_POINT('Ctrl Pts',(18.0464929897183,15.4195875638871,39.4303386041457));
#51936=CARTESIAN_POINT('Ctrl Pts',(18.0907799873747,15.423781652023,39.4953708899986));
#51937=CARTESIAN_POINT('Ctrl Pts',(18.1382932624232,15.4279757401589,39.558153007021));
#51938=CARTESIAN_POINT('Ctrl Pts',(18.1887625663253,15.4321698282949,39.6183574677116));
#51939=CARTESIAN_POINT('Ctrl Pts',(18.2392613895006,15.4363663695345,39.6785971417255));
#51940=CARTESIAN_POINT('Ctrl Pts',(18.2927193568771,15.440562910774,39.7362558104875));
#51941=CARTESIAN_POINT('Ctrl Pts',(18.3488288009787,15.4447594520136,39.7910423153849));
#51942=CARTESIAN_POINT('Ctrl Pts',(18.405030866315,15.4489629205867,39.845919257709));
#51943=CARTESIAN_POINT('Ctrl Pts',(18.4638927850808,15.4531663891597,39.8979142602253));
#51944=CARTESIAN_POINT('Ctrl Pts',(18.5250737735749,15.4573698577328,39.9467763988917));
#51945=CARTESIAN_POINT('Ctrl Pts',(18.5532671735569,15.4593068985311,39.9692930311545));
#51946=CARTESIAN_POINT('Ctrl Pts',(18.5819526347241,15.4612439393293,39.991144991887));
#51947=CARTESIAN_POINT('Ctrl Pts',(18.6110949153144,15.4631809801276,40.0123109335656));
#51948=CARTESIAN_POINT('Ctrl Pts',(18.6748491549338,15.4674186225051,40.0586154262208));
#51949=CARTESIAN_POINT('Ctrl Pts',(18.7410412070984,15.4716562648826,40.1018151107839));
#51950=CARTESIAN_POINT('Ctrl Pts',(18.8093361667405,15.4758939072601,40.1416439643258));
#51951=CARTESIAN_POINT('Ctrl Pts',(18.8775329155506,15.4801254557416,40.1814155424132));
#51952=CARTESIAN_POINT('Ctrl Pts',(18.9478261647317,15.484357004223,40.2178256817351));
#51953=CARTESIAN_POINT('Ctrl Pts',(19.0198504197545,15.4885885527045,40.250650422836));
#51954=CARTESIAN_POINT('Ctrl Pts',(19.0917914847737,15.4928152136306,40.2834372504544));
#51955=CARTESIAN_POINT('Ctrl Pts',(19.1654591580007,15.4970418745567,40.3126467161055));
#51956=CARTESIAN_POINT('Ctrl Pts',(19.2404629602685,15.5012685354828,40.3381005174424));
#51957=CARTESIAN_POINT('Ctrl Pts',(19.315419417799,15.5054925284089,40.3635382515468));
#51958=CARTESIAN_POINT('Ctrl Pts',(19.3917098875559,15.5097165213349,40.3852248766461));
#51959=CARTESIAN_POINT('Ctrl Pts',(19.4689246353764,15.5139405142609,40.4030304813419));
#51960=CARTESIAN_POINT('Ctrl Pts',(19.5461146843157,15.5181631560474,40.4208303905128));
#51961=CARTESIAN_POINT('Ctrl Pts',(19.6242279677574,15.5223857978338,40.4347516392608));
#51962=CARTESIAN_POINT('Ctrl Pts',(19.7028417834731,15.5266084396203,40.4447147876129));
#51963=CARTESIAN_POINT('Ctrl Pts',(19.7814549292675,15.5308310454228,40.4546778510623));
#51964=CARTESIAN_POINT('Ctrl Pts',(19.8605681336227,15.5350536512253,40.4606828236603));
#51965=CARTESIAN_POINT('Ctrl Pts',(19.9397522317301,15.5392762570278,40.4627019802164));
#51966=CARTESIAN_POINT('Ctrl Pts',(20.0190150682599,15.5435030616698,40.4647231445645));
#51967=CARTESIAN_POINT('Ctrl Pts',(20.0983484696451,15.5477298663118,40.462750564019));
#51968=CARTESIAN_POINT('Ctrl Pts',(20.1773225311129,15.5519566709537,40.4568086814291));
#51969=CARTESIAN_POINT('Ctrl Pts',(20.256334862027,15.5561855238312,40.4508639195071));
#51970=CARTESIAN_POINT('Ctrl Pts',(20.3349870404514,15.5604143767087,40.4409460825169));
#51971=CARTESIAN_POINT('Ctrl Pts',(20.4128561007656,15.5646432295861,40.4271313415793));
#51972=CARTESIAN_POINT('Ctrl Pts',(20.4908651088454,15.5688796826389,40.4132917725249));
#51973=CARTESIAN_POINT('Ctrl Pts',(20.5680877286801,15.5731161356917,40.3955414109331));
#51974=CARTESIAN_POINT('Ctrl Pts',(20.6441132013823,15.5773525887445,40.3740071734067));
#51975=CARTESIAN_POINT('Ctrl Pts',(20.7132106584581,15.5812029841786,40.3544352983462));
#51976=CARTESIAN_POINT('Ctrl Pts',(20.7813191600196,15.5850533796127,40.3317384773659));
#51977=CARTESIAN_POINT('Ctrl Pts',(20.8481452737109,15.5889037750468,40.3060462451141));
#51978=CARTESIAN_POINT('Ctrl Pts',(20.9216923096317,15.5931414174243,40.277770060492));
#51979=CARTESIAN_POINT('Ctrl Pts',(20.993961810663,15.5973790598018,40.2457588165799));
#51980=CARTESIAN_POINT('Ctrl Pts',(21.0645483180642,15.6016167021793,40.2101486486517));
#51981=CARTESIAN_POINT('Ctrl Pts',(21.1350333192977,15.6058482506607,40.1745896895425));
#51982=CARTESIAN_POINT('Ctrl Pts',(21.2038397181442,15.6100797991422,40.1354422936695));
#51983=CARTESIAN_POINT('Ctrl Pts',(21.270580690617,15.6143113476237,40.092891153458));
#51984=CARTESIAN_POINT('Ctrl Pts',(21.3372445754236,15.6185380085498,40.0503891609886));
#51985=CARTESIAN_POINT('Ctrl Pts',(21.4018473814208,15.6227646694759,40.0044914876315));
#51986=CARTESIAN_POINT('Ctrl Pts',(21.4640269848645,15.626991330402,39.9554286374012));
#51987=CARTESIAN_POINT('Ctrl Pts',(21.5261673386048,15.631215323328,39.906396757171));
#51988=CARTESIAN_POINT('Ctrl Pts',(21.5858871588354,15.635439316254,39.8542039554113));
#51989=CARTESIAN_POINT('Ctrl Pts',(21.6428544342319,15.63966330918,39.7991232294405));
#51990=CARTESIAN_POINT('Ctrl Pts',(21.6998034873587,15.6438859509665,39.7440601222842));
#51991=CARTESIAN_POINT('Ctrl Pts',(21.7540014073151,15.648108592753,39.6861112509478));
#51992=CARTESIAN_POINT('Ctrl Pts',(21.8051514626409,15.6523312345394,39.6255879646305));
#51993=CARTESIAN_POINT('Ctrl Pts',(21.8563010820825,15.6565538403419,39.565065194073));
#51994=CARTESIAN_POINT('Ctrl Pts',(21.904402587041,15.6607764461444,39.5019684111127));
#51995=CARTESIAN_POINT('Ctrl Pts',(21.949199110099,15.6649990519469,39.4366425363908));
#51996=CARTESIAN_POINT('Ctrl Pts',(21.9940401775497,15.6692258565889,39.3712517034709));
#51997=CARTESIAN_POINT('Ctrl Pts',(22.0355694328128,15.6734526612309,39.3036277387348));
#51998=CARTESIAN_POINT('Ctrl Pts',(22.0735733677598,15.6776794658729,39.2341445804734));
#51999=CARTESIAN_POINT('Ctrl Pts',(22.1115957187478,15.6819083187503,39.164627751891));
#52000=CARTESIAN_POINT('Ctrl Pts',(22.1460891420403,15.6861371716278,39.0932503576331));
#52001=CARTESIAN_POINT('Ctrl Pts',(22.1768872999061,15.6903660245052,39.020408672497));
#52002=CARTESIAN_POINT('Ctrl Pts',(22.2077408088106,15.694602477558,38.9474360748902));
#52003=CARTESIAN_POINT('Ctrl Pts',(22.2348856215499,15.6988389306108,38.8729943695623));
#52004=CARTESIAN_POINT('Ctrl Pts',(22.2582046136914,15.7030753836636,38.7974972140468));
#52005=CARTESIAN_POINT('Ctrl Pts',(22.2793986030383,15.7069257790977,38.728879929903));
#52006=CARTESIAN_POINT('Ctrl Pts',(22.2974328529144,15.7107761745318,38.6593912293901));
#52007=CARTESIAN_POINT('Ctrl Pts',(22.3122563000806,15.7146265699659,38.5893477737126));
#52008=CARTESIAN_POINT('Ctrl Pts',(22.3285705901236,15.7188642123434,38.5122598171312));
#52009=CARTESIAN_POINT('Ctrl Pts',(22.3410562523573,15.7231018547209,38.43421041768));
#52010=CARTESIAN_POINT('Ctrl Pts',(22.3496067806518,15.7273394970983,38.3556138048215));
#52011=CARTESIAN_POINT('Ctrl Pts',(22.358145012951,15.7315710455798,38.2771302169765));
#52012=CARTESIAN_POINT('Ctrl Pts',(22.3627592990368,15.7358025940613,38.1981014406366));
#52013=CARTESIAN_POINT('Ctrl Pts',(22.3633940093584,15.7400341425427,38.1189525045558));
#52014=CARTESIAN_POINT('Ctrl Pts',(22.364027986572,15.7442608034688,38.0398949876819));
#52015=CARTESIAN_POINT('Ctrl Pts',(22.3606915187227,15.7484874643949,37.9607180532591));
#52016=CARTESIAN_POINT('Ctrl Pts',(22.3533808513365,15.7527141253211,37.8818509466842));
#52017=CARTESIAN_POINT('Ctrl Pts',(22.3460747986714,15.7569381182471,37.8030336234847));
#52018=CARTESIAN_POINT('Ctrl Pts',(22.3347995689948,15.7611621111731,37.7245262054935));
#52019=CARTESIAN_POINT('Ctrl Pts',(22.3196034453482,15.7653861040991,37.6467558083896));
#52020=CARTESIAN_POINT('Ctrl Pts',(22.3044121825251,15.7696087458856,37.5690102879042));
#52021=CARTESIAN_POINT('Ctrl Pts',(22.2853026061308,15.773831387672,37.4920017798888));
#52022=CARTESIAN_POINT('Ctrl Pts',(22.2623743754399,15.7780540294585,37.4161486811793));
#52023=CARTESIAN_POINT('Ctrl Pts',(22.239446340136,15.782276635261,37.3402962288652));
#52024=CARTESIAN_POINT('Ctrl Pts',(22.2126998522416,15.7864992410634,37.2655996145877));
#52025=CARTESIAN_POINT('Ctrl Pts',(22.1822844324412,15.7907218468659,37.192462068658));
#52026=CARTESIAN_POINT('Ctrl Pts',(22.1518387684096,15.7949486515079,37.1192517968258));
#52027=CARTESIAN_POINT('Ctrl Pts',(22.1177170654331,15.7991754561499,37.0476041239026));
#52028=CARTESIAN_POINT('Ctrl Pts',(22.0801167881635,15.8034022607919,36.9779017028351));
#52029=CARTESIAN_POINT('Ctrl Pts',(22.0424982904583,15.8076311136693,36.9081655051956));
#52030=CARTESIAN_POINT('Ctrl Pts',(22.0013981037828,15.8118599665468,36.8403768386156));
#52031=CARTESIAN_POINT('Ctrl Pts',(21.9570581066831,15.8160888194242,36.7748909448781));
#52032=CARTESIAN_POINT('Ctrl Pts',(21.912638420892,15.820325272477,36.7092873586391));
#52033=CARTESIAN_POINT('Ctrl Pts',(21.8649675731551,15.8245617255298,36.6459951898754));
#52034=CARTESIAN_POINT('Ctrl Pts',(21.8143288123796,15.8287981785825,36.5853378589701));
#52035=CARTESIAN_POINT('Ctrl Pts',(21.7683046381822,15.8326485740167,36.5302080824672));
#52036=CARTESIAN_POINT('Ctrl Pts',(21.7198295025753,15.8364989694508,36.4772545661008));
#52037=CARTESIAN_POINT('Ctrl Pts',(21.6691412468445,15.840349364885,36.4266925151119));
#52038=CARTESIAN_POINT('Ctrl Pts',(21.6133551063818,15.8445870072624,36.3710452722176));
#52039=CARTESIAN_POINT('Ctrl Pts',(21.5546783845076,15.8488246496399,36.3180863935836));
#52040=CARTESIAN_POINT('Ctrl Pts',(21.4934005898209,15.8530622920174,36.2681307035647));
#52041=CARTESIAN_POINT('Ctrl Pts',(21.4322109150079,15.8572938404988,36.2182468517885));
#52042=CARTESIAN_POINT('Ctrl Pts',(21.3684279558925,15.8615253889803,36.1713579058385));
#52043=CARTESIAN_POINT('Ctrl Pts',(21.3023779741795,15.8657569374617,36.1277418897943));
#52044=CARTESIAN_POINT('Ctrl Pts',(21.2364042820192,15.8699835983878,36.084176251453));
#52045=CARTESIAN_POINT('Ctrl Pts',(21.1681691600272,15.8742102593139,36.0438762875696));
#52046=CARTESIAN_POINT('Ctrl Pts',(21.0980306445605,15.87843692024,36.0070788011714));
#52047=CARTESIAN_POINT('Ctrl Pts',(21.0279364027105,15.882660913166,35.9703045424933));
#52048=CARTESIAN_POINT('Ctrl Pts',(20.9559415662199,15.886884906092,35.9370285901768));
#52049=CARTESIAN_POINT('Ctrl Pts',(20.8824307107632,15.891108899018,35.907442935383));
#52050=CARTESIAN_POINT('Ctrl Pts',(20.8089433694144,15.8953315408045,35.8778667442293));
#52051=CARTESIAN_POINT('Ctrl Pts',(20.7339414066413,15.8995541825909,35.8519786814036));
#52052=CARTESIAN_POINT('Ctrl Pts',(20.6578300500723,15.9037768243773,35.8299228942342));
#52053=CARTESIAN_POINT('Ctrl Pts',(20.5817193420994,15.9079994301798,35.8078672950171));
#52054=CARTESIAN_POINT('Ctrl Pts',(20.5044997097749,15.9122220359823,35.789644035625));
#52055=CARTESIAN_POINT('Ctrl Pts',(20.4265907993584,15.9164446417848,35.7753471805874));
#52056=CARTESIAN_POINT('Ctrl Pts',(20.34860441853,15.9206714464267,35.7610361091626));
#52057=CARTESIAN_POINT('Ctrl Pts',(20.269927852669,15.9248982510687,35.7506593257667));
#52058=CARTESIAN_POINT('Ctrl Pts',(20.1909895839562,15.9291250557107,35.7442594752986));
#52059=CARTESIAN_POINT('Ctrl Pts',(20.1120130631414,15.9333539085881,35.7378565235752));
#52060=CARTESIAN_POINT('Ctrl Pts',(20.0327750559952,15.9375827614656,35.7354343582328));
#52061=CARTESIAN_POINT('Ctrl Pts',(19.9537052264222,15.941811614343,35.7369834459235));
#52062=CARTESIAN_POINT('Ctrl Pts',(19.8744932910383,15.9460480673958,35.7385353176643));
#52063=CARTESIAN_POINT('Ctrl Pts',(19.7954506058933,15.9502845204486,35.7440726704425));
#52064=CARTESIAN_POINT('Ctrl Pts',(19.7170026603079,15.9545209735013,35.7535339451364));
#52065=CARTESIAN_POINT('Ctrl Pts',(19.6457034843836,15.9583713689355,35.7621330369779));
#52066=CARTESIAN_POINT('Ctrl Pts',(19.574895757171,15.9622217643697,35.7739727766214));
#52067=CARTESIAN_POINT('Ctrl Pts',(19.5048894728339,15.9660721598039,35.7889707905807));
#52068=CARTESIAN_POINT('Ctrl Pts',(19.4278424260391,15.9703098021814,35.8054772041732));
#52069=CARTESIAN_POINT('Ctrl Pts',(19.35147711472,15.9745474445589,35.8258718050086));
#52070=CARTESIAN_POINT('Ctrl Pts',(19.2762152246405,15.9787850869364,35.8500831037886));
#52071=CARTESIAN_POINT('Ctrl Pts',(19.2010615641123,15.9830166354179,35.8742595857708));
#52072=CARTESIAN_POINT('Ctrl Pts',(19.1270086162236,15.9872481838993,35.9022417235528));
#52073=CARTESIAN_POINT('Ctrl Pts',(19.0544672022013,15.9914797323808,35.9339071651504));
#52074=CARTESIAN_POINT('Ctrl Pts',(18.9820095755155,15.9957063933069,35.9655360322884));
#52075=CARTESIAN_POINT('Ctrl Pts',(18.9110604406773,15.999933054233,36.0008395622537));
#52076=CARTESIAN_POINT('Ctrl Pts',(18.8420133359816,16.0041597151591,36.0396463102527));
#52077=CARTESIAN_POINT('Ctrl Pts',(18.7730098159699,16.0083837080851,36.078428562223));
#52078=CARTESIAN_POINT('Ctrl Pts',(18.7059063505851,16.0126077010112,36.120709413885));
#52079=CARTESIAN_POINT('Ctrl Pts',(18.6410733331933,16.0168316939372,36.1662707647807));
#52080=CARTESIAN_POINT('Ctrl Pts',(18.5762610541068,16.0210543357236,36.2118175418492));
#52081=CARTESIAN_POINT('Ctrl Pts',(18.5137181640778,16.0252769775101,36.2606424650291));
#52082=CARTESIAN_POINT('Ctrl Pts',(18.453786163424,16.0294996192965,36.3124840665099));
#52083=CARTESIAN_POINT('Ctrl Pts',(18.3938546734911,16.033722225099,36.3643252262135));
#52084=CARTESIAN_POINT('Ctrl Pts',(18.3365343822978,16.0379448309015,36.4191827053458));
#52085=CARTESIAN_POINT('Ctrl Pts',(18.2821326258983,16.042167436704,36.4767556789267));
#52086=CARTESIAN_POINT('Ctrl Pts',(18.2276767739346,16.046394241346,36.5343859014403));
#52087=CARTESIAN_POINT('Ctrl Pts',(18.1761455764438,16.050621045988,36.5947366705696));
#52088=CARTESIAN_POINT('Ctrl Pts',(18.1278080449245,16.05484785063,36.657471759635));
#52089=CARTESIAN_POINT('Ctrl Pts',(18.0794470898843,16.0590767035074,36.7202372490254));
#52090=CARTESIAN_POINT('Ctrl Pts',(18.0342831512126,16.0633055563849,36.7853889742914));
#52091=CARTESIAN_POINT('Ctrl Pts',(17.9925421130222,16.0675344092623,36.8525613149695));
#52092=CARTESIAN_POINT('Ctrl Pts',(17.9507260570391,16.0717708623151,36.9198543790639));
#52093=CARTESIAN_POINT('Ctrl Pts',(17.9123454208389,16.0760073153679,36.9891749035545));
#52094=CARTESIAN_POINT('Ctrl Pts',(17.8775801734251,16.0802437684207,37.0601324504237));
#52095=CARTESIAN_POINT('Ctrl Pts',(17.8459829980898,16.0840941638548,37.1246238093691));
#52096=CARTESIAN_POINT('Ctrl Pts',(17.8173718101545,16.0879445592889,37.1904669076602));
#52097=CARTESIAN_POINT('Ctrl Pts',(17.7918462500092,16.0917949547231,37.2573568624254));
#52098=CARTESIAN_POINT('Ctrl Pts',(17.759851353345,16.0966212152764,37.3411997704125));
#52099=CARTESIAN_POINT('Ctrl Pts',(17.7326042815355,16.1014474758297,37.4269487816098));
#52100=CARTESIAN_POINT('Ctrl Pts',(17.7103056779464,16.1062737363831,37.5140901498903));
#52101=CARTESIAN_POINT('Ctrl Pts',(17.6880976991037,16.1110803823163,37.6008773630611));
#52102=CARTESIAN_POINT('Ctrl Pts',(17.6707981761703,16.1158870282495,37.6890454480439));
#52103=CARTESIAN_POINT('Ctrl Pts',(17.6585584633483,16.1206936741827,37.7780652685057));
#52104=CARTESIAN_POINT('Ctrl Pts',(17.6464027197852,16.1254673446285,37.8664743778784));
#52105=CARTESIAN_POINT('Ctrl Pts',(17.6392377111805,16.1302410150742,37.9557233688363));
#52106=CARTESIAN_POINT('Ctrl Pts',(17.6371636382762,16.13501468552,38.0452755208704));
#52107=CARTESIAN_POINT('Ctrl Pts',(17.6367532753299,16.135959173761,38.0629937432554));
#52108=CARTESIAN_POINT('Ctrl Pts',(17.6365420478448,16.136903662002,38.0807237808861));
#52109=CARTESIAN_POINT('Ctrl Pts',(17.636530500807,16.137848150243,38.0984614018017));
#52110=CARTESIAN_POINT('',(17.6365307541938,16.9315981503216,38.1018881282061));
#52111=CARTESIAN_POINT('Ctrl Pts',(17.6365305008067,16.1378481502717,38.0984614023413));
#52112=CARTESIAN_POINT('Ctrl Pts',(17.6364785885184,16.1420943096752,38.1782048682515));
#52113=CARTESIAN_POINT('Ctrl Pts',(17.6404668253251,16.1463404690787,38.2579711622715));
#52114=CARTESIAN_POINT('Ctrl Pts',(17.648475589581,16.1505866284822,38.3373254897886));
#52115=CARTESIAN_POINT('Ctrl Pts',(17.6564848530562,16.1548330525664,38.4166847637895));
#52116=CARTESIAN_POINT('Ctrl Pts',(17.6685150947909,16.1590794766506,38.495631561438));
#52117=CARTESIAN_POINT('Ctrl Pts',(17.6844948615814,16.1633259007348,38.5737366302674));
#52118=CARTESIAN_POINT('Ctrl Pts',(17.7004803878264,16.1675738553223,38.6518698498574));
#52119=CARTESIAN_POINT('Ctrl Pts',(17.7204181734841,16.1718218099098,38.7291602865282));
#52120=CARTESIAN_POINT('Ctrl Pts',(17.7441860494605,16.1760697644973,38.8051906561003));
#52121=CARTESIAN_POINT('Ctrl Pts',(17.767985373847,16.1803233397561,38.8813216250804));
#52122=CARTESIAN_POINT('Ctrl Pts',(17.7956247620737,16.184576915015,38.956188759763));
#52123=CARTESIAN_POINT('Ctrl Pts',(17.8269329028224,16.1888304902738,39.0293921842065));
#52124=CARTESIAN_POINT('Ctrl Pts',(17.8582656665114,16.1930874108456,39.1026531810099));
#52125=CARTESIAN_POINT('Ctrl Pts',(17.8932727228514,16.1973443314174,39.1742474499582));
#52126=CARTESIAN_POINT('Ctrl Pts',(17.9317366813445,16.2016012519892,39.243799495368));
#52127=CARTESIAN_POINT('Ctrl Pts',(17.9702674063473,16.205865561809,39.3134722706117));
#52128=CARTESIAN_POINT('Ctrl Pts',(18.0122667634631,16.2101298716289,39.3810953587803));
#52129=CARTESIAN_POINT('Ctrl Pts',(18.0574742721319,16.2143941814487,39.4463224864312));
#52130=CARTESIAN_POINT('Ctrl Pts',(18.0685123018993,16.2154353708465,39.4622485791945));
#52131=CARTESIAN_POINT('Ctrl Pts',(18.0797414043603,16.2164765602444,39.4780319944199));
#52132=CARTESIAN_POINT('Ctrl Pts',(18.0911574403174,16.2175177496422,39.4936680104115));
#52133=CARTESIAN_POINT('Ctrl Pts',(18.1376207234194,16.2217553920197,39.5573066184481));
#52134=CARTESIAN_POINT('Ctrl Pts',(18.1873571594556,16.2259930343972,39.6187385925859));
#52135=CARTESIAN_POINT('Ctrl Pts',(18.2401296669689,16.2302306767746,39.6776079525082));
#52136=CARTESIAN_POINT('Ctrl Pts',(18.2928262855455,16.2344622252561,39.7363926559807));
#52137=CARTESIAN_POINT('Ctrl Pts',(18.3485499948283,16.2386937737375,39.792621717413));
#52138=CARTESIAN_POINT('Ctrl Pts',(18.4070216891549,16.242925322219,39.8459697998755));
#52139=CARTESIAN_POINT('Ctrl Pts',(18.46542584706,16.247151983145,39.8992562638295));
#52140=CARTESIAN_POINT('Ctrl Pts',(18.5265713379303,16.2513786440711,39.9496680472584));
#52141=CARTESIAN_POINT('Ctrl Pts',(18.590141263079,16.2556053049972,39.9969155971807));
#52142=CARTESIAN_POINT('Ctrl Pts',(18.6536710609099,16.2598292979232,40.0441333229772));
#52143=CARTESIAN_POINT('Ctrl Pts',(18.7196218801348,16.2640532908492,40.0881905009103));
#52144=CARTESIAN_POINT('Ctrl Pts',(18.7876436429308,16.2682772837752,40.1288377225332));
#52145=CARTESIAN_POINT('Ctrl Pts',(18.8556436474293,16.2724999255617,40.1694719422241));
#52146=CARTESIAN_POINT('Ctrl Pts',(18.9257128779157,16.2767225673481,40.206698131335));
#52147=CARTESIAN_POINT('Ctrl Pts',(18.9974734222548,16.2809452091346,40.2403109357788));
#52148=CARTESIAN_POINT('Ctrl Pts',(19.069233355074,16.285167814937,40.2739234537854));
#52149=CARTESIAN_POINT('Ctrl Pts',(19.1426841479714,16.2893904207395,40.3039224508015));
#52150=CARTESIAN_POINT('Ctrl Pts',(19.2174258642835,16.293613026542,40.3301498073016));
#52151=CARTESIAN_POINT('Ctrl Pts',(19.2922419016392,16.297839831184,40.3564032435415));
#52152=CARTESIAN_POINT('Ctrl Pts',(19.3683509831628,16.3020666358259,40.3788773922223));
#52153=CARTESIAN_POINT('Ctrl Pts',(19.4453364548924,16.3062934404679,40.3974635563222));
#52154=CARTESIAN_POINT('Ctrl Pts',(19.5223592324327,16.3105222933453,40.4160587269516));
#52155=CARTESIAN_POINT('Ctrl Pts',(19.6002587849685,16.3147511462228,40.4307620726978));
#52156=CARTESIAN_POINT('Ctrl Pts',(19.6786091846356,16.3189799991002,40.4415162576201));
#52157=CARTESIAN_POINT('Ctrl Pts',(19.7571003971406,16.323216452153,40.4522897701695));
#52158=CARTESIAN_POINT('Ctrl Pts',(19.83604360763,16.3274529052057,40.4590999000014));
#52159=CARTESIAN_POINT('Ctrl Pts',(19.9150089292952,16.3316893582585,40.4619413538021));
#52160=CARTESIAN_POINT('Ctrl Pts',(19.9867783340819,16.3355397536927,40.4645238728587));
#52161=CARTESIAN_POINT('Ctrl Pts',(20.0585657317189,16.339390149127,40.4638287408858));
#52162=CARTESIAN_POINT('Ctrl Pts',(20.1300520943976,16.3432405445612,40.4598891697796));
#52163=CARTESIAN_POINT('Ctrl Pts',(20.208728075884,16.3474781869387,40.4555533830392));
#52164=CARTESIAN_POINT('Ctrl Pts',(20.2873346771541,16.3517158293162,40.4472707051577));
#52165=CARTESIAN_POINT('Ctrl Pts',(20.3654442259973,16.3559534716937,40.4350462433505));
#52166=CARTESIAN_POINT('Ctrl Pts',(20.443441450244,16.3601850201752,40.4228393607991));
#52167=CARTESIAN_POINT('Ctrl Pts',(20.5209425822431,16.3644165686567,40.4067020232024));
#52168=CARTESIAN_POINT('Ctrl Pts',(20.5975227802602,16.3686481171381,40.3866912708038));
#52169=CARTESIAN_POINT('Ctrl Pts',(20.6740145260339,16.3728747780642,40.3667036313768));
#52170=CARTESIAN_POINT('Ctrl Pts',(20.7495870004239,16.3771014389903,40.3428515858283));
#52171=CARTESIAN_POINT('Ctrl Pts',(20.8238248076045,16.3813280999164,40.3152433562197));
#52172=CARTESIAN_POINT('Ctrl Pts',(20.8980157535678,16.3855520928424,40.2876525537859));
#52173=CARTESIAN_POINT('Ctrl Pts',(20.9708732663339,16.3897760857684,40.2563104364766));
#52174=CARTESIAN_POINT('Ctrl Pts',(21.0419975654431,16.3940000786945,40.2213749113513));
#52175=CARTESIAN_POINT('Ctrl Pts',(21.1130991138386,16.3982227204809,40.1864505611429));
#52176=CARTESIAN_POINT('Ctrl Pts',(21.1824681290684,16.4024453622674,40.1479352921867));
#52177=CARTESIAN_POINT('Ctrl Pts',(21.249726635242,16.4066680040538,40.1060343411982));
#52178=CARTESIAN_POINT('Ctrl Pts',(21.3169845682606,16.4108906098563,40.064133747276));
#52179=CARTESIAN_POINT('Ctrl Pts',(21.3821316308602,16.4151132156588,40.0188477777724));
#52180=CARTESIAN_POINT('Ctrl Pts',(21.4448174819599,16.4193358214613,39.9704258565159));
#52181=CARTESIAN_POINT('Ctrl Pts',(21.5075656660929,16.4235626261033,39.9219557858735));
#52182=CARTESIAN_POINT('Ctrl Pts',(21.5678473782707,16.4277894307452,39.8703438218898));
#52183=CARTESIAN_POINT('Ctrl Pts',(21.6253446365292,16.4320162353872,39.8158803144176));
#52184=CARTESIAN_POINT('Ctrl Pts',(21.6828697569516,16.4362450882647,39.761390414884));
#52185=CARTESIAN_POINT('Ctrl Pts',(21.7376074114044,16.4404739411421,39.7040465586615));
#52186=CARTESIAN_POINT('Ctrl Pts',(21.7892776549551,16.4447027940196,39.6441748328406));
#52187=CARTESIAN_POINT('Ctrl Pts',(21.8410407612566,16.4489392470723,39.5841955044081));
#52188=CARTESIAN_POINT('Ctrl Pts',(21.8897251528208,16.4531757001251,39.5216795994815));
#52189=CARTESIAN_POINT('Ctrl Pts',(21.9350923865942,16.4574121531779,39.4569848548327));
#52190=CARTESIAN_POINT('Ctrl Pts',(21.976325415169,16.461262548612,39.3981855842386));
#52191=CARTESIAN_POINT('Ctrl Pts',(22.0148187226789,16.4651129440462,39.3375870781129));
#52192=CARTESIAN_POINT('Ctrl Pts',(22.0504265113351,16.4689633394803,39.2754750369591));
#52193=CARTESIAN_POINT('Ctrl Pts',(22.0896154925085,16.4732009818578,39.2071161833692));
#52194=CARTESIAN_POINT('Ctrl Pts',(22.1254557885139,16.4774386242354,39.13666709751));
#52195=CARTESIAN_POINT('Ctrl Pts',(22.1577188864489,16.4816762666129,39.064489319776));
#52196=CARTESIAN_POINT('Ctrl Pts',(22.1899355887829,16.4859078150943,38.9924153365189));
#52197=CARTESIAN_POINT('Ctrl Pts',(22.2185851191369,16.4901393635758,38.9186180226358));
#52198=CARTESIAN_POINT('Ctrl Pts',(22.2434840702714,16.4943709120572,38.8434848131188));
#52199=CARTESIAN_POINT('Ctrl Pts',(22.2683542624298,16.4985975729833,38.7684383845336));
#52200=CARTESIAN_POINT('Ctrl Pts',(22.28948233747,16.5028242339094,38.6920595693594));
#52201=CARTESIAN_POINT('Ctrl Pts',(22.3067329646642,16.5070508948356,38.614755738804));
#52202=CARTESIAN_POINT('Ctrl Pts',(22.3239727027249,16.5112748877616,38.5375007048354));
#52203=CARTESIAN_POINT('Ctrl Pts',(22.3373397492575,16.5154988806876,38.4593222707827));
#52204=CARTESIAN_POINT('Ctrl Pts',(22.3467489526675,16.5197228736136,38.3806417539391));
#52205=CARTESIAN_POINT('Ctrl Pts',(22.3561551463312,16.5239455154001,38.3019864048362));
#52206=CARTESIAN_POINT('Ctrl Pts',(22.3616059552865,16.5281681571865,38.2228297569886));
#52207=CARTESIAN_POINT('Ctrl Pts',(22.3630678002548,16.532390798973,38.1436005997561));
#52208=CARTESIAN_POINT('Ctrl Pts',(22.3645296327657,16.5366134047755,38.0643721176886));
#52209=CARTESIAN_POINT('Ctrl Pts',(22.3620025616588,16.540836010578,37.9850715961843));
#52210=CARTESIAN_POINT('Ctrl Pts',(22.3555051174012,16.5450586163805,37.9061286952722));
#52211=CARTESIAN_POINT('Ctrl Pts',(22.3490012122692,16.5492854210225,37.8271072957774));
#52212=CARTESIAN_POINT('Ctrl Pts',(22.3385190863278,16.5535122256644,37.7484446954828));
#52213=CARTESIAN_POINT('Ctrl Pts',(22.3241292157766,16.5577390303064,37.6705656868929));
#52214=CARTESIAN_POINT('Ctrl Pts',(22.3097323721462,16.5619678831839,37.5926489395));
#52215=CARTESIAN_POINT('Ctrl Pts',(22.2914241199844,16.5661967360613,37.5155169969323));
#52216=CARTESIAN_POINT('Ctrl Pts',(22.2693256192087,16.5704255889388,37.4395821967096));
#52217=CARTESIAN_POINT('Ctrl Pts',(22.2471874025845,16.5746620419916,37.3635109250106));
#52218=CARTESIAN_POINT('Ctrl Pts',(22.2212454803348,16.5788984950444,37.2886415386048));
#52219=CARTESIAN_POINT('Ctrl Pts',(22.1916701532164,16.5831349480972,37.2153687884771));
#52220=CARTESIAN_POINT('Ctrl Pts',(22.1647899534174,16.5869853435312,37.1487732050921));
#52221=CARTESIAN_POINT('Ctrl Pts',(22.1349091057282,16.5908357389653,37.0834964970803));
#52222=CARTESIAN_POINT('Ctrl Pts',(22.1021879121243,16.5946861343994,37.0198164864161));
#52223=CARTESIAN_POINT('Ctrl Pts',(22.066175840369,16.5989237767769,36.9497319674593));
#52224=CARTESIAN_POINT('Ctrl Pts',(22.0265875321937,16.6031614191544,36.8813187642604));
#52225=CARTESIAN_POINT('Ctrl Pts',(21.983601884425,16.6073990615319,36.8149653681688));
#52226=CARTESIAN_POINT('Ctrl Pts',(21.9406780517048,16.6116306100133,36.748707390865));
#52227=CARTESIAN_POINT('Ctrl Pts',(21.8943668343264,16.6158621584948,36.6845037284246));
#52228=CARTESIAN_POINT('Ctrl Pts',(21.8448934038699,16.6200937069762,36.6227191298683));
#52229=CARTESIAN_POINT('Ctrl Pts',(21.7954771165918,16.6243203679023,36.5610058942294));
#52230=CARTESIAN_POINT('Ctrl Pts',(21.7429061660821,16.6285470288284,36.50170653399));
#52231=CARTESIAN_POINT('Ctrl Pts',(21.6874486175196,16.6327736897545,36.4451563203338));
#52232=CARTESIAN_POINT('Ctrl Pts',(21.6320260754899,16.6369976826806,36.3886418029347));
#52233=CARTESIAN_POINT('Ctrl Pts',(21.5737208794609,16.6412216756066,36.3348733214615));
#52234=CARTESIAN_POINT('Ctrl Pts',(21.5128401078154,16.6454456685326,36.2841516447993));
#52235=CARTESIAN_POINT('Ctrl Pts',(21.4519788102601,16.649668310319,36.2334461926113));
#52236=CARTESIAN_POINT('Ctrl Pts',(21.3885439330015,16.6538909521055,36.1857859097344));
#52237=CARTESIAN_POINT('Ctrl Pts',(21.3228768951412,16.658113593892,36.141432370021));
#52238=CARTESIAN_POINT('Ctrl Pts',(21.2572104168741,16.6623361996944,36.0970792082741));
#52239=CARTESIAN_POINT('Ctrl Pts',(21.1893122050906,16.6665588054969,36.0560329948581));
#52240=CARTESIAN_POINT('Ctrl Pts',(21.1195527744545,16.6707814112994,36.0185120643849));
#52241=CARTESIAN_POINT('Ctrl Pts',(21.049723977018,16.6750082159414,35.980953824162));
#52242=CARTESIAN_POINT('Ctrl Pts',(20.9780306776654,16.6792350205834,35.9469280915867));
#52243=CARTESIAN_POINT('Ctrl Pts',(20.9048675837599,16.6834618252254,35.9166069761125));
#52244=CARTESIAN_POINT('Ctrl Pts',(20.8316690363011,16.6876906781028,35.8862711675571));
#52245=CARTESIAN_POINT('Ctrl Pts',(20.756999717534,16.6919195309803,35.8596437099928));
#52246=CARTESIAN_POINT('Ctrl Pts',(20.6812714756874,16.6961483838577,35.8368474162543));
#52247=CARTESIAN_POINT('Ctrl Pts',(20.6054071335952,16.7003848369105,35.8140101525805));
#52248=CARTESIAN_POINT('Ctrl Pts',(20.5284805219995,16.7046212899633,35.7950179231385));
#52249=CARTESIAN_POINT('Ctrl Pts',(20.4509154854594,16.7088577430161,35.7799427451304));
#52250=CARTESIAN_POINT('Ctrl Pts',(20.380418761237,16.7127081384502,35.7662413312712));
#52251=CARTESIAN_POINT('Ctrl Pts',(20.3093950395558,16.7165585338844,35.7557749743961));
#52252=CARTESIAN_POINT('Ctrl Pts',(20.2381646343263,16.7204089293185,35.7485604307454));
#52253=CARTESIAN_POINT('Ctrl Pts',(20.1597703527705,16.724646571696,35.7406202966913));
#52254=CARTESIAN_POINT('Ctrl Pts',(20.0808314112834,16.7288842140735,35.7365899080065));
#52255=CARTESIAN_POINT('Ctrl Pts',(20.0017710825654,16.7331218564509,35.7365306635866));
#52256=CARTESIAN_POINT('Ctrl Pts',(19.9228244457023,16.7373534049324,35.7364715043625));
#52257=CARTESIAN_POINT('Ctrl Pts',(19.8437572331678,16.7415849534138,35.7403721489073));
#52258=CARTESIAN_POINT('Ctrl Pts',(19.7649979899845,16.7458165018953,35.7482422539325));
#52259=CARTESIAN_POINT('Ctrl Pts',(19.6863297159023,16.7500431628214,35.756103268769));
#52260=CARTESIAN_POINT('Ctrl Pts',(19.6079691683695,16.7542698237475,35.7679245864878));
#52261=CARTESIAN_POINT('Ctrl Pts',(19.5303435129165,16.7584964846736,35.7836638359166));
#52262=CARTESIAN_POINT('Ctrl Pts',(19.4527668571963,16.7627204775996,35.7993931502408));
#52263=CARTESIAN_POINT('Ctrl Pts',(19.3759246310148,16.7669444705256,35.8190353944952));
#52264=CARTESIAN_POINT('Ctrl Pts',(19.3002362933157,16.7711684634516,35.8424966897682));
#52265=CARTESIAN_POINT('Ctrl Pts',(19.2245721662411,16.7753911052381,35.865950480416));
#52266=CARTESIAN_POINT('Ctrl Pts',(19.1500616421277,16.7796137470245,35.8932207575148));
#52267=CARTESIAN_POINT('Ctrl Pts',(19.0771099933496,16.783836388811,35.9241634995881));
#52268=CARTESIAN_POINT('Ctrl Pts',(19.0041589662422,16.7880589946134,35.9551059779772));
#52269=CARTESIAN_POINT('Ctrl Pts',(18.9327672190563,16.7922816004159,35.9897206747529));
#52270=CARTESIAN_POINT('Ctrl Pts',(18.8633195899172,16.7965042062183,36.0278156244595));
#52271=CARTESIAN_POINT('Ctrl Pts',(18.7938029040242,16.8007310108603,36.0659484547044));
#52272=CARTESIAN_POINT('Ctrl Pts',(18.7262346096606,16.8049578155023,36.1075682245992));
#52273=CARTESIAN_POINT('Ctrl Pts',(18.6609739371107,16.8091846201442,36.1524375122212));
#52274=CARTESIAN_POINT('Ctrl Pts',(18.5956816403823,16.8134134730217,36.1973285427139));
#52275=CARTESIAN_POINT('Ctrl Pts',(18.5326995660242,16.8176423258991,36.2454719427909));
#52276=CARTESIAN_POINT('Ctrl Pts',(18.4723549213669,16.8218711787766,36.2965890777119));
#52277=CARTESIAN_POINT('Ctrl Pts',(18.4119018241592,16.8261076318293,36.3477980813261));
#52278=CARTESIAN_POINT('Ctrl Pts',(18.3540959705091,16.8303440848821,36.4019911771457));
#52279=CARTESIAN_POINT('Ctrl Pts',(18.2992284869659,16.8345805379349,36.4588520172295));
#52280=CARTESIAN_POINT('Ctrl Pts',(18.2493609431761,16.8384309333691,36.5105312678474));
#52281=CARTESIAN_POINT('Ctrl Pts',(18.2019203203939,16.8422813288033,36.5644135560128));
#52282=CARTESIAN_POINT('Ctrl Pts',(18.1570950331286,16.8461317242375,36.6202393017853));
#52283=CARTESIAN_POINT('Ctrl Pts',(18.1079067904915,16.8503568881221,36.6814987045908));
#52284=CARTESIAN_POINT('Ctrl Pts',(18.0616790360622,16.8545820520066,36.7453345810201));
#52285=CARTESIAN_POINT('Ctrl Pts',(18.0186939304945,16.8588072158912,36.8114284265744));
#52286=CARTESIAN_POINT('Ctrl Pts',(17.975768405893,16.8630265233437,36.8774306605082));
#52287=CARTESIAN_POINT('Ctrl Pts',(17.936076864836,16.8672458307963,36.9456842612171));
#52288=CARTESIAN_POINT('Ctrl Pts',(17.8998612449744,16.8714651382489,37.0158378117001));
#52289=CARTESIAN_POINT('Ctrl Pts',(17.8636843923002,16.8756799291231,37.0859162659717));
#52290=CARTESIAN_POINT('Ctrl Pts',(17.8309762887945,16.8798947199974,37.1578902158748));
#52291=CARTESIAN_POINT('Ctrl Pts',(17.8019347238809,16.8841095108716,37.2313807031736));
#52292=CARTESIAN_POINT('Ctrl Pts',(17.7729126268906,16.8883214763738,37.3048219263509));
#52293=CARTESIAN_POINT('Ctrl Pts',(17.7475523634037,16.892533441876,37.379777232228));
#52294=CARTESIAN_POINT('Ctrl Pts',(17.7260044227758,16.8967454073782,37.4558458603218));
#52295=CARTESIAN_POINT('Ctrl Pts',(17.7044654610623,16.9009556177764,37.531882791015));
#52296=CARTESIAN_POINT('Ctrl Pts',(17.6867357926461,16.9051658281745,37.6090316686098));
#52297=CARTESIAN_POINT('Ctrl Pts',(17.6729161652158,16.9093760385726,37.6868762088842));
#52298=CARTESIAN_POINT('Ctrl Pts',(17.6590929138932,16.9135873530055,37.7647411621709));
#52299=CARTESIAN_POINT('Ctrl Pts',(17.6491818400631,16.9177986674384,37.8433016790901));
#52300=CARTESIAN_POINT('Ctrl Pts',(17.6432324255559,16.9220099818713,37.9221319563585));
#52301=CARTESIAN_POINT('Ctrl Pts',(17.6387172882919,16.9252060380047,37.9819579311661));
#52302=CARTESIAN_POINT('Ctrl Pts',(17.6364828620914,16.9284020941382,38.0419390384473));
#52303=CARTESIAN_POINT('Ctrl Pts',(17.636530754193,16.9315981502717,38.1018881272695));
#52304=CARTESIAN_POINT('',(17.6365300019755,17.7253481502437,38.1000966336477));
#52305=CARTESIAN_POINT('Ctrl Pts',(17.6365307541938,16.9315981503216,38.1018881282061));
#52306=CARTESIAN_POINT('Ctrl Pts',(17.6366053049449,16.9365732560039,38.1952072189802));
#52307=CARTESIAN_POINT('Ctrl Pts',(17.6422106724848,16.9415483616861,38.2882936701097));
#52308=CARTESIAN_POINT('Ctrl Pts',(17.6532411624811,16.9465234673684,38.3805590836651));
#52309=CARTESIAN_POINT('Ctrl Pts',(17.6643975571371,16.9515553601007,38.4738776367906));
#52310=CARTESIAN_POINT('Ctrl Pts',(17.6811035375494,16.956587252833,38.5663562147621));
#52311=CARTESIAN_POINT('Ctrl Pts',(17.7032004638078,16.9616191455653,38.6574067917125));
#52312=CARTESIAN_POINT('Ctrl Pts',(17.7181829172308,16.9650309367624,38.7191421214297));
#52313=CARTESIAN_POINT('Ctrl Pts',(17.7356427284869,16.9684427279595,38.7802213906737));
#52314=CARTESIAN_POINT('Ctrl Pts',(17.7555180592357,16.9718545191566,38.8404669192362));
#52315=CARTESIAN_POINT('Ctrl Pts',(17.7802043717861,16.9760921615341,38.9152953568933));
#52316=CARTESIAN_POINT('Ctrl Pts',(17.8086831558674,16.9803298039116,38.9890283845905));
#52317=CARTESIAN_POINT('Ctrl Pts',(17.8408380437667,16.9845674462891,39.0612544344007));
#52318=CARTESIAN_POINT('Ctrl Pts',(17.8729466916755,16.9887989947706,39.1333766203169));
#52319=CARTESIAN_POINT('Ctrl Pts',(17.908720756057,16.9930305432521,39.2039957072802));
#52320=CARTESIAN_POINT('Ctrl Pts',(17.947994467672,16.9972620917336,39.2727163920553));
#52321=CARTESIAN_POINT('Ctrl Pts',(17.9872228170654,17.0014887526597,39.3413577025416));
#52322=CARTESIAN_POINT('Ctrl Pts',(18.0299425494248,17.0057154135858,39.4081045633627));
#52323=CARTESIAN_POINT('Ctrl Pts',(18.0759409430028,17.0099420745119,39.4725841271438));
#52324=CARTESIAN_POINT('Ctrl Pts',(18.1219103009614,17.014166067438,39.5370229894149));
#52325=CARTESIAN_POINT('Ctrl Pts',(18.171153940697,17.018390060364,39.5991970147754));
#52326=CARTESIAN_POINT('Ctrl Pts',(18.22341524062,17.02261405329,39.6587613780303));
#52327=CARTESIAN_POINT('Ctrl Pts',(18.2756598235857,17.0268366950765,39.718306688278));
#52328=CARTESIAN_POINT('Ctrl Pts',(18.3309198409661,17.031059336863,39.7752436419715));
#52329=CARTESIAN_POINT('Ctrl Pts',(18.3888986580057,17.0352819786495,39.8292607977758));
#52330=CARTESIAN_POINT('Ctrl Pts',(18.4468769809688,17.039504584452,39.8832774932636));
#52331=CARTESIAN_POINT('Ctrl Pts',(18.5075737135671,17.0437271902545,39.934374121833));
#52332=CARTESIAN_POINT('Ctrl Pts',(18.5706567610301,17.047949796057,39.9822774360096));
#52333=CARTESIAN_POINT('Ctrl Pts',(18.633802536487,17.052176600699,40.0302283838838));
#52334=CARTESIAN_POINT('Ctrl Pts',(18.6993389924538,17.056403405341,40.07497939045));
#52335=CARTESIAN_POINT('Ctrl Pts',(18.7669029535764,17.060630209983,40.1162991134753));
#52336=CARTESIAN_POINT('Ctrl Pts',(18.8344996550106,17.0648590628604,40.1576388593144));
#52337=CARTESIAN_POINT('Ctrl Pts',(18.904125406601,17.0690879157379,40.195543784812));
#52338=CARTESIAN_POINT('Ctrl Pts',(18.9753924414283,17.0733167686154,40.229828582731));
#52339=CARTESIAN_POINT('Ctrl Pts',(19.0467875587346,17.0775532216682,40.264174997945));
#52340=CARTESIAN_POINT('Ctrl Pts',(19.1198294200048,17.0817896747209,40.2948881035024));
#52341=CARTESIAN_POINT('Ctrl Pts',(19.1941105159324,17.0860261277737,40.3218309072405));
#52342=CARTESIAN_POINT('Ctrl Pts',(19.2616225570264,17.0898765232077,40.3463184790842));
#52343=CARTESIAN_POINT('Ctrl Pts',(19.3301578021318,17.0937269186418,40.3676921508715));
#52344=CARTESIAN_POINT('Ctrl Pts',(19.3994024300127,17.0975773140758,40.3858856051486));
#52345=CARTESIAN_POINT('Ctrl Pts',(19.4756112180581,17.1018149564533,40.4059088350113));
#52346=CARTESIAN_POINT('Ctrl Pts',(19.5529654791961,17.1060525988307,40.4221544128668));
#52347=CARTESIAN_POINT('Ctrl Pts',(19.6310566193519,17.1102902412082,40.4344959247718));
#52348=CARTESIAN_POINT('Ctrl Pts',(19.7090354613836,17.1145217896897,40.4468196890983));
#52349=CARTESIAN_POINT('Ctrl Pts',(19.7877486188433,17.1187533381711,40.4552504641836));
#52350=CARTESIAN_POINT('Ctrl Pts',(19.8667742505727,17.1229848866526,40.4597121308731));
#52351=CARTESIAN_POINT('Ctrl Pts',(19.9457086055152,17.1272115475786,40.4641686442143));
#52352=CARTESIAN_POINT('Ctrl Pts',(20.0249542518364,17.1314382085047,40.4646651332847));
#52353=CARTESIAN_POINT('Ctrl Pts',(20.1040826279532,17.1356648694308,40.4611770893896));
#52354=CARTESIAN_POINT('Ctrl Pts',(20.1831610557731,17.1398888623568,40.4576912472565));
#52355=CARTESIAN_POINT('Ctrl Pts',(20.2621218932258,17.1441128552828,40.4502258850654));
#52356=CARTESIAN_POINT('Ctrl Pts',(20.3405361893824,17.1483368482088,40.4388085737445));
#52357=CARTESIAN_POINT('Ctrl Pts',(20.4189254029551,17.1525594899953,40.4273949145086));
#52358=CARTESIAN_POINT('Ctrl Pts',(20.4967679588492,17.1567821317817,40.4120318839297));
#52359=CARTESIAN_POINT('Ctrl Pts',(20.5736411301864,17.1610047735682,40.392798790705));
#52360=CARTESIAN_POINT('Ctrl Pts',(20.6505136464356,17.1652273793707,40.3735658613786));
#52361=CARTESIAN_POINT('Ctrl Pts',(20.726416340144,17.1694499851731,40.3504630501428));
#52362=CARTESIAN_POINT('Ctrl Pts',(20.8009392218789,17.1736725909756,40.3236202022279));
#52363=CARTESIAN_POINT('Ctrl Pts',(20.8755362070547,17.1778993956176,40.296750662546));
#52364=CARTESIAN_POINT('Ctrl Pts',(20.9487501975282,17.1821262002595,40.2661338167213));
#52365=CARTESIAN_POINT('Ctrl Pts',(21.0201894385494,17.1863530049015,40.2319483929899));
#52366=CARTESIAN_POINT('Ctrl Pts',(21.0916632977751,17.1905818577789,40.1977464036011));
#52367=CARTESIAN_POINT('Ctrl Pts',(21.1613602816399,17.1948107106564,40.1599726150488));
#52368=CARTESIAN_POINT('Ctrl Pts',(21.2289138665968,17.1990395635338,40.1188514431196));
#52369=CARTESIAN_POINT('Ctrl Pts',(21.2965888601495,17.2032760165866,40.0776563674333));
#52370=CARTESIAN_POINT('Ctrl Pts',(21.3621123692442,17.2075124696394,40.0331021520699));
#52371=CARTESIAN_POINT('Ctrl Pts',(21.4251476538011,17.2117489226921,39.985456073677));
#52372=CARTESIAN_POINT('Ctrl Pts',(21.4824386868489,17.2155993181263,39.9421518660256));
#52373=CARTESIAN_POINT('Ctrl Pts',(21.5376745363659,17.2194497135605,39.8962943192532));
#52374=CARTESIAN_POINT('Ctrl Pts',(21.5906287467406,17.2233001089947,39.8481105888766));
#52375=CARTESIAN_POINT('Ctrl Pts',(21.6489087363638,17.2275377513722,39.795080862128));
#52376=CARTESIAN_POINT('Ctrl Pts',(21.7046432978637,17.2317753937497,39.739033924919));
#52377=CARTESIAN_POINT('Ctrl Pts',(21.757503974408,17.2360130361272,39.6802437219746));
#52378=CARTESIAN_POINT('Ctrl Pts',(21.8102886352249,17.2402445846087,39.6215380616492));
#52379=CARTESIAN_POINT('Ctrl Pts',(21.8602073075257,17.2444761330901,39.5600973155472));
#52380=CARTESIAN_POINT('Ctrl Pts',(21.9069665142878,17.2487076815716,39.4962339181832));
#52381=CARTESIAN_POINT('Ctrl Pts',(21.9536717128749,17.2529343424977,39.4324442848067));
#52382=CARTESIAN_POINT('Ctrl Pts',(21.9972244224118,17.2571610034238,39.3662379372689));
#52383=CARTESIAN_POINT('Ctrl Pts',(22.0373708020521,17.2613876643499,39.2979610410383));
#52384=CARTESIAN_POINT('Ctrl Pts',(22.0774918400465,17.2656116572759,39.2297272433123));
#52385=CARTESIAN_POINT('Ctrl Pts',(22.114210579034,17.2698356502019,39.1594258941711));
#52386=CARTESIAN_POINT('Ctrl Pts',(22.1473166541412,17.2740596431279,39.0874318344817));
#52387=CARTESIAN_POINT('Ctrl Pts',(22.1804121395224,17.2782822849144,39.0154608037186));
#52388=CARTESIAN_POINT('Ctrl Pts',(22.2098970600938,17.2825049267009,38.9417985632177));
#52389=CARTESIAN_POINT('Ctrl Pts',(22.2356078400915,17.2867275684873,38.8668428953975));
#52390=CARTESIAN_POINT('Ctrl Pts',(22.2613184009903,17.2909501742898,38.7918878663251));
#52391=CARTESIAN_POINT('Ctrl Pts',(22.283254734519,17.2951727800923,38.715639875725));
#52392=CARTESIAN_POINT('Ctrl Pts',(22.3013025918172,17.2993953858948,38.6385135298163));
#52393=CARTESIAN_POINT('Ctrl Pts',(22.3193683953931,17.3036221905368,38.5613104916558));
#52394=CARTESIAN_POINT('Ctrl Pts',(22.3335378921486,17.3078489951787,38.4832278110472));
#52395=CARTESIAN_POINT('Ctrl Pts',(22.3437477653784,17.3120757998207,38.4046914064819));
#52396=CARTESIAN_POINT('Ctrl Pts',(22.3539625861338,17.3163046526982,38.326116944551));
#52397=CARTESIAN_POINT('Ctrl Pts',(22.3602139239478,17.3205335055756,38.2470887885748));
#52398=CARTESIAN_POINT('Ctrl Pts',(22.3624905221608,17.3247623584531,38.1680365607634));
#52399=CARTESIAN_POINT('Ctrl Pts',(22.3647712119197,17.3289988115059,38.0888422587751));
#52400=CARTESIAN_POINT('Ctrl Pts',(22.363062898846,17.3332352645586,38.0096242682856));
#52401=CARTESIAN_POINT('Ctrl Pts',(22.3574064930663,17.3374717176114,37.9308105578091));
#52402=CARTESIAN_POINT('Ctrl Pts',(22.3522655417288,17.3413221130456,37.8591789482557));
#52403=CARTESIAN_POINT('Ctrl Pts',(22.3438639675438,17.3451725084797,37.7878814923479));
#52404=CARTESIAN_POINT('Ctrl Pts',(22.3322690560765,17.3490229039139,37.717231805177));
#52405=CARTESIAN_POINT('Ctrl Pts',(22.3195080061954,17.3532605462914,37.6394766464063));
#52406=CARTESIAN_POINT('Ctrl Pts',(22.3028303492847,17.3574981886689,37.5622143899281));
#52407=CARTESIAN_POINT('Ctrl Pts',(22.2822870979711,17.3617358310464,37.4858696853805));
#52408=CARTESIAN_POINT('Ctrl Pts',(22.2617733886591,17.3659673795279,37.4096347675142));
#52409=CARTESIAN_POINT('Ctrl Pts',(22.237405245159,17.3701989280093,37.3343152301535));
#52410=CARTESIAN_POINT('Ctrl Pts',(22.2092850086877,17.3744304764908,37.2603273308677));
#52411=CARTESIAN_POINT('Ctrl Pts',(22.1811972518661,17.3786571374169,37.1864248896487));
#52412=CARTESIAN_POINT('Ctrl Pts',(22.1493661800651,17.382883798343,37.1138514659295));
#52413=CARTESIAN_POINT('Ctrl Pts',(22.1139440056845,17.3871104592691,37.0430084287326));
#52414=CARTESIAN_POINT('Ctrl Pts',(22.0785441908843,17.3913344521951,36.9722101098683));
#52415=CARTESIAN_POINT('Ctrl Pts',(22.0395579819799,17.3955584451212,36.9031404276685));
#52416=CARTESIAN_POINT('Ctrl Pts',(21.9971853117504,17.3997824380472,36.836179889609));
#52417=CARTESIAN_POINT('Ctrl Pts',(21.9548261953766,17.4040050798337,36.7692407703904));
#52418=CARTESIAN_POINT('Ctrl Pts',(21.9090830192574,17.4082277216201,36.7044098514143));
#52419=CARTESIAN_POINT('Ctrl Pts',(21.8602004300706,17.4124503634066,36.6420408781914));
#52420=CARTESIAN_POINT('Ctrl Pts',(21.8113182574454,17.4166729692091,36.5796724364565));
#52421=CARTESIAN_POINT('Ctrl Pts',(21.7592970152437,17.4208955750116,36.5197662668323));
#52422=CARTESIAN_POINT('Ctrl Pts',(21.7044223134702,17.4251181808141,36.4626438938811));
#52423=CARTESIAN_POINT('Ctrl Pts',(21.649493045849,17.4293449854561,36.4054647200616));
#52424=CARTESIAN_POINT('Ctrl Pts',(21.5917049764482,17.4335717900981,36.3510752111073));
#52425=CARTESIAN_POINT('Ctrl Pts',(21.5313809289529,17.43779859474,36.2997603239182));
#52426=CARTESIAN_POINT('Ctrl Pts',(21.4710276494813,17.4420274476175,36.2484205704339));
#52427=CARTESIAN_POINT('Ctrl Pts',(21.4081363161896,17.446256300495,36.2001586925353));
#52428=CARTESIAN_POINT('Ctrl Pts',(21.3430611978254,17.4504851533724,36.155217991703));
#52429=CARTESIAN_POINT('Ctrl Pts',(21.2778691252131,17.4547216064252,36.1101965225831));
#52430=CARTESIAN_POINT('Ctrl Pts',(21.2104858251109,17.458958059478,36.0685084041545));
#52431=CARTESIAN_POINT('Ctrl Pts',(21.1412925752695,17.4631945125308,36.0303522767063));
#52432=CARTESIAN_POINT('Ctrl Pts',(21.0784047372744,17.4670449079649,35.9956732239522));
#52433=CARTESIAN_POINT('Ctrl Pts',(21.0140223370739,17.4708953033989,35.963911293723));
#52434=CARTESIAN_POINT('Ctrl Pts',(20.9484450821268,17.474745698833,35.9351807541761));
#52435=CARTESIAN_POINT('Ctrl Pts',(20.8762725067844,17.4789833412105,35.9035606896927));
#52436=CARTESIAN_POINT('Ctrl Pts',(20.8023814628332,17.483220983588,35.8754944441318));
#52437=CARTESIAN_POINT('Ctrl Pts',(20.7271559430759,17.4874586259655,35.8511703765404));
#52438=CARTESIAN_POINT('Ctrl Pts',(20.6520386005681,17.4916901744469,35.8268812879128));
#52439=CARTESIAN_POINT('Ctrl Pts',(20.5755910356176,17.4959217229284,35.8063238333286));
#52440=CARTESIAN_POINT('Ctrl Pts',(20.4982181411682,17.5001532714098,35.7896387458428));
#52441=CARTESIAN_POINT('Ctrl Pts',(20.4209346145485,17.5043799323359,35.7729729300938));
#52442=CARTESIAN_POINT('Ctrl Pts',(20.3427283382872,17.508606593262,35.7601706913982));
#52443=CARTESIAN_POINT('Ctrl Pts',(20.2640188624652,17.5128332541881,35.7513228231273));
#52444=CARTESIAN_POINT('Ctrl Pts',(20.1853590705172,17.5170572471141,35.7424805399067));
#52445=CARTESIAN_POINT('Ctrl Pts',(20.1061971741,17.5212812400401,35.7375877248133));
#52446=CARTESIAN_POINT('Ctrl Pts',(20.0269611991178,17.5255052329662,35.7366837844584));
#52447=CARTESIAN_POINT('Ctrl Pts',(19.947750569552,17.5297278747526,35.7357801332491));
#52448=CARTESIAN_POINT('Ctrl Pts',(19.868466376881,17.5339505165391,35.7388628283737));
#52449=CARTESIAN_POINT('Ctrl Pts',(19.7895385366271,17.5381731583255,35.7459191999137));
#52450=CARTESIAN_POINT('Ctrl Pts',(19.7106113689705,17.542395764128,35.7529755113217));
#52451=CARTESIAN_POINT('Ctrl Pts',(19.6320410144762,17.5466183699305,35.7640053886495));
#52452=CARTESIAN_POINT('Ctrl Pts',(19.5542526573517,17.550840975733,35.7789442601648));
#52453=CARTESIAN_POINT('Ctrl Pts',(19.4763869496902,17.555067780375,35.7938979864704));
#52454=CARTESIAN_POINT('Ctrl Pts',(19.3993052540812,17.559294585017,35.8127683826339));
#52455=CARTESIAN_POINT('Ctrl Pts',(19.323422336034,17.5635213896589,35.8354397544949));
#52456=CARTESIAN_POINT('Ctrl Pts',(19.2475026464544,17.5677502425364,35.8581221125053));
#52457=CARTESIAN_POINT('Ctrl Pts',(19.1727833340701,17.5719790954138,35.884608958642));
#52458=CARTESIAN_POINT('Ctrl Pts',(19.0996613376738,17.5762079482913,35.914735545976));
#52459=CARTESIAN_POINT('Ctrl Pts',(19.0264079250261,17.5804444013441,35.9449162773894));
#52460=CARTESIAN_POINT('Ctrl Pts',(18.9547579892537,17.5846808543968,35.9787496197392));
#52461=CARTESIAN_POINT('Ctrl Pts',(18.8850857062837,17.5889173074496,36.0160238584458));
#52462=CARTESIAN_POINT('Ctrl Pts',(18.8217624882773,17.5927677028838,36.0499013868261));
#52463=CARTESIAN_POINT('Ctrl Pts',(18.7600728064957,17.5966180983179,36.0866205484366));
#52464=CARTESIAN_POINT('Ctrl Pts',(18.7002756582113,17.600468493752,36.1259921286221));
#52465=CARTESIAN_POINT('Ctrl Pts',(18.6345424421239,17.604701118256,36.1692721287941));
#52466=CARTESIAN_POINT('Ctrl Pts',(18.5708485327689,17.6089337427599,36.2159212483599));
#52467=CARTESIAN_POINT('Ctrl Pts',(18.5095604553716,17.6131663672639,36.265720739716));
#52468=CARTESIAN_POINT('Ctrl Pts',(18.4483605673713,17.6173929013075,36.3154485729732));
#52469=CARTESIAN_POINT('Ctrl Pts',(18.3895599986511,17.6216194353511,36.3683174822045));
#52470=CARTESIAN_POINT('Ctrl Pts',(18.3334967480836,17.6258459693948,36.4240652303112));
#52471=CARTESIAN_POINT('Ctrl Pts',(18.2774981086243,17.6300676324927,36.479748730916));
#52472=CARTESIAN_POINT('Ctrl Pts',(18.2242308501914,17.6342892955907,36.5383041478187));
#52473=CARTESIAN_POINT('Ctrl Pts',(18.1739990900591,17.6385109586886,36.5994297358021));
#52474=CARTESIAN_POINT('Ctrl Pts',(18.1237988641362,17.6427299715348,36.6605169507107));
#52475=CARTESIAN_POINT('Ctrl Pts',(18.0766306519891,17.6469489843811,36.7241707721064));
#52476=CARTESIAN_POINT('Ctrl Pts',(18.0327600941566,17.6511679972273,36.7900543546554));
#52477=CARTESIAN_POINT('Ctrl Pts',(17.9889033281849,17.6553856837161,36.8559172249717));
#52478=CARTESIAN_POINT('Ctrl Pts',(17.9483424182565,17.659603370205,36.9240080735154));
#52479=CARTESIAN_POINT('Ctrl Pts',(17.9113003524991,17.6638210566939,36.9939601167094));
#52480=CARTESIAN_POINT('Ctrl Pts',(17.8742583231946,17.6680387390321,37.0639120910639));
#52481=CARTESIAN_POINT('Ctrl Pts',(17.8407353497272,17.6722564213704,37.135724840284));
#52482=CARTESIAN_POINT('Ctrl Pts',(17.8109083021627,17.6764741037086,37.2090073067864));
#52483=CARTESIAN_POINT('Ctrl Pts',(17.7810515334304,17.6806959887574,37.2823627956183));
#52484=CARTESIAN_POINT('Ctrl Pts',(17.7548982238135,17.6849178738061,37.3571904904136));
#52485=CARTESIAN_POINT('Ctrl Pts',(17.7325766757284,17.6891397588548,37.4330802826057));
#52486=CARTESIAN_POINT('Ctrl Pts',(17.7102440755141,17.6933637342971,37.5090076503188));
#52487=CARTESIAN_POINT('Ctrl Pts',(17.6917471255497,17.6975877097393,37.5859977053169));
#52488=CARTESIAN_POINT('Ctrl Pts',(17.6771632698953,17.7018116851816,37.6636286373093));
#52489=CARTESIAN_POINT('Ctrl Pts',(17.6625534885534,17.7060431695755,37.7413975736359));
#52490=CARTESIAN_POINT('Ctrl Pts',(17.6518707623599,17.7102746539695,37.8198091963865));
#52491=CARTESIAN_POINT('Ctrl Pts',(17.6451407419896,17.7145061383634,37.8984353308179));
#52492=CARTESIAN_POINT('Ctrl Pts',(17.6393928015494,17.7181201423235,37.9655879266325));
#52493=CARTESIAN_POINT('Ctrl Pts',(17.6365272544186,17.7217341462836,38.0328967675363));
#52494=CARTESIAN_POINT('Ctrl Pts',(17.6365300019755,17.7253481502437,38.1000966336477));
#52495=CARTESIAN_POINT('',(17.6365308155374,18.5190981502267,38.0980365857439));
#52496=CARTESIAN_POINT('Ctrl Pts',(17.6365300019755,17.7253481502717,38.100096634168));
#52497=CARTESIAN_POINT('Ctrl Pts',(17.6365302156428,17.7256291964049,38.1053224896805));
#52498=CARTESIAN_POINT('Ctrl Pts',(17.6365477615718,17.725910242538,38.1105483033315));
#52499=CARTESIAN_POINT('Ctrl Pts',(17.6365826391035,17.7261912886711,38.1157740011787));
#52500=CARTESIAN_POINT('Ctrl Pts',(17.6371085260988,17.7304289310486,38.1945676084847));
#52501=CARTESIAN_POINT('Ctrl Pts',(17.6415800413973,17.7346665734261,38.2734827912252));
#52502=CARTESIAN_POINT('Ctrl Pts',(17.6500127662927,17.7389042158035,38.3520921306049));
#52503=CARTESIAN_POINT('Ctrl Pts',(17.6584333645989,17.743135764285,38.4305884266698));
#52504=CARTESIAN_POINT('Ctrl Pts',(17.670803810442,17.7473673127664,38.508779290557));
#52505=CARTESIAN_POINT('Ctrl Pts',(17.6870876759688,17.7515988612478,38.5862376191171));
#52506=CARTESIAN_POINT('Ctrl Pts',(17.7033527331813,17.7558255221739,38.6636064811689));
#52507=CARTESIAN_POINT('Ctrl Pts',(17.7235221315334,17.7600521831,38.7402440328805));
#52508=CARTESIAN_POINT('Ctrl Pts',(17.7475078644291,17.7642788440261,38.8157301307695));
#52509=CARTESIAN_POINT('Ctrl Pts',(17.7714784567827,17.7685028369521,38.8911685794812));
#52510=CARTESIAN_POINT('Ctrl Pts',(17.7992604605148,17.7727268298781,38.9654565714615));
#52511=CARTESIAN_POINT('Ctrl Pts',(17.8307154869953,17.7769508228041,39.0381871575214));
#52512=CARTESIAN_POINT('Ctrl Pts',(17.8621604518751,17.7811734645905,39.1108944790603));
#52513=CARTESIAN_POINT('Ctrl Pts',(17.8972759204384,17.7853961063769,39.1820449540007));
#52514=CARTESIAN_POINT('Ctrl Pts',(17.9358751752938,17.7896187481634,39.2512511233139));
#52515=CARTESIAN_POINT('Ctrl Pts',(17.9744741012189,17.7938413539658,39.3204567028747));
#52516=CARTESIAN_POINT('Ctrl Pts',(18.0165565248192,17.7980639597683,39.3877176010481));
#52517=CARTESIAN_POINT('Ctrl Pts',(18.061890256853,17.8022865655707,39.4526718243605));
#52518=CARTESIAN_POINT('Ctrl Pts',(18.1072690674647,17.8065133702127,39.5176906363111));
#52519=CARTESIAN_POINT('Ctrl Pts',(18.1559053755455,17.8107401748546,39.5803978064397));
#52520=CARTESIAN_POINT('Ctrl Pts',(18.207524548805,17.8149669794966,39.6404616833156));
#52521=CARTESIAN_POINT('Ctrl Pts',(18.2591687358114,17.819195832374,39.7005546660937));
#52522=CARTESIAN_POINT('Ctrl Pts',(18.3137983440383,17.8234246852514,39.7580014637972));
#52523=CARTESIAN_POINT('Ctrl Pts',(18.3711012062747,17.8276535381289,39.8125066892425));
#52524=CARTESIAN_POINT('Ctrl Pts',(18.4285070543117,17.8318899911816,39.8671098725221));
#52525=CARTESIAN_POINT('Ctrl Pts',(18.4885953997276,17.8361264442344,39.9187606140064));
#52526=CARTESIAN_POINT('Ctrl Pts',(18.5510204556017,17.8403628972871,39.9672034492297));
#52527=CARTESIAN_POINT('Ctrl Pts',(18.6077568686182,17.8442132927215,40.0112318072093));
#52528=CARTESIAN_POINT('Ctrl Pts',(18.6664229068114,17.8480636881558,40.0526106620861));
#52529=CARTESIAN_POINT('Ctrl Pts',(18.7267402548508,17.8519140835901,40.0911805699842));
#52530=CARTESIAN_POINT('Ctrl Pts',(18.7931239171296,17.8561517259677,40.1336295804805));
#52531=CARTESIAN_POINT('Ctrl Pts',(18.8617573107764,17.8603893683452,40.1728349091079));
#52532=CARTESIAN_POINT('Ctrl Pts',(18.9322903694693,17.8646270107228,40.2085508259874));
#52533=CARTESIAN_POINT('Ctrl Pts',(19.0027219988558,17.8688585592043,40.2442153819768));
#52534=CARTESIAN_POINT('Ctrl Pts',(19.0750474534436,17.8730901076858,40.2764002813037));
#52535=CARTESIAN_POINT('Ctrl Pts',(19.1488886212691,17.8773216561673,40.3049035946941));
#52536=CARTESIAN_POINT('Ctrl Pts',(19.2226445005066,17.8815483170935,40.3333739859703));
#52537=CARTESIAN_POINT('Ctrl Pts',(19.2979121788094,17.8857749780197,40.3581710738102));
#52538=CARTESIAN_POINT('Ctrl Pts',(19.3742913063108,17.8900016389458,40.3791399850693));
#52539=CARTESIAN_POINT('Ctrl Pts',(19.4506222209268,17.8942256318719,40.4000956600982));
#52540=CARTESIAN_POINT('Ctrl Pts',(19.5280627413151,17.898449624798,40.4172278311821));
#52541=CARTESIAN_POINT('Ctrl Pts',(19.6061961611427,17.902673617724,40.4304310711543));
#52542=CARTESIAN_POINT('Ctrl Pts',(19.6843045882309,17.9068962595106,40.4436300877719));
#52543=CARTESIAN_POINT('Ctrl Pts',(19.7631050127389,17.9111189012971,40.4529025908986));
#52544=CARTESIAN_POINT('Ctrl Pts',(19.8421707709355,17.9153415430836,40.4581943039862));
#52545=CARTESIAN_POINT('Ctrl Pts',(19.9212358553596,17.9195641488861,40.4634859719796));
#52546=CARTESIAN_POINT('Ctrl Pts',(20.0005658011548,17.9237867546887,40.4647968875055));
#52547=CARTESIAN_POINT('Ctrl Pts',(20.0797305548749,17.9280093604912,40.4621247806836));
#52548=CARTESIAN_POINT('Ctrl Pts',(20.1589740277818,17.9322361651333,40.4594500167944));
#52549=CARTESIAN_POINT('Ctrl Pts',(20.2380515109032,17.9364629697753,40.4527843350827));
#52550=CARTESIAN_POINT('Ctrl Pts',(20.3165353004896,17.9406897744173,40.4421775860178));
#52551=CARTESIAN_POINT('Ctrl Pts',(20.3950571219453,17.9449186272949,40.4315656971081));
#52552=CARTESIAN_POINT('Ctrl Pts',(20.4729842153547,17.9491474801724,40.4170090225433));
#52553=CARTESIAN_POINT('Ctrl Pts',(20.5498988662793,17.9533763330499,40.3986086395393));
#52554=CARTESIAN_POINT('Ctrl Pts',(20.6269517496866,17.9576127861027,40.3801751870149));
#52555=CARTESIAN_POINT('Ctrl Pts',(20.7029881040009,17.9618492391555,40.357884355413));
#52556=CARTESIAN_POINT('Ctrl Pts',(20.7776054042554,17.9660856922084,40.3318871557883));
#52557=CARTESIAN_POINT('Ctrl Pts',(20.84542301219,17.969936087642,40.3082590174674));
#52558=CARTESIAN_POINT('Ctrl Pts',(20.9120684013927,17.9737864830757,40.2815699604525));
#52559=CARTESIAN_POINT('Ctrl Pts',(20.9772563226411,17.9776368785093,40.2519666634867));
#52560=CARTESIAN_POINT('Ctrl Pts',(21.0490004077203,17.9818745208867,40.2193860654945));
#52561=CARTESIAN_POINT('Ctrl Pts',(21.1192480819326,17.9861121632642,40.1831525894848));
#52562=CARTESIAN_POINT('Ctrl Pts',(21.1876026569099,17.9903498056416,40.1434261352445));
#52563=CARTESIAN_POINT('Ctrl Pts',(21.2558589353261,17.994581354123,40.1037568092045));
#52564=CARTESIAN_POINT('Ctrl Pts',(21.3222271188972,17.9988129026045,40.0606047138301));
#52565=CARTESIAN_POINT('Ctrl Pts',(21.3863319959239,18.0030444510859,40.0141771177134));
#52566=CARTESIAN_POINT('Ctrl Pts',(21.4503628300475,18.0072711120119,39.9678031467523));
#52567=CARTESIAN_POINT('Ctrl Pts',(21.5121351749246,18.011497772938,39.9181614669805));
#52568=CARTESIAN_POINT('Ctrl Pts',(21.5713011878368,18.0157244338641,39.8655036159698));
#52569=CARTESIAN_POINT('Ctrl Pts',(21.630429853318,18.01994842679,39.8128790042356));
#52570=CARTESIAN_POINT('Ctrl Pts',(21.6869551031147,18.024172419716,39.7572423111346));
#52571=CARTESIAN_POINT('Ctrl Pts',(21.740561669731,18.028396412642,39.6988857103506));
#52572=CARTESIAN_POINT('Ctrl Pts',(21.794151089076,18.0326190544284,39.6405477762436));
#52573=CARTESIAN_POINT('Ctrl Pts',(21.8448233623029,18.0368416962148,39.5794920071253));
#52574=CARTESIAN_POINT('Ctrl Pts',(21.8923007103463,18.0410643380012,39.5160467727172));
#52575=CARTESIAN_POINT('Ctrl Pts',(21.9397776538033,18.0452869438037,39.4526020789686));
#52576=CARTESIAN_POINT('Ctrl Pts',(21.9840594464951,18.0495095496061,39.3867683365935));
#52577=CARTESIAN_POINT('Ctrl Pts',(22.0249100909219,18.0537321554085,39.3189050679124));
#52578=CARTESIAN_POINT('Ctrl Pts',(22.0658013560714,18.0579589600505,39.2509743179208));
#52579=CARTESIAN_POINT('Ctrl Pts',(22.1032544154758,18.0621857646924,39.1810104130094));
#52580=CARTESIAN_POINT('Ctrl Pts',(22.1370782727308,18.0664125693344,39.1093992753722));
#52581=CARTESIAN_POINT('Ctrl Pts',(22.1709185204344,18.0706414222118,39.0377534362324));
#52582=CARTESIAN_POINT('Ctrl Pts',(22.2011258837041,18.0748702750892,38.9644592081811));
#52583=CARTESIAN_POINT('Ctrl Pts',(22.2275577761299,18.0790991279666,38.8899220182418));
#52584=CARTESIAN_POINT('Ctrl Pts',(22.2540371724587,18.0833355810193,38.8152508686382));
#52585=CARTESIAN_POINT('Ctrl Pts',(22.2767274056021,18.0875720340721,38.7393327438554));
#52586=CARTESIAN_POINT('Ctrl Pts',(22.2955360451978,18.0918084871248,38.6625875097242));
#52587=CARTESIAN_POINT('Ctrl Pts',(22.3126306994114,18.0956588825593,38.5928358813121));
#52588=CARTESIAN_POINT('Ctrl Pts',(22.3265195678366,18.0995092779938,38.522401422398));
#52589=CARTESIAN_POINT('Ctrl Pts',(22.3371704232296,18.1033596734283,38.4516032617607));
#52590=CARTESIAN_POINT('Ctrl Pts',(22.348892470208,18.1075973158057,38.3736846970679));
#52591=CARTESIAN_POINT('Ctrl Pts',(22.3567356866119,18.1118349581831,38.295033031655));
#52592=CARTESIAN_POINT('Ctrl Pts',(22.3606182756164,18.1160726005605,38.216068073672));
#52593=CARTESIAN_POINT('Ctrl Pts',(22.3644952813055,18.1203041490418,38.1372166703975));
#52594=CARTESIAN_POINT('Ctrl Pts',(22.3644229475746,18.1245356975232,38.0580533335972));
#52595=CARTESIAN_POINT('Ctrl Pts',(22.360370904268,18.1287672460045,37.9790056398634));
#52596=CARTESIAN_POINT('Ctrl Pts',(22.3563235411834,18.1329939069305,37.9000492483988));
#52597=CARTESIAN_POINT('Ctrl Pts',(22.3483056271484,18.1372205678565,37.8212087003508));
#52598=CARTESIAN_POINT('Ctrl Pts',(22.3363388257283,18.1414472287825,37.7429127105393));
#52599=CARTESIAN_POINT('Ctrl Pts',(22.3243795781262,18.1456712217084,37.6646661435963));
#52600=CARTESIAN_POINT('Ctrl Pts',(22.3084764614353,18.1498952146343,37.5869639147795));
#52601=CARTESIAN_POINT('Ctrl Pts',(22.2887029593892,18.1541192075602,37.5102295322897));
#52602=CARTESIAN_POINT('Ctrl Pts',(22.2689357823444,18.1583418493466,37.4335196950256));
#52603=CARTESIAN_POINT('Ctrl Pts',(22.2453007953191,18.1625644911329,37.3577775429256));
#52604=CARTESIAN_POINT('Ctrl Pts',(22.2179222520145,18.1667871329193,37.283414839151));
#52605=CARTESIAN_POINT('Ctrl Pts',(22.190543942021,18.1710097387217,37.2090527690711));
#52606=CARTESIAN_POINT('Ctrl Pts',(22.1594223024813,18.175232344524,37.1360705633542));
#52607=CARTESIAN_POINT('Ctrl Pts',(22.1247304631931,18.1794549503264,37.0648618934272));
#52608=CARTESIAN_POINT('Ctrl Pts',(22.0900041273234,18.1836817549683,36.9935824156175));
#52609=CARTESIAN_POINT('Ctrl Pts',(22.0517007061414,18.1879085596101,36.9240804187054));
#52610=CARTESIAN_POINT('Ctrl Pts',(22.010039971138,18.192135364252,36.8567261945462));
#52611=CARTESIAN_POINT('Ctrl Pts',(21.9683590480724,18.1963642171294,36.7893393317102));
#52612=CARTESIAN_POINT('Ctrl Pts',(21.9233178369004,18.2005930700067,36.7241027012231));
#52613=CARTESIAN_POINT('Ctrl Pts',(21.8751788223621,18.204821922884,36.6613566025368));
#52614=CARTESIAN_POINT('Ctrl Pts',(21.8269532914656,18.2090583759367,36.598497735361));
#52615=CARTESIAN_POINT('Ctrl Pts',(21.7756191373549,18.2132948289894,36.5381387014706));
#52616=CARTESIAN_POINT('Ctrl Pts',(21.7214782587364,18.217531282042,36.4805855855903));
#52617=CARTESIAN_POINT('Ctrl Pts',(21.6722711061265,18.2213816774772,36.4282771445646));
#52618=CARTESIAN_POINT('Ctrl Pts',(21.620746126031,18.2252320729123,36.3782862444275));
#52619=CARTESIAN_POINT('Ctrl Pts',(21.5671534828053,18.2290824683475,36.3308136327025));
#52620=CARTESIAN_POINT('Ctrl Pts',(21.5081708510469,18.2333201107254,36.2785665441573));
#52621=CARTESIAN_POINT('Ctrl Pts',(21.446461859556,18.2375577531032,36.2291742280913));
#52622=CARTESIAN_POINT('Ctrl Pts',(21.3823341468647,18.2417953954811,36.1829338177017));
#52623=CARTESIAN_POINT('Ctrl Pts',(21.3182986523408,18.2460269439629,36.1367599028368));
#52624=CARTESIAN_POINT('Ctrl Pts',(21.251851721123,18.2502584924448,36.0937291643045));
#52625=CARTESIAN_POINT('Ctrl Pts',(21.1833355018012,18.2544900409266,36.0540998237752));
#52626=CARTESIAN_POINT('Ctrl Pts',(21.1148984206048,18.2587167018531,36.0145162562285));
#52627=CARTESIAN_POINT('Ctrl Pts',(21.0443972047368,18.2629433627796,35.9783265128687));
#52628=CARTESIAN_POINT('Ctrl Pts',(20.9722032814123,18.2671700237061,35.9457457855418));
#52629=CARTESIAN_POINT('Ctrl Pts',(20.9000549291419,18.2713940166325,35.9131856241852));
#52630=CARTESIAN_POINT('Ctrl Pts',(20.8262164164086,18.2756180095589,35.8842301493618));
#52631=CARTESIAN_POINT('Ctrl Pts',(20.7510830103226,18.2798420024853,35.8590482485103));
#52632=CARTESIAN_POINT('Ctrl Pts',(20.6759736373538,18.2840646442721,35.8338744026587));
#52633=CARTESIAN_POINT('Ctrl Pts',(20.599570637706,18.2882872860589,35.8124718826541));
#52634=CARTESIAN_POINT('Ctrl Pts',(20.5222870618533,18.2925099278458,35.7949605934126));
#52635=CARTESIAN_POINT('Ctrl Pts',(20.445004144586,18.2967325336486,35.7774494533967));
#52636=CARTESIAN_POINT('Ctrl Pts',(20.3668411235336,18.3009551394515,35.763829580409));
#52637=CARTESIAN_POINT('Ctrl Pts',(20.2882224775962,18.3051777452544,35.7541700308189));
#52638=CARTESIAN_POINT('Ctrl Pts',(20.2095256555063,18.3094045498967,35.7445008760465));
#52639=CARTESIAN_POINT('Ctrl Pts',(20.1303727698975,18.3136313545391,35.7387999682103));
#52640=CARTESIAN_POINT('Ctrl Pts',(20.0511940760366,18.3178581591814,35.7370845111433));
#52641=CARTESIAN_POINT('Ctrl Pts',(19.9719770135682,18.3220870120592,35.7353682227959));
#52642=CARTESIAN_POINT('Ctrl Pts',(19.8927345871141,18.3263158649371,35.7376412190946));
#52643=CARTESIAN_POINT('Ctrl Pts',(19.813895142625,18.3305447178149,35.7438685471813));
#52644=CARTESIAN_POINT('Ctrl Pts',(19.7349140063775,18.334781170868,35.7501070671413));
#52645=CARTESIAN_POINT('Ctrl Pts',(19.6563377651814,18.3390176239211,35.7603140584373));
#52646=CARTESIAN_POINT('Ctrl Pts',(19.578587517784,18.3432540769743,35.7744028808212));
#52647=CARTESIAN_POINT('Ctrl Pts',(19.5079224605854,18.347104472405,35.7872078232227));
#52648=CARTESIAN_POINT('Ctrl Pts',(19.4379398374659,18.3509548678358,35.8032186358183));
#52649=CARTESIAN_POINT('Ctrl Pts',(19.3689442223624,18.3548052632666,35.8223347378488));
#52650=CARTESIAN_POINT('Ctrl Pts',(19.2930094910718,18.3590429056437,35.8433734092026));
#52651=CARTESIAN_POINT('Ctrl Pts',(19.2179854814123,18.3632805480208,35.8682530894602));
#52652=CARTESIAN_POINT('Ctrl Pts',(19.1442889073757,18.3675181903979,35.896877450785));
#52653=CARTESIAN_POINT('Ctrl Pts',(19.0706983119047,18.371749738879,35.9254606491549));
#52654=CARTESIAN_POINT('Ctrl Pts',(18.9984317945087,18.37598128736,35.9577776661635));
#52655=CARTESIAN_POINT('Ctrl Pts',(18.9278922126119,18.3802128358411,35.9936820436787));
#52656=CARTESIAN_POINT('Ctrl Pts',(18.85743410588,18.3844394967668,36.0295449506463));
#52657=CARTESIAN_POINT('Ctrl Pts',(18.7886993864146,18.3886661576926,36.068986772376));
#52658=CARTESIAN_POINT('Ctrl Pts',(18.7220707527108,18.3928928186183,36.1118130671834));
#52659=CARTESIAN_POINT('Ctrl Pts',(18.6554841770769,18.3971168115439,36.1546123286989));
#52660=CARTESIAN_POINT('Ctrl Pts',(18.5910014417465,18.4013408044696,36.2007915700013));
#52661=CARTESIAN_POINT('Ctrl Pts',(18.5289793788504,18.4055647973952,36.250111145757));
#52662=CARTESIAN_POINT('Ctrl Pts',(18.4669771551121,18.4097874391813,36.2994149455323));
#52663=CARTESIAN_POINT('Ctrl Pts',(18.4074344074242,18.4140100809674,36.3518567934551));
#52664=CARTESIAN_POINT('Ctrl Pts',(18.3506765581838,18.4182327227535,36.4071554633767));
#52665=CARTESIAN_POINT('Ctrl Pts',(18.2939191926152,18.4224553285556,36.4624536620611));
#52666=CARTESIAN_POINT('Ctrl Pts',(18.2399470130703,18.4266779343577,36.5206083061871));
#52667=CARTESIAN_POINT('Ctrl Pts',(18.1890490076465,18.4309005401598,36.5813009039991));
#52668=CARTESIAN_POINT('Ctrl Pts',(18.1381003906889,18.4351273448015,36.6420538528099));
#52669=CARTESIAN_POINT('Ctrl Pts',(18.0902323558881,18.4393541494431,36.7053494363262));
#52670=CARTESIAN_POINT('Ctrl Pts',(18.045693538211,18.4435809540847,36.7708360920076));
#52671=CARTESIAN_POINT('Ctrl Pts',(18.0011331378032,18.4478098069618,36.836354481375));
#52672=CARTESIAN_POINT('Ctrl Pts',(17.9599054124639,18.4520386598389,36.9040656571423));
#52673=CARTESIAN_POINT('Ctrl Pts',(17.922214205294,18.456267512716,36.9735912676928));
#52674=CARTESIAN_POINT('Ctrl Pts',(17.8844552587651,18.4605039657685,37.0432418310013));
#52675=CARTESIAN_POINT('Ctrl Pts',(17.8502457329749,18.4647404188209,37.1147129209253));
#52676=CARTESIAN_POINT('Ctrl Pts',(17.8197421672373,18.4689768718733,37.1876041300088));
#52677=CARTESIAN_POINT('Ctrl Pts',(17.792018316911,18.4728272673107,37.2538529413159));
#52678=CARTESIAN_POINT('Ctrl Pts',(17.7673552403086,18.4766776627481,37.3212743498509));
#52679=CARTESIAN_POINT('Ctrl Pts',(17.7458343539072,18.4805280581856,37.3895581087274));
#52680=CARTESIAN_POINT('Ctrl Pts',(17.7172495838534,18.4856422837868,37.4802549094767));
#52681=CARTESIAN_POINT('Ctrl Pts',(17.6941206659814,18.490756509388,37.5727480809934));
#52682=CARTESIAN_POINT('Ctrl Pts',(17.6766370864719,18.4958707349892,37.6664389167118));
#52683=CARTESIAN_POINT('Ctrl Pts',(17.659368835943,18.5009219734323,37.7589758495841));
#52684=CARTESIAN_POINT('Ctrl Pts',(17.6476077702664,18.5059732118755,37.8526810990171));
#52685=CARTESIAN_POINT('Ctrl Pts',(17.6414902309452,18.5110244503186,37.9469571622939));
#52686=CARTESIAN_POINT('Ctrl Pts',(17.638230886581,18.5137156836213,37.9971862069121));
#52687=CARTESIAN_POINT('Ctrl Pts',(17.6365727340863,18.516406916924,38.0475769344872));
#52688=CARTESIAN_POINT('Ctrl Pts',(17.6365308155374,18.5190981502267,38.0980365857439));
#52689=CARTESIAN_POINT('',(17.6365304226752,19.3128481502999,38.1014134921557));
#52690=CARTESIAN_POINT('Ctrl Pts',(17.6365308155367,18.5190981502717,38.0980365865869));
#52691=CARTESIAN_POINT('Ctrl Pts',(17.6364653475663,18.523301293328,38.1768439990069));
#52692=CARTESIAN_POINT('Ctrl Pts',(17.6403457991141,18.5275044363842,38.2557159250519));
#52693=CARTESIAN_POINT('Ctrl Pts',(17.6481648313519,18.5317075794405,38.3342259174604));
#52694=CARTESIAN_POINT('Ctrl Pts',(17.6559813183685,18.5359093543058,38.4127103535983));
#52695=CARTESIAN_POINT('Ctrl Pts',(17.6677337940143,18.5401111291712,38.4908326190067));
#52696=CARTESIAN_POINT('Ctrl Pts',(17.6833629476021,18.5443129040365,38.5681700634994));
#52697=CARTESIAN_POINT('Ctrl Pts',(17.6989919989068,18.5485146514038,38.6455070018668));
#52698=CARTESIAN_POINT('Ctrl Pts',(17.7184975824096,18.5527163987711,38.7220586655415));
#52699=CARTESIAN_POINT('Ctrl Pts',(17.7417693239072,18.5569181461385,38.7974128292865));
#52700=CARTESIAN_POINT('Ctrl Pts',(17.7650647959264,18.5611241780866,38.8728438327307));
#52701=CARTESIAN_POINT('Ctrl Pts',(17.7921339562944,18.5653302100348,38.9470744436813));
#52702=CARTESIAN_POINT('Ctrl Pts',(17.8228167847401,18.5695362419829,39.0197084799492));
#52703=CARTESIAN_POINT('Ctrl Pts',(17.8535149226381,18.5737443725657,39.0923787575735));
#52704=CARTESIAN_POINT('Ctrl Pts',(17.8878301126272,18.5779525031484,39.1634504473205));
#52705=CARTESIAN_POINT('Ctrl Pts',(17.9255556060353,18.5821606337312,39.2325506157556));
#52706=CARTESIAN_POINT('Ctrl Pts',(17.9633505311331,18.5863765091461,39.3017779592391));
#52707=CARTESIAN_POINT('Ctrl Pts',(18.0045680504769,18.5905923845611,39.3690261279718));
#52708=CARTESIAN_POINT('Ctrl Pts',(18.0489573443338,18.5948082599761,39.4339501477458));
#52709=CARTESIAN_POINT('Ctrl Pts',(18.0891173410826,18.5986224576856,39.4926883748382));
#52710=CARTESIAN_POINT('Ctrl Pts',(18.131872794144,18.6024366553952,39.5495244326457));
#52711=CARTESIAN_POINT('Ctrl Pts',(18.177010871039,18.6062508531047,39.6042277342843));
#52712=CARTESIAN_POINT('Ctrl Pts',(18.2271600877748,18.6104884954849,39.6650040880581));
#52713=CARTESIAN_POINT('Ctrl Pts',(18.2804460833656,18.6147261378651,39.7233839064688));
#52714=CARTESIAN_POINT('Ctrl Pts',(18.3366111180252,18.6189637802453,39.7790258688366));
#52715=CARTESIAN_POINT('Ctrl Pts',(18.392695385161,18.6231953287294,39.8345878158792));
#52716=CARTESIAN_POINT('Ctrl Pts',(18.4516501391006,18.6274268772136,39.8874193984905));
#52717=CARTESIAN_POINT('Ctrl Pts',(18.5131775036553,18.6316584256977,39.9372123734787));
#52718=CARTESIAN_POINT('Ctrl Pts',(18.5746338024049,18.6358850866265,39.9869478362059));
#52719=CARTESIAN_POINT('Ctrl Pts',(18.6386564442277,18.6401117475553,40.033651372513));
#52720=CARTESIAN_POINT('Ctrl Pts',(18.7049119446151,18.6443384084841,40.0770526977547));
#52721=CARTESIAN_POINT('Ctrl Pts',(18.7711256224658,18.6485624014127,40.1204266267274));
#52722=CARTESIAN_POINT('Ctrl Pts',(18.8395689701737,18.6527863943414,40.1605022258573));
#52723=CARTESIAN_POINT('Ctrl Pts',(18.9098777588544,18.6570103872701,40.1970512488396));
#52724=CARTESIAN_POINT('Ctrl Pts',(18.9801640576806,18.6612330290593,40.2335885807912));
#52725=CARTESIAN_POINT('Ctrl Pts',(19.0523141969129,18.6654556708484,40.2666013606293));
#52726=CARTESIAN_POINT('Ctrl Pts',(19.1259387702036,18.6696783126375,40.2959069669425));
#52727=CARTESIAN_POINT('Ctrl Pts',(19.1995627160894,18.6739009184426,40.3252123235229));
#52728=CARTESIAN_POINT('Ctrl Pts',(19.2746606349845,18.6781235242478,40.3508103973575));
#52729=CARTESIAN_POINT('Ctrl Pts',(19.3508239309417,18.6823461300529,40.3725670226117));
#52730=CARTESIAN_POINT('Ctrl Pts',(19.4270629615204,18.6865729346975,40.394345282037));
#52731=CARTESIAN_POINT('Ctrl Pts',(19.5043690334875,18.6907997393421,40.4122743337015));
#52732=CARTESIAN_POINT('Ctrl Pts',(19.582319788744,18.6950265439867,40.426270337262));
#52733=CARTESIAN_POINT('Ctrl Pts',(19.6603083175704,18.6992553968668,40.4402731230406));
#52734=CARTESIAN_POINT('Ctrl Pts',(19.7389416864538,18.7034842497468,40.4503390043688));
#52735=CARTESIAN_POINT('Ctrl Pts',(19.8177913202494,18.7077131026269,40.4564359609214));
#52736=CARTESIAN_POINT('Ctrl Pts',(19.8967826641148,18.7119495556822,40.4625438750409));
#52737=CARTESIAN_POINT('Ctrl Pts',(19.9759905797868,18.7161860087375,40.464668599304));
#52738=CARTESIAN_POINT('Ctrl Pts',(20.0549856210584,18.7204224617929,40.4628302991067));
#52739=CARTESIAN_POINT('Ctrl Pts',(20.1267820366863,18.7242728572032,40.4611595187276));
#52740=CARTESIAN_POINT('Ctrl Pts',(20.1984023756985,18.7281232526135,40.4562157707697));
#52741=CARTESIAN_POINT('Ctrl Pts',(20.2695301359815,18.7319736480237,40.4480510954189));
#52742=CARTESIAN_POINT('Ctrl Pts',(20.347811449674,18.7362112903979,40.4390652717435));
#52743=CARTESIAN_POINT('Ctrl Pts',(20.4257898477129,18.740448932772,40.4261435866177));
#52744=CARTESIAN_POINT('Ctrl Pts',(20.503038710321,18.7446865751462,40.4093164566206));
#52745=CARTESIAN_POINT('Ctrl Pts',(20.5801764860331,18.7489181236243,40.3925135246967));
#52746=CARTESIAN_POINT('Ctrl Pts',(20.6565863554827,18.7531496721024,40.3718164000696));
#52747=CARTESIAN_POINT('Ctrl Pts',(20.7318475988545,18.7573812205805,40.3473071736972));
#52748=CARTESIAN_POINT('Ctrl Pts',(20.8070219134126,18.7616078815033,40.3228262561578));
#52749=CARTESIAN_POINT('Ctrl Pts',(20.8810497948919,18.7658345424261,40.2945421313271));
#52750=CARTESIAN_POINT('Ctrl Pts',(20.9535229827976,18.7700612033489,40.2625874230136));
#52751=CARTESIAN_POINT('Ctrl Pts',(21.025950423369,18.7742851962716,40.2306528855077));
#52752=CARTESIAN_POINT('Ctrl Pts',(21.0968246904719,18.7785091891943,40.1950525521099));
#52753=CARTESIAN_POINT('Ctrl Pts',(21.1657560529569,18.7827331821171,40.1559677200516));
#52754=CARTESIAN_POINT('Ctrl Pts',(21.2346653661889,18.7869558239003,40.1168953901595));
#52755=CARTESIAN_POINT('Ctrl Pts',(21.3016326014543,18.7911784656835,40.0743410060243));
#52756=CARTESIAN_POINT('Ctrl Pts',(21.3662925958599,18.7954011074667,40.028531820686));
#52757=CARTESIAN_POINT('Ctrl Pts',(21.4309520392545,18.7996237132659,39.9827230257183));
#52758=CARTESIAN_POINT('Ctrl Pts',(21.493303899202,18.8038463190652,39.9336597568539));
#52759=CARTESIAN_POINT('Ctrl Pts',(21.5530132150415,18.8080689248644,39.881611740758));
#52760=CARTESIAN_POINT('Ctrl Pts',(21.6127819041329,18.8122957295033,39.8295119695894));
#52761=CARTESIAN_POINT('Ctrl Pts',(21.6699024461431,18.8165225341421,39.7744218314421));
#52762=CARTESIAN_POINT('Ctrl Pts',(21.7240746056064,18.8207493387809,39.7166499915576));
#52763=CARTESIAN_POINT('Ctrl Pts',(21.7782730159494,18.8249781916552,39.6588501564514));
#52764=CARTESIAN_POINT('Ctrl Pts',(21.8295198941157,18.8292070445296,39.5983663889541));
#52765=CARTESIAN_POINT('Ctrl Pts',(21.8775550906141,18.8334358974039,39.5355407770625));
#52766=CARTESIAN_POINT('Ctrl Pts',(21.9256766168881,18.8376723504536,39.4726022537773));
#52767=CARTESIAN_POINT('Ctrl Pts',(21.9705746620337,18.8419088035034,39.4073138636635));
#52768=CARTESIAN_POINT('Ctrl Pts',(22.0120323793199,18.8461452565531,39.3400468319658));
#52769=CARTESIAN_POINT('Ctrl Pts',(22.0497121564072,18.8499956520164,39.2789096800526));
#52770=CARTESIAN_POINT('Ctrl Pts',(22.0845505022411,18.8538460474796,39.2161386405155));
#52771=CARTESIAN_POINT('Ctrl Pts',(22.1164187882959,18.8576964429429,39.1520275440539));
#52772=CARTESIAN_POINT('Ctrl Pts',(22.1514921724919,18.8619340853174,39.0814685841664));
#52773=CARTESIAN_POINT('Ctrl Pts',(22.1830990023349,18.866171727692,39.0090213011705));
#52774=CARTESIAN_POINT('Ctrl Pts',(22.211032569004,18.8704093700665,38.9350601293942));
#52775=CARTESIAN_POINT('Ctrl Pts',(22.2389259661075,18.8746409185449,38.8612053166863));
#52776=CARTESIAN_POINT('Ctrl Pts',(22.2631564259306,18.8788724670234,38.7858413734966));
#52777=CARTESIAN_POINT('Ctrl Pts',(22.2835637991729,18.8831040155018,38.7093659130664));
#52778=CARTESIAN_POINT('Ctrl Pts',(22.3039476013352,18.8873306764248,38.6329787839059));
#52779=CARTESIAN_POINT('Ctrl Pts',(22.3205169719132,18.8915573373479,38.5554831394366));
#52780=CARTESIAN_POINT('Ctrl Pts',(22.3331609340279,18.8957839982709,38.4772936480062));
#52781=CARTESIAN_POINT('Ctrl Pts',(22.3457969148797,18.9000079911938,38.3991535122201));
#52782=CARTESIAN_POINT('Ctrl Pts',(22.3545123308703,18.9042319841167,38.3203208603617));
#52783=CARTESIAN_POINT('Ctrl Pts',(22.3592471218585,18.9084559770396,38.2412213117851));
#52784=CARTESIAN_POINT('Ctrl Pts',(22.3639803983169,18.912678618823,38.1621470649863));
#52785=CARTESIAN_POINT('Ctrl Pts',(22.3647355502911,18.9169012606063,38.0828065586014));
#52786=CARTESIAN_POINT('Ctrl Pts',(22.3615044418532,18.9211239023896,38.0036298178498));
#52787=CARTESIAN_POINT('Ctrl Pts',(22.3582733609497,18.925346508189,37.924453751817));
#52788=CARTESIAN_POINT('Ctrl Pts',(22.3510561077185,18.9295691139883,37.8454419169673));
#52789=CARTESIAN_POINT('Ctrl Pts',(22.3398966161269,18.9337917197877,37.7670221227501));
#52790=CARTESIAN_POINT('Ctrl Pts',(22.3287260278533,18.9380185244265,37.6885243501131));
#52791=CARTESIAN_POINT('Ctrl Pts',(22.3136054370985,18.9422453290653,37.610620259233));
#52792=CARTESIAN_POINT('Ctrl Pts',(22.2946303442971,18.9464721337041,37.5337297253689));
#52793=CARTESIAN_POINT('Ctrl Pts',(22.2756460564984,18.9507009865784,37.4568019316996));
#52794=CARTESIAN_POINT('Ctrl Pts',(22.2528036809747,18.9549298394526,37.3808891229445));
#52795=CARTESIAN_POINT('Ctrl Pts',(22.2262485756469,18.9591586923269,37.306395740731));
#52796=CARTESIAN_POINT('Ctrl Pts',(22.1996457449755,18.9633951453765,37.2317684775848));
#52797=CARTESIAN_POINT('Ctrl Pts',(22.1693170318744,18.9676315984261,37.1585661722692));
#52798=CARTESIAN_POINT('Ctrl Pts',(22.1354558077887,18.9718680514757,37.0871728015691));
#52799=CARTESIAN_POINT('Ctrl Pts',(22.1046802740975,18.9757184469378,37.0222853338347));
#52800=CARTESIAN_POINT('Ctrl Pts',(22.070987433048,18.9795688423999,36.9588920675937));
#52801=CARTESIAN_POINT('Ctrl Pts',(22.0345537526132,18.9834192378619,36.8972608476367));
#52802=CARTESIAN_POINT('Ctrl Pts',(21.9944558171186,18.9876568802583,36.8294311732038));
#52803=CARTESIAN_POINT('Ctrl Pts',(21.9508868598386,18.9918945226547,36.763481597527));
#52804=CARTESIAN_POINT('Ctrl Pts',(21.9040484626433,18.996132165051,36.6997893398471));
#52805=CARTESIAN_POINT('Ctrl Pts',(21.8572774209003,19.0003637135514,36.6361886741322));
#52806=CARTESIAN_POINT('Ctrl Pts',(21.8072465515749,19.0045952620518,36.5748392544678));
#52807=CARTESIAN_POINT('Ctrl Pts',(21.7542022245776,19.0088268105522,36.5160918599278));
#52808=CARTESIAN_POINT('Ctrl Pts',(21.7012191652426,19.0130534714972,36.4574123202506));
#52809=CARTESIAN_POINT('Ctrl Pts',(21.6452298776808,19.0172801324422,36.4013291793598));
#52810=CARTESIAN_POINT('Ctrl Pts',(21.5865218050746,19.0215067933872,36.3481612508787));
#52811=CARTESIAN_POINT('Ctrl Pts',(21.5278507908333,19.0257307863321,36.295026883651));
#52812=CARTESIAN_POINT('Ctrl Pts',(21.4664647445317,19.029954779277,36.2448043901422));
#52813=CARTESIAN_POINT('Ctrl Pts',(21.4026880115855,19.0341787722219,36.1977758325964));
#52814=CARTESIAN_POINT('Ctrl Pts',(21.3389316790685,19.0384014140273,36.1507623181975));
#52815=CARTESIAN_POINT('Ctrl Pts',(21.2727865554974,19.0426240558326,36.1069409889715));
#52816=CARTESIAN_POINT('Ctrl Pts',(21.2046089464197,19.0468466976379,36.066552747892));
#52817=CARTESIAN_POINT('Ctrl Pts',(21.13643191833,19.0510693034592,36.0261648509883));
#52818=CARTESIAN_POINT('Ctrl Pts',(21.0662228432157,19.0552919092805,35.9892102217553));
#52819=CARTESIAN_POINT('Ctrl Pts',(20.9943645113807,19.0595145151017,35.9558848772963));
#52820=CARTESIAN_POINT('Ctrl Pts',(20.9224347256623,19.0637413197623,35.9225263950618));
#52821=CARTESIAN_POINT('Ctrl Pts',(20.8488528336226,19.0679681244228,35.8928046039927));
#52822=CARTESIAN_POINT('Ctrl Pts',(20.7740230392906,19.0721949290833,35.8668679448928));
#52823=CARTESIAN_POINT('Ctrl Pts',(20.6991569837533,19.0764237819792,35.840918717343));
#52824=CARTESIAN_POINT('Ctrl Pts',(20.623042271929,19.0806526348751,35.8187584069275));
#52825=CARTESIAN_POINT('Ctrl Pts',(20.5460973002749,19.084881487771,35.8004852295468));
#52826=CARTESIAN_POINT('Ctrl Pts',(20.4690140416526,19.0891179408419,35.7821792112638));
#52827=CARTESIAN_POINT('Ctrl Pts',(20.3910980037781,19.0933543939127,35.7677743702033));
#52828=CARTESIAN_POINT('Ctrl Pts',(20.3127765512825,19.0975908469836,35.7573175055361));
#52829=CARTESIAN_POINT('Ctrl Pts',(20.2415923448588,19.1014412422494,35.7478135498598));
#52830=CARTESIAN_POINT('Ctrl Pts',(20.1700735816283,19.1052916375152,35.741570175401));
#52831=CARTESIAN_POINT('Ctrl Pts',(20.0985410056413,19.109142032781,35.7385851463355));
#52832=CARTESIAN_POINT('Ctrl Pts',(20.019814160111,19.1133796751298,35.7352999029496));
#52833=CARTESIAN_POINT('Ctrl Pts',(19.9407750679908,19.1176173174786,35.7359497917051));
#52834=CARTESIAN_POINT('Ctrl Pts',(19.8618498944411,19.1218549598274,35.7405710459448));
#52835=CARTESIAN_POINT('Ctrl Pts',(19.7830382183881,19.1260865082802,35.7451856546395));
#52836=CARTESIAN_POINT('Ctrl Pts',(19.7043405996813,19.130318056733,35.7537602601678));
#52837=CARTESIAN_POINT('Ctrl Pts',(19.6261854034043,19.1345496051858,35.7662791323143));
#52838=CARTESIAN_POINT('Ctrl Pts',(19.5481204785333,19.1387762660835,35.7787835448183));
#52839=CARTESIAN_POINT('Ctrl Pts',(19.4705971915837,19.1430029269812,35.7952230967783));
#52840=CARTESIAN_POINT('Ctrl Pts',(19.3940394505008,19.1472295878789,35.815530203012));
#52841=CARTESIAN_POINT('Ctrl Pts',(19.3175300350472,19.1514535807767,35.835824490768));
#52842=CARTESIAN_POINT('Ctrl Pts',(19.2419854076235,19.1556775736744,35.8599813671734));
#52843=CARTESIAN_POINT('Ctrl Pts',(19.1678187338312,19.1599015665722,35.8878822858768));
#52844=CARTESIAN_POINT('Ctrl Pts',(19.0936757839217,19.1641242083306,35.9157742798422));
#52845=CARTESIAN_POINT('Ctrl Pts',(19.0209103508,19.168346850089,35.9474077729394));
#52846=CARTESIAN_POINT('Ctrl Pts',(18.949918469925,19.1725694918474,35.982615004045));
#52847=CARTESIAN_POINT('Ctrl Pts',(18.8789271940157,19.176792097622,36.017821935128));
#52848=CARTESIAN_POINT('Ctrl Pts',(18.8097098596318,19.1810147033967,36.0566023341128));
#52849=CARTESIAN_POINT('Ctrl Pts',(18.7426392655245,19.1852373091714,36.0987417896985));
#52850=CARTESIAN_POINT('Ctrl Pts',(18.6755019783107,19.1894641137861,36.1409231475699));
#52851=CARTESIAN_POINT('Ctrl Pts',(18.6105160932173,19.1936909184008,36.1864699840429));
#52852=CARTESIAN_POINT('Ctrl Pts',(18.548026155031,19.1979177230155,36.2351240270662));
#52853=CARTESIAN_POINT('Ctrl Pts',(18.4855059353114,19.2021465758659,36.2838016469895));
#52854=CARTESIAN_POINT('Ctrl Pts',(18.4254844273257,19.2063754287164,36.3355891663651));
#52855=CARTESIAN_POINT('Ctrl Pts',(18.3682717692599,19.2106042815668,36.3901890683746));
#52856=CARTESIAN_POINT('Ctrl Pts',(18.3109562874994,19.2148407345933,36.4448870983832));
#52857=CARTESIAN_POINT('Ctrl Pts',(18.2564600654632,19.2190771876198,36.5024072692392));
#52858=CARTESIAN_POINT('Ctrl Pts',(18.2050549912046,19.2233136406463,36.5624165530611));
#52859=CARTESIAN_POINT('Ctrl Pts',(18.1583343324713,19.2271640363309,36.6169573413142));
#52860=CARTESIAN_POINT('Ctrl Pts',(18.1141667590309,19.2310144320155,36.6735536290899));
#52861=CARTESIAN_POINT('Ctrl Pts',(18.0727249877601,19.2348648277001,36.7319351374677));
#52862=CARTESIAN_POINT('Ctrl Pts',(18.0266912746906,19.2391418652087,36.7967855896276));
#52863=CARTESIAN_POINT('Ctrl Pts',(17.9838497684247,19.2434189027173,36.8640810570083));
#52864=CARTESIAN_POINT('Ctrl Pts',(17.9444667914954,19.2476959402259,36.9334779600732));
#52865=CARTESIAN_POINT('Ctrl Pts',(17.9051427866996,19.2519665732916,37.0027709481031));
#52866=CARTESIAN_POINT('Ctrl Pts',(17.8692672489419,19.2562372063573,37.0741587279191));
#52867=CARTESIAN_POINT('Ctrl Pts',(17.8370642044437,19.260507839423,37.1472675164553));
#52868=CARTESIAN_POINT('Ctrl Pts',(17.8041745185864,19.2648695319937,37.2219351488433));
#52869=CARTESIAN_POINT('Ctrl Pts',(17.7751160414248,19.2692312245644,37.2983976442449));
#52870=CARTESIAN_POINT('Ctrl Pts',(17.7500787937588,19.2735929171352,37.376228622695));
#52871=CARTESIAN_POINT('Ctrl Pts',(17.7256186167874,19.2778540792884,37.4522657147962));
#52872=CARTESIAN_POINT('Ctrl Pts',(17.7049964412684,19.2821152414415,37.5296084235428));
#52873=CARTESIAN_POINT('Ctrl Pts',(17.688340841097,19.2863764035947,37.6078390771711));
#52874=CARTESIAN_POINT('Ctrl Pts',(17.6710958262146,19.2907883613742,37.688838186912));
#52875=CARTESIAN_POINT('Ctrl Pts',(17.6581035610096,19.2952003191537,37.7707887872257));
#52876=CARTESIAN_POINT('Ctrl Pts',(17.6494498003634,19.2996122769332,37.8532122371583));
#52877=CARTESIAN_POINT('Ctrl Pts',(17.6407960397172,19.3040242347127,37.9356356870909));
#52878=CARTESIAN_POINT('Ctrl Pts',(17.6364808544133,19.3084361924922,38.0185314454336));
#52879=CARTESIAN_POINT('Ctrl Pts',(17.6365304226749,19.3128481502717,38.1014134916261));
#52880=CARTESIAN_POINT('',(17.6365301782972,20.106598150223,38.1009180413976));
#52881=CARTESIAN_POINT('Ctrl Pts',(17.6365304226752,19.3128481502999,38.1014134921557));
#52882=CARTESIAN_POINT('Ctrl Pts',(17.6365835982443,19.3175811845135,38.1903272079986));
#52883=CARTESIAN_POINT('Ctrl Pts',(17.6416582714512,19.3223142187271,38.2790563289598));
#52884=CARTESIAN_POINT('Ctrl Pts',(17.6516677115378,19.3270472529406,38.3670690994213));
#52885=CARTESIAN_POINT('Ctrl Pts',(17.6617198026594,19.3318004549964,38.4554568994273));
#52886=CARTESIAN_POINT('Ctrl Pts',(17.6767486737287,19.3365536570522,38.5431219950087));
#52887=CARTESIAN_POINT('Ctrl Pts',(17.6966167680631,19.3413068591079,38.6295433199767));
#52888=CARTESIAN_POINT('Ctrl Pts',(17.7165895218556,19.3460850996774,38.7164198878526));
#52889=CARTESIAN_POINT('Ctrl Pts',(17.7414524899748,19.3508633402468,38.8020393177264));
#52890=CARTESIAN_POINT('Ctrl Pts',(17.7710177346128,19.3556415808162,38.8858934415614));
#52891=CARTESIAN_POINT('Ctrl Pts',(17.7812189048112,19.3572902614172,38.9148264065869));
#52892=CARTESIAN_POINT('Ctrl Pts',(17.791979480223,19.3589389420181,38.943549408275));
#52893=CARTESIAN_POINT('Ctrl Pts',(17.803290462004,19.3605876226191,38.9720422275196));
#52894=CARTESIAN_POINT('Ctrl Pts',(17.8323633443828,19.3648252651262,39.0452779906548));
#52895=CARTESIAN_POINT('Ctrl Pts',(17.8651571983814,19.3690629076334,39.1171957494667));
#52896=CARTESIAN_POINT('Ctrl Pts',(17.9015314954163,19.3733005501405,39.1873915468544));
#52897=CARTESIAN_POINT('Ctrl Pts',(17.9378534847901,19.377532098752,39.2574863999413));
#52898=CARTESIAN_POINT('Ctrl Pts',(17.9777454782337,19.3817636473636,39.325863796429));
#52899=CARTESIAN_POINT('Ctrl Pts',(18.0210185951564,19.3859951959751,39.3921389399687));
#52900=CARTESIAN_POINT('Ctrl Pts',(18.0642417304364,19.3902218570314,39.4583375338909));
#52901=CARTESIAN_POINT('Ctrl Pts',(18.110837973413,19.3944485180877,39.5224383097033));
#52902=CARTESIAN_POINT('Ctrl Pts',(18.1605729027309,19.3986751791439,39.584081667137));
#52903=CARTESIAN_POINT('Ctrl Pts',(18.2102764378123,19.4028991722001,39.6456861133635));
#52904=CARTESIAN_POINT('Ctrl Pts',(18.2631144331148,19.4071231652563,39.7048358562903));
#52905=CARTESIAN_POINT('Ctrl Pts',(18.3188103033576,19.4113471583124,39.7612018675656));
#52906=CARTESIAN_POINT('Ctrl Pts',(18.3744883580162,19.4155698002288,39.8175498488969));
#52907=CARTESIAN_POINT('Ctrl Pts',(18.4330221430347,19.4197924421453,39.8711155336049));
#52908=CARTESIAN_POINT('Ctrl Pts',(18.49409710648,19.4240150840617,39.9216055874387));
#52909=CARTESIAN_POINT('Ctrl Pts',(18.5551715494589,19.4282376899937,39.9720952110084));
#52910=CARTESIAN_POINT('Ctrl Pts',(18.6187867655975,19.4324602959258,40.0195089582365));
#52911=CARTESIAN_POINT('Ctrl Pts',(18.6845950662279,19.4366829018579,40.0635937209891));
#52912=CARTESIAN_POINT('Ctrl Pts',(18.7504688047415,19.4409097066279,40.1077223203631));
#52913=CARTESIAN_POINT('Ctrl Pts',(18.8185395934184,19.445136511398,40.1485150615237));
#52914=CARTESIAN_POINT('Ctrl Pts',(18.8884311983215,19.4493633161681,40.1857625080615));
#52915=CARTESIAN_POINT('Ctrl Pts',(18.9583566714606,19.453592169173,40.2230280040533));
#52916=CARTESIAN_POINT('Ctrl Pts',(19.0301042937365,19.4578210221779,40.2567445833614));
#52917=CARTESIAN_POINT('Ctrl Pts',(19.1032760080623,19.4620498751829,40.2867502196601));
#52918=CARTESIAN_POINT('Ctrl Pts',(19.1765792279461,19.4662863283606,40.3168097826431));
#52919=CARTESIAN_POINT('Ctrl Pts',(19.2513112106449,19.4705227815383,40.3431449203859));
#52920=CARTESIAN_POINT('Ctrl Pts',(19.3270570515768,19.4747592347161,40.3656430056537));
#52921=CARTESIAN_POINT('Ctrl Pts',(19.395900336271,19.4786096289901,40.3860908886016));
#52922=CARTESIAN_POINT('Ctrl Pts',(19.4655806860639,19.4824600232642,40.4033697608079));
#52923=CARTESIAN_POINT('Ctrl Pts',(19.5357809044098,19.4863104175383,40.4174319994747));
#52924=CARTESIAN_POINT('Ctrl Pts',(19.6130414087937,19.490548059681,40.4329085275791));
#52925=CARTESIAN_POINT('Ctrl Pts',(19.6912217391311,19.4947857018238,40.4445462172815));
#52926=CARTESIAN_POINT('Ctrl Pts',(19.7699065342695,19.4990233439665,40.4522430652312));
#52927=CARTESIAN_POINT('Ctrl Pts',(19.8484781775839,19.5032548922135,40.4599288448113));
#52928=CARTESIAN_POINT('Ctrl Pts',(19.9275523823503,19.5074864404605,40.463684991685));
#52929=CARTESIAN_POINT('Ctrl Pts',(20.0067035410302,19.5117179887075,40.4634604933101));
#52930=CARTESIAN_POINT('Ctrl Pts',(20.0857632779596,19.5159446494006,40.463236254237));
#52931=CARTESIAN_POINT('Ctrl Pts',(20.1648993257691,19.5201713100938,40.4590405081321));
#52932=CARTESIAN_POINT('Ctrl Pts',(20.2436824236344,19.5243979707869,40.4508741602459));
#52933=CARTESIAN_POINT('Ctrl Pts',(20.3224157911697,19.5286219634811,40.4427129672112));
#52934=CARTESIAN_POINT('Ctrl Pts',(20.4007961859249,19.5328459561752,40.4305861954623));
#52935=CARTESIAN_POINT('Ctrl Pts',(20.4783970415405,19.5370699488693,40.4145467615811));
#52936=CARTESIAN_POINT('Ctrl Pts',(20.5559730747929,19.5412925904252,40.3985124582702));
#52937=CARTESIAN_POINT('Ctrl Pts',(20.6327696053325,19.5455152319811,40.3785680729797));
#52938=CARTESIAN_POINT('Ctrl Pts',(20.7083693428251,19.549737873537,40.3548178008534));
#52939=CARTESIAN_POINT('Ctrl Pts',(20.783968436111,19.5539604791105,40.33106773111));
#52940=CARTESIAN_POINT('Ctrl Pts',(20.858370309833,19.5581830846841,40.3035119808758));
#52941=CARTESIAN_POINT('Ctrl Pts',(20.9311733805399,19.5624056902577,40.2723044391323));
#52942=CARTESIAN_POINT('Ctrl Pts',(21.0040488446322,19.5666324946749,40.2410658654615));
#52943=CARTESIAN_POINT('Ctrl Pts',(21.0753218982057,19.5708592990922,40.2061684319789));
#52944=CARTESIAN_POINT('Ctrl Pts',(21.1446120543996,19.5750861035094,40.1678137454382));
#52945=CARTESIAN_POINT('Ctrl Pts',(21.2139357874224,19.579314956164,40.12944047287));
#52946=CARTESIAN_POINT('Ctrl Pts',(21.2812743101845,19.5835438088187,40.087606857488));
#52947=CARTESIAN_POINT('Ctrl Pts',(21.346275027494,19.5877726614733,40.0425586197709));
#52948=CARTESIAN_POINT('Ctrl Pts',(21.4113925654325,19.5920091143091,39.9974294204323));
#52949=CARTESIAN_POINT('Ctrl Pts',(21.4741635305669,19.5962455671449,39.949074341736));
#52950=CARTESIAN_POINT('Ctrl Pts',(21.5342675963127,19.6004820199807,39.8977801266575));
#52951=CARTESIAN_POINT('Ctrl Pts',(21.5888945573553,19.6043324174729,39.8511602008002));
#52952=CARTESIAN_POINT('Ctrl Pts',(21.6413187786523,19.6081828149651,39.8021130789163));
#52953=CARTESIAN_POINT('Ctrl Pts',(21.691327649107,19.6120332124573,39.750878924775));
#52954=CARTESIAN_POINT('Ctrl Pts',(21.7463660469705,19.6162708548432,39.6944920131293));
#52955=CARTESIAN_POINT('Ctrl Pts',(21.7986848613811,19.6205084972291,39.6352438729319));
#52956=CARTESIAN_POINT('Ctrl Pts',(21.8479724291805,19.624746139615,39.5734274131726));
#52957=CARTESIAN_POINT('Ctrl Pts',(21.8971891194963,19.6289776881025,39.5116998479422));
#52958=CARTESIAN_POINT('Ctrl Pts',(21.9433829300499,19.63320923659,39.447411661293));
#52959=CARTESIAN_POINT('Ctrl Pts',(21.9862793947481,19.6374407850776,39.3808921136844));
#52960=CARTESIAN_POINT('Ctrl Pts',(22.0291263128098,19.6416674460062,39.3144493980451));
#52961=CARTESIAN_POINT('Ctrl Pts',(22.068683200752,19.6458941069349,39.2457808351275));
#52962=CARTESIAN_POINT('Ctrl Pts',(22.104717156022,19.6501207678636,39.1752470107128));
#52963=CARTESIAN_POINT('Ctrl Pts',(22.1407283655185,19.65434476079,39.1047577094813));
#52964=CARTESIAN_POINT('Ctrl Pts',(22.1732208436059,19.6585687537165,39.0324059001456));
#52965=CARTESIAN_POINT('Ctrl Pts',(22.202006785044,19.662792746643,38.9585782198032));
#52966=CARTESIAN_POINT('Ctrl Pts',(22.2307835186341,19.6670153884278,38.8847741549488));
#52967=CARTESIAN_POINT('Ctrl Pts',(22.255855899816,19.6712380302126,38.8094955930018));
#52968=CARTESIAN_POINT('Ctrl Pts',(22.2770841885425,19.6754606719974,38.7331493024475));
#52969=CARTESIAN_POINT('Ctrl Pts',(22.298312296358,19.6796832777962,38.656803662529));
#52970=CARTESIAN_POINT('Ctrl Pts',(22.3156962526527,19.6839058835949,38.5793907641174));
#52971=CARTESIAN_POINT('Ctrl Pts',(22.329146553743,19.6881284893937,38.5013312498262));
#52972=CARTESIAN_POINT('Ctrl Pts',(22.3426102294212,19.6923552940287,38.4231941154261));
#52973=CARTESIAN_POINT('Ctrl Pts',(22.3521323568461,19.6965820986637,38.3444095438386));
#52974=CARTESIAN_POINT('Ctrl Pts',(22.35767494485,19.7008089032988,38.2654064549122));
#52975=CARTESIAN_POINT('Ctrl Pts',(22.3632202186926,19.7050377561675,38.1863650825061));
#52976=CARTESIAN_POINT('Ctrl Pts',(22.3647821022416,19.7092666090362,38.1071054510986));
#52977=CARTESIAN_POINT('Ctrl Pts',(22.3623747923296,19.713495461905,38.0280570957931));
#52978=CARTESIAN_POINT('Ctrl Pts',(22.3599631559557,19.7177319149462,37.9488666733233));
#52979=CARTESIAN_POINT('Ctrl Pts',(22.3535681106041,19.7219683679874,37.8698887540043));
#52980=CARTESIAN_POINT('Ctrl Pts',(22.3432558305,19.7262048210286,37.7915481338562));
#52981=CARTESIAN_POINT('Ctrl Pts',(22.3338832832305,19.7300552164779,37.720346502592));
#52982=CARTESIAN_POINT('Ctrl Pts',(22.321275613787,19.7339056119271,37.6496714687195));
#52983=CARTESIAN_POINT('Ctrl Pts',(22.3055185558231,19.7377560073764,37.5798321139715));
#52984=CARTESIAN_POINT('Ctrl Pts',(22.2881767552031,19.741993650618,37.5029687700501));
#52985=CARTESIAN_POINT('Ctrl Pts',(22.2669543952425,19.7462312938597,37.4268293289515));
#52986=CARTESIAN_POINT('Ctrl Pts',(22.2419275386174,19.7504689371013,37.3518346756972));
#52987=CARTESIAN_POINT('Ctrl Pts',(22.2169366715643,19.7547004864507,37.2769478676078));
#52988=CARTESIAN_POINT('Ctrl Pts',(22.1881523199338,19.7589320358002,37.2032030190581));
#52989=CARTESIAN_POINT('Ctrl Pts',(22.1557012881523,19.7631635851496,37.1310095990369));
#52990=CARTESIAN_POINT('Ctrl Pts',(22.1232877381884,19.7673902469453,37.0588995643644));
#52991=CARTESIAN_POINT('Ctrl Pts',(22.0872161155294,19.771616908741,36.9883378225812));
#52992=CARTESIAN_POINT('Ctrl Pts',(22.0476621269062,19.7758435705367,36.9197160278416));
#52993=CARTESIAN_POINT('Ctrl Pts',(22.0081331059825,19.7800675643329,36.8511375492987));
#52994=CARTESIAN_POINT('Ctrl Pts',(21.9651263157194,19.7842915581291,36.7844969922669));
#52995=CARTESIAN_POINT('Ctrl Pts',(21.9188638645174,19.7885155519253,36.7201623608739));
#52996=CARTESIAN_POINT('Ctrl Pts',(21.8726162114092,19.7927381945814,36.655848308371));
#52997=CARTESIAN_POINT('Ctrl Pts',(21.8231152388519,19.7969608372374,36.5938390970891));
#52998=CARTESIAN_POINT('Ctrl Pts',(21.7706261064023,19.8011834798935,36.5344733690459));
#52999=CARTESIAN_POINT('Ctrl Pts',(21.7181374212705,19.8054060865637,36.4751081469234));
#53000=CARTESIAN_POINT('Ctrl Pts',(21.662660938458,19.809628693234,36.4183867134876));
#53001=CARTESIAN_POINT('Ctrl Pts',(21.604500801512,19.8138512999042,36.3646131212761));
#53002=CARTESIAN_POINT('Ctrl Pts',(21.5462828319092,19.8180781054051,36.3107860582532));
#53003=CARTESIAN_POINT('Ctrl Pts',(21.4853762227442,19.8223049109059,36.2599130106039));
#53004=CARTESIAN_POINT('Ctrl Pts',(21.4221201011581,19.8265317164068,36.2122593242762));
#53005=CARTESIAN_POINT('Ctrl Pts',(21.3588333268225,19.8307605701396,36.1645825458514));
#53006=CARTESIAN_POINT('Ctrl Pts',(21.2931951606116,19.8349894238724,36.1201284997407));
#53007=CARTESIAN_POINT('Ctrl Pts',(21.225573653567,19.8392182776052,36.0791190879761));
#53008=CARTESIAN_POINT('Ctrl Pts',(21.1578306161347,19.8434547314975,36.0380359734811));
#53009=CARTESIAN_POINT('Ctrl Pts',(21.0880975292011,19.8476911853897,36.0004100861761));
#53010=CARTESIAN_POINT('Ctrl Pts',(21.0167667614865,19.8519276392819,35.9664171462921));
#53011=CARTESIAN_POINT('Ctrl Pts',(20.9519363359535,19.8557780269531,35.935521968399));
#53012=CARTESIAN_POINT('Ctrl Pts',(20.8857866695396,19.8596284146243,35.9076272632682));
#53013=CARTESIAN_POINT('Ctrl Pts',(20.8186237068181,19.8634788022955,35.8828293553415));
#53014=CARTESIAN_POINT('Ctrl Pts',(20.7447058271781,19.867716442818,35.8555373971078));
#53015=CARTESIAN_POINT('Ctrl Pts',(20.6692828805866,19.8719540833406,35.8318947553759));
#53016=CARTESIAN_POINT('Ctrl Pts',(20.5927493369304,19.8761917238632,35.8120667263951));
#53017=CARTESIAN_POINT('Ctrl Pts',(20.5163258515487,19.8804232704905,35.7922672109072));
#53018=CARTESIAN_POINT('Ctrl Pts',(20.438795390803,19.8846548171177,35.7762715309429));
#53019=CARTESIAN_POINT('Ctrl Pts',(20.3605704686141,19.888886363745,35.7641962030035));
#53020=CARTESIAN_POINT('Ctrl Pts',(20.2824358982314,19.8931130228266,35.7521348223798));
#53021=CARTESIAN_POINT('Ctrl Pts',(20.2036089213631,19.8973396819081,35.7439848664458));
#53022=CARTESIAN_POINT('Ctrl Pts',(20.1245137269355,19.9015663409897,35.7398121319046));
#53023=CARTESIAN_POINT('Ctrl Pts',(20.0454684597556,19.9057903320779,35.735642031318));
#53024=CARTESIAN_POINT('Ctrl Pts',(19.9661557779702,19.9100143231661,35.7354441936097));
#53025=CARTESIAN_POINT('Ctrl Pts',(19.8870052893639,19.9142383142543,35.739232617078));
#53026=CARTESIAN_POINT('Ctrl Pts',(19.8078801186683,19.9184609542121,35.7430198287413));
#53027=CARTESIAN_POINT('Ctrl Pts',(19.7289175060268,19.92268359417,35.7507907471139));
#53028=CARTESIAN_POINT('Ctrl Pts',(19.6505458625885,19.9269062341278,35.7625072734347));
#53029=CARTESIAN_POINT('Ctrl Pts',(19.5721748867913,19.9311288381133,35.7742236999433));
#53030=CARTESIAN_POINT('Ctrl Pts',(19.4943953335967,19.9353514420988,35.7898855968436));
#53031=CARTESIAN_POINT('Ctrl Pts',(19.4176278185341,19.9395740460843,35.8094033346845));
#53032=CARTESIAN_POINT('Ctrl Pts',(19.3407839674375,19.9438008489402,35.8289404805614));
#53033=CARTESIAN_POINT('Ctrl Pts',(19.2649546200374,19.9480276517961,35.852341010371));
#53034=CARTESIAN_POINT('Ctrl Pts',(19.1905469649741,19.9522544546519,35.8794648786864));
#53035=CARTESIAN_POINT('Ctrl Pts',(19.1161032530027,19.9564833057573,35.9066018908486));
#53036=CARTESIAN_POINT('Ctrl Pts',(19.0430830381416,19.9607121568626,35.9374656531096));
#53037=CARTESIAN_POINT('Ctrl Pts',(18.9718728096299,19.964941007968,35.9718682086577));
#53038=CARTESIAN_POINT('Ctrl Pts',(18.9005345999336,19.9691774592929,36.0063325935231));
#53039=CARTESIAN_POINT('Ctrl Pts',(18.831013288595,19.9734139106179,36.0443482541861));
#53040=CARTESIAN_POINT('Ctrl Pts',(18.763669861402,19.9776503619428,36.0856816961329));
#53041=CARTESIAN_POINT('Ctrl Pts',(18.702462991796,19.9815007737,36.1232486970571));
#53042=CARTESIAN_POINT('Ctrl Pts',(18.6430550338593,19.9853511854573,36.1635556649019));
#53043=CARTESIAN_POINT('Ctrl Pts',(18.5856933321888,19.9892015972146,36.2063983813155));
#53044=CARTESIAN_POINT('Ctrl Pts',(18.5231591640587,19.9933992114621,36.2531043463293));
#53045=CARTESIAN_POINT('Ctrl Pts',(18.4628128069114,19.9975968257097,36.303007336959));
#53046=CARTESIAN_POINT('Ctrl Pts',(18.4050040176627,20.0017944399573,36.3558732106788));
#53047=CARTESIAN_POINT('Ctrl Pts',(18.344864939825,20.0061612612184,36.4108701226693));
#53048=CARTESIAN_POINT('Ctrl Pts',(18.287472821428,20.0105280824795,36.4690736301524));
#53049=CARTESIAN_POINT('Ctrl Pts',(18.2331876128407,20.0148949037405,36.5301705731258));
#53050=CARTESIAN_POINT('Ctrl Pts',(18.1811422599262,20.0190815460978,36.5887466022467));
#53051=CARTESIAN_POINT('Ctrl Pts',(18.1319528489829,20.0232681884551,36.649981609482));
#53052=CARTESIAN_POINT('Ctrl Pts',(18.0859008250745,20.0274548308124,36.7135603909836));
#53053=CARTESIAN_POINT('Ctrl Pts',(18.0398760992656,20.0316389914682,36.77710148511));
#53054=CARTESIAN_POINT('Ctrl Pts',(17.9969853508088,20.0358231521239,36.8429832103659));
#53055=CARTESIAN_POINT('Ctrl Pts',(17.9574694509647,20.0400073127797,36.9108577052523));
#53056=CARTESIAN_POINT('Ctrl Pts',(17.9179640881504,20.0441903577168,36.9787141012071));
#53057=CARTESIAN_POINT('Ctrl Pts',(17.881832027718,20.0483734026539,37.0485617982512));
#53058=CARTESIAN_POINT('Ctrl Pts',(17.8492696610642,20.0525564475911,37.1200257911143));
#53059=CARTESIAN_POINT('Ctrl Pts',(17.8167053584166,20.0567397412309,37.1914940328654));
#53060=CARTESIAN_POINT('Ctrl Pts',(17.787711366745,20.0609230348707,37.2645783245426));
#53061=CARTESIAN_POINT('Ctrl Pts',(17.7624364599671,20.0651063285106,37.338882502359));
#53062=CARTESIAN_POINT('Ctrl Pts',(17.7371370902075,20.069293671061,37.4132585974235));
#53063=CARTESIAN_POINT('Ctrl Pts',(17.7155641412164,20.0734810136113,37.4888564804706));
#53064=CARTESIAN_POINT('Ctrl Pts',(17.6978166147843,20.0776683561617,37.5652644562621));
#53065=CARTESIAN_POINT('Ctrl Pts',(17.6800588871303,20.0818581055832,37.6417163511154));
#53066=CARTESIAN_POINT('Ctrl Pts',(17.6661310406482,20.0860478550048,37.7189787943313));
#53067=CARTESIAN_POINT('Ctrl Pts',(17.656080564927,20.0902376044263,37.7966320340127));
#53068=CARTESIAN_POINT('Ctrl Pts',(17.6460147322593,20.0944337557099,37.8744039264516));
#53069=CARTESIAN_POINT('Ctrl Pts',(17.639838124863,20.0986299069934,37.9525673304946));
#53070=CARTESIAN_POINT('Ctrl Pts',(17.6375461898729,20.1028260582769,38.0307003902189));
#53071=CARTESIAN_POINT('Ctrl Pts',(17.6368594185172,20.104083422259,38.0541127241566));
#53072=CARTESIAN_POINT('Ctrl Pts',(17.6365210907241,20.105340786241,38.0775223592207));
#53073=CARTESIAN_POINT('Ctrl Pts',(17.6365301782972,20.106598150223,38.1009180413976));
#53074=CARTESIAN_POINT('',(17.6365309629368,20.9003481398077,38.0978665184563));
#53075=CARTESIAN_POINT('Ctrl Pts',(17.6365301782975,20.1065981502717,38.1009180423036));
#53076=CARTESIAN_POINT('Ctrl Pts',(17.6365502375663,20.1093735642257,38.152559972328));
#53077=CARTESIAN_POINT('Ctrl Pts',(17.6382627322631,20.1121489781797,38.2041669172878));
#53078=CARTESIAN_POINT('Ctrl Pts',(17.6416616041977,20.1149243921337,38.2556613368326));
#53079=CARTESIAN_POINT('Ctrl Pts',(17.6468511805558,20.1191620400701,38.3342857238022));
#53080=CARTESIAN_POINT('Ctrl Pts',(17.6559866728642,20.1233996880065,38.4127978873952));
#53081=CARTESIAN_POINT('Ctrl Pts',(17.6690583310005,20.1276373359429,38.4907702350764));
#53082=CARTESIAN_POINT('Ctrl Pts',(17.6821111916988,20.131868890014,38.5686304561741));
#53083=CARTESIAN_POINT('Ctrl Pts',(17.6990889004778,20.136100444085,38.6459519444627));
#53084=CARTESIAN_POINT('Ctrl Pts',(17.7199298079772,20.1403319981561,38.7223105015577));
#53085=CARTESIAN_POINT('Ctrl Pts',(17.7407466437816,20.1445586646915,38.7985808628823));
#53086=CARTESIAN_POINT('Ctrl Pts',(17.7654176882308,20.1487853312269,38.8738900533054));
#53087=CARTESIAN_POINT('Ctrl Pts',(17.793830215714,20.1530119977623,38.9478238754621));
#53088=CARTESIAN_POINT('Ctrl Pts',(17.8222248084113,20.157235996307,39.0217110285122));
#53089=CARTESIAN_POINT('Ctrl Pts',(17.8543560286524,20.1614599948517,39.0942241000917));
#53090=CARTESIAN_POINT('Ctrl Pts',(17.8900616382825,20.1656839933964,39.1649650466813));
#53091=CARTESIAN_POINT('Ctrl Pts',(17.925755826695,20.169906640803,39.2356833652371));
#53092=CARTESIAN_POINT('Ctrl Pts',(17.9650219229629,20.1741292882097,39.3046302662762));
#53093=CARTESIAN_POINT('Ctrl Pts',(18.0076505987758,20.1783519356164,39.3714300233758));
#53094=CARTESIAN_POINT('Ctrl Pts',(18.050278911258,20.1825745470328,39.4382292111312));
#53095=CARTESIAN_POINT('Ctrl Pts',(18.0962694929201,20.1867971584492,39.5028808969397));
#53096=CARTESIAN_POINT('Ctrl Pts',(18.1453691309369,20.1910197698656,39.5650374672404));
#53097=CARTESIAN_POINT('Ctrl Pts',(18.1945175916058,20.1952465800724,39.6272558434675));
#53098=CARTESIAN_POINT('Ctrl Pts',(18.2467809926973,20.1994733902792,39.6869737795948));
#53099=CARTESIAN_POINT('Ctrl Pts',(18.3018655490479,20.203700200486,39.7438764635427));
#53100=CARTESIAN_POINT('Ctrl Pts',(18.3569767981394,20.2079290589103,39.8008067212554));
#53101=CARTESIAN_POINT('Ctrl Pts',(18.414911582831,20.2121579173346,39.8549186887404));
#53102=CARTESIAN_POINT('Ctrl Pts',(18.475340795717,20.2163867757588,39.9059359766324));
#53103=CARTESIAN_POINT('Ctrl Pts',(18.5358786116362,20.2206232342631,39.9570449525001));
#53104=CARTESIAN_POINT('Ctrl Pts',(18.5989194393215,20.2248596927673,40.0050478512135));
#53105=CARTESIAN_POINT('Ctrl Pts',(18.6641029740525,20.2290961512716,40.0497101263943));
#53106=CARTESIAN_POINT('Ctrl Pts',(18.7233456442571,20.2329464965319,40.0903018563465));
#53107=CARTESIAN_POINT('Ctrl Pts',(18.7843576564607,20.2367968417922,40.1281345668769));
#53108=CARTESIAN_POINT('Ctrl Pts',(18.8468517562158,20.2406471870526,40.1630655754865));
#53109=CARTESIAN_POINT('Ctrl Pts',(18.915631758473,20.2448848151924,40.2015100824148));
#53110=CARTESIAN_POINT('Ctrl Pts',(18.9864655113814,20.2491224433323,40.2365834365342));
#53111=CARTESIAN_POINT('Ctrl Pts',(19.0589890180882,20.2533600714721,40.2680610629826));
#53112=CARTESIAN_POINT('Ctrl Pts',(19.1314082327038,20.2575916057106,40.2994934231769));
#53113=CARTESIAN_POINT('Ctrl Pts',(19.205511949012,20.261823139949,40.3273401393661));
#53114=CARTESIAN_POINT('Ctrl Pts',(19.2809107665492,20.2660546741875,40.3514220206872));
#53115=CARTESIAN_POINT('Ctrl Pts',(19.3562224971132,20.2702813209287,40.3754760870077));
#53116=CARTESIAN_POINT('Ctrl Pts',(19.4328259119544,20.27450796767,40.3957738180204));
#53117=CARTESIAN_POINT('Ctrl Pts',(19.5103121972968,20.2787346144113,40.412184312892));
#53118=CARTESIAN_POINT('Ctrl Pts',(19.5877495714838,20.2829585931943,40.4285844490755));
#53119=CARTESIAN_POINT('Ctrl Pts',(19.6660682526112,20.2871825719772,40.4411021225969));
#53120=CARTESIAN_POINT('Ctrl Pts',(19.7448460262413,20.2914065507602,40.449656760162));
#53121=CARTESIAN_POINT('Ctrl Pts',(19.823598602073,20.2956291784646,40.4582086614473));
#53122=CARTESIAN_POINT('Ctrl Pts',(19.9028095131013,20.299851806169,40.4627999934345));
#53123=CARTESIAN_POINT('Ctrl Pts',(19.9820496330305,20.3040744338734,40.4634018332111));
#53124=CARTESIAN_POINT('Ctrl Pts',(20.0612890792022,20.3082970256739,40.4640036678705));
#53125=CARTESIAN_POINT('Ctrl Pts',(20.1405572650074,20.3125196174744,40.460616075635));
#53126=CARTESIAN_POINT('Ctrl Pts',(20.2194247591814,20.3167422092749,40.4532622497202));
#53127=CARTESIAN_POINT('Ctrl Pts',(20.2983706813693,20.3209690001372,40.4459011109578));
#53128=CARTESIAN_POINT('Ctrl Pts',(20.3769146481654,20.3251957909996,40.4345659037171));
#53129=CARTESIAN_POINT('Ctrl Pts',(20.4546326594229,20.329422581862,40.4193317110509));
#53130=CARTESIAN_POINT('Ctrl Pts',(20.5323883334244,20.3336514210596,40.4040901357781));
#53131=CARTESIAN_POINT('Ctrl Pts',(20.6093167990298,20.3378802602573,40.3849459243705));
#53132=CARTESIAN_POINT('Ctrl Pts',(20.6850070606099,20.3421090994549,40.3620247053944));
#53133=CARTESIAN_POINT('Ctrl Pts',(20.7608333604773,20.3463455391553,40.3390622900568));
#53134=CARTESIAN_POINT('Ctrl Pts',(20.8354165674048,20.3505819788557,40.3123094618713));
#53135=CARTESIAN_POINT('Ctrl Pts',(20.9083638047661,20.354818418556,40.281940796422));
#53136=CARTESIAN_POINT('Ctrl Pts',(20.9746659120371,20.3586689396946,40.2543385651775));
#53137=CARTESIAN_POINT('Ctrl Pts',(21.0396165636773,20.3625194608332,40.2237499834598));
#53138=CARTESIAN_POINT('Ctrl Pts',(21.1029396668827,20.3663699819718,40.1903383774204));
#53139=CARTESIAN_POINT('Ctrl Pts',(21.1726292584982,20.3706076335093,40.1535675771558));
#53140=CARTESIAN_POINT('Ctrl Pts',(21.2406088047282,20.3748452850467,40.1132388818508));
#53141=CARTESIAN_POINT('Ctrl Pts',(21.3064917779805,20.3790829365842,40.0695353957138));
#53142=CARTESIAN_POINT('Ctrl Pts',(21.3722800075188,20.3833144941215,40.0258947578422));
#53143=CARTESIAN_POINT('Ctrl Pts',(21.4359772641782,20.3875460516589,39.978889224043));
#53144=CARTESIAN_POINT('Ctrl Pts',(21.4972212636356,20.3917776091963,39.9287479128129));
#53145=CARTESIAN_POINT('Ctrl Pts',(21.5583945218872,20.3960042789816,39.8786645183885));
#53146=CARTESIAN_POINT('Ctrl Pts',(21.6171197933096,20.4002309487669,39.8254528399105));
#53147=CARTESIAN_POINT('Ctrl Pts',(21.6730647353122,20.4044576185522,39.7693845669452));
#53148=CARTESIAN_POINT('Ctrl Pts',(21.7289743615636,20.408681620214,39.7133516875848));
#53149=CARTESIAN_POINT('Ctrl Pts',(21.7821068118514,20.4129056218758,39.65446612396));
#53150=CARTESIAN_POINT('Ctrl Pts',(21.8321646673188,20.4171296235375,39.5930382020326));
#53151=CARTESIAN_POINT('Ctrl Pts',(21.8822065090906,20.4213522739253,39.5316299311276));
#53152=CARTESIAN_POINT('Ctrl Pts',(21.9291754133107,20.4255749243131,39.467681280123));
#53153=CARTESIAN_POINT('Ctrl Pts',(21.9728135265791,20.4297975747009,39.4015364882502));
#53154=CARTESIAN_POINT('Ctrl Pts',(22.0164512664753,20.4340201889593,39.335392262319));
#53155=CARTESIAN_POINT('Ctrl Pts',(22.0567580151298,20.4382428032177,39.2670523249554));
#53156=CARTESIAN_POINT('Ctrl Pts',(22.093519471624,20.4424654174761,39.1968895399407));
#53157=CARTESIAN_POINT('Ctrl Pts',(22.1303174801156,20.4466922302892,39.1266569919137));
#53158=CARTESIAN_POINT('Ctrl Pts',(22.163562936996,20.4509190431022,39.0545983920297));
#53159=CARTESIAN_POINT('Ctrl Pts',(22.1930880263597,20.4551458559153,38.9811102936283));
#53160=CARTESIAN_POINT('Ctrl Pts',(22.2226274220386,20.459374716821,38.9075865867352));
#53161=CARTESIAN_POINT('Ctrl Pts',(22.2484427061719,20.4636035777266,38.8326324452511));
#53162=CARTESIAN_POINT('Ctrl Pts',(22.2704155425845,20.4678324386323,38.7566610273883));
#53163=CARTESIAN_POINT('Ctrl Pts',(22.2924278671954,20.4720688993805,38.6805530784764));
#53164=CARTESIAN_POINT('Ctrl Pts',(22.3105838387478,20.4763053601287,38.6034246576765));
#53165=CARTESIAN_POINT('Ctrl Pts',(22.3248160438984,20.4805418208769,38.5257003675506));
#53166=CARTESIAN_POINT('Ctrl Pts',(22.3377510215795,20.4843921395483,38.4550604387819));
#53167=CARTESIAN_POINT('Ctrl Pts',(22.3474455405035,20.4882424582196,38.3839286802298));
#53168=CARTESIAN_POINT('Ctrl Pts',(22.3538863219802,20.4920927768909,38.3126255490165));
#53169=CARTESIAN_POINT('Ctrl Pts',(22.3609750725108,20.4963304534248,38.2341490301268));
#53170=CARTESIAN_POINT('Ctrl Pts',(22.3641483276393,20.5005681299588,38.1551703345829));
#53171=CARTESIAN_POINT('Ctrl Pts',(22.3633492908255,20.5048058064928,38.0761133833532));
#53172=CARTESIAN_POINT('Ctrl Pts',(22.3625514030035,20.5090373893705,37.9971701137321));
#53173=CARTESIAN_POINT('Ctrl Pts',(22.3577925715276,20.5132689722482,37.9181492767671));
#53174=CARTESIAN_POINT('Ctrl Pts',(22.3490677962963,20.5175005551259,37.839479503103));
#53175=CARTESIAN_POINT('Ctrl Pts',(22.3403530979342,20.5217272506448,37.7609005908076));
#53176=CARTESIAN_POINT('Ctrl Pts',(22.3276816099419,20.5259539461637,37.6826723995959));
#53177=CARTESIAN_POINT('Ctrl Pts',(22.3111003420476,20.5301806416826,37.6052216153798));
#53178=CARTESIAN_POINT('Ctrl Pts',(22.2945295402749,20.5344046693049,37.5278197182165));
#53179=CARTESIAN_POINT('Ctrl Pts',(22.2740539549072,20.5386286969271,37.4511947112408));
#53180=CARTESIAN_POINT('Ctrl Pts',(22.2497720166536,20.5428527245494,37.3757650146655));
#53181=CARTESIAN_POINT('Ctrl Pts',(22.2254978451484,20.5470754010867,37.300359444808));
#53182=CARTESIAN_POINT('Ctrl Pts',(22.1974198819901,20.5512980776241,37.2261488720142));
#53183=CARTESIAN_POINT('Ctrl Pts',(22.1656865434081,20.5555207541615,37.153536986142));
#53184=CARTESIAN_POINT('Ctrl Pts',(22.1339534752,20.5597433947209,37.0809257189366));
#53185=CARTESIAN_POINT('Ctrl Pts',(22.0985652825216,20.5639660352802,37.0099135405335));
#53186=CARTESIAN_POINT('Ctrl Pts',(22.059718100853,20.5681886758396,36.9408831871126));
#53187=CARTESIAN_POINT('Ctrl Pts',(22.0208322931237,20.572415515004,36.8717841962637));
#53188=CARTESIAN_POINT('Ctrl Pts',(21.9784808568169,20.5766423541684,36.8046713760373));
#53189=CARTESIAN_POINT('Ctrl Pts',(21.9329051031451,20.5808691933328,36.7399013627182));
#53190=CARTESIAN_POINT('Ctrl Pts',(21.8873072652332,20.5850980806592,36.6750999643664));
#53191=CARTESIAN_POINT('Ctrl Pts',(21.8384822865885,20.5893269679857,36.6126440042219));
#53192=CARTESIAN_POINT('Ctrl Pts',(21.7867123412089,20.5935558553122,36.552857650159));
#53193=CARTESIAN_POINT('Ctrl Pts',(21.7348493611133,20.597792342286,36.4929638552549));
#53194=CARTESIAN_POINT('Ctrl Pts',(21.6800311647458,20.6020288292599,36.4357495915753));
#53195=CARTESIAN_POINT('Ctrl Pts',(21.6225772454314,20.6062653162338,36.381502538987));
#53196=CARTESIAN_POINT('Ctrl Pts',(21.5703635869588,20.6101154014259,36.3322032551298));
#53197=CARTESIAN_POINT('Ctrl Pts',(21.5159737244961,20.6139654866179,36.2853542747074));
#53198=CARTESIAN_POINT('Ctrl Pts',(21.45966920065,20.61781557181,36.2411411388775));
#53199=CARTESIAN_POINT('Ctrl Pts',(21.3976985092085,20.6220531077158,36.19247864409));
#53200=CARTESIAN_POINT('Ctrl Pts',(21.3331753313424,20.6262906436217,36.1468271399636));
#53201=CARTESIAN_POINT('Ctrl Pts',(21.2664243354685,20.6305281795275,36.1044650232499));
#53202=CARTESIAN_POINT('Ctrl Pts',(21.1997693343686,20.6347596214224,36.0621638276021));
#53203=CARTESIAN_POINT('Ctrl Pts',(21.1308932703097,20.6389910633172,36.0231428742147));
#53204=CARTESIAN_POINT('Ctrl Pts',(21.0601529588401,20.6432225052121,35.9876396744962));
#53205=CARTESIAN_POINT('Ctrl Pts',(20.9894943510225,20.6474490598758,35.9521774802668));
#53206=CARTESIAN_POINT('Ctrl Pts',(20.9169761915445,20.6516756145395,35.9202251748641));
#53207=CARTESIAN_POINT('Ctrl Pts',(20.8429819769238,20.6559021692032,35.89197558268));
#53208=CARTESIAN_POINT('Ctrl Pts',(20.7690344666336,20.6601260561123,35.8637438213262));
#53209=CARTESIAN_POINT('Ctrl Pts',(20.6936131872793,20.6643499430214,35.8392103010606));
#53210=CARTESIAN_POINT('Ctrl Pts',(20.6171226929917,20.6685738299305,35.8185202120784));
#53211=CARTESIAN_POINT('Ctrl Pts',(20.5406566594799,20.6727963660894,35.7978367395476));
#53212=CARTESIAN_POINT('Ctrl Pts',(20.4631225422344,20.6770189022483,35.7809943799041));
#53213=CARTESIAN_POINT('Ctrl Pts',(20.384939748247,20.6812414384072,35.768088374076));
#53214=CARTESIAN_POINT('Ctrl Pts',(20.306757610646,20.6854639391157,35.7551824766007));
#53215=CARTESIAN_POINT('Ctrl Pts',(20.2279272699033,20.6896864398241,35.7462129421741));
#53216=CARTESIAN_POINT('Ctrl Pts',(20.1488765312761,20.6939089405326,35.7412235758056));
#53217=CARTESIAN_POINT('Ctrl Pts',(20.0697471555963,20.6981356416447,35.736229246181));
#53218=CARTESIAN_POINT('Ctrl Pts',(19.9903974130468,20.7023623427568,35.7352230230069));
#53219=CARTESIAN_POINT('Ctrl Pts',(19.9112578054728,20.7065890438688,35.7381966077147));
#53220=CARTESIAN_POINT('Ctrl Pts',(19.8320798343499,20.7108177939076,35.7411716338911));
#53221=CARTESIAN_POINT('Ctrl Pts',(19.7531126687147,20.7150465439464,35.7481302700112));
#53222=CARTESIAN_POINT('Ctrl Pts',(19.6747818161435,20.7192752939852,35.7590122653484));
#53223=CARTESIAN_POINT('Ctrl Pts',(19.5963101386655,20.7235116465626,35.7699138245731));
#53224=CARTESIAN_POINT('Ctrl Pts',(19.518477521625,20.72774799914,35.7847527485802));
#53225=CARTESIAN_POINT('Ctrl Pts',(19.4416991776763,20.7319843517174,35.8034176190059));
#53226=CARTESIAN_POINT('Ctrl Pts',(19.3718987127443,20.7358356900546,35.820386162043));
#53227=CARTESIAN_POINT('Ctrl Pts',(19.302969678025,20.7396870283918,35.8405161048758));
#53228=CARTESIAN_POINT('Ctrl Pts',(19.2352103821458,20.743538366729,35.8636889122212));
#53229=CARTESIAN_POINT('Ctrl Pts',(19.1606528728991,20.7477761054771,35.8891866210671));
#53230=CARTESIAN_POINT('Ctrl Pts',(19.0872319476852,20.7520138442252,35.9184648282699));
#53231=CARTESIAN_POINT('Ctrl Pts',(19.0153578995573,20.7562515829733,35.9514026959582));
#53232=CARTESIAN_POINT('Ctrl Pts',(18.9435872179411,20.7604832271673,35.9842931936628));
#53233=CARTESIAN_POINT('Ctrl Pts',(18.8733594180529,20.7647148713613,36.0208327059724));
#53234=CARTESIAN_POINT('Ctrl Pts',(18.8050679923315,20.7689465155553,36.0608511731732));
#53235=CARTESIAN_POINT('Ctrl Pts',(18.7368554662643,20.7731732707715,36.1008234055327));
#53236=CARTESIAN_POINT('Ctrl Pts',(18.6705752709255,20.7774000259878,36.1442663694814));
#53237=CARTESIAN_POINT('Ctrl Pts',(18.6065979340457,20.781626781204,36.1909632995947));
#53238=CARTESIAN_POINT('Ctrl Pts',(18.5426609944809,20.7858508675132,36.2376307437887));
#53239=CARTESIAN_POINT('Ctrl Pts',(18.4810244047791,20.7900749538225,36.2875478002407));
#53240=CARTESIAN_POINT('Ctrl Pts',(18.4220301955602,20.7942990401317,36.3404541105228));
#53241=CARTESIAN_POINT('Ctrl Pts',(18.3630548709045,20.7985217742739,36.3933434850314));
#53242=CARTESIAN_POINT('Ctrl Pts',(18.306720595762,20.8027445084161,36.4492199004445));
#53243=CARTESIAN_POINT('Ctrl Pts',(18.2533355846976,20.8069672425583,36.5077833497868));
#53244=CARTESIAN_POINT('Ctrl Pts',(18.1999510430786,20.8111899395675,36.5663462841466));
#53245=CARTESIAN_POINT('Ctrl Pts',(18.1495160287036,20.8154126365768,36.6275958580747));
#53246=CARTESIAN_POINT('Ctrl Pts',(18.1023001799655,20.819635333586,36.6911970208929));
#53247=CARTESIAN_POINT('Ctrl Pts',(18.0550374092106,20.8238622270137,36.7548613890736));
#53248=CARTESIAN_POINT('Ctrl Pts',(18.0110004744393,20.8280891204415,36.8208816369771));
#53249=CARTESIAN_POINT('Ctrl Pts',(17.9704167741943,20.8323160138692,36.8888920896847));
#53250=CARTESIAN_POINT('Ctrl Pts',(17.9298134195799,20.8365449543485,36.9569354793241));
#53251=CARTESIAN_POINT('Ctrl Pts',(17.8926668509941,20.8407738948277,37.0269705792204));
#53252=CARTESIAN_POINT('Ctrl Pts',(17.8591581683313,20.845002835307,37.0986076230182));
#53253=CARTESIAN_POINT('Ctrl Pts',(17.8255892882827,20.8492393729563,37.1703733607072));
#53254=CARTESIAN_POINT('Ctrl Pts',(17.795671529851,20.8534759106056,37.2437463574324));
#53255=CARTESIAN_POINT('Ctrl Pts',(17.7695374667954,20.857712448255,37.3183176291674));
#53256=CARTESIAN_POINT('Ctrl Pts',(17.7457904962732,20.861562019386,37.3860775403581));
#53257=CARTESIAN_POINT('Ctrl Pts',(17.7251670205788,20.865411590517,37.4548263636818));
#53258=CARTESIAN_POINT('Ctrl Pts',(17.7077299169298,20.8692611616481,37.5242497875283));
#53259=CARTESIAN_POINT('Ctrl Pts',(17.6828131325473,20.8747620140699,37.6234525288718));
#53260=CARTESIAN_POINT('Ctrl Pts',(17.6643259671831,20.8802628664916,37.7243300595161));
#53261=CARTESIAN_POINT('Ctrl Pts',(17.6524475134137,20.8857637189134,37.8261610626257));
#53262=CARTESIAN_POINT('Ctrl Pts',(17.6419497240976,20.8906251925449,37.9161559758721));
#53263=CARTESIAN_POINT('Ctrl Pts',(17.6366130815916,20.8954866661763,38.0068955425699));
#53264=CARTESIAN_POINT('Ctrl Pts',(17.6365309629368,20.9003481398077,38.0978665184563));
#53265=CARTESIAN_POINT('',(17.6389973268257,21.6940981586901,38.1008155980709));
#53266=CARTESIAN_POINT('Ctrl Pts',(17.6368549259571,20.9003481502717,38.0978670066765));
#53267=CARTESIAN_POINT('Ctrl Pts',(17.6421592816668,20.9318934190369,38.6880864281803));
#53268=CARTESIAN_POINT('Ctrl Pts',(18.164146447441,21.0053462861083,40.0707873438575));
#53269=CARTESIAN_POINT('Ctrl Pts',(20.4819917868442,21.1207067514864,40.8493537277608));
#53270=CARTESIAN_POINT('Ctrl Pts',(22.5685527330183,21.2464295464053,39.1923202798239));
#53271=CARTESIAN_POINT('Ctrl Pts',(22.3147694606222,21.3721523413244,36.539764552403));
#53272=CARTESIAN_POINT('Ctrl Pts',(19.950593046619,21.4978751362435,35.3092112299817));
#53273=CARTESIAN_POINT('Ctrl Pts',(17.972450588763,21.6051904058926,36.4295872739547));
#53274=CARTESIAN_POINT('Ctrl Pts',(17.6411648689987,21.6705980772353,37.6595592470186));
#53275=CARTESIAN_POINT('Ctrl Pts',(17.6396904081475,21.6940981502717,38.1008152004127));
#53276=CARTESIAN_POINT('',(17.8640015678817,21.7500582353796,39.1118986969983));
#53277=CARTESIAN_POINT('Ctrl Pts',(17.6365301412143,21.6940981886575,38.1008170136285));
#53278=CARTESIAN_POINT('Ctrl Pts',(17.6365600512031,21.6987000667762,38.1873410991501));
#53279=CARTESIAN_POINT('Ctrl Pts',(17.6413455319869,21.7033019448949,38.2737209365862));
#53280=CARTESIAN_POINT('Ctrl Pts',(17.6508139214875,21.7079038230136,38.3594517477744));
#53281=CARTESIAN_POINT('Ctrl Pts',(17.6602963768197,21.7125125374841,38.4453099169623));
#53282=CARTESIAN_POINT('Ctrl Pts',(17.6744755305038,21.7171212519547,38.5305168200371));
#53283=CARTESIAN_POINT('Ctrl Pts',(17.6932279303512,21.7217299664253,38.6145804694974));
#53284=CARTESIAN_POINT('Ctrl Pts',(17.712060860961,21.7263584726714,38.6990051239404));
#53285=CARTESIAN_POINT('Ctrl Pts',(17.7355062649425,21.7309869789176,38.7822763791188));
#53286=CARTESIAN_POINT('Ctrl Pts',(17.7633902310012,21.7356154851638,38.8639156904523));
#53287=CARTESIAN_POINT('Ctrl Pts',(17.7909121752497,21.7401838988031,38.9444950660788));
#53288=CARTESIAN_POINT('Ctrl Pts',(17.8227578968555,21.7447523124424,39.0234843889073));
#53289=CARTESIAN_POINT('Ctrl Pts',(17.8587159851212,21.7493207260817,39.1004465045792));
#53290=CARTESIAN_POINT('Ctrl Pts',(17.860498178638,21.7495471507211,39.1042609838856));
#53291=CARTESIAN_POINT('Ctrl Pts',(17.8622905760233,21.7497735753605,39.1080707250178));
#53292=CARTESIAN_POINT('Ctrl Pts',(17.8640931615355,21.75,39.111875693107));
#53293=CARTESIAN_POINT('',(17.63653,21.75,38.1));
#53294=CARTESIAN_POINT('Origin',(20.,21.75,38.1));
#53295=CARTESIAN_POINT('',(17.9450946017473,21.75,36.932372385933));
#53296=CARTESIAN_POINT('Origin',(20.,21.75,38.1));
#53297=CARTESIAN_POINT('',(17.6365309178096,21.0215268497626,38.0979171101847));
#53298=CARTESIAN_POINT('Ctrl Pts',(17.9450946017473,21.75,36.932372385933));
#53299=CARTESIAN_POINT('Ctrl Pts',(17.9851605709061,21.7456651391115,36.8618603705277));
#53300=CARTESIAN_POINT('Ctrl Pts',(18.028888487075,21.7413302782229,36.7933619642338));
#53301=CARTESIAN_POINT('Ctrl Pts',(18.0760493998635,21.7369954173344,36.7272638530531));
#53302=CARTESIAN_POINT('Ctrl Pts',(18.1231813997955,21.7326632140112,36.6612062645235));
#53303=CARTESIAN_POINT('Ctrl Pts',(18.1737419548967,21.7283310106881,36.5975463986434));
#53304=CARTESIAN_POINT('Ctrl Pts',(18.2274587566072,21.723998807365,36.5366420814888));
#53305=CARTESIAN_POINT('Ctrl Pts',(18.2811699013855,21.7196670602675,36.4757441781859));
#53306=CARTESIAN_POINT('Ctrl Pts',(18.3380363499296,21.71533531317,36.4176015811557));
#53307=CARTESIAN_POINT('Ctrl Pts',(18.3977459308174,21.7110035660725,36.3625385360568));
#53308=CARTESIAN_POINT('Ctrl Pts',(18.4574542812051,21.706671908244,36.3074766257017));
#53309=CARTESIAN_POINT('Ctrl Pts',(18.5200053258509,21.7023402504155,36.2554944382585));
#53310=CARTESIAN_POINT('Ctrl Pts',(18.5850514603843,21.698008592587,36.2068779566179));
#53311=CARTESIAN_POINT('Ctrl Pts',(18.6501122764574,21.6936759570615,36.1582505017685));
#53312=CARTESIAN_POINT('Ctrl Pts',(18.7176689517958,21.6893433215361,36.1129905258459));
#53313=CARTESIAN_POINT('Ctrl Pts',(18.7873432679355,21.6850106860106,36.0713418003324));
#53314=CARTESIAN_POINT('Ctrl Pts',(18.8570504778676,21.6806760050139,36.0296734121281));
#53315=CARTESIAN_POINT('Ctrl Pts',(18.9288769414282,21.6763413240172,35.9916198898748));
#53316=CARTESIAN_POINT('Ctrl Pts',(19.0024190898503,21.6720066430205,35.9573794622927));
#53317=CARTESIAN_POINT('Ctrl Pts',(19.0760706189195,21.6676655149696,35.9230881082663));
#53318=CARTESIAN_POINT('Ctrl Pts',(19.1514425308926,21.6633243869187,35.8926213592826));
#53319=CARTESIAN_POINT('Ctrl Pts',(19.2281105539884,21.6589832588679,35.8661295641788));
#53320=CARTESIAN_POINT('Ctrl Pts',(19.3048387862111,21.6546387216313,35.8396169644711));
#53321=CARTESIAN_POINT('Ctrl Pts',(19.3828647373174,21.6502941843947,35.8170856609605));
#53322=CARTESIAN_POINT('Ctrl Pts',(19.461750524746,21.6459496471581,35.7986356343923));
#53323=CARTESIAN_POINT('Ctrl Pts',(19.5407886017683,21.6415967227604,35.780149989912));
#53324=CARTESIAN_POINT('Ctrl Pts',(19.6206894004145,21.6372437983627,35.7657614431077));
#53325=CARTESIAN_POINT('Ctrl Pts',(19.7010063587428,21.6328908739649,35.7555185555463));
#53326=CARTESIAN_POINT('Ctrl Pts',(19.7539840523267,21.6300196510036,35.748762266838));
#53327=CARTESIAN_POINT('Ctrl Pts',(19.8071426961314,21.6271484280423,35.7438086087321));
#53328=CARTESIAN_POINT('Ctrl Pts',(19.860354082761,21.6242772050809,35.7406591050256));
#53329=CARTESIAN_POINT('Ctrl Pts',(19.9381292905192,21.6200805476269,35.7360557048773));
#53330=CARTESIAN_POINT('Ctrl Pts',(20.0163084813515,21.6158838901729,35.7352919334201));
#53331=CARTESIAN_POINT('Ctrl Pts',(20.0944748898714,21.6116872327189,35.7384189753295));
#53332=CARTESIAN_POINT('Ctrl Pts',(20.1725163937938,21.6074972812377,35.7415410204389));
#53333=CARTESIAN_POINT('Ctrl Pts',(20.250544682398,21.6033073297565,35.7485415218038));
#53334=CARTESIAN_POINT('Ctrl Pts',(20.3281387129406,21.5991173782753,35.7594198526926));
#53335=CARTESIAN_POINT('Ctrl Pts',(20.4057359322867,21.5949272546039,35.7702986306371));
#53336=CARTESIAN_POINT('Ctrl Pts',(20.4828983768163,21.5907371309325,35.7850555670828));
#53337=CARTESIAN_POINT('Ctrl Pts',(20.5592058395492,21.5865470072611,35.803637818219));
#53338=CARTESIAN_POINT('Ctrl Pts',(20.6353510052443,21.5823657954921,35.8221805470829));
#53339=CARTESIAN_POINT('Ctrl Pts',(20.7106443491242,21.5781845837231,35.8445322558333));
#53340=CARTESIAN_POINT('Ctrl Pts',(20.7846763779237,21.5740033719541,35.8705889964324));
#53341=CARTESIAN_POINT('Ctrl Pts',(20.8586776733355,21.5698238959582,35.8966349199307));
#53342=CARTESIAN_POINT('Ctrl Pts',(20.9314182411447,21.5656444199623,35.926382664346));
#53343=CARTESIAN_POINT('Ctrl Pts',(21.0025041375631,21.5614649439663,35.9596785533316));
#53344=CARTESIAN_POINT('Ctrl Pts',(21.0735837645821,21.557285836578,35.9929715057962));
#53345=CARTESIAN_POINT('Ctrl Pts',(21.1430085765028,21.5531067291897,36.0298117771111));
#53346=CARTESIAN_POINT('Ctrl Pts',(21.2104064971494,21.5489276218014,36.06999838607));
#53347=CARTESIAN_POINT('Ctrl Pts',(21.2781053581212,21.5447298541648,36.1103644333714));
#53348=CARTESIAN_POINT('Ctrl Pts',(21.3437587583622,21.5405320865282,36.1541065357132));
#53349=CARTESIAN_POINT('Ctrl Pts',(21.4070181129212,21.5363343188915,36.2009764427971));
#53350=CARTESIAN_POINT('Ctrl Pts',(21.4700838811366,21.5321493972679,36.2477029185418));
#53351=CARTESIAN_POINT('Ctrl Pts',(21.5307698904924,21.5279644756442,36.2975377427675));
#53352=CARTESIAN_POINT('Ctrl Pts',(21.5887647458843,21.5237795540205,36.3501951471278));
#53353=CARTESIAN_POINT('Ctrl Pts',(21.6470266323214,21.5195753633774,36.4030950068167));
#53354=CARTESIAN_POINT('Ctrl Pts',(21.7025721844741,21.5153711727343,36.4588431509752));
#53355=CARTESIAN_POINT('Ctrl Pts',(21.7551252698619,21.5111669820912,36.5171147457911));
#53356=CARTESIAN_POINT('Ctrl Pts',(21.8076783552497,21.5069627914481,36.575386340607));
#53357=CARTESIAN_POINT('Ctrl Pts',(21.8572387223883,21.5027586008049,36.6361809685824));
#53358=CARTESIAN_POINT('Ctrl Pts',(21.9035741464061,21.4985544101618,36.6991445791823));
#53359=CARTESIAN_POINT('Ctrl Pts',(21.9503378161638,21.4943113631411,36.7626901181573));
#53360=CARTESIAN_POINT('Ctrl Pts',(21.9940026520819,21.4900683161204,36.8286974682417));
#53361=CARTESIAN_POINT('Ctrl Pts',(22.0343003622833,21.4858252690997,36.8968323155462));
#53362=CARTESIAN_POINT('Ctrl Pts',(22.0745401666081,21.481588319134,36.9648692563433));
#53363=CARTESIAN_POINT('Ctrl Pts',(22.1114222185724,21.4773513691683,37.035027223734));
#53364=CARTESIAN_POINT('Ctrl Pts',(22.1447201399324,21.4731144192026,37.1069411083585));
#53365=CARTESIAN_POINT('Ctrl Pts',(22.1779793978106,21.4688823889205,37.1787714910387));
#53366=CARTESIAN_POINT('Ctrl Pts',(22.2076626007544,21.4646503586385,37.2523533168423));
#53367=CARTESIAN_POINT('Ctrl Pts',(22.2335888985862,21.4604183283564,37.3272962579277));
#53368=CARTESIAN_POINT('Ctrl Pts',(22.2594987142216,21.4561889885146,37.4021915553317));
#53369=CARTESIAN_POINT('Ctrl Pts',(22.281656213478,21.4519596486727,37.4784458097847));
#53370=CARTESIAN_POINT('Ctrl Pts',(22.2999288277623,21.4477303088309,37.5556491681572));
#53371=CARTESIAN_POINT('Ctrl Pts',(22.3181954730667,21.4435023505562,37.6328273070788));
#53372=CARTESIAN_POINT('Ctrl Pts',(22.3325796461432,21.4392743922816,37.7109534797209));
#53373=CARTESIAN_POINT('Ctrl Pts',(22.3429991708417,21.4350464340069,37.7896045645709));
#53374=CARTESIAN_POINT('Ctrl Pts',(22.353418512125,21.4308185501571,37.8682542649241));
#53375=CARTESIAN_POINT('Ctrl Pts',(22.3598732837732,21.4265906663073,37.9474283956148));
#53376=CARTESIAN_POINT('Ctrl Pts',(22.3623329819944,21.4223627824575,38.0266970458871));
#53377=CARTESIAN_POINT('Ctrl Pts',(22.3647950655226,21.4181307985919,38.1060425674101));
#53378=CARTESIAN_POINT('Ctrl Pts',(22.3632543219911,21.4138988147263,38.185482323399));
#53379=CARTESIAN_POINT('Ctrl Pts',(22.3577324085168,21.4096668308607,38.26458532963));
#53380=CARTESIAN_POINT('Ctrl Pts',(22.3522078826181,21.405432844838,38.3437257595965));
#53381=CARTESIAN_POINT('Ctrl Pts',(22.3426984899765,21.4011988588153,38.4225286577333));
#53382=CARTESIAN_POINT('Ctrl Pts',(22.3292776621049,21.3969648727926,38.5005696115769));
#53383=CARTESIAN_POINT('Ctrl Pts',(22.3158331840349,21.3927234256348,38.5787480892799));
#53384=CARTESIAN_POINT('Ctrl Pts',(22.2984636004284,21.388481978477,38.6561614826017));
#53385=CARTESIAN_POINT('Ctrl Pts',(22.2772931704297,21.3842405313192,38.7323972302391));
#53386=CARTESIAN_POINT('Ctrl Pts',(22.2583113111591,21.3804375592937,38.8007518282861));
#53387=CARTESIAN_POINT('Ctrl Pts',(22.2362746075327,21.3766345872682,38.8681596607891));
#53388=CARTESIAN_POINT('Ctrl Pts',(22.2113054209498,21.3728316152427,38.9343373275709));
#53389=CARTESIAN_POINT('Ctrl Pts',(22.1834357300525,21.3685868772538,39.0082024136995));
#53390=CARTESIAN_POINT('Ctrl Pts',(22.1518106828993,21.3643421392649,39.0808028936984));
#53391=CARTESIAN_POINT('Ctrl Pts',(22.1165658357701,21.3600974012759,39.1517316690823));
#53392=CARTESIAN_POINT('Ctrl Pts',(22.0813703688881,21.3558586104318,39.2225610687918));
#53393=CARTESIAN_POINT('Ctrl Pts',(22.0425653810947,21.3516198195878,39.2917230008846));
#53394=CARTESIAN_POINT('Ctrl Pts',(22.0003350258194,21.3473810287437,39.3588289102893));
#53395=CARTESIAN_POINT('Ctrl Pts',(21.9581515078158,21.3431469391008,39.4258603931899));
#53396=CARTESIAN_POINT('Ctrl Pts',(21.9125504199301,21.338912849458,39.4908399919148));
#53397=CARTESIAN_POINT('Ctrl Pts',(21.8637617976855,21.3346787598151,39.5534037300035));
#53398=CARTESIAN_POINT('Ctrl Pts',(21.8150026522956,21.3304472283024,39.6159296686601));
#53399=CARTESIAN_POINT('Ctrl Pts',(21.7630600820158,21.3262156967897,39.6760422768745));
#53400=CARTESIAN_POINT('Ctrl Pts',(21.7082067031625,21.3219841652769,39.733407573195));
#53401=CARTESIAN_POINT('Ctrl Pts',(21.6533695550489,21.3177538858455,39.7907558955165));
#53402=CARTESIAN_POINT('Ctrl Pts',(21.5956236314241,21.313523606414,39.845358183187));
#53403=CARTESIAN_POINT('Ctrl Pts',(21.5352800179998,21.3092933269825,39.8969156093792));
#53404=CARTESIAN_POINT('Ctrl Pts',(21.4749356576554,21.3050629951896,39.948473673738));
#53405=CARTESIAN_POINT('Ctrl Pts',(21.4119938996078,21.3008326633966,39.9969864995924));
#53406=CARTESIAN_POINT('Ctrl Pts',(21.3467995518017,21.2966023316037,40.0421949974621));
#53407=CARTESIAN_POINT('Ctrl Pts',(21.2815391889019,21.2923677162224,40.0874492729693));
#53408=CARTESIAN_POINT('Ctrl Pts',(21.2140220648128,21.2881331008411,40.1293922706003));
#53409=CARTESIAN_POINT('Ctrl Pts',(21.1446221918467,21.2838984854598,40.1678081339506));
#53410=CARTESIAN_POINT('Ctrl Pts',(21.075187789895,21.2796617632018,40.2062431106037));
#53411=CARTESIAN_POINT('Ctrl Pts',(21.0038691928153,21.2754250409438,40.2411472514391));
#53412=CARTESIAN_POINT('Ctrl Pts',(20.9310629697655,21.2711883186858,40.2723517641559));
#53413=CARTESIAN_POINT('Ctrl Pts',(20.8581260144692,21.2669439888883,40.3036123082927));
#53414=CARTESIAN_POINT('Ctrl Pts',(20.7836965347698,21.2626996590908,40.3311597882819));
#53415=CARTESIAN_POINT('Ctrl Pts',(20.7081887250828,21.2584553292933,40.3548745354378));
#53416=CARTESIAN_POINT('Ctrl Pts',(20.6409028730737,21.2546731596368,40.3760070113257));
#53417=CARTESIAN_POINT('Ctrl Pts',(20.5727611740573,21.2508909899802,40.3940966556243));
#53418=CARTESIAN_POINT('Ctrl Pts',(20.5040626209202,21.2471088203236,40.409093180253));
#53419=CARTESIAN_POINT('Ctrl Pts',(20.4271862073671,21.2428764220362,40.4258748878229));
#53420=CARTESIAN_POINT('Ctrl Pts',(20.3493230194014,21.2386440237488,40.4388454898891));
#53421=CARTESIAN_POINT('Ctrl Pts',(20.2708853972536,21.2344116254614,40.4478951302081));
#53422=CARTESIAN_POINT('Ctrl Pts',(20.1925620912636,21.2301853955342,40.4569315814466));
#53423=CARTESIAN_POINT('Ctrl Pts',(20.1136664765453,21.225959165607,40.462058364944));
#53424=CARTESIAN_POINT('Ctrl Pts',(20.0346221513252,21.2217329356798,40.4632163987959));
#53425=CARTESIAN_POINT('Ctrl Pts',(19.9556708721593,21.2175116806072,40.4643730694825));
#53426=CARTESIAN_POINT('Ctrl Pts',(19.8765716979425,21.2132904255345,40.4615702671053));
#53427=CARTESIAN_POINT('Ctrl Pts',(19.7977528874448,21.2090691704619,40.4548007445139));
#53428=CARTESIAN_POINT('Ctrl Pts',(19.7189848419724,21.2048506341834,40.4480355819856));
#53429=CARTESIAN_POINT('Ctrl Pts',(19.6404972689457,21.2006320979049,40.4373088100029));
#53430=CARTESIAN_POINT('Ctrl Pts',(19.5627167333875,21.1964135616264,40.4226652332269));
#53431=CARTESIAN_POINT('Ctrl Pts',(19.4849619080215,21.1921964197761,40.4080264968543));
#53432=CARTESIAN_POINT('Ctrl Pts',(19.4079141177169,21.1879792779259,40.3894736133584));
#53433=CARTESIAN_POINT('Ctrl Pts',(19.3319916212802,21.1837621360757,40.3671028311173));
#53434=CARTESIAN_POINT('Ctrl Pts',(19.2560704177342,21.1795450660396,40.3447324298302));
#53435=CARTESIAN_POINT('Ctrl Pts',(19.1812749205266,21.1753279960034,40.3185443932312));
#53436=CARTESIAN_POINT('Ctrl Pts',(19.1080086049598,21.1711109259673,40.2886849458235));
#53437=CARTESIAN_POINT('Ctrl Pts',(19.0346696529475,21.1668896751152,40.2587958956698));
#53438=CARTESIAN_POINT('Ctrl Pts',(18.9628633472858,21.1626684242631,40.2252283418271));
#53439=CARTESIAN_POINT('Ctrl Pts',(18.8929729394482,21.1584471734111,40.1881766036679));
#53440=CARTESIAN_POINT('Ctrl Pts',(18.8230489316763,21.1542238931854,40.1511070528216));
#53441=CARTESIAN_POINT('Ctrl Pts',(18.7550430607771,21.1500006129597,40.1105502221402));
#53442=CARTESIAN_POINT('Ctrl Pts',(18.6893114773836,21.145777332734,40.0667450362417));
#53443=CARTESIAN_POINT('Ctrl Pts',(18.6234610884587,21.1415464192059,40.0228606753392));
#53444=CARTESIAN_POINT('Ctrl Pts',(18.5598935789063,21.1373155056779,39.975716508835));
#53445=CARTESIAN_POINT('Ctrl Pts',(18.4989335617418,21.1330845921498,39.9255930512671));
#53446=CARTESIAN_POINT('Ctrl Pts',(18.4427483096401,21.1291850699014,39.8793955724827));
#53447=CARTESIAN_POINT('Ctrl Pts',(18.3887778975703,21.125285547653,39.8306678864608));
#53448=CARTESIAN_POINT('Ctrl Pts',(18.337247647282,21.1213860254047,39.7796562310279));
#53449=CARTESIAN_POINT('Ctrl Pts',(18.282035136839,21.117207850223,39.7249993733074));
#53450=CARTESIAN_POINT('Ctrl Pts',(18.2294031944704,21.1130296750413,39.6675008619878));
#53451=CARTESIAN_POINT('Ctrl Pts',(18.1796642322315,21.1088514998596,39.6074376051706));
#53452=CARTESIAN_POINT('Ctrl Pts',(18.1299893454759,21.1046787071503,39.5474517239568));
#53453=CARTESIAN_POINT('Ctrl Pts',(18.0832003544408,21.1005059144411,39.4849080160239));
#53454=CARTESIAN_POINT('Ctrl Pts',(18.0395737127453,21.0963331217318,39.420120908531));
#53455=CARTESIAN_POINT('Ctrl Pts',(17.9959887861599,21.0921643189815,39.3553957494537));
#53456=CARTESIAN_POINT('Ctrl Pts',(17.9555604796703,21.0879955162312,39.288431843644));
#53457=CARTESIAN_POINT('Ctrl Pts',(17.9185246427869,21.0838267134808,39.2195761600777));
#53458=CARTESIAN_POINT('Ctrl Pts',(17.8815119282262,21.0796605134097,39.1507634646947));
#53459=CARTESIAN_POINT('Ctrl Pts',(17.84788770825,21.0754943133386,39.080061759597));
#53460=CARTESIAN_POINT('Ctrl Pts',(17.8178432905259,21.0713281132674,39.0078449956887));
#53461=CARTESIAN_POINT('Ctrl Pts',(17.7877954584808,21.0671614397392,38.9356200248913));
#53462=CARTESIAN_POINT('Ctrl Pts',(17.7613284441657,21.0629947662109,38.8618800900702));
#53463=CARTESIAN_POINT('Ctrl Pts',(17.7385860222733,21.0588280926827,38.7870205690096));
#53464=CARTESIAN_POINT('Ctrl Pts',(17.71584385661,21.0546614660985,38.712161891359));
#53465=CARTESIAN_POINT('Ctrl Pts',(17.6968263319712,21.0504948395144,38.6361841176834));
#53466=CARTESIAN_POINT('Ctrl Pts',(17.6816271136747,21.0463282129303,38.5594971173486));
#53467=CARTESIAN_POINT('Ctrl Pts',(17.6664112266698,21.0421570168819,38.4827260157645));
#53468=CARTESIAN_POINT('Ctrl Pts',(17.655022096355,21.0379858208336,38.4052446104354));
#53469=CARTESIAN_POINT('Ctrl Pts',(17.6475019384674,21.0338146247853,38.3274715617071));
#53470=CARTESIAN_POINT('Ctrl Pts',(17.6401174850886,21.0297186997777,38.2511019613542));
#53471=CARTESIAN_POINT('Ctrl Pts',(17.6364634691103,21.0256227747701,38.1744516028563));
#53472=CARTESIAN_POINT('Ctrl Pts',(17.6365309178096,21.0215268497626,38.0979171101847));
#53473=CARTESIAN_POINT('',(17.6365304175565,20.2277768497005,38.1014049071763));
#53474=CARTESIAN_POINT('Ctrl Pts',(17.6365309178101,21.0215268497283,38.0979171095448));
#53475=CARTESIAN_POINT('Ctrl Pts',(17.6366289743903,21.0155722163544,37.9866516826965));
#53476=CARTESIAN_POINT('Ctrl Pts',(17.6445876386274,21.0096175829806,37.8757208437721));
#53477=CARTESIAN_POINT('Ctrl Pts',(17.6602453328089,21.0036629496068,37.7660261413564));
#53478=CARTESIAN_POINT('Ctrl Pts',(17.667257080226,21.0009963765664,37.7169032285298));
#53479=CARTESIAN_POINT('Ctrl Pts',(17.6758121746669,20.998329803526,37.6680277892764));
#53480=CARTESIAN_POINT('Ctrl Pts',(17.6858932263815,20.9956632304856,37.6194791563385));
#53481=CARTESIAN_POINT('Ctrl Pts',(17.7019167800207,20.9914247861888,37.542312443379));
#53482=CARTESIAN_POINT('Ctrl Pts',(17.7218343216131,20.9871863418919,37.4658039032194));
#53483=CARTESIAN_POINT('Ctrl Pts',(17.7455768104442,20.9829478975951,37.3903757872696));
#53484=CARTESIAN_POINT('Ctrl Pts',(17.7692852625888,20.9787155294346,37.315055803334));
#53485=CARTESIAN_POINT('Ctrl Pts',(17.796807632849,20.9744831612742,37.2408136109299));
#53486=CARTESIAN_POINT('Ctrl Pts',(17.8280239551717,20.9702507931137,37.168060891693));
#53487=CARTESIAN_POINT('Ctrl Pts',(17.8592043978289,20.9660232895863,37.0953917935567));
#53488=CARTESIAN_POINT('Ctrl Pts',(17.8940701712237,20.9617957860589,37.024209194865));
#53489=CARTESIAN_POINT('Ctrl Pts',(17.9324521150821,20.9575682825315,36.9549077834203));
#53490=CARTESIAN_POINT('Ctrl Pts',(17.9708099591438,20.9533434334287,36.8856498859238));
#53491=CARTESIAN_POINT('Ctrl Pts',(18.0126793649726,20.9491185843258,36.8182712399529));
#53492=CARTESIAN_POINT('Ctrl Pts',(18.0578443805922,20.944893735223,36.7531436635993));
#53493=CARTESIAN_POINT('Ctrl Pts',(18.1029950844597,20.9406702248774,36.688036724673));
#53494=CARTESIAN_POINT('Ctrl Pts',(18.151439057479,20.9364467145319,36.6251798236107));
#53495=CARTESIAN_POINT('Ctrl Pts',(18.2029168089793,20.9322232041863,36.5649161438375));
#53496=CARTESIAN_POINT('Ctrl Pts',(18.2543942584224,20.9279997186231,36.5046528176749));
#53497=CARTESIAN_POINT('Ctrl Pts',(18.3089051455131,20.92377623306,36.4469830378799));
#53498=CARTESIAN_POINT('Ctrl Pts',(18.3661504179376,20.9195527474968,36.3922160604765));
#53499=CARTESIAN_POINT('Ctrl Pts',(18.4234527579256,20.9153250515592,36.3373944861111));
#53500=CARTESIAN_POINT('Ctrl Pts',(18.4834945888465,20.9110973556216,36.2854818191307));
#53501=CARTESIAN_POINT('Ctrl Pts',(18.545941224779,20.906869659684,36.2367492066008));
#53502=CARTESIAN_POINT('Ctrl Pts',(18.6084182291228,20.9026399077764,36.1879928949236));
#53503=CARTESIAN_POINT('Ctrl Pts',(18.673301984301,20.8984101558689,36.1424199881516));
#53504=CARTESIAN_POINT('Ctrl Pts',(18.7402281479184,20.8941804039613,36.1002586863289));
#53505=CARTESIAN_POINT('Ctrl Pts',(18.8072746087764,20.8899430492351,36.0580216011654));
#53506=CARTESIAN_POINT('Ctrl Pts',(18.876370403896,20.8857056945089,36.0192086037558));
#53507=CARTESIAN_POINT('Ctrl Pts',(18.9471260920909,20.8814683397827,35.9840021325757));
#53508=CARTESIAN_POINT('Ctrl Pts',(19.0112907143594,20.8776257050439,35.9520752305512));
#53509=CARTESIAN_POINT('Ctrl Pts',(19.0768198616208,20.8737830703051,35.9231137278017));
#53510=CARTESIAN_POINT('Ctrl Pts',(19.1434112199942,20.8699404355663,35.8972185530861));
#53511=CARTESIAN_POINT('Ctrl Pts',(19.2168352001274,20.8657035263996,35.8686663979671));
#53512=CARTESIAN_POINT('Ctrl Pts',(19.2918266078201,20.8614666172328,35.8437355749677));
#53513=CARTESIAN_POINT('Ctrl Pts',(19.3679940539443,20.8572297080661,35.8225982073753));
#53514=CARTESIAN_POINT('Ctrl Pts',(19.4440517504979,20.852998903856,35.8014912965874));
#53515=CARTESIAN_POINT('Ctrl Pts',(19.5212816721688,20.848768099646,35.7841671107602));
#53516=CARTESIAN_POINT('Ctrl Pts',(19.5992735321796,20.844537295436,35.7707493181523));
#53517=CARTESIAN_POINT('Ctrl Pts',(19.6771750513255,20.8403113919234,35.7573470678713));
#53518=CARTESIAN_POINT('Ctrl Pts',(19.7558362950933,20.8360854884108,35.7478422978333));
#53519=CARTESIAN_POINT('Ctrl Pts',(19.8348344164102,20.8318595848983,35.7423081688021));
#53520=CARTESIAN_POINT('Ctrl Pts',(19.9137825196011,20.8276363570414,35.7367775437372));
#53521=CARTESIAN_POINT('Ctrl Pts',(19.9930666103936,20.8234131291846,35.7352126023477));
#53522=CARTESIAN_POINT('Ctrl Pts',(20.0722575189492,20.8191899013277,35.7376348098028));
#53523=CARTESIAN_POINT('Ctrl Pts',(20.1514229684259,20.8149680311961,35.7400562385427));
#53524=CARTESIAN_POINT('Ctrl Pts',(20.2304948267515,20.8107461610644,35.7464622563771));
#53525=CARTESIAN_POINT('Ctrl Pts',(20.3090442131256,20.8065242909328,35.7568222186028));
#53526=CARTESIAN_POINT('Ctrl Pts',(20.387592827256,20.8023024623076,35.7671820789765));
#53527=CARTESIAN_POINT('Ctrl Pts',(20.4656185148977,20.7980806336825,35.7814957437255));
#53528=CARTESIAN_POINT('Ctrl Pts',(20.5426992946748,20.7938588050574,35.7996809098607));
#53529=CARTESIAN_POINT('Ctrl Pts',(20.6198566757411,20.789632780866,35.8178841480389));
#53530=CARTESIAN_POINT('Ctrl Pts',(20.6960668157271,20.7854067566747,35.8399664649233));
#53531=CARTESIAN_POINT('Ctrl Pts',(20.7709202847241,20.7811807324833,35.8657949164186));
#53532=CARTESIAN_POINT('Ctrl Pts',(20.8458099792685,20.7769526630957,35.8916358676658));
#53533=CARTESIAN_POINT('Ctrl Pts',(20.9193412592673,20.772724593708,35.9212263898056));
#53534=CARTESIAN_POINT('Ctrl Pts',(20.9911245636103,20.7684965243204,35.9543852768243));
#53535=CARTESIAN_POINT('Ctrl Pts',(21.0630369701737,20.764260850753,35.9876038000771));
#53536=CARTESIAN_POINT('Ctrl Pts',(21.1331947033183,20.7600251771856,36.0244032930327));
#53537=CARTESIAN_POINT('Ctrl Pts',(21.2012329159404,20.7557895036182,36.0645565783935));
#53538=CARTESIAN_POINT('Ctrl Pts',(21.2631930631457,20.7519322159613,36.1011228457284));
#53539=CARTESIAN_POINT('Ctrl Pts',(21.3233955865241,20.7480749283044,36.1404697551222));
#53540=CARTESIAN_POINT('Ctrl Pts',(21.3815882815538,20.7442176406474,36.1823962189302));
#53541=CARTESIAN_POINT('Ctrl Pts',(21.4455221670195,20.7399797996754,36.2284590749934));
#53542=CARTESIAN_POINT('Ctrl Pts',(21.507269817599,20.7357419587034,36.2778092114351));
#53543=CARTESIAN_POINT('Ctrl Pts',(21.5664737493925,20.7315041177315,36.3302117546542));
#53544=CARTESIAN_POINT('Ctrl Pts',(21.6255925687079,20.7272723691445,36.3825389631754));
#53545=CARTESIAN_POINT('Ctrl Pts',(21.6821745834153,20.7230406205575,36.4379095558165));
#53546=CARTESIAN_POINT('Ctrl Pts',(21.735892690379,20.7188088719706,36.4960464444415));
#53547=CARTESIAN_POINT('Ctrl Pts',(21.7895487710125,20.7145820096287,36.5541162045311));
#53548=CARTESIAN_POINT('Ctrl Pts',(21.8403471989748,20.7103551472868,36.6149455705054));
#53549=CARTESIAN_POINT('Ctrl Pts',(21.8879964182131,20.7061282849448,36.6782194382696));
#53550=CARTESIAN_POINT('Ctrl Pts',(21.9356155691283,20.7019040899009,36.7414533780112));
#53551=CARTESIAN_POINT('Ctrl Pts',(21.9800891745965,20.6976798948569,36.8071283842608));
#53552=CARTESIAN_POINT('Ctrl Pts',(22.021165614587,20.6934556998129,36.8748959230697));
#53553=CARTESIAN_POINT('Ctrl Pts',(22.0622289200178,20.6892328554931,36.9426417926012));
#53554=CARTESIAN_POINT('Ctrl Pts',(22.0998969743171,20.6850100111733,37.0124784654269));
#53555=CARTESIAN_POINT('Ctrl Pts',(22.1339620363046,20.6807871668535,37.0840292974152));
#53556=CARTESIAN_POINT('Ctrl Pts',(22.168026809056,20.6765643583885,37.1555795218871));
#53557=CARTESIAN_POINT('Ctrl Pts',(22.1984884501264,20.6723415499236,37.2288434527625));
#53558=CARTESIAN_POINT('Ctrl Pts',(22.2251863134758,20.6681187414587,37.3034221248239));
#53559=CARTESIAN_POINT('Ctrl Pts',(22.2519107153947,20.6638917353809,37.3780749305809));
#53560=CARTESIAN_POINT('Ctrl Pts',(22.2748637079411,20.659664729303,37.4540446457334));
#53561=CARTESIAN_POINT('Ctrl Pts',(22.2939339613271,20.6554377232252,37.5309152769839));
#53562=CARTESIAN_POINT('Ctrl Pts',(22.3130134538007,20.6512086692627,37.6078231502409));
#53563=CARTESIAN_POINT('Ctrl Pts',(22.3282063697943,20.6469796153002,37.6856323484805));
#53564=CARTESIAN_POINT('Ctrl Pts',(22.3394526809638,20.6427505613377,37.7639172803742));
#53565=CARTESIAN_POINT('Ctrl Pts',(22.3507191953941,20.638513910157,37.8423428460157));
#53566=CARTESIAN_POINT('Ctrl Pts',(22.35802489553,20.6342772589763,37.9212453851012));
#53567=CARTESIAN_POINT('Ctrl Pts',(22.3613617695357,20.6300406077956,38.0001950187851));
#53568=CARTESIAN_POINT('Ctrl Pts',(22.3643929964548,20.6261920204398,38.0719131161635));
#53569=CARTESIAN_POINT('Ctrl Pts',(22.3641498335398,20.6223434330841,38.1436698003567));
#53570=CARTESIAN_POINT('Ctrl Pts',(22.3606634171487,20.6184948457283,38.2151463062182));
#53571=CARTESIAN_POINT('Ctrl Pts',(22.3568244818374,20.6142571195816,38.2938499524566));
#53572=CARTESIAN_POINT('Ctrl Pts',(22.3490381141486,20.6100193934349,38.3725090644142));
#53573=CARTESIAN_POINT('Ctrl Pts',(22.3373067419008,20.6057816672882,38.4506959297812));
#53574=CARTESIAN_POINT('Ctrl Pts',(22.3255922336675,20.6015500329332,38.5287704004171));
#53575=CARTESIAN_POINT('Ctrl Pts',(22.3099440519533,20.5973183985781,38.6063735128841));
#53576=CARTESIAN_POINT('Ctrl Pts',(22.2904165743647,20.593086764223,38.683080060348));
#53577=CARTESIAN_POINT('Ctrl Pts',(22.2709116382999,20.5888600146507,38.7596980616877));
#53578=CARTESIAN_POINT('Ctrl Pts',(22.2475364204582,20.5846332650784,38.8354211027636));
#53579=CARTESIAN_POINT('Ctrl Pts',(22.2203965385268,20.580406515506,38.9098331016933));
#53580=CARTESIAN_POINT('Ctrl Pts',(22.1932737771888,20.5761824322851,38.9841981594616));
#53581=CARTESIAN_POINT('Ctrl Pts',(22.162391225789,20.5719583490641,39.0572533774481));
#53582=CARTESIAN_POINT('Ctrl Pts',(22.1279042839611,20.5677342658431,39.1285979774431));
#53583=CARTESIAN_POINT('Ctrl Pts',(22.0934283608841,20.5635115322379,39.1999197824805));
#53584=CARTESIAN_POINT('Ctrl Pts',(22.0553505381311,20.5592887986327,39.2695316331428));
#53585=CARTESIAN_POINT('Ctrl Pts',(22.013873680876,20.5550660650275,39.3370542584603));
#53586=CARTESIAN_POINT('Ctrl Pts',(21.9723971633108,20.550843366006,39.4045763307767));
#53587=CARTESIAN_POINT('Ctrl Pts',(21.9275219131607,20.5466206669844,39.4700088131039));
#53588=CARTESIAN_POINT('Ctrl Pts',(21.87949515537,20.5423979679628,39.5329997912912));
#53589=CARTESIAN_POINT('Ctrl Pts',(21.8314206244279,20.5381710685402,39.5960534278315));
#53590=CARTESIAN_POINT('Ctrl Pts',(21.7801886088114,20.5339441691177,39.6566603354425));
#53591=CARTESIAN_POINT('Ctrl Pts',(21.7260874621062,20.5297172696951,39.7145007011642));
#53592=CARTESIAN_POINT('Ctrl Pts',(21.6719600866439,20.525488321031,39.7723691084525));
#53593=CARTESIAN_POINT('Ctrl Pts',(21.6149611465521,20.5212593723669,39.8274679757241));
#53594=CARTESIAN_POINT('Ctrl Pts',(21.5554149711715,20.5170304237028,39.8795153015233));
#53595=CARTESIAN_POINT('Ctrl Pts',(21.4957617723445,20.5127938742708,39.9316561729473));
#53596=CARTESIAN_POINT('Ctrl Pts',(21.4335525594428,20.5085573248387,39.9807342531313));
#53597=CARTESIAN_POINT('Ctrl Pts',(21.3691435720366,20.5043207754067,40.0265088424534));
#53598=CARTESIAN_POINT('Ctrl Pts',(21.3106178253108,20.5004712005408,40.0681022928246));
#53599=CARTESIAN_POINT('Ctrl Pts',(21.2502764098076,20.496621625675,40.1069685961243));
#53600=CARTESIAN_POINT('Ctrl Pts',(21.1884039076456,20.4927720508092,40.142960252475));
#53601=CARTESIAN_POINT('Ctrl Pts',(21.1202957754743,20.4885345083695,40.1825792173162));
#53602=CARTESIAN_POINT('Ctrl Pts',(21.0500763465617,20.4842969659297,40.218862981822));
#53603=CARTESIAN_POINT('Ctrl Pts',(20.9781056839902,20.48005942349,40.2515807472289));
#53604=CARTESIAN_POINT('Ctrl Pts',(20.9062385473929,20.4758279765299,40.2842514498686));
#53605=CARTESIAN_POINT('Ctrl Pts',(20.8326256029833,20.4715965295698,40.3133661476995));
#53606=CARTESIAN_POINT('Ctrl Pts',(20.7576530952229,20.4673650826097,40.3387389817036));
#53607=CARTESIAN_POINT('Ctrl Pts',(20.6827672186168,20.4631385251104,40.3640824972553));
#53608=CARTESIAN_POINT('Ctrl Pts',(20.6065253424046,20.4589119676111,40.3856925918189));
#53609=CARTESIAN_POINT('Ctrl Pts',(20.5293339526429,20.4546854101117,40.4034313550613));
#53610=CARTESIAN_POINT('Ctrl Pts',(20.4521913100054,20.4504615217252,40.4211589160997));
#53611=CARTESIAN_POINT('Ctrl Pts',(20.3741007997041,20.4462376333386,40.435019893715));
#53612=CARTESIAN_POINT('Ctrl Pts',(20.2954831726098,20.442013744952,40.444926466993));
#53613=CARTESIAN_POINT('Ctrl Pts',(20.2168907117464,20.4377912086712,40.4548298690852));
#53614=CARTESIAN_POINT('Ctrl Pts',(20.137771933949,20.4335686723905,40.4607813219791));
#53615=CARTESIAN_POINT('Ctrl Pts',(20.0585553895328,20.4293461361097,40.4627445285635));
#53616=CARTESIAN_POINT('Ctrl Pts',(19.9793395355902,20.4251236366338,40.464707718036));
#53617=CARTESIAN_POINT('Ctrl Pts',(19.9000263854131,20.4209011371578,40.4626827201305));
#53618=CARTESIAN_POINT('Ctrl Pts',(19.8210456905612,20.4166786376819,40.4566853409043));
#53619=CARTESIAN_POINT('Ctrl Pts',(19.7419864678658,20.412451939917,40.4506819986861));
#53620=CARTESIAN_POINT('Ctrl Pts',(19.6632608293097,20.4082252421521,40.440698421369));
#53621=CARTESIAN_POINT('Ctrl Pts',(19.5852939882527,20.4039985443872,40.4268023905611));
#53622=CARTESIAN_POINT('Ctrl Pts',(19.5072893735799,20.3997697988587,40.4128996273612));
#53623=CARTESIAN_POINT('Ctrl Pts',(19.4300447461438,20.3955410533302,40.3950807400925));
#53624=CARTESIAN_POINT('Ctrl Pts',(19.3539731854504,20.3913123078018,40.3734642719389));
#53625=CARTESIAN_POINT('Ctrl Pts',(19.2777648958508,20.3870759616438,40.3518089509471));
#53626=CARTESIAN_POINT('Ctrl Pts',(19.2027343308353,20.3828396154858,40.3263425617609));
#53627=CARTESIAN_POINT('Ctrl Pts',(19.1292772947068,20.3786032693277,40.2972328987586));
#53628=CARTESIAN_POINT('Ctrl Pts',(19.062496193662,20.3747519315152,40.2707687851923));
#53629=CARTESIAN_POINT('Ctrl Pts',(18.9970155875755,20.3709005937027,40.2412942454285));
#53630=CARTESIAN_POINT('Ctrl Pts',(18.93311451783,20.3670492558902,40.2089679487453));
#53631=CARTESIAN_POINT('Ctrl Pts',(18.8628033540714,20.3628115796712,40.1733989113433));
#53632=CARTESIAN_POINT('Ctrl Pts',(18.7941409339877,20.3585739034522,40.1342431012601));
#53633=CARTESIAN_POINT('Ctrl Pts',(18.7275168743918,20.3543362272333,40.0916769657609));
#53634=CARTESIAN_POINT('Ctrl Pts',(18.6609886168593,20.3501046445806,40.0491720382342));
#53635=CARTESIAN_POINT('Ctrl Pts',(18.5964932907581,20.345873061928,40.003266774239));
#53636=CARTESIAN_POINT('Ctrl Pts',(18.5343970626178,20.3416414792753,39.9541840444888));
#53637=CARTESIAN_POINT('Ctrl Pts',(18.4723725518753,20.3374147838454,39.9051580023307));
#53638=CARTESIAN_POINT('Ctrl Pts',(18.4127419986812,20.3331880884155,39.8529620764125));
#53639=CARTESIAN_POINT('Ctrl Pts',(18.3558423626936,20.3289613929855,39.7978622160196));
#53640=CARTESIAN_POINT('Ctrl Pts',(18.2989786407279,20.3247373653694,39.7427971336629));
#53641=CARTESIAN_POINT('Ctrl Pts',(18.2448427504704,20.3205133377532,39.6848320802046));
#53642=CARTESIAN_POINT('Ctrl Pts',(18.1937373959541,20.316289310137,39.6242722349126));
#53643=CARTESIAN_POINT('Ctrl Pts',(18.1426483868449,20.3120666335232,39.5637317589279));
#53644=CARTESIAN_POINT('Ctrl Pts',(18.0945882907818,20.3078439569093,39.5005984971424));
#53645=CARTESIAN_POINT('Ctrl Pts',(18.0498208341514,20.3036212802954,39.4352122160878));
#53646=CARTESIAN_POINT('Ctrl Pts',(18.0050537580744,20.2993986395771,39.3698264908604));
#53647=CARTESIAN_POINT('Ctrl Pts',(17.9635795294206,20.2951759988588,39.302188172045));
#53648=CARTESIAN_POINT('Ctrl Pts',(17.9256188197863,20.2909533581405,39.2326663939904));
#53649=CARTESIAN_POINT('Ctrl Pts',(17.8876203643672,20.2867265186891,39.1630754877741));
#53650=CARTESIAN_POINT('Ctrl Pts',(17.8531426316743,20.2824996792377,39.0915977937849));
#53651=CARTESIAN_POINT('Ctrl Pts',(17.8223602217603,20.2782728397863,39.0186269303302));
#53652=CARTESIAN_POINT('Ctrl Pts',(17.7915628953729,20.2740439521023,38.9456207068131));
#53653=CARTESIAN_POINT('Ctrl Pts',(17.7644646194336,20.2698150644182,38.8711203135116));
#53654=CARTESIAN_POINT('Ctrl Pts',(17.7411908066013,20.2655861767341,38.7955368205332));
#53655=CARTESIAN_POINT('Ctrl Pts',(17.7178751682447,20.2613496892878,38.7198174959552));
#53656=CARTESIAN_POINT('Ctrl Pts',(17.6983978413546,20.2571132018415,38.6430116379728));
#53657=CARTESIAN_POINT('Ctrl Pts',(17.6828335197367,20.2528767143951,38.5655426335408));
#53658=CARTESIAN_POINT('Ctrl Pts',(17.6686887939989,20.2490266299204,38.4951394481165));
#53659=CARTESIAN_POINT('Ctrl Pts',(17.6577752103282,20.2451765454458,38.4241889452537));
#53660=CARTESIAN_POINT('Ctrl Pts',(17.6501115451052,20.2413264609711,38.3530112457031));
#53661=CARTESIAN_POINT('Ctrl Pts',(17.6411212934931,20.2368099238901,38.2695126312));
#53662=CARTESIAN_POINT('Ctrl Pts',(17.6365804216128,20.2322933868092,38.1855264951044));
#53663=CARTESIAN_POINT('Ctrl Pts',(17.6365304175568,20.2277768497283,38.1014049076941));
#53664=CARTESIAN_POINT('',(17.6365302000601,19.4340268497732,38.1009724567951));
#53665=CARTESIAN_POINT('Ctrl Pts',(17.6365304175565,20.2277768497005,38.1014049071763));
#53666=CARTESIAN_POINT('Ctrl Pts',(17.636484138951,20.2235968064934,38.0235505989471));
#53667=CARTESIAN_POINT('Ctrl Pts',(17.6402889455708,20.2194167632863,37.9455442675965));
#53668=CARTESIAN_POINT('Ctrl Pts',(17.6479635155589,20.2152367200793,37.8678043567206));
#53669=CARTESIAN_POINT('Ctrl Pts',(17.6556272462681,20.2110625806106,37.7901742428201));
#53670=CARTESIAN_POINT('Ctrl Pts',(17.6671498382723,20.206888441142,37.7128102782396));
#53671=CARTESIAN_POINT('Ctrl Pts',(17.6824979511222,20.2027143016734,37.636130735716));
#53672=CARTESIAN_POINT('Ctrl Pts',(17.6978340511278,20.1985434292701,37.5595112096529));
#53673=CARTESIAN_POINT('Ctrl Pts',(17.7169896401562,20.1943725568669,37.4835755141203));
#53674=CARTESIAN_POINT('Ctrl Pts',(17.7398797370693,20.1902016844636,37.4087353343398));
#53675=CARTESIAN_POINT('Ctrl Pts',(17.7627594901109,20.1860326968478,37.3339289743031));
#53676=CARTESIAN_POINT('Ctrl Pts',(17.7893702621519,20.1818637092321,37.2602176082695));
#53677=CARTESIAN_POINT('Ctrl Pts',(17.8195766931931,20.1776947216163,37.1879996469116));
#53678=CARTESIAN_POINT('Ctrl Pts',(17.8497794653506,20.1735262389871,37.1157904332647));
#53679=CARTESIAN_POINT('Ctrl Pts',(17.8835768446866,20.1693577563579,37.0450747094514));
#53680=CARTESIAN_POINT('Ctrl Pts',(17.9207852401966,20.1651892737287,36.9762311520977));
#53681=CARTESIAN_POINT('Ctrl Pts',(17.9580268962399,20.1610170648986,36.9073260555832));
#53682=CARTESIAN_POINT('Ctrl Pts',(17.998685430597,20.1568448560685,36.8402968943004));
#53683=CARTESIAN_POINT('Ctrl Pts',(18.0425315311718,20.1526726472385,36.7754972123686));
#53684=CARTESIAN_POINT('Ctrl Pts',(18.086395999869,20.1484986905758,36.7106703843857));
#53685=CARTESIAN_POINT('Ctrl Pts',(18.1334504035067,20.1443247339132,36.648075281336));
#53686=CARTESIAN_POINT('Ctrl Pts',(18.1834239701309,20.1401507772506,36.5880337409171));
#53687=CARTESIAN_POINT('Ctrl Pts',(18.2334869365173,20.1359693536257,36.5278847897251));
#53688=CARTESIAN_POINT('Ctrl Pts',(18.2864791712429,20.1317879300009,36.4702988826972));
#53689=CARTESIAN_POINT('Ctrl Pts',(18.3420920191528,20.1276065063761,36.4155619429782));
#53690=CARTESIAN_POINT('Ctrl Pts',(18.3953045286807,20.1236055596014,36.3631875360599));
#53691=CARTESIAN_POINT('Ctrl Pts',(18.4509157702733,20.1196046128267,36.3134214308127));
#53692=CARTESIAN_POINT('Ctrl Pts',(18.5086289464615,20.115603666052,36.2664780280653));
#53693=CARTESIAN_POINT('Ctrl Pts',(18.5697562366471,20.1113660369581,36.2167576142609));
#53694=CARTESIAN_POINT('Ctrl Pts',(18.6334874181541,20.1071284078643,36.1700040667915));
#53695=CARTESIAN_POINT('Ctrl Pts',(18.6995026334712,20.1028907787704,36.1265013198506));
#53696=CARTESIAN_POINT('Ctrl Pts',(18.7654229125818,20.0986592437933,36.0830611340291));
#53697=CARTESIAN_POINT('Ctrl Pts',(18.8336203142797,20.0944277088162,36.0428627205079));
#53698=CARTESIAN_POINT('Ctrl Pts',(18.9037421375054,20.0901961738392,36.0061496854315));
#53699=CARTESIAN_POINT('Ctrl Pts',(18.9737829633769,20.0859695266862,35.9694790573914));
#53700=CARTESIAN_POINT('Ctrl Pts',(19.0457433801388,20.0817428795332,35.9362860235704));
#53701=CARTESIAN_POINT('Ctrl Pts',(19.119243243195,20.0775162323802,35.9067699673216));
#53702=CARTESIAN_POINT('Ctrl Pts',(19.1926967079603,20.0732922533846,35.8772725436867));
#53703=CARTESIAN_POINT('Ctrl Pts',(19.267687256218,20.069068274389,35.8514476645989));
#53704=CARTESIAN_POINT('Ctrl Pts',(19.343812871453,20.0648442953935,35.8294474475958));
#53705=CARTESIAN_POINT('Ctrl Pts',(19.4199141336261,20.0606216676753,35.8074542686001));
#53706=CARTESIAN_POINT('Ctrl Pts',(19.4971492916794,20.0563990399571,35.7892834520501));
#53707=CARTESIAN_POINT('Ctrl Pts',(19.5751006209999,20.0521764122389,35.7750374285539));
#53708=CARTESIAN_POINT('Ctrl Pts',(19.6530512838556,20.0479538206231,35.7607915268578));
#53709=CARTESIAN_POINT('Ctrl Pts',(19.7317176444084,20.0437312290074,35.7504704343655));
#53710=CARTESIAN_POINT('Ctrl Pts',(19.8106726977706,20.0395086373916,35.7441252975741));
#53711=CARTESIAN_POINT('Ctrl Pts',(19.8897062604247,20.035281847024,35.7377738514689));
#53712=CARTESIAN_POINT('Ctrl Pts',(19.9690286209409,20.0310550566564,35.7354062958549));
#53713=CARTESIAN_POINT('Ctrl Pts',(20.0482091834768,20.0268282662887,35.7370217276648));
#53714=CARTESIAN_POINT('Ctrl Pts',(20.1274281143302,20.0225994277564,35.7386379422601));
#53715=CARTESIAN_POINT('Ctrl Pts',(20.206504642121,20.018370589224,35.7442409559412));
#53716=CARTESIAN_POINT('Ctrl Pts',(20.285012271772,20.0141417506917,35.7537778353619));
#53717=CARTESIAN_POINT('Ctrl Pts',(20.3636609982,20.0099053119364,35.7633318548102));
#53718=CARTESIAN_POINT('Ctrl Pts',(20.4417383205281,20.0056688731811,35.7768337866482));
#53719=CARTESIAN_POINT('Ctrl Pts',(20.5188271578966,20.0014324344259,35.7941793605901));
#53720=CARTESIAN_POINT('Ctrl Pts',(20.588893600923,19.9975819133282,35.8099448424658));
#53721=CARTESIAN_POINT('Ctrl Pts',(20.6581433553679,19.9937313922306,35.8288848728598));
#53722=CARTESIAN_POINT('Ctrl Pts',(20.7262763156345,19.9898808711329,35.8508861402214));
#53723=CARTESIAN_POINT('Ctrl Pts',(20.8012592810361,19.9856432233173,35.8750993883015));
#53724=CARTESIAN_POINT('Ctrl Pts',(20.8751708046757,19.9814055755017,35.9031119602584));
#53725=CARTESIAN_POINT('Ctrl Pts',(20.9475985911541,19.9771679276862,35.934810088943));
#53726=CARTESIAN_POINT('Ctrl Pts',(21.0199222248094,19.9729363737056,35.9664626349894));
#53727=CARTESIAN_POINT('Ctrl Pts',(21.0907659326345,19.9687048197251,36.0017900262271));
#53728=CARTESIAN_POINT('Ctrl Pts',(21.1597333717074,19.9644732657445,36.0406289922775));
#53729=CARTESIAN_POINT('Ctrl Pts',(21.2286211526561,19.9602465992537,36.0794230989098));
#53730=CARTESIAN_POINT('Ctrl Pts',(21.2956365650567,19.956019932763,36.1217204913904));
#53731=CARTESIAN_POINT('Ctrl Pts',(21.3604054249507,19.9517932662722,36.1673108059844));
#53732=CARTESIAN_POINT('Ctrl Pts',(21.4251334013478,19.9475692677442,36.2128723429916));
#53733=CARTESIAN_POINT('Ctrl Pts',(21.4876172576274,19.9433452692162,36.2617224072757));
#53734=CARTESIAN_POINT('Ctrl Pts',(21.5475105542658,19.9391212706881,36.3136065591993));
#53735=CARTESIAN_POINT('Ctrl Pts',(21.607384693123,19.9348986232703,36.3654741151883));
#53736=CARTESIAN_POINT('Ctrl Pts',(21.6646695637755,19.9306759758524,36.4203735248843));
#53737=CARTESIAN_POINT('Ctrl Pts',(21.7190518572336,19.9264533284345,36.4780101254811));
#53738=CARTESIAN_POINT('Ctrl Pts',(21.7734336875416,19.922230716979,36.5356462352124));
#53739=CARTESIAN_POINT('Ctrl Pts',(21.8249126691398,19.9180081055235,36.5960191475558));
#53740=CARTESIAN_POINT('Ctrl Pts',(21.8732134622141,19.9137854940681,36.6587984992098));
#53741=CARTESIAN_POINT('Ctrl Pts',(21.9215622840979,19.9095586837788,36.7216402767027));
#53742=CARTESIAN_POINT('Ctrl Pts',(21.9667263182471,19.9053318734896,36.7868929009139));
#53743=CARTESIAN_POINT('Ctrl Pts',(22.0084719329765,19.9011050632003,36.854194663944));
#53744=CARTESIAN_POINT('Ctrl Pts',(22.0502377769302,19.8968762046698,36.921529040279));
#53745=CARTESIAN_POINT('Ctrl Pts',(22.0885816744786,19.8926473461392,36.9909141227472));
#53746=CARTESIAN_POINT('Ctrl Pts',(22.1233158727043,19.8884184876086,37.0619633216394));
#53747=CARTESIAN_POINT('Ctrl Pts',(22.1581124953498,19.8841820289591,37.1331402103948));
#53748=CARTESIAN_POINT('Ctrl Pts',(22.1892862714249,19.8799455703095,37.2059867594037));
#53749=CARTESIAN_POINT('Ctrl Pts',(22.2166976374358,19.8757091116599,37.2800963318252));
#53750=CARTESIAN_POINT('Ctrl Pts',(22.2416107143402,19.8718587665112,37.3474515112919));
#53751=CARTESIAN_POINT('Ctrl Pts',(22.2634164966769,19.8680084213625,37.4158495119528));
#53752=CARTESIAN_POINT('Ctrl Pts',(22.2820466887331,19.8641580762139,37.4849769505601));
#53753=CARTESIAN_POINT('Ctrl Pts',(22.3025508506449,19.859920433354,37.5610577654804));
#53754=CARTESIAN_POINT('Ctrl Pts',(22.3192846692418,19.8556827904941,37.6383078896525));
#53755=CARTESIAN_POINT('Ctrl Pts',(22.3321191526145,19.8514451476342,37.7163195354094));
#53756=CARTESIAN_POINT('Ctrl Pts',(22.3449351795729,19.8472135986458,37.7942189978223));
#53757=CARTESIAN_POINT('Ctrl Pts',(22.3538629315615,19.8429820496574,37.8728773483324));
#53758=CARTESIAN_POINT('Ctrl Pts',(22.3588236267975,19.8387505006691,37.9518732348229));
#53759=CARTESIAN_POINT('Ctrl Pts',(22.363778592335,19.8345238392013,38.0307778795422));
#53760=CARTESIAN_POINT('Ctrl Pts',(22.3647755775293,19.8302971777336,38.1100188200074));
#53761=CARTESIAN_POINT('Ctrl Pts',(22.3617873675864,19.8260705162658,38.1891676578667));
#53762=CARTESIAN_POINT('Ctrl Pts',(22.3588010438797,19.8218465227772,38.2682665349113));
#53763=CARTESIAN_POINT('Ctrl Pts',(22.3518345357827,19.8176225292887,38.3472729575328));
#53764=CARTESIAN_POINT('Ctrl Pts',(22.3409127046275,19.8133985358001,38.4257578091368));
#53765=CARTESIAN_POINT('Ctrl Pts',(22.3299943670141,19.8091758934309,38.5042175559662));
#53766=CARTESIAN_POINT('Ctrl Pts',(22.3151232833054,19.8049532510617,38.5821555991126));
#53767=CARTESIAN_POINT('Ctrl Pts',(22.2963760908792,19.8007306086925,38.6591487191602));
#53768=CARTESIAN_POINT('Ctrl Pts',(22.277629058124,19.7965080022878,38.7361411834523));
#53769=CARTESIAN_POINT('Ctrl Pts',(22.2550060945822,19.7922853958832,38.8121882855207));
#53770=CARTESIAN_POINT('Ctrl Pts',(22.2286344535998,19.7880627894785,38.8868792239778));
#53771=CARTESIAN_POINT('Ctrl Pts',(22.2022365892431,19.7838359842078,38.9616444334458));
#53772=CARTESIAN_POINT('Ctrl Pts',(22.1720827579782,19.7796091789371,39.0350503425325));
#53773=CARTESIAN_POINT('Ctrl Pts',(22.1383492103446,19.7753823736664,39.1067040754455));
#53774=CARTESIAN_POINT('Ctrl Pts',(22.1045993159032,19.7711535201446,39.1783925307605));
#53775=CARTESIAN_POINT('Ctrl Pts',(22.0672664704473,19.7669246666229,39.2483267043674));
#53776=CARTESIAN_POINT('Ctrl Pts',(22.0265727705049,19.7626958131012,39.316138662632));
#53777=CARTESIAN_POINT('Ctrl Pts',(21.9858059348948,19.7584593593851,39.3840724941313));
#53778=CARTESIAN_POINT('Ctrl Pts',(21.9416664376352,19.7542229056691,39.4498760991301));
#53779=CARTESIAN_POINT('Ctrl Pts',(21.8944194233604,19.7499864519531,39.5132110561749));
#53780=CARTESIAN_POINT('Ctrl Pts',(21.8514779789693,19.7461360617336,39.5707743663161));
#53781=CARTESIAN_POINT('Ctrl Pts',(21.8059702735828,19.7422856715142,39.6262986659425));
#53782=CARTESIAN_POINT('Ctrl Pts',(21.758122026966,19.7384352812947,39.6795560702923));
#53783=CARTESIAN_POINT('Ctrl Pts',(21.7054614747271,19.7341976406364,39.7381698027102));
#53784=CARTESIAN_POINT('Ctrl Pts',(21.6497676973461,19.7299599999782,39.7942572176017));
#53785=CARTESIAN_POINT('Ctrl Pts',(21.5913125590873,19.7257223593199,39.8474881344922));
#53786=CARTESIAN_POINT('Ctrl Pts',(21.5329414820595,19.7214908125876,39.9006425028271));
#53787=CARTESIAN_POINT('Ctrl Pts',(21.471817273861,19.7172592658554,39.9509482178125));
#53788=CARTESIAN_POINT('Ctrl Pts',(21.4082505087409,19.7130277191232,39.9981098349493));
#53789=CARTESIAN_POINT('Ctrl Pts',(21.3447571655755,19.7088010599833,40.0452169786814));
#53790=CARTESIAN_POINT('Ctrl Pts',(21.2788272465766,19.7045744008434,40.0891869634653));
#53791=CARTESIAN_POINT('Ctrl Pts',(21.2108053066442,19.7003477417035,40.1297637671173));
#53792=CARTESIAN_POINT('Ctrl Pts',(21.1428263046473,19.6961237505853,40.1703149572074));
#53793=CARTESIAN_POINT('Ctrl Pts',(21.0727583044157,19.6918997594672,40.2074769780759));
#53794=CARTESIAN_POINT('Ctrl Pts',(21.0009748102995,19.6876757683491,40.2410371015108));
#53795=CARTESIAN_POINT('Ctrl Pts',(20.9292142780913,19.6834531283897,40.2745864898252));
#53796=CARTESIAN_POINT('Ctrl Pts',(20.8557397660526,19.6792304884303,40.3045360702867));
#53797=CARTESIAN_POINT('Ctrl Pts',(20.7809480151741,19.6750078484709,40.3307197579471));
#53798=CARTESIAN_POINT('Ctrl Pts',(20.7061569019417,19.6707852445122,40.3569032223753));
#53799=CARTESIAN_POINT('Ctrl Pts',(20.6300490151142,19.6665626405534,40.3793207042952));
#53800=CARTESIAN_POINT('Ctrl Pts',(20.5530382307178,19.6623400365946,40.3978553384111));
#53801=CARTESIAN_POINT('Ctrl Pts',(20.4759508691915,19.6581132338098,40.416408402791));
#53802=CARTESIAN_POINT('Ctrl Pts',(20.3979592735295,19.6538864310249,40.4310707970902));
#53803=CARTESIAN_POINT('Ctrl Pts',(20.3194889535093,19.6496596282401,40.4417765157003));
#53804=CARTESIAN_POINT('Ctrl Pts',(20.2409806083215,19.64543077723,40.4524874220903));
#53805=CARTESIAN_POINT('Ctrl Pts',(20.1619935443124,19.64120192622,40.4592377932839));
#53806=CARTESIAN_POINT('Ctrl Pts',(20.0829573037273,19.63697307521,40.462013659287));
#53807=CARTESIAN_POINT('Ctrl Pts',(20.003779017554,19.6327366240203,40.4647945141347));
#53808=CARTESIAN_POINT('Ctrl Pts',(19.9245518480421,19.6285001728305,40.4635865984202));
#53809=CARTESIAN_POINT('Ctrl Pts',(19.8457040132688,19.6242637216408,40.4584281183404));
#53810=CARTESIAN_POINT('Ctrl Pts',(19.7740410538062,19.6204133098858,40.4537396960152));
#53811=CARTESIAN_POINT('Ctrl Pts',(19.702691649299,19.6165628981307,40.4457885773075));
#53812=CARTESIAN_POINT('Ctrl Pts',(19.6319698377279,19.6127124863756,40.4346400665966));
#53813=CARTESIAN_POINT('Ctrl Pts',(19.5541356153086,19.6084748431607,40.422370363049));
#53814=CARTESIAN_POINT('Ctrl Pts',(19.4767695491811,19.6042371999458,40.4061810158533));
#53815=CARTESIAN_POINT('Ctrl Pts',(19.4002966028418,19.5999995567309,40.3861203547357));
#53816=CARTESIAN_POINT('Ctrl Pts',(19.3239336273925,19.5957680074017,40.3660885415815));
#53817=CARTESIAN_POINT('Ctrl Pts',(19.2484616708388,19.5915364580726,40.3421965881955));
#53818=CARTESIAN_POINT('Ctrl Pts',(19.174297628942,19.5873049087434,40.3145442048713));
#53819=CARTESIAN_POINT('Ctrl Pts',(19.1002192483423,19.583078246958,40.2869237607317));
#53820=CARTESIAN_POINT('Ctrl Pts',(19.0274462173227,19.5788515851727,40.255551681003));
#53821=CARTESIAN_POINT('Ctrl Pts',(18.9563808583605,19.5746249233873,40.220577640197));
#53822=CARTESIAN_POINT('Ctrl Pts',(18.8853603579469,19.5704009295954,40.1856256760362));
#53823=CARTESIAN_POINT('Ctrl Pts',(18.8160458095101,19.5661769358035,40.1470764702211));
#53824=CARTESIAN_POINT('Ctrl Pts',(18.7488189757804,19.5619529420116,40.1051275484449));
#53825=CARTESIAN_POINT('Ctrl Pts',(18.6816136459818,19.5577302993539,40.0631920449227));
#53826=CARTESIAN_POINT('Ctrl Pts',(18.6164951021841,19.5535076566961,40.0178592329244));
#53827=CARTESIAN_POINT('Ctrl Pts',(18.5538186280841,19.5492850140384,39.9693715201702));
#53828=CARTESIAN_POINT('Ctrl Pts',(18.4911426880302,19.5450624073605,39.9208842205643));
#53829=CARTESIAN_POINT('Ctrl Pts',(18.4309091461991,19.5408398006825,39.8692423616193));
#53830=CARTESIAN_POINT('Ctrl Pts',(18.3734413246954,19.5366171940046,39.8147295170642));
#53831=CARTESIAN_POINT('Ctrl Pts',(18.3159163588249,19.5323903884867,39.7601624664873));
#53832=CARTESIAN_POINT('Ctrl Pts',(18.261162947618,19.5281635829688,39.7027190511352));
#53833=CARTESIAN_POINT('Ctrl Pts',(18.2094680812797,19.5239367774509,39.6427202886278));
#53834=CARTESIAN_POINT('Ctrl Pts',(18.1577481645001,19.5197079236959,39.5826924517541));
#53835=CARTESIAN_POINT('Ctrl Pts',(18.1090900332376,19.5154790699409,39.5201071714882));
#53836=CARTESIAN_POINT('Ctrl Pts',(18.0637392217108,19.5112502161859,39.4553171729743));
#53837=CARTESIAN_POINT('Ctrl Pts',(18.0183069049348,19.507013762263,39.3904107327738));
#53838=CARTESIAN_POINT('Ctrl Pts',(17.9761940342619,19.5027773083402,39.3232920551766));
#53839=CARTESIAN_POINT('Ctrl Pts',(17.9376016541955,19.4985408544173,39.2543411558647));
#53840=CARTESIAN_POINT('Ctrl Pts',(17.9025261815392,19.4946904667638,39.1916737230896));
#53841=CARTESIAN_POINT('Ctrl Pts',(17.870358322029,19.4908400791102,39.1274933400953));
#53842=CARTESIAN_POINT('Ctrl Pts',(17.8412142337764,19.4869896914566,39.0620989847467));
#53843=CARTESIAN_POINT('Ctrl Pts',(17.8061044677336,19.4823511449177,38.9833186675543));
#53844=CARTESIAN_POINT('Ctrl Pts',(17.7752695283484,19.4777125983789,38.9025216574394));
#53845=CARTESIAN_POINT('Ctrl Pts',(17.7489228730776,19.47307405184,38.820168181432));
#53846=CARTESIAN_POINT('Ctrl Pts',(17.7226474238737,19.468448041718,38.7380372789183));
#53847=CARTESIAN_POINT('Ctrl Pts',(17.7008361972315,19.4638220315961,38.654358589239));
#53848=CARTESIAN_POINT('Ctrl Pts',(17.6836548021214,19.4591960214741,38.5696119303901));
#53849=CARTESIAN_POINT('Ctrl Pts',(17.6665514361944,19.4545910203441,38.4852501478869));
#53850=CARTESIAN_POINT('Ctrl Pts',(17.6540360738757,19.4499860192141,38.3998303703967));
#53851=CARTESIAN_POINT('Ctrl Pts',(17.6462241266023,19.4453810180841,38.3138447537604));
#53852=CARTESIAN_POINT('Ctrl Pts',(17.6398037036987,19.4415962953138,38.2431755591149));
#53853=CARTESIAN_POINT('Ctrl Pts',(17.6365594758146,19.4378115725435,38.1721245756472));
#53854=CARTESIAN_POINT('Ctrl Pts',(17.6365302000601,19.4340268497732,38.1009724567951));
#53855=CARTESIAN_POINT('',(17.6365309432187,18.6402768496835,38.0978884751228));
#53856=CARTESIAN_POINT('Ctrl Pts',(17.6365302000598,19.4340268497283,38.1009724559519));
#53857=CARTESIAN_POINT('Ctrl Pts',(17.63649691118,19.4297233127912,38.0200667225018));
#53858=CARTESIAN_POINT('Ctrl Pts',(17.6406222859428,19.4254197758541,37.9391804309353));
#53859=CARTESIAN_POINT('Ctrl Pts',(17.6488740476656,19.421116238917,37.8587590475074));
#53860=CARTESIAN_POINT('Ctrl Pts',(17.6571302401675,19.416810391198,37.7782944818598));
#53861=CARTESIAN_POINT('Ctrl Pts',(17.6695171805407,19.412504543479,37.6982957614949));
#53862=CARTESIAN_POINT('Ctrl Pts',(17.6859509702447,19.40819869576,37.6192011555873));
#53863=CARTESIAN_POINT('Ctrl Pts',(17.7024111899348,19.4038859230713,37.5399793441248));
#53864=CARTESIAN_POINT('Ctrl Pts',(17.722931163855,19.3995731503826,37.4616649852144));
#53865=CARTESIAN_POINT('Ctrl Pts',(17.7473763108829,19.3952603776939,37.3846840165853));
#53866=CARTESIAN_POINT('Ctrl Pts',(17.7718426238678,19.3909438707687,37.3076363935866));
#53867=CARTESIAN_POINT('Ctrl Pts',(17.8002407241596,19.3866273638435,37.2319248753286));
#53868=CARTESIAN_POINT('Ctrl Pts',(17.8323876855168,19.3823108569183,37.1579557892536));
#53869=CARTESIAN_POINT('Ctrl Pts',(17.864600726392,19.3779854772199,37.0838346564112));
#53870=CARTESIAN_POINT('Ctrl Pts',(17.9005778246042,19.3736600975215,37.0114635075962));
#53871=CARTESIAN_POINT('Ctrl Pts',(17.9400898782929,19.3693347178231,36.9412244689378));
#53872=CARTESIAN_POINT('Ctrl Pts',(17.9646562138912,19.3666454440612,36.8975538511211));
#53873=CARTESIAN_POINT('Ctrl Pts',(17.9905881561757,19.3639561702994,36.8547068782714));
#53874=CARTESIAN_POINT('Ctrl Pts',(18.0178225475708,19.3612668965376,36.8127692561234));
#53875=CARTESIAN_POINT('Ctrl Pts',(18.0607373325429,19.357029254376,36.7466857512411));
#53876=CARTESIAN_POINT('Ctrl Pts',(18.1070410082588,19.3527916122144,36.6826266423791));
#53877=CARTESIAN_POINT('Ctrl Pts',(18.1565163086918,19.3485539700528,36.6209603383341));
#53878=CARTESIAN_POINT('Ctrl Pts',(18.2059204616512,19.3443224217913,36.5593827129168));
#53879=CARTESIAN_POINT('Ctrl Pts',(18.2584868908242,19.3400908735297,36.5001914215271));
#53880=CARTESIAN_POINT('Ctrl Pts',(18.3139546935983,19.3358593252681,36.4437265727964));
#53881=CARTESIAN_POINT('Ctrl Pts',(18.3693584294601,19.3316326645669,36.3873269425949));
#53882=CARTESIAN_POINT('Ctrl Pts',(18.4276565524602,19.3274060038657,36.3336478296785));
#53883=CARTESIAN_POINT('Ctrl Pts',(18.4885484672282,19.3231793431644,36.2829956783261));
#53884=CARTESIAN_POINT('Ctrl Pts',(18.5494019450779,19.3189553504662,36.2323755002267));
#53885=CARTESIAN_POINT('Ctrl Pts',(18.6128456054235,19.314731357768,36.1847787901325));
#53886=CARTESIAN_POINT('Ctrl Pts',(18.6785435287391,19.3105073650697,36.1404737216708));
#53887=CARTESIAN_POINT('Ctrl Pts',(18.7442204370482,19.3062847235136,36.0961828252142));
#53888=CARTESIAN_POINT('Ctrl Pts',(18.8121497880337,19.3020620819576,36.0551817414331));
#53889=CARTESIAN_POINT('Ctrl Pts',(18.8819654611021,19.2978394404015,36.0176961771318));
#53890=CARTESIAN_POINT('Ctrl Pts',(18.9517805391862,19.2936168348317,35.9802109322907));
#53891=CARTESIAN_POINT('Ctrl Pts',(19.0234814937076,19.2893942292619,35.9462413678524));
#53892=CARTESIAN_POINT('Ctrl Pts',(19.0966776302458,19.2851716236921,35.91596723074));
#53893=CARTESIAN_POINT('Ctrl Pts',(19.1699465509169,19.2809448192847,35.8856629898964));
#53894=CARTESIAN_POINT('Ctrl Pts',(19.2447131892359,19.2767180148774,35.8590616960446));
#53895=CARTESIAN_POINT('Ctrl Pts',(19.3205674566373,19.2724912104701,35.8362946614191));
#53896=CARTESIAN_POINT('Ctrl Pts',(19.3964584816635,19.2682623578287,35.8135165942948));
#53897=CARTESIAN_POINT('Ctrl Pts',(19.4734377299283,19.2640335051874,35.7945765999174));
#53898=CARTESIAN_POINT('Ctrl Pts',(19.5510830450083,19.2598046525461,35.7795552132358));
#53899=CARTESIAN_POINT('Ctrl Pts',(19.6288679057476,19.2555681997291,35.7645068298282));
#53900=CARTESIAN_POINT('Ctrl Pts',(19.7073207599213,19.2513317469122,35.7533911918268));
#53901=CARTESIAN_POINT('Ctrl Pts',(19.7860126529992,19.2470952940952,35.7462370858084));
#53902=CARTESIAN_POINT('Ctrl Pts',(19.8575335882865,19.2432448966029,35.7397349121592));
#53903=CARTESIAN_POINT('Ctrl Pts',(19.9292516733776,19.2393944991107,35.7365045079458));
#53904=CARTESIAN_POINT('Ctrl Pts',(20.0008465413715,19.2355441016184,35.736530151606));
#53905=CARTESIAN_POINT('Ctrl Pts',(20.0796419011123,19.2313064591162,35.7365583743193));
#53906=CARTESIAN_POINT('Ctrl Pts',(20.1585837540419,19.2270688166141,35.7405313790339));
#53907=CARTESIAN_POINT('Ctrl Pts',(20.2372447882762,19.2228311741119,35.7484674462522));
#53908=CARTESIAN_POINT('Ctrl Pts',(20.3157927048903,19.2185996255041,35.7563921010978));
#53909=CARTESIAN_POINT('Ctrl Pts',(20.3940601422223,19.2143680768964,35.7682684540193));
#53910=CARTESIAN_POINT('Ctrl Pts',(20.4716197755453,19.2101365282886,35.7840627754158));
#53911=CARTESIAN_POINT('Ctrl Pts',(20.5490898253874,19.2059098672343,35.7998388539426));
#53912=CARTESIAN_POINT('Ctrl Pts',(20.6258532388433,19.2016832061799,35.8195238148475));
#53913=CARTESIAN_POINT('Ctrl Pts',(20.7014893249499,19.1974565451256,35.8430323068592));
#53914=CARTESIAN_POINT('Ctrl Pts',(20.7770776672229,19.1932325520703,35.8665259595846));
#53915=CARTESIAN_POINT('Ctrl Pts',(20.8515396481232,19.189008559015,35.8938382140542));
#53916=CARTESIAN_POINT('Ctrl Pts',(20.9244674525116,19.1847845659597,35.9248332546339));
#53917=CARTESIAN_POINT('Ctrl Pts',(20.9973719293108,19.180561924043,35.9558183807567));
#53918=CARTESIAN_POINT('Ctrl Pts',(21.068742772998,19.1763392821263,35.9904837704438));
#53919=CARTESIAN_POINT('Ctrl Pts',(21.1381913529671,19.1721166402096,36.0286451571662));
#53920=CARTESIAN_POINT('Ctrl Pts',(21.20763934113,19.1678940342762,36.0668062186963));
#53921=CARTESIAN_POINT('Ctrl Pts',(21.2751646879985,19.1636714283428,36.1084629910251));
#53922=CARTESIAN_POINT('Ctrl Pts',(21.3404039408185,19.1594488224093,36.1533855758424));
#53923=CARTESIAN_POINT('Ctrl Pts',(21.4057080657035,19.1552220176362,36.1983528304057));
#53924=CARTESIAN_POINT('Ctrl Pts',(21.4687211687671,19.150995212863,36.2465921177412));
#53925=CARTESIAN_POINT('Ctrl Pts',(21.529109870627,19.1467684080899,36.2978309056997));
#53926=CARTESIAN_POINT('Ctrl Pts',(21.5895278357976,19.1425395550809,36.3490945230804));
#53927=CARTESIAN_POINT('Ctrl Pts',(21.6473185241433,19.1383107020719,36.40336021534));
#53928=CARTESIAN_POINT('Ctrl Pts',(21.702184582739,19.134081849063,36.4603176871157));
#53929=CARTESIAN_POINT('Ctrl Pts',(21.7571492476496,19.1298453958797,36.5173775239335));
#53930=CARTESIAN_POINT('Ctrl Pts',(21.809178471871,19.1256089426963,36.5771384521025));
#53931=CARTESIAN_POINT('Ctrl Pts',(21.8580146120605,19.121372489513,36.6392563050728));
#53932=CARTESIAN_POINT('Ctrl Pts',(21.9024004193097,19.1175220952418,36.6957134910415));
#53933=CARTESIAN_POINT('Ctrl Pts',(21.9441489652272,19.1136717009706,36.7541169965109));
#53934=CARTESIAN_POINT('Ctrl Pts',(21.9830990514481,19.1098213066993,36.8141895190015));
#53935=CARTESIAN_POINT('Ctrl Pts',(22.0259664888743,19.1055836643344,36.8803037525952));
#53936=CARTESIAN_POINT('Ctrl Pts',(22.0656045182654,19.1013460219694,36.9486881595004));
#53937=CARTESIAN_POINT('Ctrl Pts',(22.1017652036544,19.0971083796045,37.0189942323893));
#53938=CARTESIAN_POINT('Ctrl Pts',(22.1378738885597,19.0928768311355,37.0891992023881));
#53939=CARTESIAN_POINT('Ctrl Pts',(22.1705149474696,19.0886452826664,37.16131993703));
#53940=CARTESIAN_POINT('Ctrl Pts',(22.1994840670144,19.0844137341974,37.2349796072636));
#53941=CARTESIAN_POINT('Ctrl Pts',(22.2284197264279,19.0801870732834,37.3085541985484));
#53942=CARTESIAN_POINT('Ctrl Pts',(22.2536917040894,19.0759604123695,37.3836637590193));
#53943=CARTESIAN_POINT('Ctrl Pts',(22.2751426013675,19.0717337514555,37.4599089249624));
#53944=CARTESIAN_POINT('Ctrl Pts',(22.2965799581715,19.0675097585415,37.5361059625835));
#53945=CARTESIAN_POINT('Ctrl Pts',(22.3142008954915,19.0632857656275,37.6134367327756));
#53946=CARTESIAN_POINT('Ctrl Pts',(22.3278973563818,19.0590617727134,37.6914852033883));
#53947=CARTESIAN_POINT('Ctrl Pts',(22.3415894361502,19.0548391309388,37.7695087084378));
#53948=CARTESIAN_POINT('Ctrl Pts',(22.3513594513638,19.0506164891641,37.848248996637));
#53949=CARTESIAN_POINT('Ctrl Pts',(22.3571504317852,19.0463938473895,37.927279755573));
#53950=CARTESIAN_POINT('Ctrl Pts',(22.362941362858,19.0421712415986,38.0063098410382));
#53951=CARTESIAN_POINT('Ctrl Pts',(22.3647532937258,19.0379486358077,38.0856299246948));
#53952=CARTESIAN_POINT('Ctrl Pts',(22.3625812383724,19.0337260300168,38.1648099760127));
#53953=CARTESIAN_POINT('Ctrl Pts',(22.3604070231885,19.0294992253861,38.2440687617366));
#53954=CARTESIAN_POINT('Ctrl Pts',(22.3542409214272,19.0252724207553,38.3231867672943));
#53955=CARTESIAN_POINT('Ctrl Pts',(22.3441300812228,19.0210456161245,38.4017359826181));
#53956=CARTESIAN_POINT('Ctrl Pts',(22.3340143414819,19.0168167632581,38.4803232615191));
#53957=CARTESIAN_POINT('Ctrl Pts',(22.3199501385357,19.0125879103916,38.55834073918));
#53958=CARTESIAN_POINT('Ctrl Pts',(22.3020359093354,19.0083590575252,38.6353700711007));
#53959=CARTESIAN_POINT('Ctrl Pts',(22.2840894843374,19.0041226044829,38.7125378416199));
#53960=CARTESIAN_POINT('Ctrl Pts',(22.2622793369081,18.9998861514407,38.7887134662149));
#53961=CARTESIAN_POINT('Ctrl Pts',(22.2367539327763,18.9956496983985,38.8634934741764));
#53962=CARTESIAN_POINT('Ctrl Pts',(22.2135545956821,18.9917993028591,38.931458964699));
#53963=CARTESIAN_POINT('Ctrl Pts',(22.1872869971439,18.9879489073197,38.9982715923177));
#53964=CARTESIAN_POINT('Ctrl Pts',(22.1580960113827,18.9840985117803,39.0636451870654));
#53965=CARTESIAN_POINT('Ctrl Pts',(22.1259691931705,18.9798608694289,39.1355936170194));
#53966=CARTESIAN_POINT('Ctrl Pts',(22.0901801186355,18.9756232270776,39.2060687372696));
#53967=CARTESIAN_POINT('Ctrl Pts',(22.050886178917,18.9713855847262,39.274672857449));
#53968=CARTESIAN_POINT('Ctrl Pts',(22.011648745431,18.9671540362714,39.3431783222022));
#53969=CARTESIAN_POINT('Ctrl Pts',(21.9689166870622,18.9629224878167,39.4098177266965));
#53970=CARTESIAN_POINT('Ctrl Pts',(21.9228948984556,18.9586909393619,39.4742145576268));
#53971=CARTESIAN_POINT('Ctrl Pts',(21.8769262662932,18.9544642784631,39.5385370084286));
#53972=CARTESIAN_POINT('Ctrl Pts',(21.8276757260957,18.9502376175643,39.6006216536557));
#53973=CARTESIAN_POINT('Ctrl Pts',(21.7753926134654,18.9460109566655,39.6601190688382));
#53974=CARTESIAN_POINT('Ctrl Pts',(21.72314250357,18.9417869637672,39.7195789273925));
#53975=CARTESIAN_POINT('Ctrl Pts',(21.667863929452,18.9375629708689,39.7764544462935));
#53976=CARTESIAN_POINT('Ctrl Pts',(21.6098470677578,18.9333389779706,39.8304285189894));
#53977=CARTESIAN_POINT('Ctrl Pts',(21.5518487640723,18.9291163362122,39.8843853268543));
#53978=CARTESIAN_POINT('Ctrl Pts',(21.4911142551494,18.9248936944538,39.9354422124553));
#53979=CARTESIAN_POINT('Ctrl Pts',(21.4279701497255,18.9206710526954,39.9833193283118));
#53980=CARTESIAN_POINT('Ctrl Pts',(21.3648265823997,18.9164484469212,40.0311960361717));
#53981=CARTESIAN_POINT('Ctrl Pts',(21.2992738338036,18.9122258411471,40.0758927460787));
#53982=CARTESIAN_POINT('Ctrl Pts',(21.2316699285407,18.908003235373,40.1171711945268));
#53983=CARTESIAN_POINT('Ctrl Pts',(21.163998799875,18.9037764307596,40.1584906890913));
#53984=CARTESIAN_POINT('Ctrl Pts',(21.0942728414268,18.8995496261463,40.1963848877761));
#53985=CARTESIAN_POINT('Ctrl Pts',(21.0228767613701,18.895322821533,40.2306603605336));
#53986=CARTESIAN_POINT('Ctrl Pts',(20.9514460840272,18.8910939686844,40.264952442583));
#53987=CARTESIAN_POINT('Ctrl Pts',(20.8783441056562,18.8868651158357,40.295622123797));
#53988=CARTESIAN_POINT('Ctrl Pts',(20.8039753446254,18.8826362629871,40.3225242599654));
#53989=CARTESIAN_POINT('Ctrl Pts',(20.729472926633,18.8783998099632,40.3494747451681));
#53990=CARTESIAN_POINT('Ctrl Pts',(20.6536996262899,18.8741633569393,40.3726440186046));
#53991=CARTESIAN_POINT('Ctrl Pts',(20.5770747172652,18.8699269039153,40.391936999918));
#53992=CARTESIAN_POINT('Ctrl Pts',(20.5074324440273,18.8660765082306,40.4094718602305));
#53993=CARTESIAN_POINT('Ctrl Pts',(20.4370871063224,18.8622261125459,40.4238053109777));
#53994=CARTESIAN_POINT('Ctrl Pts',(20.3663576230851,18.8583757168611,40.4349031099614));
#53995=CARTESIAN_POINT('Ctrl Pts',(20.2885146476296,18.8541380744656,40.4471170503772));
#53996=CARTESIAN_POINT('Ctrl Pts',(20.20991408771,18.8499004320701,40.4554568677485));
#53997=CARTESIAN_POINT('Ctrl Pts',(20.130975226485,18.8456627896745,40.4598381154111));
#53998=CARTESIAN_POINT('Ctrl Pts',(20.0521498824351,18.8414312411748,40.464213062668));
#53999=CARTESIAN_POINT('Ctrl Pts',(19.9729876673909,18.837199692675,40.4646407193865));
#54000=CARTESIAN_POINT('Ctrl Pts',(19.8939159576045,18.8329681441752,40.4610880154812));
#54001=CARTESIAN_POINT('Ctrl Pts',(19.8149355778206,18.8287414832305,40.4575394150468));
#54002=CARTESIAN_POINT('Ctrl Pts',(19.7360459614858,18.8245148222859,40.4500196111653));
#54003=CARTESIAN_POINT('Ctrl Pts',(19.6576759516972,18.8202881613412,40.4385475592456));
#54004=CARTESIAN_POINT('Ctrl Pts',(19.5793554114975,18.8160641683964,40.4270827488421));
#54005=CARTESIAN_POINT('Ctrl Pts',(19.5015542894333,18.8118401754516,40.4116707099863));
#54006=CARTESIAN_POINT('Ctrl Pts',(19.4246965493785,18.8076161825068,40.3923822501064));
#54007=CARTESIAN_POINT('Ctrl Pts',(19.3478633940053,18.8033935407014,40.3730999600755));
#54008=CARTESIAN_POINT('Ctrl Pts',(19.2719734757476,18.7991708988961,40.3499438253615));
#54009=CARTESIAN_POINT('Ctrl Pts',(19.1974393343323,18.7949482570907,40.3230354965279));
#54010=CARTESIAN_POINT('Ctrl Pts',(19.1229058280705,18.7907256512692,40.2961273969976));
#54011=CARTESIAN_POINT('Ctrl Pts',(19.0497285161126,18.7865030454477,40.2654673274486));
#54012=CARTESIAN_POINT('Ctrl Pts',(18.9783021555091,18.7822804396262,40.2312259278318));
#54013=CARTESIAN_POINT('Ctrl Pts',(18.9068047705569,18.7780536349651,40.1969504795378));
#54014=CARTESIAN_POINT('Ctrl Pts',(18.8370622384995,18.773826830304,40.1590867908324));
#54015=CARTESIAN_POINT('Ctrl Pts',(18.7694462318672,18.769600025643,40.1178522900932));
#54016=CARTESIAN_POINT('Ctrl Pts',(18.7017974597021,18.7653711727464,40.0765978078369));
#54017=CARTESIAN_POINT('Ctrl Pts',(18.6362776537237,18.7611423198498,40.0319695237864));
#54018=CARTESIAN_POINT('Ctrl Pts',(18.5732287644304,18.7569134669532,39.9842277681457));
#54019=CARTESIAN_POINT('Ctrl Pts',(18.510066562469,18.7526770138814,39.9364002101098));
#54020=CARTESIAN_POINT('Ctrl Pts',(18.4493845101543,18.7484405608096,39.8854483021046));
#54021=CARTESIAN_POINT('Ctrl Pts',(18.3914905928753,18.7442041077378,39.8316720036114));
#54022=CARTESIAN_POINT('Ctrl Pts',(18.3388724094092,18.7403537124725,39.7827962102079));
#54023=CARTESIAN_POINT('Ctrl Pts',(18.2885570812017,18.7365033172073,39.7315879983667));
#54024=CARTESIAN_POINT('Ctrl Pts',(18.2407469317621,18.7326529219421,39.6782962595139));
#54025=CARTESIAN_POINT('Ctrl Pts',(18.1886714455363,18.7284590173434,39.6202501491145));
#54026=CARTESIAN_POINT('Ctrl Pts',(18.1393638736236,18.7242651127447,39.5595033357046));
#54027=CARTESIAN_POINT('Ctrl Pts',(18.0931208954266,18.720071208146,39.4963532939201));
#54028=CARTESIAN_POINT('Ctrl Pts',(18.0469392292103,18.7158828641017,39.4332869806126));
#54029=CARTESIAN_POINT('Ctrl Pts',(18.0038143777873,18.7116945200574,39.3678241414009));
#54030=CARTESIAN_POINT('Ctrl Pts',(17.9640048148198,18.7075061760132,39.3002974826363));
#54031=CARTESIAN_POINT('Ctrl Pts',(17.9242350131353,18.7033220152335,39.232838268636));
#54032=CARTESIAN_POINT('Ctrl Pts',(17.8877741716712,18.6991378544537,39.1633197354723));
#54033=CARTESIAN_POINT('Ctrl Pts',(17.8548382602009,18.694953693674,39.0921046068849));
#54034=CARTESIAN_POINT('Ctrl Pts',(17.8219244767009,18.6907723440199,39.0209373241344));
#54035=CARTESIAN_POINT('Ctrl Pts',(17.7925311220298,18.6865909943659,38.9480761426687));
#54036=CARTESIAN_POINT('Ctrl Pts',(17.7668280953728,18.6824096447118,38.8739080599681));
#54037=CARTESIAN_POINT('Ctrl Pts',(17.7411275740086,18.6782287026169,38.7997472064849));
#54038=CARTESIAN_POINT('Ctrl Pts',(17.7191168349262,18.674047760522,38.7242801531567));
#54039=CARTESIAN_POINT('Ctrl Pts',(17.700917020489,18.6698668184272,38.6479123052303));
#54040=CARTESIAN_POINT('Ctrl Pts',(17.6827181465883,18.6656860923965,38.5715484038688));
#54041=CARTESIAN_POINT('Ctrl Pts',(17.6683299089655,18.6615053663659,38.494284268536));
#54042=CARTESIAN_POINT('Ctrl Pts',(17.6578226295373,18.6573246403352,38.4165368954679));
#54043=CARTESIAN_POINT('Ctrl Pts',(17.647308431712,18.6531411615537,38.338738330537));
#54044=CARTESIAN_POINT('Ctrl Pts',(17.6406803453056,18.6489576827721,38.2604563692487));
#54045=CARTESIAN_POINT('Ctrl Pts',(17.6379568524747,18.6447742039905,38.1821133979853));
#54046=CARTESIAN_POINT('Ctrl Pts',(17.6369809093477,18.6432750859031,38.1540397847621));
#54047=CARTESIAN_POINT('Ctrl Pts',(17.6365058655876,18.6417759678157,38.125958345013));
#54048=CARTESIAN_POINT('Ctrl Pts',(17.6365309432179,18.6402768497283,38.0978884759611));
#54049=CARTESIAN_POINT('',(17.6365300981239,17.8465268496895,38.1006810474926));
#54050=CARTESIAN_POINT('Ctrl Pts',(17.6365309432187,18.6402768496835,38.0978884751228));
#54051=CARTESIAN_POINT('Ctrl Pts',(17.6366239153381,18.6347190625734,37.9938230531207));
#54052=CARTESIAN_POINT('Ctrl Pts',(17.6435944777715,18.6291612754634,37.8900613092647));
#54053=CARTESIAN_POINT('Ctrl Pts',(17.6572963530161,18.6236034883533,37.7873819210152));
#54054=CARTESIAN_POINT('Ctrl Pts',(17.6709982282606,18.6180457012432,37.6847025327657));
#54055=CARTESIAN_POINT('Ctrl Pts',(17.6914312182393,18.6124879141331,37.5831051765486));
#54056=CARTESIAN_POINT('Ctrl Pts',(17.7183944712534,18.606930127023,37.4833423542249));
#54057=CARTESIAN_POINT('Ctrl Pts',(17.7389531254918,18.6026924846485,37.4072762590498));
#54058=CARTESIAN_POINT('Ctrl Pts',(17.7633584640601,18.598454842274,37.3320966078432));
#54059=CARTESIAN_POINT('Ctrl Pts',(17.7915167929748,18.5942171998995,37.2582207146837));
#54060=CARTESIAN_POINT('Ctrl Pts',(17.819634629107,18.5899856514211,37.1844510579588));
#54061=CARTESIAN_POINT('Ctrl Pts',(17.8514945721677,18.5857541029427,37.1119818704062));
#54062=CARTESIAN_POINT('Ctrl Pts',(17.8869527113608,18.5815225544643,37.0412169264318));
#54063=CARTESIAN_POINT('Ctrl Pts',(17.9223698954232,18.5772958935414,36.9705337179233));
#54064=CARTESIAN_POINT('Ctrl Pts',(17.9613768076314,18.5730692326184,36.9015512581737));
#54065=CARTESIAN_POINT('Ctrl Pts',(18.003781427272,18.5688425716955,36.8346534661225));
#54066=CARTESIAN_POINT('Ctrl Pts',(18.0461592797947,18.5646185787726,36.7677979020432));
#54067=CARTESIAN_POINT('Ctrl Pts',(18.0919303323664,18.5603945858498,36.7030247886281));
#54068=CARTESIAN_POINT('Ctrl Pts',(18.1408571981563,18.556170592927,36.6406924644706));
#54069=CARTESIAN_POINT('Ctrl Pts',(18.1897684135824,18.5519479511438,36.5783800787158));
#54070=CARTESIAN_POINT('Ctrl Pts',(18.2418331484101,18.5477253093606,36.5185073002988));
#54071=CARTESIAN_POINT('Ctrl Pts',(18.2967722374415,18.5435026675774,36.4614013213267));
#54072=CARTESIAN_POINT('Ctrl Pts',(18.3517108582994,18.5392800617782,36.4042958289937));
#54073=CARTESIAN_POINT('Ctrl Pts',(18.4095234586276,18.535057455979,36.3499574260545));
#54074=CARTESIAN_POINT('Ctrl Pts',(18.4698933782484,18.5308348501798,36.2986771064099));
#54075=CARTESIAN_POINT('Ctrl Pts',(18.5303233280054,18.5266080455411,36.2473457950696));
#54076=CARTESIAN_POINT('Ctrl Pts',(18.5933153184537,18.5223812409024,36.1990789453668));
#54077=CARTESIAN_POINT('Ctrl Pts',(18.6585193644235,18.5181544362638,36.1541274077491));
#54078=CARTESIAN_POINT('Ctrl Pts',(18.7237550071312,18.5139255833897,36.1091540874042));
#54079=CARTESIAN_POINT('Ctrl Pts',(18.7912044414011,18.5096967305156,36.0674995261933));
#54080=CARTESIAN_POINT('Ctrl Pts',(18.8604906106194,18.5054678776415,36.0293699527889));
#54081=CARTESIAN_POINT('Ctrl Pts',(18.9299013022672,18.501231424592,35.9911718521854));
#54082=CARTESIAN_POINT('Ctrl Pts',(19.0011549020658,18.4969949715426,35.9565116032249));
#54083=CARTESIAN_POINT('Ctrl Pts',(19.0738519992355,18.4927585184932,35.9255482710394));
#54084=CARTESIAN_POINT('Ctrl Pts',(19.1399243880608,18.4889081230301,35.8974065514503));
#54085=CARTESIAN_POINT('Ctrl Pts',(19.2071886823368,18.485057727567,35.8723181385503));
#54086=CARTESIAN_POINT('Ctrl Pts',(19.2753351555784,18.481207332104,35.8503664066877));
#54087=CARTESIAN_POINT('Ctrl Pts',(19.3503353434361,18.4769696897239,35.8262069170592));
#54088=CARTESIAN_POINT('Ctrl Pts',(19.4266858091362,18.4727320473439,35.8057568091963));
#54089=CARTESIAN_POINT('Ctrl Pts',(19.5039854804583,18.4684944049639,35.7891646451329));
#54090=CARTESIAN_POINT('Ctrl Pts',(19.5811739918204,18.4642628564798,35.7725963412523));
#54091=CARTESIAN_POINT('Ctrl Pts',(19.659308543504,18.4600313079958,35.7598750611734));
#54092=CARTESIAN_POINT('Ctrl Pts',(19.7379720864863,18.4557997595117,35.7510998715485));
#54093=CARTESIAN_POINT('Ctrl Pts',(19.8165447709051,18.451573098583,35.7423348175098));
#54094=CARTESIAN_POINT('Ctrl Pts',(19.8956447688872,18.4473464376543,35.7375068480514));
#54095=CARTESIAN_POINT('Ctrl Pts',(19.9748454995802,18.4431197767256,35.7366638639397));
#54096=CARTESIAN_POINT('Ctrl Pts',(20.0539962363043,18.4388957837969,35.7358214119457));
#54097=CARTESIAN_POINT('Ctrl Pts',(20.1332471120084,18.4346717908682,35.7389589573902));
#54098=CARTESIAN_POINT('Ctrl Pts',(20.2121683099733,18.4304477979396,35.7460724205824));
#54099=CARTESIAN_POINT('Ctrl Pts',(20.2910642632106,18.4262251561504,35.7531836083727));
#54100=CARTESIAN_POINT('Ctrl Pts',(20.3696302815773,18.4220025143613,35.7642681463416));
#54101=CARTESIAN_POINT('Ctrl Pts',(20.4474399346824,18.4177798725722,35.7792699541413));
#54102=CARTESIAN_POINT('Ctrl Pts',(20.5252489247195,18.413557266767,35.7942716341006));
#54103=CARTESIAN_POINT('Ctrl Pts',(20.6023011022857,18.4093346609618,35.8131904273686));
#54104=CARTESIAN_POINT('Ctrl Pts',(20.6781799926426,18.4051120551566,35.8359190963044));
#54105=CARTESIAN_POINT('Ctrl Pts',(20.7541343348171,18.4008852505119,35.8586703659843));
#54106=CARTESIAN_POINT('Ctrl Pts',(20.8289126092223,18.3966584458673,35.8852389439191));
#54107=CARTESIAN_POINT('Ctrl Pts',(20.9021138761845,18.3924316412226,35.9154677857044));
#54108=CARTESIAN_POINT('Ctrl Pts',(20.9753506151981,18.3882027883424,35.9457112758568));
#54109=CARTESIAN_POINT('Ctrl Pts',(21.0470084001397,18.3839739354622,35.9796183625193));
#54110=CARTESIAN_POINT('Ctrl Pts',(21.1167089871477,18.3797450825821,36.0169850027128));
#54111=CARTESIAN_POINT('Ctrl Pts',(21.1865348413843,18.3755086295266,36.054418798947));
#54112=CARTESIAN_POINT('Ctrl Pts',(21.2543960669251,18.3712721764711,36.0953243294549));
#54113=CARTESIAN_POINT('Ctrl Pts',(21.3199418157071,18.3670357234157,36.1394531262814));
#54114=CARTESIAN_POINT('Ctrl Pts',(21.3795145400991,18.3631853280054,36.1795605733691));
#54115=CARTESIAN_POINT('Ctrl Pts',(21.4371747410107,18.3593349325951,36.2223298945484));
#54116=CARTESIAN_POINT('Ctrl Pts',(21.4926838832828,18.3554845371848,36.2675466539396));
#54117=CARTESIAN_POINT('Ctrl Pts',(21.5537757630851,18.3512468948079,36.3173110119662));
#54118=CARTESIAN_POINT('Ctrl Pts',(21.6124909669647,18.3470092524311,36.3702272225976));
#54119=CARTESIAN_POINT('Ctrl Pts',(21.6684865531871,18.3427716100542,36.4260397069423));
#54120=CARTESIAN_POINT('Ctrl Pts',(21.7244016155589,18.3385400615734,36.4817719307441));
#54121=CARTESIAN_POINT('Ctrl Pts',(21.7776044977201,18.3343085130925,36.5403918288483));
#54122=CARTESIAN_POINT('Ctrl Pts',(21.827785081266,18.3300769646117,36.6016034778466));
#54123=CARTESIAN_POINT('Ctrl Pts',(21.8779077048521,18.3258503036862,36.6627444257));
#54124=CARTESIAN_POINT('Ctrl Pts',(21.9250146713074,18.3216236427608,36.7264708148327));
#54125=CARTESIAN_POINT('Ctrl Pts',(21.9688335951169,18.3173969818353,36.7924508744835));
#54126=CARTESIAN_POINT('Ctrl Pts',(22.0126248590562,18.3131729889099,36.8583892854646));
#54127=CARTESIAN_POINT('Ctrl Pts',(22.0531319413554,18.3089489959845,36.9265781538065));
#54128=CARTESIAN_POINT('Ctrl Pts',(22.0901242998228,18.3047250030591,36.9966546994752));
#54129=CARTESIAN_POINT('Ctrl Pts',(22.1271048254487,18.3005023612733,37.0667088295776));
#54130=CARTESIAN_POINT('Ctrl Pts',(22.1605726411276,18.2962797194875,37.1386490236881));
#54131=CARTESIAN_POINT('Ctrl Pts',(22.1903426696324,18.2920570777017,37.2120870366484));
#54132=CARTESIAN_POINT('Ctrl Pts',(22.2201124444467,18.2878344718998,37.2855244237939));
#54133=CARTESIAN_POINT('Ctrl Pts',(22.2461843199563,18.283611866098,37.360459169439));
#54134=CARTESIAN_POINT('Ctrl Pts',(22.2684215523446,18.2793892602961,37.4364835331671));
#54135=CARTESIAN_POINT('Ctrl Pts',(22.2906808968064,18.2751624556548,37.5125834933672));
#54136=CARTESIAN_POINT('Ctrl Pts',(22.3090978496328,18.2709356510134,37.5897747849498));
#54137=CARTESIAN_POINT('Ctrl Pts',(22.3235859045743,18.266708846372,37.6676355877691));
#54138=CARTESIAN_POINT('Ctrl Pts',(22.3380809801734,18.2624799934952,37.7455341205693));
#54139=CARTESIAN_POINT('Ctrl Pts',(22.3486433026082,18.2582511406184,37.8241023457273));
#54140=CARTESIAN_POINT('Ctrl Pts',(22.3552381453472,18.2540222877416,37.9029118988845));
#54141=CARTESIAN_POINT('Ctrl Pts',(22.3618448404639,18.2497858346894,37.9818630900791));
#54142=CARTESIAN_POINT('Ctrl Pts',(22.3644697930266,18.2455493816372,38.0610560062585));
#54143=CARTESIAN_POINT('Ctrl Pts',(22.3631304556828,18.2413129285851,38.1400610824187));
#54144=CARTESIAN_POINT('Ctrl Pts',(22.3619131688777,18.2374625331453,38.2118666190837));
#54145=CARTESIAN_POINT('Ctrl Pts',(22.3574218676397,18.2336121377055,38.2835167544354));
#54146=CARTESIAN_POINT('Ctrl Pts',(22.349706592117,18.2297617422657,38.3546946639842));
#54147=CARTESIAN_POINT('Ctrl Pts',(22.3412153659513,18.2255240998886,38.4330311700753));
#54148=CARTESIAN_POINT('Ctrl Pts',(22.3287864436435,18.2212864575114,38.5110896251283));
#54149=CARTESIAN_POINT('Ctrl Pts',(22.3124475466707,18.2170488151343,38.5884432257658));
#54150=CARTESIAN_POINT('Ctrl Pts',(22.296132145673,18.2128172666532,38.6656855888899));
#54151=CARTESIAN_POINT('Ctrl Pts',(22.2759180322438,18.208585718172,38.7422246556667));
#54152=CARTESIAN_POINT('Ctrl Pts',(22.2518846384725,18.2043541696909,38.8176391961925));
#54153=CARTESIAN_POINT('Ctrl Pts',(22.2278790039346,18.2001275087652,38.8929666308411));
#54154=CARTESIAN_POINT('Ctrl Pts',(22.200062997182,18.1959008478394,38.9671716760173));
#54155=CARTESIAN_POINT('Ctrl Pts',(22.1685666608388,18.1916741869137,39.0398452417278));
#54156=CARTESIAN_POINT('Ctrl Pts',(22.1370902059647,18.187450193988,39.1124729336189));
#54157=CARTESIAN_POINT('Ctrl Pts',(22.1019382185961,18.1832262010624,39.183570635881));
#54158=CARTESIAN_POINT('Ctrl Pts',(22.0632895308391,18.1790022081367,39.2527474800795));
#54159=CARTESIAN_POINT('Ctrl Pts',(22.0246532057381,18.1747795663506,39.3219021965016));
#54160=CARTESIAN_POINT('Ctrl Pts',(21.9825226298382,18.1705569245645,39.3891368660561));
#54161=CARTESIAN_POINT('Ctrl Pts',(21.9371227453085,18.1663342827784,39.4540848978215));
#54162=CARTESIAN_POINT('Ctrl Pts',(21.8917232476619,18.1621116769763,39.519032376121));
#54163=CARTESIAN_POINT('Ctrl Pts',(21.8430547665216,18.1578890711742,39.5816928719838));
#54164=CARTESIAN_POINT('Ctrl Pts',(21.7913849075893,18.1536664653721,39.6417297278581));
#54165=CARTESIAN_POINT('Ctrl Pts',(21.7396636696142,18.1494396607305,39.7018262826798));
#54166=CARTESIAN_POINT('Ctrl Pts',(21.6849353988243,18.1452128560889,39.7592936301455));
#54167=CARTESIAN_POINT('Ctrl Pts',(21.6275068580425,18.1409860514472,39.8138295912735));
#54168=CARTESIAN_POINT('Ctrl Pts',(21.5700504883961,18.1367571985702,39.8683919795727));
#54169=CARTESIAN_POINT('Ctrl Pts',(21.5098915982557,18.1325283456931,39.9200198460559));
#54170=CARTESIAN_POINT('Ctrl Pts',(21.4473706257125,18.128299492816,39.9684508858208));
#54171=CARTESIAN_POINT('Ctrl Pts',(21.3847372892809,18.1240630397636,40.0169689667773));
#54172=CARTESIAN_POINT('Ctrl Pts',(21.3197337736478,18.1198265867112,40.0622784724595));
#54173=CARTESIAN_POINT('Ctrl Pts',(21.2527299270681,18.1155901336588,40.1041602158331));
#54174=CARTESIAN_POINT('Ctrl Pts',(21.1918319773058,18.1117397382215,40.1422253782695));
#54175=CARTESIAN_POINT('Ctrl Pts',(21.1292822262864,18.1078893427841,40.1774594856631));
#54176=CARTESIAN_POINT('Ctrl Pts',(21.0653736864354,18.1040389473468,40.2097320562458));
#54177=CARTESIAN_POINT('Ctrl Pts',(20.9950376544135,18.0998013049689,40.2452503854585));
#54178=CARTESIAN_POINT('Ctrl Pts',(20.9227914424757,18.0955636625911,40.2773141559457));
#54179=CARTESIAN_POINT('Ctrl Pts',(20.8490081719268,18.0913260202132,40.3057142981133));
#54180=CARTESIAN_POINT('Ctrl Pts',(20.7753310046163,18.0870944717314,40.334073599762));
#54181=CARTESIAN_POINT('Ctrl Pts',(20.7001216021157,18.0828629232496,40.3587795687255));
#54182=CARTESIAN_POINT('Ctrl Pts',(20.6237765582469,18.0786313747678,40.3796695476059));
#54183=CARTESIAN_POINT('Ctrl Pts',(20.5475196950119,18.0744047138413,40.4005353979838));
#54184=CARTESIAN_POINT('Ctrl Pts',(20.4701302469447,18.0701780529149,40.4175938941423));
#54185=CARTESIAN_POINT('Ctrl Pts',(20.3920221732022,18.0659513919884,40.4307314424056));
#54186=CARTESIAN_POINT('Ctrl Pts',(20.3139634037098,18.061727399062,40.4438606978389));
#54187=CARTESIAN_POINT('Ctrl Pts',(20.2351873699961,18.0575034061356,40.4530738404765));
#54188=CARTESIAN_POINT('Ctrl Pts',(20.1561193035916,18.0532794132093,40.4583081231989));
#54189=CARTESIAN_POINT('Ctrl Pts',(20.0770765288943,18.0490567714224,40.4635407316178));
#54190=CARTESIAN_POINT('Ctrl Pts',(19.9977423744188,18.0448341296356,40.4647969765657));
#54191=CARTESIAN_POINT('Ctrl Pts',(19.9185468054221,18.0406114878488,40.4620660062736));
#54192=CARTESIAN_POINT('Ctrl Pts',(19.8393519113042,18.0363888820459,40.4593350592539));
#54193=CARTESIAN_POINT('Ctrl Pts',(19.760296068762,18.0321662762431,40.4526169821363));
#54194=CARTESIAN_POINT('Ctrl Pts',(19.6818073561958,18.0279436704402,40.4419530060035));
#54195=CARTESIAN_POINT('Ctrl Pts',(19.603240596679,18.0237168657979,40.4312784259152));
#54196=CARTESIAN_POINT('Ctrl Pts',(19.5252425591924,18.0194900611555,40.4166501724801));
#54197=CARTESIAN_POINT('Ctrl Pts',(19.4482337137936,18.0152632565132,40.3981610923314));
#54198=CARTESIAN_POINT('Ctrl Pts',(19.3711875512577,18.0110344036353,40.3796630526985));
#54199=CARTESIAN_POINT('Ctrl Pts',(19.2951319860325,18.0068055507575,40.3573005917263));
#54200=CARTESIAN_POINT('Ctrl Pts',(19.2204723697479,18.0025766978797,40.3312165100173));
#54201=CARTESIAN_POINT('Ctrl Pts',(19.145678573772,17.9983402448265,40.3050855494973));
#54202=CARTESIAN_POINT('Ctrl Pts',(19.0722861748444,17.9941037917734,40.2752197809421));
#54203=CARTESIAN_POINT('Ctrl Pts',(19.0006803634098,17.9898673387202,40.2418101467743));
#54204=CARTESIAN_POINT('Ctrl Pts',(18.9355998147263,17.9860169432894,40.2114450509896));
#54205=CARTESIAN_POINT('Ctrl Pts',(18.8719950122391,17.9821665478585,40.1781532688296));
#54206=CARTESIAN_POINT('Ctrl Pts',(18.8101349099469,17.9783161524276,40.1421095730575));
#54207=CARTESIAN_POINT('Ctrl Pts',(18.7420533334829,17.9740785100502,40.1024408441219));
#54208=CARTESIAN_POINT('Ctrl Pts',(18.6758298955651,17.9698408676728,40.0592892881113));
#54209=CARTESIAN_POINT('Ctrl Pts',(18.6118430810831,17.9656032252954,40.0128541003859));
#54210=CARTESIAN_POINT('Ctrl Pts',(18.5479482821514,17.9613716768141,39.9664856882828));
#54211=CARTESIAN_POINT('Ctrl Pts',(18.4862840955409,17.9571401283328,39.9168432949561));
#54212=CARTESIAN_POINT('Ctrl Pts',(18.4272028493791,17.9529085798514,39.8641710699075));
#54213=CARTESIAN_POINT('Ctrl Pts',(18.3681898436882,17.9486819189254,39.8115596827334));
#54214=CARTESIAN_POINT('Ctrl Pts',(18.3117541978809,17.9444552579994,39.7559257286738));
#54215=CARTESIAN_POINT('Ctrl Pts',(18.2582165346876,17.9402285970734,39.6975546315742));
#54216=CARTESIAN_POINT('Ctrl Pts',(18.2047126661356,17.9360046041475,39.63922038013));
#54217=CARTESIAN_POINT('Ctrl Pts',(18.1541034652771,17.9317806112216,39.578152759642));
#54218=CARTESIAN_POINT('Ctrl Pts',(18.1066730372676,17.9275566182957,39.5146743275717));
#54219=CARTESIAN_POINT('Ctrl Pts',(18.0592577809519,17.9233339765093,39.4512162005118));
#54220=CARTESIAN_POINT('Ctrl Pts',(18.0150195587025,17.919111334723,39.3853491684802));
#54221=CARTESIAN_POINT('Ctrl Pts',(17.9742015190833,17.9148886929366,39.3174280083913));
#54222=CARTESIAN_POINT('Ctrl Pts',(17.9333838273021,17.9106660871342,39.2495074271044));
#54223=CARTESIAN_POINT('Ctrl Pts',(17.895986500441,17.9064434813319,39.1795331550997));
#54224=CARTESIAN_POINT('Ctrl Pts',(17.8622079693646,17.9022208755295,39.1078867370154));
#54225=CARTESIAN_POINT('Ctrl Pts',(17.8283958498744,17.8979940708876,39.0361690757642));
#54226=CARTESIAN_POINT('Ctrl Pts',(17.7982099144151,17.8937672662457,38.9627763721112));
#54227=CARTESIAN_POINT('Ctrl Pts',(17.7718011537476,17.8895404616039,38.8881118844807));
#54228=CARTESIAN_POINT('Ctrl Pts',(17.7453795958575,17.8853116087265,38.8134112157477));
#54229=CARTESIAN_POINT('Ctrl Pts',(17.7227389930867,17.8810827558492,38.7374379851508));
#54230=CARTESIAN_POINT('Ctrl Pts',(17.703980201933,17.8768539029718,38.6606099604754));
#54231=CARTESIAN_POINT('Ctrl Pts',(17.6851876971208,17.8726174499192,38.5836438590035));
#54232=CARTESIAN_POINT('Ctrl Pts',(17.6702910319215,17.8683809968665,38.505820355379));
#54233=CARTESIAN_POINT('Ctrl Pts',(17.6593397037708,17.8641445438138,38.4275665101261));
#54234=CARTESIAN_POINT('Ctrl Pts',(17.6493863434018,17.8602941483787,38.3564437466272));
#54235=CARTESIAN_POINT('Ctrl Pts',(17.642691386469,17.8564437529437,38.284965839398));
#54236=CARTESIAN_POINT('Ctrl Pts',(17.6392546229838,17.8525933575086,38.2134535402565));
#54237=CARTESIAN_POINT('Ctrl Pts',(17.6374496869478,17.8505711882485,38.1758963658105));
#54238=CARTESIAN_POINT('Ctrl Pts',(17.6365409370372,17.8485490189884,38.138295778481));
#54239=CARTESIAN_POINT('Ctrl Pts',(17.6365300981241,17.8465268497283,38.1006810482146));
#54240=CARTESIAN_POINT('',(17.6365305274028,17.0527768497571,38.101578924073));
#54241=CARTESIAN_POINT('Ctrl Pts',(17.6365300981239,17.8465268496895,38.1006810474926));
#54242=CARTESIAN_POINT('Ctrl Pts',(17.6365075550966,17.8423210898796,38.0224489608224));
#54243=CARTESIAN_POINT('Ctrl Pts',(17.6403735597462,17.8381153300697,37.9440613389769));
#54244=CARTESIAN_POINT('Ctrl Pts',(17.6481482955731,17.8339095702598,37.8659401758429));
#54245=CARTESIAN_POINT('Ctrl Pts',(17.6559120990009,17.8297097243544,37.7879288623243));
#54246=CARTESIAN_POINT('Ctrl Pts',(17.6675736759225,17.8255098784489,37.7101837339056));
#54247=CARTESIAN_POINT('Ctrl Pts',(17.6831011931123,17.8213100325435,37.6331270413244));
#54248=CARTESIAN_POINT('Ctrl Pts',(17.6986118056779,17.8171147589607,37.556154239453));
#54249=CARTESIAN_POINT('Ctrl Pts',(17.7179799045057,17.8129194853778,37.4798688494731));
#54250=CARTESIAN_POINT('Ctrl Pts',(17.7411220056558,17.808724211795,37.4046866551204));
#54251=CARTESIAN_POINT('Ctrl Pts',(17.7642507353119,17.804531362239,37.3295479010006));
#54252=CARTESIAN_POINT('Ctrl Pts',(17.7911490007325,17.800338512683,37.2555115321422));
#54253=CARTESIAN_POINT('Ctrl Pts',(17.8216828405759,17.7961456631271,37.182980483382));
#54254=CARTESIAN_POINT('Ctrl Pts',(17.8522089048497,17.7919538812977,37.1104679049554));
#54255=CARTESIAN_POINT('Ctrl Pts',(17.8863685204665,17.7877620994684,37.0394603244555));
#54256=CARTESIAN_POINT('Ctrl Pts',(17.9239793027399,17.7835703176391,36.9703414208498));
#54257=CARTESIAN_POINT('Ctrl Pts',(17.9615926609566,17.7793782487167,36.9012177833255));
#54258=CARTESIAN_POINT('Ctrl Pts',(18.0026574252911,17.7751861797943,36.8339834969267));
#54259=CARTESIAN_POINT('Ctrl Pts',(18.0469456729691,17.770994110872,36.7689969058767));
#54260=CARTESIAN_POINT('Ctrl Pts',(18.0912795208766,17.7667977256961,36.7039434030922));
#54261=CARTESIAN_POINT('Ctrl Pts',(18.1388432071584,17.7626013405202,36.6411426088292));
#54262=CARTESIAN_POINT('Ctrl Pts',(18.1893664066169,17.7584049553443,36.5809225064492));
#54263=CARTESIAN_POINT('Ctrl Pts',(18.2399186658585,17.7542061565042,36.5206677668504));
#54264=CARTESIAN_POINT('Ctrl Pts',(18.2934335010051,17.750007357664,36.4629970215123));
#54265=CARTESIAN_POINT('Ctrl Pts',(18.349603130203,17.7458085588238,36.408201958547));
#54266=CARTESIAN_POINT('Ctrl Pts',(18.405866185116,17.7416027762134,36.3533157561526));
#54267=CARTESIAN_POINT('Ctrl Pts',(18.4647924894867,17.737396993603,36.3013150964894));
#54268=CARTESIAN_POINT('Ctrl Pts',(18.5260410722742,17.7331912109926,36.2524514836472));
#54269=CARTESIAN_POINT('Ctrl Pts',(18.556723491604,17.7310843281915,36.2279733032394));
#54270=CARTESIAN_POINT('Ctrl Pts',(18.5879882269045,17.7289774453905,36.2042816852787));
#54271=CARTESIAN_POINT('Ctrl Pts',(18.6197899146442,17.7268705625894,36.1814040130392));
#54272=CARTESIAN_POINT('Ctrl Pts',(18.6837536906915,17.7226329202119,36.1353894016265));
#54273=CARTESIAN_POINT('Ctrl Pts',(18.7501411602903,17.7183952778343,36.0924906324536));
#54274=CARTESIAN_POINT('Ctrl Pts',(18.8186162142466,17.7141576354568,36.0529722054503));
#54275=CARTESIAN_POINT('Ctrl Pts',(18.8869927983881,17.7099260869753,36.013510607496));
#54276=CARTESIAN_POINT('Ctrl Pts',(18.9574506024816,17.7056945384938,35.9774199304681));
#54277=CARTESIAN_POINT('Ctrl Pts',(19.0296231191284,17.7014629900123,35.9449224723992));
#54278=CARTESIAN_POINT('Ctrl Pts',(19.1017122745253,17.6972363290861,35.9124625497919));
#54279=CARTESIAN_POINT('Ctrl Pts',(19.1755117813665,17.6930096681599,35.8835877900102));
#54280=CARTESIAN_POINT('Ctrl Pts',(19.2506303551274,17.6887830072338,35.858474721034));
#54281=CARTESIAN_POINT('Ctrl Pts',(19.3257015117036,17.6845590143077,35.8333775042096));
#54282=CARTESIAN_POINT('Ctrl Pts',(19.4020896390851,17.6803350213816,35.8120374133194));
#54283=CARTESIAN_POINT('Ctrl Pts',(19.4793844176147,17.6761110284556,35.794582498488));
#54284=CARTESIAN_POINT('Ctrl Pts',(19.5566544716635,17.6718883866691,35.7771331670055));
#54285=CARTESIAN_POINT('Ctrl Pts',(19.6348301440226,17.6676657448825,35.7635666468885));
#54286=CARTESIAN_POINT('Ctrl Pts',(19.7134883762113,17.663443103096,35.7539604584888));
#54287=CARTESIAN_POINT('Ctrl Pts',(19.7921459381002,17.6592204972935,35.74435435195));
#54288=CARTESIAN_POINT('Ctrl Pts',(19.8712855861536,17.6549978914909,35.738708565434));
#54289=CARTESIAN_POINT('Ctrl Pts',(19.9504780341298,17.6507752856884,35.7370488757073));
#54290=CARTESIAN_POINT('Ctrl Pts',(20.029749228831,17.6465484810464,35.7353875356321));
#54291=CARTESIAN_POINT('Ctrl Pts',(20.1090728585694,17.6423216764043,35.7377202196232));
#54292=CARTESIAN_POINT('Ctrl Pts',(20.1880191339567,17.6380948717623,35.7440205335856));
#54293=CARTESIAN_POINT('Ctrl Pts',(20.2670036653259,17.6338660188848,35.7503239005698));
#54294=CARTESIAN_POINT('Ctrl Pts',(20.3456100126528,17.6296371660073,35.7605986668219));
#54295=CARTESIAN_POINT('Ctrl Pts',(20.4234155604438,17.6254083131298,35.7747667420076));
#54296=CARTESIAN_POINT('Ctrl Pts',(20.5013609418544,17.6211718600769,35.7889602803292));
#54297=CARTESIAN_POINT('Ctrl Pts',(20.5785021905825,17.6169354070241,35.8070610011872));
#54298=CARTESIAN_POINT('Ctrl Pts',(20.6544291280943,17.6126989539713,35.8289401246991));
#54299=CARTESIAN_POINT('Ctrl Pts',(20.7234370292418,17.6088485585376,35.848825457125));
#54300=CARTESIAN_POINT('Ctrl Pts',(20.7914417997745,17.604998163104,35.8718312140375));
#54301=CARTESIAN_POINT('Ctrl Pts',(20.8581505983656,17.6011477676704,35.8978265301242));
#54302=CARTESIAN_POINT('Ctrl Pts',(20.9315685204291,17.5969101252929,35.9264362807235));
#54303=CARTESIAN_POINT('Ctrl Pts',(21.0036919659445,17.5926724829154,35.9587752529252));
#54304=CARTESIAN_POINT('Ctrl Pts',(21.0741160983171,17.5884348405379,35.9947054723303));
#54305=CARTESIAN_POINT('Ctrl Pts',(21.1444389580236,17.5842032920565,36.0305840226698));
#54306=CARTESIAN_POINT('Ctrl Pts',(21.2130669433908,17.579971743575,36.0700433530018));
#54307=CARTESIAN_POINT('Ctrl Pts',(21.279614072805,17.5757401950936,36.1128970168661));
#54308=CARTESIAN_POINT('Ctrl Pts',(21.346084338447,17.5715135341675,36.1557011835654));
#54309=CARTESIAN_POINT('Ctrl Pts',(21.4104781322585,17.5672868732414,36.2018916401645));
#54310=CARTESIAN_POINT('Ctrl Pts',(21.4724343805696,17.5630602123153,36.2512362412096));
#54311=CARTESIAN_POINT('Ctrl Pts',(21.534351520166,17.5588362193893,36.3005496944049));
#54312=CARTESIAN_POINT('Ctrl Pts',(21.5938338025949,17.5546122264633,36.3530130488623));
#54313=CARTESIAN_POINT('Ctrl Pts',(21.6505504591888,17.5503882335373,36.4083518029532));
#54314=CARTESIAN_POINT('Ctrl Pts',(21.707248973679,17.5461655917509,36.4636728556936));
#54315=CARTESIAN_POINT('Ctrl Pts',(21.7611832837885,17.5419429499644,36.5218671544669));
#54316=CARTESIAN_POINT('Ctrl Pts',(21.8120580744441,17.537720308178,36.5826220063076));
#54317=CARTESIAN_POINT('Ctrl Pts',(21.8629324315612,17.5334977023755,36.6433763404151));
#54318=CARTESIAN_POINT('Ctrl Pts',(21.9107470212018,17.529275096573,36.706690823882));
#54319=CARTESIAN_POINT('Ctrl Pts',(21.955246544318,17.5250524907706,36.772219373604));
#54320=CARTESIAN_POINT('Ctrl Pts',(21.9997903164985,17.5208256861286,36.8378130830583));
#54321=CARTESIAN_POINT('Ctrl Pts',(22.0410121735985,17.5165988814866,36.9056248677755));
#54322=CARTESIAN_POINT('Ctrl Pts',(22.078700307134,17.5123720768447,36.9752798241247));
#54323=CARTESIAN_POINT('Ctrl Pts',(22.1164067036787,17.5081432239672,37.0449685340452));
#54324=CARTESIAN_POINT('Ctrl Pts',(22.1505757630878,17.5039143710898,37.1165017713586));
#54325=CARTESIAN_POINT('Ctrl Pts',(22.1810429481826,17.4996855182123,37.1894825102816));
#54326=CARTESIAN_POINT('Ctrl Pts',(22.2115648894856,17.4954490651596,37.2625944115855));
#54327=CARTESIAN_POINT('Ctrl Pts',(22.2383715040085,17.4912126121068,37.3371585703252));
#54328=CARTESIAN_POINT('Ctrl Pts',(22.2613475462707,17.486976159054,37.4127608015579));
#54329=CARTESIAN_POINT('Ctrl Pts',(22.2822298379241,17.4831257636198,37.4814735861281));
#54330=CARTESIAN_POINT('Ctrl Pts',(22.2999484669787,17.4792753681856,37.5510434348584));
#54331=CARTESIAN_POINT('Ctrl Pts',(22.3144538081643,17.4754249727513,37.621153458012));
#54332=CARTESIAN_POINT('Ctrl Pts',(22.3304179992604,17.4711873303739,37.6983146769765));
#54333=CARTESIAN_POINT('Ctrl Pts',(22.3425492376475,17.4669496879964,37.7764199493418));
#54334=CARTESIAN_POINT('Ctrl Pts',(22.3507428986342,17.4627120456189,37.8550545664423));
#54335=CARTESIAN_POINT('Ctrl Pts',(22.3589247768149,17.4584804971375,37.9335761038776));
#54336=CARTESIAN_POINT('Ctrl Pts',(22.3631802743976,17.454248948656,38.0126250119418));
#54337=CARTESIAN_POINT('Ctrl Pts',(22.3634556917679,17.4500174001746,38.0917760137368));
#54338=CARTESIAN_POINT('Ctrl Pts',(22.3637307910235,17.4457907392485,38.1708355939388));
#54339=CARTESIAN_POINT('Ctrl Pts',(22.3600349440432,17.4415640783224,38.2499965671349));
#54340=CARTESIAN_POINT('Ctrl Pts',(22.3523663448958,17.4373374173963,38.3288296753077));
#54341=CARTESIAN_POINT('Ctrl Pts',(22.3447025864073,17.4331134244703,38.407613021566));
#54342=CARTESIAN_POINT('Ctrl Pts',(22.3330710985764,17.4288894315443,38.4860684482406));
#54343=CARTESIAN_POINT('Ctrl Pts',(22.3175221027841,17.4246654386183,38.5637690632276));
#54344=CARTESIAN_POINT('Ctrl Pts',(22.3019780806894,17.4204427968318,38.6414448239178));
#54345=CARTESIAN_POINT('Ctrl Pts',(22.2825191309671,17.4162201550454,38.718365793051));
#54346=CARTESIAN_POINT('Ctrl Pts',(22.2592468111238,17.4119975132589,38.7941140304928));
#54347=CARTESIAN_POINT('Ctrl Pts',(22.2359746895996,17.4077749074565,38.8698616224328));
#54348=CARTESIAN_POINT('Ctrl Pts',(22.2088894016045,17.403552301654,38.9444360548706));
#54349=CARTESIAN_POINT('Ctrl Pts',(22.1781422966946,17.3993296958515,39.0174347803794));
#54350=CARTESIAN_POINT('Ctrl Pts',(22.1473646177353,17.3951028912096,39.0905060937514));
#54351=CARTESIAN_POINT('Ctrl Pts',(22.112918030922,17.3908760865676,39.1619981374081));
#54352=CARTESIAN_POINT('Ctrl Pts',(22.0750017358759,17.3866492819256,39.2315291587105));
#54353=CARTESIAN_POINT('Ctrl Pts',(22.0370670672575,17.3824204290482,39.3010938735276));
#54354=CARTESIAN_POINT('Ctrl Pts',(21.9956595861073,17.3781915761707,39.3686952726717));
#54355=CARTESIAN_POINT('Ctrl Pts',(21.9510227810537,17.3739627232933,39.433979215996));
#54356=CARTESIAN_POINT('Ctrl Pts',(21.9063057538799,17.3697262702405,39.4993804888727));
#54357=CARTESIAN_POINT('Ctrl Pts',(21.8583480906393,17.3654898171878,39.5624556098572));
#54358=CARTESIAN_POINT('Ctrl Pts',(21.8074345054459,17.361253364135,39.6228824476707));
#54359=CARTESIAN_POINT('Ctrl Pts',(21.7611605509071,17.3574029687007,39.677802735356));
#54360=CARTESIAN_POINT('Ctrl Pts',(21.7124455390639,17.3535525732665,39.7305356595026));
#54361=CARTESIAN_POINT('Ctrl Pts',(21.6615282856477,17.3497021778322,39.7808670967369));
#54362=CARTESIAN_POINT('Ctrl Pts',(21.6054901164498,17.3454645354547,39.836260532291));
#54363=CARTESIAN_POINT('Ctrl Pts',(21.5465735991057,17.3412268930772,39.8889525098605));
#54364=CARTESIAN_POINT('Ctrl Pts',(21.4850696683363,17.3369892506997,39.9386295225214));
#54365=CARTESIAN_POINT('Ctrl Pts',(21.4236541826332,17.3327577022183,39.9882350976885));
#54366=CARTESIAN_POINT('Ctrl Pts',(21.359659034336,17.3285261537368,40.0348340260054));
#54367=CARTESIAN_POINT('Ctrl Pts',(21.2934117438425,17.3242946052554,40.0781497672801));
#54368=CARTESIAN_POINT('Ctrl Pts',(21.2272409707988,17.3200679443292,40.1214154776775));
#54369=CARTESIAN_POINT('Ctrl Pts',(21.158823615332,17.3158412834031,40.1614052817935));
#54370=CARTESIAN_POINT('Ctrl Pts',(21.0885187850471,17.311614622477,40.1978840043004));
#54371=CARTESIAN_POINT('Ctrl Pts',(21.0182583333618,17.307390629551,40.234339700301));
#54372=CARTESIAN_POINT('Ctrl Pts',(20.9461131867294,17.303166636625,40.2672884984783));
#54373=CARTESIAN_POINT('Ctrl Pts',(20.8724687883813,17.2989426436989,40.2965401553808));
#54374=CARTESIAN_POINT('Ctrl Pts',(20.7988479468578,17.2947200019125,40.3257824554801));
#54375=CARTESIAN_POINT('Ctrl Pts',(20.7237292412991,17.290497360126,40.3513297898209));
#54376=CARTESIAN_POINT('Ctrl Pts',(20.6475185494969,17.2862747183395,40.373039852039));
#54377=CARTESIAN_POINT('Ctrl Pts',(20.5713085071374,17.2820521125371,40.394749729251));
#54378=CARTESIAN_POINT('Ctrl Pts',(20.4940069482651,17.2778295067346,40.4126222723031));
#54379=CARTESIAN_POINT('Ctrl Pts',(20.4160339418098,17.2736069009321,40.4265653225651));
#54380=CARTESIAN_POINT('Ctrl Pts',(20.3379834012073,17.2693800962901,40.440522237401));
#54381=CARTESIAN_POINT('Ctrl Pts',(20.2592605418775,17.2651532916481,40.4505417717367));
#54382=CARTESIAN_POINT('Ctrl Pts',(20.1802940351675,17.2609264870061,40.4565832261524));
#54383=CARTESIAN_POINT('Ctrl Pts',(20.1012892626721,17.2566976341287,40.4626276081512));
#54384=CARTESIAN_POINT('Ctrl Pts',(20.022041076807,17.2524687812512,40.4646900577993));
#54385=CARTESIAN_POINT('Ctrl Pts',(19.9429790937746,17.2482399283738,40.4627820587505));
#54386=CARTESIAN_POINT('Ctrl Pts',(19.863775019033,17.244003475321,40.4608706306093));
#54387=CARTESIAN_POINT('Ctrl Pts',(19.7847582843649,17.2397670222682,40.4549745307829));
#54388=CARTESIAN_POINT('Ctrl Pts',(19.7063540952675,17.2355305692154,40.4451572492125));
#54389=CARTESIAN_POINT('Ctrl Pts',(19.6350946884117,17.2316801737813,40.4362345925318));
#54390=CARTESIAN_POINT('Ctrl Pts',(19.564341435708,17.2278297783472,40.424073552306));
#54391=CARTESIAN_POINT('Ctrl Pts',(19.4944039542023,17.2239793829131,40.4087579083511));
#54392=CARTESIAN_POINT('Ctrl Pts',(19.4174326299637,17.2197417405356,40.3919019196681));
#54393=CARTESIAN_POINT('Ctrl Pts',(19.3411606841025,17.2155040981581,40.3711608784529));
#54394=CARTESIAN_POINT('Ctrl Pts',(19.2660094735217,17.2112664557806,40.3466081874551));
#54395=CARTESIAN_POINT('Ctrl Pts',(19.1909663333313,17.2070349072992,40.3220908041906));
#54396=CARTESIAN_POINT('Ctrl Pts',(19.1170411697246,17.2028033588177,40.2937728008795));
#54397=CARTESIAN_POINT('Ctrl Pts',(19.0446442442947,17.1985718103363,40.2617783931154));
#54398=CARTESIAN_POINT('Ctrl Pts',(18.9723309393126,17.1943451494102,40.2298209397757));
#54399=CARTESIAN_POINT('Ctrl Pts',(18.9015427912952,17.1901184884841,40.1941957090735));
#54400=CARTESIAN_POINT('Ctrl Pts',(18.8326725562312,17.1858918275579,40.1550759304523));
#54401=CARTESIAN_POINT('Ctrl Pts',(18.7638457942058,17.1816678346319,40.1159808454544));
#54402=CARTESIAN_POINT('Ctrl Pts',(18.6969349486741,17.1774438417059,40.0733958218646));
#54403=CARTESIAN_POINT('Ctrl Pts',(18.6323094191472,17.1732198487799,40.0275406392464));
#54404=CARTESIAN_POINT('Ctrl Pts',(18.5677045615556,17.1689972069934,39.9817001244441));
#54405=CARTESIAN_POINT('Ctrl Pts',(18.5053839503625,17.1647745652069,39.9325917989046));
#54406=CARTESIAN_POINT('Ctrl Pts',(18.4456878954677,17.1605519234204,39.8804786779415));
#54407=CARTESIAN_POINT('Ctrl Pts',(18.3859923492835,17.156329317618,39.8283660010697));
#54408=CARTESIAN_POINT('Ctrl Pts',(18.3289216671295,17.1521067118155,39.773248889047));
#54409=CARTESIAN_POINT('Ctrl Pts',(18.2747818163375,17.147884106013,39.7154295588667));
#54410=CARTESIAN_POINT('Ctrl Pts',(18.2205881304126,17.143657301371,39.6575527347835));
#54411=CARTESIAN_POINT('Ctrl Pts',(18.1693314183993,17.139430496729,39.596968668207));
#54412=CARTESIAN_POINT('Ctrl Pts',(18.1212791627667,17.135203692087,39.5340148034959));
#54413=CARTESIAN_POINT('Ctrl Pts',(18.0732036218531,17.1309748392096,39.4710304324451));
#54414=CARTESIAN_POINT('Ctrl Pts',(18.0283358963797,17.1267459863321,39.4056743625485));
#54415=CARTESIAN_POINT('Ctrl Pts',(17.9869002084452,17.1225171334547,39.3383132358745));
#54416=CARTESIAN_POINT('Ctrl Pts',(17.9453900514993,17.1182806804019,39.2708310464943));
#54417=CARTESIAN_POINT('Ctrl Pts',(17.9073244823368,17.1140442273491,39.2013370122531));
#54418=CARTESIAN_POINT('Ctrl Pts',(17.8728816957638,17.1098077742963,39.1302223840917));
#54419=CARTESIAN_POINT('Ctrl Pts',(17.841577596201,17.1059573788622,39.0655882582893));
#54420=CARTESIAN_POINT('Ctrl Pts',(17.8132655893203,17.1021069834281,38.9996159615739));
#54421=CARTESIAN_POINT('Ctrl Pts',(17.7880439305086,17.0982565879941,38.9326108259805));
#54422=CARTESIAN_POINT('Ctrl Pts',(17.7563093557472,17.0934119160922,38.8483031481727));
#54423=CARTESIAN_POINT('Ctrl Pts',(17.7293681785243,17.0885672441903,38.7620982479688));
#54424=CARTESIAN_POINT('Ctrl Pts',(17.7074200611923,17.0837225722885,38.6745151565246));
#54425=CARTESIAN_POINT('Ctrl Pts',(17.6855647710021,17.0788983903921,38.5873024881068));
#54426=CARTESIAN_POINT('Ctrl Pts',(17.6686605201809,17.0740742084958,38.4987234425967));
#54427=CARTESIAN_POINT('Ctrl Pts',(17.6568575551637,17.0692500265994,38.4093120173972));
#54428=CARTESIAN_POINT('Ctrl Pts',(17.6451385851259,17.064460175658,38.3205368823854));
#54429=CARTESIAN_POINT('Ctrl Pts',(17.6384486638185,17.0596703247165,38.2309413704542));
#54430=CARTESIAN_POINT('Ctrl Pts',(17.6368868042697,17.054880473775,38.1410665930586));
#54431=CARTESIAN_POINT('Ctrl Pts',(17.6366581565658,17.054179265769,38.1279094167254));
#54432=CARTESIAN_POINT('Ctrl Pts',(17.6365393239043,17.0534780577631,38.1147462846933));
#54433=CARTESIAN_POINT('Ctrl Pts',(17.6365305274028,17.0527768497571,38.101578924073));
#54434=CARTESIAN_POINT('',(17.6365307316195,16.259026849677,38.0981403439098));
#54435=CARTESIAN_POINT('Ctrl Pts',(17.6365305274025,17.0527768497283,38.101578923533));
#54436=CARTESIAN_POINT('Ctrl Pts',(17.6364773100099,17.0485346547335,38.0219185219947));
#54437=CARTESIAN_POINT('Ctrl Pts',(17.6404558360725,17.0442924597387,37.9422319286419));
#54438=CARTESIAN_POINT('Ctrl Pts',(17.6484474808675,17.0400502647438,37.8629531888815));
#54439=CARTESIAN_POINT('Ctrl Pts',(17.6564393552686,17.0358079478675,37.7836721713815));
#54440=CARTESIAN_POINT('Ctrl Pts',(17.6684445303095,17.0315656309911,37.7047994907601));
#54441=CARTESIAN_POINT('Ctrl Pts',(17.6843925358181,17.0273233141148,37.6267637876016));
#54442=CARTESIAN_POINT('Ctrl Pts',(17.7003457880481,17.023079601562,37.5487024115406));
#54443=CARTESIAN_POINT('Ctrl Pts',(17.7202443536963,17.0188358890093,37.4714790125329));
#54444=CARTESIAN_POINT('Ctrl Pts',(17.743967017387,17.0145921764565,37.3955103817214));
#54445=CARTESIAN_POINT('Ctrl Pts',(17.767720457143,17.0103429584185,37.3194431947116));
#54446=CARTESIAN_POINT('Ctrl Pts',(17.7953077558804,17.0060937403806,37.2446344658512));
#54447=CARTESIAN_POINT('Ctrl Pts',(17.8265585157788,17.0018445223426,37.1714836805062));
#54448=CARTESIAN_POINT('Ctrl Pts',(17.8578331082664,16.9975920637476,37.0982771085941));
#54449=CARTESIAN_POINT('Ctrl Pts',(17.892776519481,16.9933396051527,37.0267314113367));
#54450=CARTESIAN_POINT('Ctrl Pts',(17.9311722225806,16.9890871465577,36.9572217764247));
#54451=CARTESIAN_POINT('Ctrl Pts',(17.9696348049536,16.984827280849,36.8875910666658));
#54452=CARTESIAN_POINT('Ctrl Pts',(18.0115614352225,16.9805674151403,36.8200038878202));
#54453=CARTESIAN_POINT('Ctrl Pts',(18.0566924234116,16.9763075494316,36.7548062951107));
#54454=CARTESIAN_POINT('Ctrl Pts',(18.0700193970146,16.975049630646,36.7355537453243));
#54455=CARTESIAN_POINT('Ctrl Pts',(18.083625526166,16.9737917118605,36.7165093401657));
#54456=CARTESIAN_POINT('Ctrl Pts',(18.0975034837418,16.972533793075,36.6976814033446));
#54457=CARTESIAN_POINT('Ctrl Pts',(18.144255167406,16.9682961506975,36.6342543650721));
#54458=CARTESIAN_POINT('Ctrl Pts',(18.1942699535504,16.96405850832,36.5730487960201));
#54459=CARTESIAN_POINT('Ctrl Pts',(18.2473091472338,16.9598208659426,36.5144195966368));
#54460=CARTESIAN_POINT('Ctrl Pts',(18.3002720684751,16.9555893174611,36.4558747083431));
#54461=CARTESIAN_POINT('Ctrl Pts',(18.3562504482264,16.9513577689797,36.3998991768475));
#54462=CARTESIAN_POINT('Ctrl Pts',(18.4149637068756,16.9471262204983,36.3468170687636));
#54463=CARTESIAN_POINT('Ctrl Pts',(18.4736091500898,16.9428995595722,36.2937962719804));
#54464=CARTESIAN_POINT('Ctrl Pts',(18.534982848783,16.9386728986461,36.2436625700329));
#54465=CARTESIAN_POINT('Ctrl Pts',(18.5987665931446,16.93444623772,36.1967040743982));
#54466=CARTESIAN_POINT('Ctrl Pts',(18.6625100752192,16.930222244794,36.1497752204293));
#54467=CARTESIAN_POINT('Ctrl Pts',(18.7286602068436,16.925998251868,36.1060178716758));
#54468=CARTESIAN_POINT('Ctrl Pts',(18.7968657816441,16.921774258942,36.0656798448816));
#54469=CARTESIAN_POINT('Ctrl Pts',(18.8650495393507,16.9175516171556,36.0253547211165));
#54470=CARTESIAN_POINT('Ctrl Pts',(18.9352870314098,16.9133289753691,35.9884469858035));
#54471=CARTESIAN_POINT('Ctrl Pts',(19.0071994174011,16.9091063335827,35.9551602754305));
#54472=CARTESIAN_POINT('Ctrl Pts',(19.0791111905786,16.9048837277802,35.921873848716));
#54473=CARTESIAN_POINT('Ctrl Pts',(19.1526974032996,16.9006611219777,35.8922085812036));
#54474=CARTESIAN_POINT('Ctrl Pts',(19.2275574052582,16.8964385161752,35.8663207753286));
#54475=CARTESIAN_POINT('Ctrl Pts',(19.3024918458803,16.8922117115333,35.8404072273534));
#54476=CARTESIAN_POINT('Ctrl Pts',(19.3787021617585,16.8879849068913,35.818278797607));
#54477=CARTESIAN_POINT('Ctrl Pts',(19.4557712098074,16.8837581022493,35.8000422906441));
#54478=CARTESIAN_POINT('Ctrl Pts',(19.5328776041666,16.8795292493719,35.7817969465895));
#54479=CARTESIAN_POINT('Ctrl Pts',(19.6108430980497,16.8753003964945,35.7674473673279));
#54480=CARTESIAN_POINT('Ctrl Pts',(19.6892415077115,16.871071543617,35.7570489547644));
#54481=CARTESIAN_POINT('Ctrl Pts',(19.7677808164956,16.8668350905643,35.7466318539749));
#54482=CARTESIAN_POINT('Ctrl Pts',(19.8467541273414,16.8625986375115,35.7401801468548));
#54483=CARTESIAN_POINT('Ctrl Pts',(19.9257315338408,16.8583621844587,35.7376971752474));
#54484=CARTESIAN_POINT('Ctrl Pts',(19.9975119222006,16.8545117890245,35.7354404707775));
#54485=CARTESIAN_POINT('Ctrl Pts',(20.0692954247503,16.8506613935902,35.7364614652437));
#54486=CARTESIAN_POINT('Ctrl Pts',(20.1407631677291,16.846810998156,35.7407254989063));
#54487=CARTESIAN_POINT('Ctrl Pts',(20.2194186568709,16.8425733557785,35.7454183804704));
#54488=CARTESIAN_POINT('Ctrl Pts',(20.2979868501066,16.838335713401,35.7540577975682));
#54489=CARTESIAN_POINT('Ctrl Pts',(20.3760401028157,16.8340980710235,35.7666367016741));
#54490=CARTESIAN_POINT('Ctrl Pts',(20.4539811118842,16.829866522542,35.7791975168222));
#54491=CARTESIAN_POINT('Ctrl Pts',(20.5314081920214,16.8256349740606,35.7956864945732));
#54492=CARTESIAN_POINT('Ctrl Pts',(20.607896764797,16.8214034255791,35.816044666757));
#54493=CARTESIAN_POINT('Ctrl Pts',(20.6842969911588,16.817176764653,35.8363793246897));
#54494=CARTESIAN_POINT('Ctrl Pts',(20.7597604136338,16.8129501037269,35.8605741760148));
#54495=CARTESIAN_POINT('Ctrl Pts',(20.8338721319363,16.8087234428008,35.88851911415));
#54496=CARTESIAN_POINT('Ctrl Pts',(20.9079370686125,16.8044994498748,35.9164464125694));
#54497=CARTESIAN_POINT('Ctrl Pts',(20.9806515572187,16.8002754569488,35.9481189342661));
#54498=CARTESIAN_POINT('Ctrl Pts',(21.0516165382129,16.7960514640227,35.9833769590555));
#54499=CARTESIAN_POINT('Ctrl Pts',(21.1225588194548,16.7918288222363,36.0186237057692));
#54500=CARTESIAN_POINT('Ctrl Pts',(21.1917522848677,16.7876061804498,36.057453469622));
#54501=CARTESIAN_POINT('Ctrl Pts',(21.258819894101,16.7833835386634,36.0996593002402));
#54502=CARTESIAN_POINT('Ctrl Pts',(21.325886931806,16.7791609328609,36.141864771194));
#54503=CARTESIAN_POINT('Ctrl Pts',(21.3908277533633,16.7749383270584,36.1874460008249));
#54504=CARTESIAN_POINT('Ctrl Pts',(21.4532931535293,16.7707157212559,36.2361519775462));
#54505=CARTESIAN_POINT('Ctrl Pts',(21.5158206675183,16.766488916614,36.28490638611));
#54506=CARTESIAN_POINT('Ctrl Pts',(21.5758674727437,16.762262111972,36.3367914594122));
#54507=CARTESIAN_POINT('Ctrl Pts',(21.6331169085232,16.75803530733,36.391515407153));
#54508=CARTESIAN_POINT('Ctrl Pts',(21.6903940863761,16.7538064544525,36.44626587316));
#54509=CARTESIAN_POINT('Ctrl Pts',(21.7448708718096,16.7495776015751,36.5038576131085));
#54510=CARTESIAN_POINT('Ctrl Pts',(21.7962688030057,16.7453487486977,36.5639632724936));
#54511=CARTESIAN_POINT('Ctrl Pts',(21.8477591075475,16.7411122956449,36.6241769549203));
#54512=CARTESIAN_POINT('Ctrl Pts',(21.8961592146095,16.7368758425921,36.6869132122772));
#54513=CARTESIAN_POINT('Ctrl Pts',(21.9412323074948,16.7326393895393,36.7518132290968));
#54514=CARTESIAN_POINT('Ctrl Pts',(21.9821979995223,16.7287889941052,36.8107990659103));
#54515=CARTESIAN_POINT('Ctrl Pts',(22.0204158313138,16.724938598671,36.8715716831065));
#54516=CARTESIAN_POINT('Ctrl Pts',(22.0557413034838,16.7210882032368,36.9338447212953));
#54517=CARTESIAN_POINT('Ctrl Pts',(22.0946195746725,16.7168505608593,37.002380763922));
#54518=CARTESIAN_POINT('Ctrl Pts',(22.1301397068541,16.7126129184818,37.0729918163567));
#54519=CARTESIAN_POINT('Ctrl Pts',(22.162074830647,16.7083752761043,37.1453153046253));
#54520=CARTESIAN_POINT('Ctrl Pts',(22.1939640304786,16.7041437276228,37.2175347888796));
#54521=CARTESIAN_POINT('Ctrl Pts',(22.2222782722452,16.6999121791414,37.2914613932861));
#54522=CARTESIAN_POINT('Ctrl Pts',(22.2468359093081,16.6956806306599,37.3667068542911));
#54523=CARTESIAN_POINT('Ctrl Pts',(22.271365181622,16.6914539697338,37.4418654047105));
#54524=CARTESIAN_POINT('Ctrl Pts',(22.2921463271752,16.6872273088077,37.5183393411322));
#54525=CARTESIAN_POINT('Ctrl Pts',(22.3090458658434,16.6830006478815,37.595720682229));
#54526=CARTESIAN_POINT('Ctrl Pts',(22.3259347369962,16.6787766549555,37.673053177812));
#54527=CARTESIAN_POINT('Ctrl Pts',(22.3389467648653,16.6745526620295,37.7512914843803));
#54528=CARTESIAN_POINT('Ctrl Pts',(22.3479987112492,16.6703286691035,37.830013902447));
#54529=CARTESIAN_POINT('Ctrl Pts',(22.3570477621636,16.666106027317,37.90871113937));
#54530=CARTESIAN_POINT('Ctrl Pts',(22.3621391935407,16.6618833855305,37.9878917149128));
#54531=CARTESIAN_POINT('Ctrl Pts',(22.3632413728821,16.657660743744,38.0671266917047));
#54532=CARTESIAN_POINT('Ctrl Pts',(22.3643435428311,16.6534381379415,38.1463609932818));
#54533=CARTESIAN_POINT('Ctrl Pts',(22.3614565232461,16.649215532139,38.225649226439));
#54534=CARTESIAN_POINT('Ctrl Pts',(22.3546007947898,16.6449929263365,38.3045618196903));
#54535=CARTESIAN_POINT('Ctrl Pts',(22.3477382491916,16.6407661216945,38.3835528813872));
#54536=CARTESIAN_POINT('Ctrl Pts',(22.3368991524943,16.6365393170525,38.4621670889591));
#54537=CARTESIAN_POINT('Ctrl Pts',(22.3221559084624,16.6323125124106,38.5399799741959));
#54538=CARTESIAN_POINT('Ctrl Pts',(22.3074055201127,16.6280836595331,38.6178305661934));
#54539=CARTESIAN_POINT('Ctrl Pts',(22.2887473260514,16.6238548066556,38.6948786061157));
#54540=CARTESIAN_POINT('Ctrl Pts',(22.2663043567007,16.6196259537782,38.7707123106814));
#54541=CARTESIAN_POINT('Ctrl Pts',(22.243821052416,16.6153895007254,38.8466823050321));
#54542=CARTESIAN_POINT('Ctrl Pts',(22.2175395374991,16.6111530476726,38.9214331600404));
#54543=CARTESIAN_POINT('Ctrl Pts',(22.1876319028733,16.6069165946198,38.9945709018468));
#54544=CARTESIAN_POINT('Ctrl Pts',(22.1604496779387,16.6030661991858,39.0610437798883));
#54545=CARTESIAN_POINT('Ctrl Pts',(22.1302728228948,16.5992158037517,39.1261841750898));
#54546=CARTESIAN_POINT('Ctrl Pts',(22.0972628992025,16.5953654083177,39.1897149960098));
#54547=CARTESIAN_POINT('Ctrl Pts',(22.0609330588231,16.5911277659402,39.2596353207192));
#54548=CARTESIAN_POINT('Ctrl Pts',(22.0210346055926,16.5868901235628,39.3278681130252));
#54549=CARTESIAN_POINT('Ctrl Pts',(21.9777481980008,16.5826524811853,39.39402569766));
#54550=CARTESIAN_POINT('Ctrl Pts',(21.934524037962,16.5784209327038,39.4600881450917));
#54551=CARTESIAN_POINT('Ctrl Pts',(21.8879218534632,16.5741893842224,39.5240809222287));
#54552=CARTESIAN_POINT('Ctrl Pts',(21.8381684694959,16.569957835741,39.5856403059459));
#54553=CARTESIAN_POINT('Ctrl Pts',(21.7884725520609,16.5657311748149,39.647128586875));
#54554=CARTESIAN_POINT('Ctrl Pts',(21.7356329613737,16.5615045138888,39.7061886970871));
#54555=CARTESIAN_POINT('Ctrl Pts',(21.6799192817715,16.5572778529627,39.7624865857));
#54556=CARTESIAN_POINT('Ctrl Pts',(21.62424077038,16.5530538600367,39.8187489373312));
#54557=CARTESIAN_POINT('Ctrl Pts',(21.5656920999659,16.5488298671107,39.872252195892));
#54558=CARTESIAN_POINT('Ctrl Pts',(21.5045817110499,16.5446058741847,39.9226969895389));
#54559=CARTESIAN_POINT('Ctrl Pts',(21.4434908696723,16.5403832323982,39.973125647279));
#54560=CARTESIAN_POINT('Ctrl Pts',(21.3798402982613,16.5361605906118,40.0204974846483));
#54561=CARTESIAN_POINT('Ctrl Pts',(21.3139725997818,16.5319379488253,40.0645524803178));
#54562=CARTESIAN_POINT('Ctrl Pts',(21.2481054626052,16.5277153430229,40.108607100565));
#54563=CARTESIAN_POINT('Ctrl Pts',(21.1800216263722,16.5234927372204,40.1493446758855));
#54564=CARTESIAN_POINT('Ctrl Pts',(21.1100925930311,16.5192701314179,40.1865485558207));
#54565=CARTESIAN_POINT('Ctrl Pts',(21.0400940242417,16.5150433267759,40.2237894302394));
#54566=CARTESIAN_POINT('Ctrl Pts',(20.9682470081103,16.510816522134,40.2574893697395));
#54567=CARTESIAN_POINT('Ctrl Pts',(20.8949470292018,16.506589717492,40.2874780583638));
#54568=CARTESIAN_POINT('Ctrl Pts',(20.8216115304079,16.5023608646146,40.3174812789811));
#54569=CARTESIAN_POINT('Ctrl Pts',(20.7468221090414,16.4981320117371,40.3437695104374));
#54570=CARTESIAN_POINT('Ctrl Pts',(20.6709911665807,16.4939031588597,40.3662218106952));
#54571=CARTESIAN_POINT('Ctrl Pts',(20.5950239392989,16.4896667058069,40.3887144626568));
#54572=CARTESIAN_POINT('Ctrl Pts',(20.5180119074963,16.4854302527541,40.4073572979661));
#54573=CARTESIAN_POINT('Ctrl Pts',(20.4403792382781,16.4811937997014,40.4220802241511));
#54574=CARTESIAN_POINT('Ctrl Pts',(20.3698210445764,16.4773434042671,40.4354614860358));
#54575=CARTESIAN_POINT('Ctrl Pts',(20.2987505439706,16.4734930088329,40.4456053320298));
#54576=CARTESIAN_POINT('Ctrl Pts',(20.2274881231335,16.4696426133987,40.4524964600894));
#54577=CARTESIAN_POINT('Ctrl Pts',(20.1490586060567,16.4654049710212,40.4600806515816));
#54578=CARTESIAN_POINT('Ctrl Pts',(20.0701021824463,16.4611673286437,40.463752665573));
#54579=CARTESIAN_POINT('Ctrl Pts',(19.9910423993541,16.4569296862662,40.4634530251923));
#54580=CARTESIAN_POINT('Ctrl Pts',(19.9120963073325,16.4526981377847,40.4631538157063));
#54581=CARTESIAN_POINT('Ctrl Pts',(19.8330476159014,16.4484665893033,40.4588942959115));
#54582=CARTESIAN_POINT('Ctrl Pts',(19.7543249095037,16.4442350408218,40.4506667545209));
#54583=CARTESIAN_POINT('Ctrl Pts',(19.6756931300059,16.4400083798957,40.4424487161678));
#54584=CARTESIAN_POINT('Ctrl Pts',(19.5973870511724,16.4357817189696,40.4302718126205));
#54585=CARTESIAN_POINT('Ctrl Pts',(19.5198336417941,16.4315550580435,40.4141803536776));
#54586=CARTESIAN_POINT('Ctrl Pts',(19.4423291865447,16.4273310651175,40.3980990521651));
#54587=CARTESIAN_POINT('Ctrl Pts',(19.3655769155092,16.4231070721915,40.3781081948856));
#54588=CARTESIAN_POINT('Ctrl Pts',(19.2899958571583,16.4188830792655,40.3543035638635));
#54589=CARTESIAN_POINT('Ctrl Pts',(19.2144389751162,16.414660437479,40.3305065472904));
#54590=CARTESIAN_POINT('Ctrl Pts',(19.1400530085988,16.4104377956926,40.3028983202196));
#54591=CARTESIAN_POINT('Ctrl Pts',(19.067242572038,16.4062151539061,40.2716247423258));
#54592=CARTESIAN_POINT('Ctrl Pts',(18.9944327559439,16.4019925481036,40.2403514309352));
#54593=CARTESIAN_POINT('Ctrl Pts',(18.9231988732689,16.3977699423011,40.2054130171434));
#54594=CARTESIAN_POINT('Ctrl Pts',(18.8539248867709,16.3935473364987,40.1670032113514));
#54595=CARTESIAN_POINT('Ctrl Pts',(18.7845820161848,16.3893205318567,40.1285552119375));
#54596=CARTESIAN_POINT('Ctrl Pts',(18.7172033455678,16.3850937272147,40.0866291532722));
#54597=CARTESIAN_POINT('Ctrl Pts',(18.6521470237565,16.3808669225727,40.0414640855117));
#54598=CARTESIAN_POINT('Ctrl Pts',(18.5870591767916,16.3766380696953,39.9962771315507));
#54599=CARTESIAN_POINT('Ctrl Pts',(18.5242962921081,16.3724092168178,39.9478483284716));
#54600=CARTESIAN_POINT('Ctrl Pts',(18.4641843088386,16.3681803639404,39.8964577934598));
#54601=CARTESIAN_POINT('Ctrl Pts',(18.4039642911624,16.3639439108876,39.8449748983949));
#54602=CARTESIAN_POINT('Ctrl Pts',(18.3464050356718,16.3597074578348,39.7905199586914));
#54603=CARTESIAN_POINT('Ctrl Pts',(18.291796229896,16.355471004782,39.7334106405624));
#54604=CARTESIAN_POINT('Ctrl Pts',(18.2421637912015,16.3516206093479,39.6815055550976));
#54605=CARTESIAN_POINT('Ctrl Pts',(18.1949682489154,16.3477702139137,39.627408471479));
#54606=CARTESIAN_POINT('Ctrl Pts',(18.150396837276,16.3439198184796,39.5713798222558));
#54607=CARTESIAN_POINT('Ctrl Pts',(18.1014491845843,16.3396913722288,39.5098500038792));
#54608=CARTESIAN_POINT('Ctrl Pts',(18.055478848153,16.3354629259781,39.4457538867371));
#54609=CARTESIAN_POINT('Ctrl Pts',(18.0127667787908,16.3312344797273,39.379411804472));
#54610=CARTESIAN_POINT('Ctrl Pts',(17.9701141914137,16.3270119221254,39.3131621119884));
#54611=CARTESIAN_POINT('Ctrl Pts',(17.9307111177636,16.3227893645235,39.244673053702));
#54612=CARTESIAN_POINT('Ctrl Pts',(17.8947981223519,16.3185668069216,39.1742976753427));
#54613=CARTESIAN_POINT('Ctrl Pts',(17.8589238529128,16.3143488026199,39.1039981846934));
#54614=CARTESIAN_POINT('Ctrl Pts',(17.8265324023101,16.3101307983182,39.0318168291015));
#54615=CARTESIAN_POINT('Ctrl Pts',(17.7978200563048,16.3059127940165,38.9581339851599));
#54616=CARTESIAN_POINT('Ctrl Pts',(17.7691276003764,16.3016977116784,38.8845021839802));
#54617=CARTESIAN_POINT('Ctrl Pts',(17.7441093602402,16.2974826293404,38.8093713963082));
#54618=CARTESIAN_POINT('Ctrl Pts',(17.7229142175799,16.2932675470023,38.7331435701324));
#54619=CARTESIAN_POINT('Ctrl Pts',(17.7017280833147,16.2890542561656,38.6569481424357));
#54620=CARTESIAN_POINT('Ctrl Pts',(17.684361942341,16.2848409653289,38.5796570559792));
#54621=CARTESIAN_POINT('Ctrl Pts',(17.6709148711716,16.2806276744923,38.501687569599));
#54622=CARTESIAN_POINT('Ctrl Pts',(17.6574647965297,16.2764134425954,38.4237006683329));
#54623=CARTESIAN_POINT('Ctrl Pts',(17.6479356260872,16.2721992106985,38.3450355274437));
#54624=CARTESIAN_POINT('Ctrl Pts',(17.6423751305849,16.2679849788017,38.2661186805136));
#54625=CARTESIAN_POINT('Ctrl Pts',(17.6384351768251,16.2649989357772,38.210201230773));
#54626=CARTESIAN_POINT('Ctrl Pts',(17.6364866553968,16.2620128927528,38.1541576109328));
#54627=CARTESIAN_POINT('Ctrl Pts',(17.6365307316187,16.2590268497283,38.0981403448729));
#54628=CARTESIAN_POINT('',(17.636530005568,15.4652768497734,38.0998377669048));
#54629=CARTESIAN_POINT('Ctrl Pts',(17.6365307316195,16.259026849677,38.0981403439098));
#54630=CARTESIAN_POINT('Ctrl Pts',(17.6366038466735,16.2540735080734,38.0052171501665));
#54631=CARTESIAN_POINT('Ctrl Pts',(17.6421609997246,16.2491201664698,37.9125229754199));
#54632=CARTESIAN_POINT('Ctrl Pts',(17.653098020552,16.2441668248662,37.8206408409181));
#54633=CARTESIAN_POINT('Ctrl Pts',(17.6641551639284,16.239159080146,37.727749554438));
#54634=CARTESIAN_POINT('Ctrl Pts',(17.6807109058829,16.2341513354258,37.6356883472259));
#54635=CARTESIAN_POINT('Ctrl Pts',(17.7026082430101,16.2291435907056,37.5450391402859));
#54636=CARTESIAN_POINT('Ctrl Pts',(17.7185635738396,16.2254947349905,37.4789882740199));
#54637=CARTESIAN_POINT('Ctrl Pts',(17.7373538323789,16.2218458792755,37.4136866406475));
#54638=CARTESIAN_POINT('Ctrl Pts',(17.7589024384412,16.2181970235604,37.3493521728034));
#54639=CARTESIAN_POINT('Ctrl Pts',(17.7839281707136,16.2139593811829,37.2746365664432));
#54640=CARTESIAN_POINT('Ctrl Pts',(17.8127413629706,16.2097217388054,37.2010335741935));
#54641=CARTESIAN_POINT('Ctrl Pts',(17.8452237804385,16.2054840964279,37.1289542315048));
#54642=CARTESIAN_POINT('Ctrl Pts',(17.8776594869154,16.2012525479464,37.0569785417395));
#54643=CARTESIAN_POINT('Ctrl Pts',(17.913753748976,16.1970209994649,36.9865225741272));
#54644=CARTESIAN_POINT('Ctrl Pts',(17.9533390046607,16.1927894509835,36.9179808753422));
#54645=CARTESIAN_POINT('Ctrl Pts',(17.9928785382819,16.1885627900573,36.8495183441121));
#54646=CARTESIAN_POINT('Ctrl Pts',(18.0359008192869,16.1843361291312,36.7829660917124));
#54647=CARTESIAN_POINT('Ctrl Pts',(18.0821914356272,16.1801094682051,36.7186959960536));
#54648=CARTESIAN_POINT('Ctrl Pts',(18.1284528318879,16.1758854752791,36.654466469682));
#54649=CARTESIAN_POINT('Ctrl Pts',(18.1779781952551,16.1716614823531,36.5925166200672));
#54650=CARTESIAN_POINT('Ctrl Pts',(18.2305093414933,16.167437489427,36.5331901039509));
#54651=CARTESIAN_POINT('Ctrl Pts',(18.2830236844577,16.1632148476406,36.4738825647609));
#54652=CARTESIAN_POINT('Ctrl Pts',(18.3385415904698,16.1589922058541,36.4171970434279));
#54653=CARTESIAN_POINT('Ctrl Pts',(18.3967650140825,16.1547695640676,36.3634436315425));
#54654=CARTESIAN_POINT('Ctrl Pts',(18.4549879415343,16.1505469582652,36.3096906777262));
#54655=CARTESIAN_POINT('Ctrl Pts',(18.5159159953454,16.1463243524627,36.2588701006136));
#54656=CARTESIAN_POINT('Ctrl Pts',(18.5792158437952,16.1421017466602,36.2112536373623));
#54657=CARTESIAN_POINT('Ctrl Pts',(18.6425786358197,16.1378749420182,36.1635898256498));
#54658=CARTESIAN_POINT('Ctrl Pts',(18.708317558001,16.1336481373762,36.119136774463));
#54659=CARTESIAN_POINT('Ctrl Pts',(18.7760683885785,16.1294213327342,36.0781241750634));
#54660=CARTESIAN_POINT('Ctrl Pts',(18.8438520500214,16.1251924798568,36.0370917016767));
#54661=CARTESIAN_POINT('Ctrl Pts',(18.9136491487901,16.1209636269793,35.9995032238547));
#54662=CARTESIAN_POINT('Ctrl Pts',(18.9850710807823,16.1167347741018,35.9655422867071));
#54663=CARTESIAN_POINT('Ctrl Pts',(19.0566213736375,16.1124983210491,35.9315203143134));
#54664=CARTESIAN_POINT('Ctrl Pts',(19.1298019005486,16.1082618679963,35.9011390893245));
#54665=CARTESIAN_POINT('Ctrl Pts',(19.2042045345491,16.1040254149435,35.8745337526559));
#54666=CARTESIAN_POINT('Ctrl Pts',(19.2718270382484,16.1001750195095,35.8503528953319));
#54667=CARTESIAN_POINT('Ctrl Pts',(19.3404586002684,16.0963246240755,35.8292905506849));
#54668=CARTESIAN_POINT('Ctrl Pts',(19.4097851015669,16.0924742286415,35.811411610934));
#54669=CARTESIAN_POINT('Ctrl Pts',(19.486083997309,16.088236586264,35.7917345273588));
#54670=CARTESIAN_POINT('Ctrl Pts',(19.5635112061767,16.0839989438865,35.7758402565973));
#54671=CARTESIAN_POINT('Ctrl Pts',(19.641657564465,16.079761301509,35.7638533565303));
#54672=CARTESIAN_POINT('Ctrl Pts',(19.7196915452233,16.0755297530276,35.751883694096));
#54673=CARTESIAN_POINT('Ctrl Pts',(19.7984421621203,16.0712982045461,35.7438103141239));
#54674=CARTESIAN_POINT('Ctrl Pts',(19.8774872328106,16.0670666560647,35.7397074200906));
#54675=CARTESIAN_POINT('Ctrl Pts',(19.9564410042614,16.0628399951386,35.7356092650132));
#54676=CARTESIAN_POINT('Ctrl Pts',(20.0356880878631,16.0586133342125,35.7354725064737));
#54677=CARTESIAN_POINT('Ctrl Pts',(20.1147998151938,16.0543866732864,35.7393197075141));
#54678=CARTESIAN_POINT('Ctrl Pts',(20.1938616047369,16.0501626803604,35.7431644800813));
#54679=CARTESIAN_POINT('Ctrl Pts',(20.272787740605,16.0459386874344,35.7509881979192));
#54680=CARTESIAN_POINT('Ctrl Pts',(20.3511494014435,16.0417146945083,35.7627613432159));
#54681=CARTESIAN_POINT('Ctrl Pts',(20.4294859965346,16.0374920527219,35.7745307226062));
#54682=CARTESIAN_POINT('Ctrl Pts',(20.5072580119162,16.0332694109354,35.790246951167));
#54683=CARTESIAN_POINT('Ctrl Pts',(20.5840430850772,16.029046769149,35.8098288021038));
#54684=CARTESIAN_POINT('Ctrl Pts',(20.6608275039008,16.0248241633465,35.8294104861703));
#54685=CARTESIAN_POINT('Ctrl Pts',(20.7366245433448,16.020601557544,35.8528576098902));
#54686=CARTESIAN_POINT('Ctrl Pts',(20.811024807616,16.0163789517415,35.8800384682767));
#54687=CARTESIAN_POINT('Ctrl Pts',(20.8854990534009,16.0121521470995,35.9072463545382));
#54688=CARTESIAN_POINT('Ctrl Pts',(20.9585733083183,16.0079253424576,35.9381952304075));
#54689=CARTESIAN_POINT('Ctrl Pts',(21.0298566329685,16.0036985378156,35.9727045911696));
#54690=CARTESIAN_POINT('Ctrl Pts',(21.1011745002687,15.9994696849381,36.0072306745633));
#54691=CARTESIAN_POINT('Ctrl Pts',(21.1706992967924,15.9952408320607,36.0453204544234));
#54692=CARTESIAN_POINT('Ctrl Pts',(21.2380655214756,15.9910119791832,36.0867478534884));
#54693=CARTESIAN_POINT('Ctrl Pts',(21.305552818027,15.9867755261305,36.128249706668));
#54694=CARTESIAN_POINT('Ctrl Pts',(21.3708734039049,15.9825390730777,36.1731008985285));
#54695=CARTESIAN_POINT('Ctrl Pts',(21.4336917557667,15.9783026200249,36.221032626588));
#54696=CARTESIAN_POINT('Ctrl Pts',(21.4907856246657,15.9744522245907,36.2645964533493));
#54697=CARTESIAN_POINT('Ctrl Pts',(21.5458127406541,15.9706018291565,36.3107042636834));
#54698=CARTESIAN_POINT('Ctrl Pts',(21.5985476815967,15.9667514337223,36.3591278764476));
#54699=CARTESIAN_POINT('Ctrl Pts',(21.6565863491395,15.9625137913448,36.4124216113454));
#54700=CARTESIAN_POINT('Ctrl Pts',(21.7120659185459,15.9582761489673,36.4687209709738));
#54701=CARTESIAN_POINT('Ctrl Pts',(21.7646591799044,15.9540385065898,36.5277505224427));
#54702=CARTESIAN_POINT('Ctrl Pts',(21.8171768100892,15.9498069581084,36.5866951871001));
#54703=CARTESIAN_POINT('Ctrl Pts',(21.866816065716,15.9455754096269,36.6483618995684));
#54704=CARTESIAN_POINT('Ctrl Pts',(21.9132848910425,15.9413438611455,36.7124368963508));
#54705=CARTESIAN_POINT('Ctrl Pts',(21.9597000435925,15.9371172002194,36.7764378847426));
#54706=CARTESIAN_POINT('Ctrl Pts',(22.0029517692095,15.9328905392933,36.8428412520777));
#54707=CARTESIAN_POINT('Ctrl Pts',(22.0427878010359,15.9286638783672,36.9112996841765));
#54708=CARTESIAN_POINT('Ctrl Pts',(22.0825986871176,15.9244398854412,36.9797149031797));
#54709=CARTESIAN_POINT('Ctrl Pts',(22.1189979238627,15.9202158925152,37.0501822079974));
#54710=CARTESIAN_POINT('Ctrl Pts',(22.1517768501069,15.9159918995891,37.1223258067004));
#54711=CARTESIAN_POINT('Ctrl Pts',(22.1845452912711,15.9117692578027,37.1944463286437));
#54712=CARTESIAN_POINT('Ctrl Pts',(22.2136955277962,15.9075466160162,37.268241653206));
#54713=CARTESIAN_POINT('Ctrl Pts',(22.2390657912856,15.9033239742298,37.3433132595358));
#54714=CARTESIAN_POINT('Ctrl Pts',(22.264435838578,15.8991013684273,37.4183842261298));
#54715=CARTESIAN_POINT('Ctrl Pts',(22.2860258281536,15.8948787626248,37.4947310083105));
#54716=CARTESIAN_POINT('Ctrl Pts',(22.3037233943808,15.8906561568223,37.5719384855126));
#54717=CARTESIAN_POINT('Ctrl Pts',(22.3214385585661,15.8864293521804,37.6492227356412));
#54718=CARTESIAN_POINT('Ctrl Pts',(22.3352534630509,15.8822025475384,37.7273689323715));
#54719=CARTESIAN_POINT('Ctrl Pts',(22.3451067251845,15.8779757428964,37.8059508741821));
#54720=CARTESIAN_POINT('Ctrl Pts',(22.3549647620363,15.873746890019,37.8845708954249));
#54721=CARTESIAN_POINT('Ctrl Pts',(22.3608572972967,15.8695180371415,37.9636266143177));
#54722=CARTESIAN_POINT('Ctrl Pts',(22.3627750246368,15.8652891842641,38.0426883619788));
#54723=CARTESIAN_POINT('Ctrl Pts',(22.3646961985532,15.8610527312113,38.1218922009259));
#54724=CARTESIAN_POINT('Ctrl Pts',(22.3626283032048,15.8568162781586,38.2011016205651));
#54725=CARTESIAN_POINT('Ctrl Pts',(22.3566141910047,15.8525798251058,38.2798888424977));
#54726=CARTESIAN_POINT('Ctrl Pts',(22.3511481301591,15.8487294296716,38.3514963773439));
#54727=CARTESIAN_POINT('Ctrl Pts',(22.3424229969077,15.8448790342374,38.4227549608094));
#54728=CARTESIAN_POINT('Ctrl Pts',(22.3305074997377,15.8410286388033,38.4933512864683));
#54729=CARTESIAN_POINT('Ctrl Pts',(22.3173936217945,15.8367909964258,38.5710477169836));
#54730=CARTESIAN_POINT('Ctrl Pts',(22.3003654146412,15.8325533540483,38.6482334713512));
#54731=CARTESIAN_POINT('Ctrl Pts',(22.2794758180211,15.8283157116708,38.7244841358731));
#54732=CARTESIAN_POINT('Ctrl Pts',(22.2586162614607,15.8240841631893,38.8006251489472));
#54733=CARTESIAN_POINT('Ctrl Pts',(22.2339064656764,15.8198526147078,38.8758332942387));
#54734=CARTESIAN_POINT('Ctrl Pts',(22.2054506603784,15.8156210662264,38.9496927830319));
#54735=CARTESIAN_POINT('Ctrl Pts',(22.1770277223214,15.8113944053003,39.0234669620759));
#54736=CARTESIAN_POINT('Ctrl Pts',(22.1448675407564,15.8071677443741,39.0958951450162));
#54737=CARTESIAN_POINT('Ctrl Pts',(22.1091241484778,15.802941083448,39.1665766579143));
#54738=CARTESIAN_POINT('Ctrl Pts',(22.0734033185423,15.798717090522,39.237213554439));
#54739=CARTESIAN_POINT('Ctrl Pts',(22.0341039783771,15.794493097596,39.3061055521348));
#54740=CARTESIAN_POINT('Ctrl Pts',(21.9914277859658,15.7902691046699,39.3728730550151));
#54741=CARTESIAN_POINT('Ctrl Pts',(21.9487652444987,15.7860464628835,39.4396192008014));
#54742=CARTESIAN_POINT('Ctrl Pts',(21.902728248056,15.781823821097,39.504241806562));
#54743=CARTESIAN_POINT('Ctrl Pts',(21.853563046577,15.7776011793105,39.5663882409732));
#54744=CARTESIAN_POINT('Ctrl Pts',(21.8043982640677,15.773378573508,39.6285341457927));
#54745=CARTESIAN_POINT('Ctrl Pts',(21.7521056214914,15.7691559677055,39.688203554468));
#54746=CARTESIAN_POINT('Ctrl Pts',(21.6969721854293,15.764933361903,39.745076242239));
#54747=CARTESIAN_POINT('Ctrl Pts',(21.6417839262414,15.7607065572611,39.8020054825985));
#54748=CARTESIAN_POINT('Ctrl Pts',(21.583749558053,15.7564797526191,39.8561321096719));
#54749=CARTESIAN_POINT('Ctrl Pts',(21.5231931947481,15.7522529479771,39.9071726349116));
#54750=CARTESIAN_POINT('Ctrl Pts',(21.4626074868906,15.7480240950996,39.9582378934955));
#54751=CARTESIAN_POINT('Ctrl Pts',(21.399497722983,15.7437952422221,40.0062137870362));
#54752=CARTESIAN_POINT('Ctrl Pts',(21.3342192725583,15.7395663893447,40.0508586247173));
#54753=CARTESIAN_POINT('Ctrl Pts',(21.2688235024532,15.7353299362919,40.0955836989552));
#54754=CARTESIAN_POINT('Ctrl Pts',(21.201251658751,15.7310934832391,40.13696551005));
#54755=CARTESIAN_POINT('Ctrl Pts',(21.1318859169762,15.7268570301863,40.1748071505205));
#54756=CARTESIAN_POINT('Ctrl Pts',(21.068841305817,15.7230066347523,40.2092003747266));
#54757=CARTESIAN_POINT('Ctrl Pts',(21.0043153897533,15.7191562393182,40.2406697220902));
#54758=CARTESIAN_POINT('Ctrl Pts',(20.9386083918615,15.7153058438842,40.2691022861145));
#54759=CARTESIAN_POINT('Ctrl Pts',(20.8662930248988,15.7110682015067,40.3003944066965));
#54760=CARTESIAN_POINT('Ctrl Pts',(20.7922753391364,15.7068305591292,40.3281249442038));
#54761=CARTESIAN_POINT('Ctrl Pts',(20.7169401784524,15.7025929167518,40.3521072846161));
#54762=CARTESIAN_POINT('Ctrl Pts',(20.6417133526858,15.6983613682703,40.3760551374816));
#54763=CARTESIAN_POINT('Ctrl Pts',(20.5651732574545,15.6941298197889,40.3962653563772));
#54764=CARTESIAN_POINT('Ctrl Pts',(20.4877254203701,15.6898982713074,40.4125990476572));
#54765=CARTESIAN_POINT('Ctrl Pts',(20.4103670376762,15.6856716103813,40.4289138730726));
#54766=CARTESIAN_POINT('Ctrl Pts',(20.3321034530588,15.6814449494552,40.4413609725379));
#54767=CARTESIAN_POINT('Ctrl Pts',(20.253354624421,15.6772182885291,40.4498514581106));
#54768=CARTESIAN_POINT('Ctrl Pts',(20.1746555044978,15.6729942956031,40.4583365842242));
#54769=CARTESIAN_POINT('Ctrl Pts',(20.0954722133811,15.6687703026771,40.4628700036633));
#54770=CARTESIAN_POINT('Ctrl Pts',(20.0162329514462,15.6645463097511,40.4634142531912));
#54771=CARTESIAN_POINT('Ctrl Pts',(19.9370190359792,15.6603236679647,40.4639583286286));
#54772=CARTESIAN_POINT('Ctrl Pts',(19.8577496536712,15.6561010261782,40.4605157648734));
#54773=CARTESIAN_POINT('Ctrl Pts',(19.7788546581015,15.6518783843917,40.4531011832594));
#54774=CARTESIAN_POINT('Ctrl Pts',(19.6999603348493,15.6476557785893,40.44568666483));
#54775=CARTESIAN_POINT('Ctrl Pts',(19.6214408585744,15.6434331727868,40.4343002411278));
#54776=CARTESIAN_POINT('Ctrl Pts',(19.5437211159885,15.6392105669843,40.419008413289));
#54777=CARTESIAN_POINT('Ctrl Pts',(19.465924091094,15.6349837623423,40.4037013796901));
#54778=CARTESIAN_POINT('Ctrl Pts',(19.3889288493932,15.6307569577003,40.3844812755086));
#54779=CARTESIAN_POINT('Ctrl Pts',(19.3131496269433,15.6265301530584,40.3614656764877));
#54780=CARTESIAN_POINT('Ctrl Pts',(19.2373336832101,15.6223013001809,40.3384389245108));
#54781=CARTESIAN_POINT('Ctrl Pts',(19.162735374289,15.6180724473035,40.3116131725631));
#54782=CARTESIAN_POINT('Ctrl Pts',(19.0897508870357,15.613843594426,40.2811549677287));
#54783=CARTESIAN_POINT('Ctrl Pts',(19.016635230665,15.6096071413733,40.2506420228257));
#54784=CARTESIAN_POINT('Ctrl Pts',(18.9451396152065,15.6053706883205,40.2164837833961));
#54785=CARTESIAN_POINT('Ctrl Pts',(18.8756372516807,15.6011342352677,40.1788936603617));
#54786=CARTESIAN_POINT('Ctrl Pts',(18.812468468774,15.5972838398335,40.1447290334203));
#54787=CARTESIAN_POINT('Ctrl Pts',(18.7509461044902,15.5934334443993,40.1077302177537));
#54788=CARTESIAN_POINT('Ctrl Pts',(18.6913282945177,15.5895830489651,40.068087601752));
#54789=CARTESIAN_POINT('Ctrl Pts',(18.6258430801067,15.5853537092646,40.0245434794524));
#54790=CARTESIAN_POINT('Ctrl Pts',(18.562408207784,15.5811243695641,39.9776440370525));
#54791=CARTESIAN_POINT('Ctrl Pts',(18.5013888786173,15.5768950298636,39.9276091342976));
#54792=CARTESIAN_POINT('Ctrl Pts',(18.4404573839953,15.5726717781049,39.877646254506));
#54793=CARTESIAN_POINT('Ctrl Pts',(18.3819348891868,15.5684485263462,39.8245571725519));
#54794=CARTESIAN_POINT('Ctrl Pts',(18.3261579033514,15.5642252745875,39.7686051289587));
#54795=CARTESIAN_POINT('Ctrl Pts',(18.270445109776,15.5600068832578,39.7127174790947));
#54796=CARTESIAN_POINT('Ctrl Pts',(18.2174718773639,15.555788491928,39.653973746503));
#54797=CARTESIAN_POINT('Ctrl Pts',(18.1675406756892,15.5515701005982,39.5926765442139));
#54798=CARTESIAN_POINT('Ctrl Pts',(18.1176407085403,15.5473543480884,39.5314176864665));
#54799=CARTESIAN_POINT('Ctrl Pts',(18.0707792919992,15.5431385955786,39.4676088933301));
#54800=CARTESIAN_POINT('Ctrl Pts',(18.0272202703293,15.5389228430688,39.4015877147163));
#54801=CARTESIAN_POINT('Ctrl Pts',(17.9836747889534,15.534708401023,39.3355870587437));
#54802=CARTESIAN_POINT('Ctrl Pts',(17.9434299231902,15.5304939589772,39.2673757756398));
#54803=CARTESIAN_POINT('Ctrl Pts',(17.9067067320743,15.5262795169313,39.1973211632686));
#54804=CARTESIAN_POINT('Ctrl Pts',(17.8699833996676,15.5220650586706,39.1272662813651));
#54805=CARTESIAN_POINT('Ctrl Pts',(17.8367819859386,15.5178506004099,39.0553684739288));
#54806=CARTESIAN_POINT('Ctrl Pts',(17.8072773195312,15.5136361421492,38.9820190969915));
#54807=CARTESIAN_POINT('Ctrl Pts',(17.7777432368352,15.5094174820542,38.9085965903869));
#54808=CARTESIAN_POINT('Ctrl Pts',(17.751913438361,15.5051988219591,38.8337200617956));
#54809=CARTESIAN_POINT('Ctrl Pts',(17.7299140914899,15.5009801618641,38.7577996723045));
#54810=CARTESIAN_POINT('Ctrl Pts',(17.7079037028745,15.4967593843713,38.6818411774307));
#54811=CARTESIAN_POINT('Ctrl Pts',(17.6897277029013,15.4925386068786,38.6048382369578));
#54812=CARTESIAN_POINT('Ctrl Pts',(17.6754613444804,15.4883178293859,38.5272124528792));
#54813=CARTESIAN_POINT('Ctrl Pts',(17.6611698301982,15.4840896093987,38.4494497913022));
#54814=CARTESIAN_POINT('Ctrl Pts',(17.6508017904135,15.4798613894116,38.3710625597964));
#54815=CARTESIAN_POINT('Ctrl Pts',(17.644380654783,15.4756331694244,38.2924784178537));
#54816=CARTESIAN_POINT('Ctrl Pts',(17.6391381545257,15.4721810628741,38.2283188348667));
#54817=CARTESIAN_POINT('Ctrl Pts',(17.6365255994157,15.4687289563237,38.1640281765003));
#54818=CARTESIAN_POINT('Ctrl Pts',(17.636530005568,15.4652768497734,38.0998377669048));
#54819=CARTESIAN_POINT('',(17.6365308344677,14.6715268497713,38.1019860710541));
#54820=CARTESIAN_POINT('Ctrl Pts',(17.6365300055681,15.4652768497283,38.0998377660665));
#54821=CARTESIAN_POINT('Ctrl Pts',(17.6365306082695,15.4648046511675,38.0910574406093));
#54822=CARTESIAN_POINT('Ctrl Pts',(17.6365801393059,15.4643324526068,38.0822773116373));
#54823=CARTESIAN_POINT('Ctrl Pts',(17.6366785934394,15.463860254046,38.0734977323131));
#54824=CARTESIAN_POINT('Ctrl Pts',(17.6375621484591,15.4596226116686,37.9947073240134));
#54825=CARTESIAN_POINT('Ctrl Pts',(17.6423918430063,15.4553849692911,37.9158132522039));
#54826=CARTESIAN_POINT('Ctrl Pts',(17.6511813180016,15.4511473269136,37.8372430020054));
#54827=CARTESIAN_POINT('Ctrl Pts',(17.6599581533869,15.4469157784321,37.7587857389101));
#54828=CARTESIAN_POINT('Ctrl Pts',(17.6726834091438,15.4426842299507,37.6806518346703));
#54829=CARTESIAN_POINT('Ctrl Pts',(17.6893187190147,15.4384526814692,37.6032682226753));
#54830=CARTESIAN_POINT('Ctrl Pts',(17.7059348146433,15.4342260205431,37.5259739908891));
#54831=CARTESIAN_POINT('Ctrl Pts',(17.726451891496,15.429999359617,37.4494287851626));
#54832=CARTESIAN_POINT('Ctrl Pts',(17.7507800366961,15.4257726986909,37.3740523451549));
#54833=CARTESIAN_POINT('Ctrl Pts',(17.7750928252128,15.4215487057649,37.2987234851051));
#54834=CARTESIAN_POINT('Ctrl Pts',(17.8032117634887,15.4173247128389,37.224562371345));
#54835=CARTESIAN_POINT('Ctrl Pts',(17.8349966170261,15.4131007199129,37.1519753206737));
#54836=CARTESIAN_POINT('Ctrl Pts',(17.8667713034602,15.4088780781264,37.0794114886103));
#54837=CARTESIAN_POINT('Ctrl Pts',(17.9022093886558,15.4046554363399,37.0084211488845));
#54838=CARTESIAN_POINT('Ctrl Pts',(17.9411223983249,15.4004327945535,36.9393909089532));
#54839=CARTESIAN_POINT('Ctrl Pts',(17.9800350763898,15.396210188751,36.8703612572753));
#54840=CARTESIAN_POINT('Ctrl Pts',(18.0224223886087,15.3919875829485,36.8032920798383));
#54841=CARTESIAN_POINT('Ctrl Pts',(18.068050504909,15.387764977146,36.738544312393));
#54842=CARTESIAN_POINT('Ctrl Pts',(18.1137239925146,15.383538172504,36.6737321616032));
#54843=CARTESIAN_POINT('Ctrl Pts',(18.1626444506268,15.3793113678621,36.6112464158093));
#54844=CARTESIAN_POINT('Ctrl Pts',(18.2145357442956,15.3750845632201,36.5514174763669));
#54845=CARTESIAN_POINT('Ctrl Pts',(18.266452183576,15.3708557103426,36.4915595448689));
#54846=CARTESIAN_POINT('Ctrl Pts',(18.3213420013016,15.3666268574652,36.4343613231174));
#54847=CARTESIAN_POINT('Ctrl Pts',(18.3788916926052,15.3623980045877,36.3801167782098));
#54848=CARTESIAN_POINT('Ctrl Pts',(18.4365448133155,15.3581615515349,36.3257747439678));
#54849=CARTESIAN_POINT('Ctrl Pts',(18.4968670015372,15.3539250984822,36.274397297954));
#54850=CARTESIAN_POINT('Ctrl Pts',(18.5595113142642,15.3496886454294,36.2262383323466));
#54851=CARTESIAN_POINT('Ctrl Pts',(18.6164470037892,15.3458382499952,36.1824679756406));
#54852=CARTESIAN_POINT('Ctrl Pts',(18.6753002715313,15.3419878545611,36.1413558540245));
#54853=CARTESIAN_POINT('Ctrl Pts',(18.7357920812526,15.3381374591269,36.1030601463548));
#54854=CARTESIAN_POINT('Ctrl Pts',(18.8023677514014,15.3338998167494,36.060912913305));
#54855=CARTESIAN_POINT('Ctrl Pts',(18.8711784054627,15.3296621743719,36.0220195410704));
#54856=CARTESIAN_POINT('Ctrl Pts',(18.9418728652621,15.3254245319944,35.9866241679173));
#54857=CARTESIAN_POINT('Ctrl Pts',(19.0124656636541,15.321192983513,35.9512796946997));
#54858=CARTESIAN_POINT('Ctrl Pts',(19.0849364722815,15.3169614350315,35.9194234390696));
#54859=CARTESIAN_POINT('Ctrl Pts',(19.1589062664445,15.31272988655,35.8912556118297));
#54860=CARTESIAN_POINT('Ctrl Pts',(19.2327906234526,15.3085032256239,35.8631203192082));
#54861=CARTESIAN_POINT('Ctrl Pts',(19.3081700894616,15.3042765646978,35.8386651547943));
#54862=CARTESIAN_POINT('Ctrl Pts',(19.3846436157027,15.3000499037717,35.8180431728));
#54863=CARTESIAN_POINT('Ctrl Pts',(19.4610688694711,15.2958259108457,35.7974342080434));
#54864=CARTESIAN_POINT('Ctrl Pts',(19.5385863612752,15.2916019179196,35.7806537447508));
#54865=CARTESIAN_POINT('Ctrl Pts',(19.6167789105024,15.2873779249936,35.7678053174179));
#54866=CARTESIAN_POINT('Ctrl Pts',(19.6949464480764,15.2831552832072,35.7549609999447));
#54867=CARTESIAN_POINT('Ctrl Pts',(19.7737881520378,15.2789326414207,35.7460462967408));
#54868=CARTESIAN_POINT('Ctrl Pts',(19.8528771166699,15.2747099996342,35.7411135470098));
#54869=CARTESIAN_POINT('Ctrl Pts',(19.9319654073316,15.2704873938317,35.7361808393142));
#54870=CARTESIAN_POINT('Ctrl Pts',(20.011300486522,15.2662647880292,35.7352300453764));
#54871=CARTESIAN_POINT('Ctrl Pts',(20.0904522949218,15.2620421822268,35.738261482881));
#54872=CARTESIAN_POINT('Ctrl Pts',(20.1696828096359,15.2578153775848,35.7412959347612));
#54873=CARTESIAN_POINT('Ctrl Pts',(20.2487292200167,15.2535885729428,35.7483205098561));
#54874=CARTESIAN_POINT('Ctrl Pts',(20.3271640530113,15.2493617683008,35.7592834167039));
#54875=CARTESIAN_POINT('Ctrl Pts',(20.4056368941516,15.2451329154233,35.7702516359843));
#54876=CARTESIAN_POINT('Ctrl Pts',(20.4834971065262,15.2409040625459,35.7851619005852));
#54877=CARTESIAN_POINT('Ctrl Pts',(20.5603274388273,15.2366752096684,35.8039112381711));
#54878=CARTESIAN_POINT('Ctrl Pts',(20.6372958520721,15.2324387566156,35.8226942724252));
#54879=CARTESIAN_POINT('Ctrl Pts',(20.7132302366212,15.2282023035628,35.8453300316111));
#54880=CARTESIAN_POINT('Ctrl Pts',(20.7877287571503,15.2239658505101,35.8716656790198));
#54881=CARTESIAN_POINT('Ctrl Pts',(20.8554384094741,15.220115455076,35.8956014232077));
#54882=CARTESIAN_POINT('Ctrl Pts',(20.9219619604967,15.2162650596419,35.9225927334175));
#54883=CARTESIAN_POINT('Ctrl Pts',(20.9870148297634,15.2124146642078,35.9524916375653));
#54884=CARTESIAN_POINT('Ctrl Pts',(21.0586102802312,15.2081770218304,35.9853975729234));
#54885=CARTESIAN_POINT('Ctrl Pts',(21.1286927534798,15.2039393794529,36.0219495558988));
#54886=CARTESIAN_POINT('Ctrl Pts',(21.1968662910727,15.1997017370754,36.0619858876363));
#54887=CARTESIAN_POINT('Ctrl Pts',(21.2649417924433,15.195470188594,36.1019646455575));
#54888=CARTESIAN_POINT('Ctrl Pts',(21.3311134088385,15.1912386401125,36.1454175661666));
#54889=CARTESIAN_POINT('Ctrl Pts',(21.395006873294,15.1870070916311,36.1921356797816));
#54890=CARTESIAN_POINT('Ctrl Pts',(21.4588265390337,15.182780430705,36.2387998326853));
#54891=CARTESIAN_POINT('Ctrl Pts',(21.5203729054523,15.1785537697789,36.2887214086112));
#54892=CARTESIAN_POINT('Ctrl Pts',(21.5792992752379,15.1743271088528,36.3416472935918));
#54893=CARTESIAN_POINT('Ctrl Pts',(21.6381884488626,15.1701031159268,36.3945397701045));
#54894=CARTESIAN_POINT('Ctrl Pts',(21.6944605606698,15.1658791230008,36.45043247908));
#54895=CARTESIAN_POINT('Ctrl Pts',(21.7478016726969,15.1616551300748,36.5090318187286));
#54896=CARTESIAN_POINT('Ctrl Pts',(21.8011257223643,15.1574324882883,36.5676124140547));
#54897=CARTESIAN_POINT('Ctrl Pts',(21.8515203187066,15.1532098465019,36.6288975743807));
#54898=CARTESIAN_POINT('Ctrl Pts',(21.8987091761125,15.1489872047154,36.6925576724263));
#54899=CARTESIAN_POINT('Ctrl Pts',(21.9458976313903,15.144764598913,36.7562172279812));
#54900=CARTESIAN_POINT('Ctrl Pts',(21.9898801240436,15.1405419931105,36.8222513035725));
#54901=CARTESIAN_POINT('Ctrl Pts',(22.0304222910095,15.136319387308,36.8902993093035));
#54902=CARTESIAN_POINT('Ctrl Pts',(22.0710047719568,15.1320925826661,36.9584149800422));
#54903=CARTESIAN_POINT('Ctrl Pts',(22.1081398533377,15.1278657780241,37.0285481774607));
#54904=CARTESIAN_POINT('Ctrl Pts',(22.1416382925597,15.1236389733821,37.1003121163373));
#54905=CARTESIAN_POINT('Ctrl Pts',(22.1751529645384,15.1194101205047,37.1721108307612));
#54906=CARTESIAN_POINT('Ctrl Pts',(22.2050273068634,15.1151812676272,37.2455414261018));
#54907=CARTESIAN_POINT('Ctrl Pts',(22.2311205749776,15.1109524147498,37.3201978322601));
#54908=CARTESIAN_POINT('Ctrl Pts',(22.2572607384126,15.106715961697,37.3949884123405));
#54909=CARTESIAN_POINT('Ctrl Pts',(22.2796061172186,15.1024795086443,37.4710087543335));
#54910=CARTESIAN_POINT('Ctrl Pts',(22.2980661879124,15.0982430555915,37.5478385771589));
#54911=CARTESIAN_POINT('Ctrl Pts',(22.3148440374552,15.0943926601573,37.617667085898));
#54912=CARTESIAN_POINT('Ctrl Pts',(22.3284130346181,15.0905422647231,37.6881638658518));
#54913=CARTESIAN_POINT('Ctrl Pts',(22.3387424011334,15.0866918692889,37.7590096452379));
#54914=CARTESIAN_POINT('Ctrl Pts',(22.3501106260407,15.0824542269114,37.8369806178621));
#54915=CARTESIAN_POINT('Ctrl Pts',(22.3575967325203,15.0782165845339,37.9156670762007));
#54916=CARTESIAN_POINT('Ctrl Pts',(22.3611208302554,15.0739789421564,37.9946488451231));
#54917=CARTESIAN_POINT('Ctrl Pts',(22.3646398601997,15.0697473936749,38.0735170351623));
#54918=CARTESIAN_POINT('Ctrl Pts',(22.3642081754316,15.0655158451935,38.1526792279952));
#54919=CARTESIAN_POINT('Ctrl Pts',(22.3597973470375,15.061284296712,38.2317077135734));
#54920=CARTESIAN_POINT('Ctrl Pts',(22.355391613272,15.0570576357859,38.3106449190683));
#54921=CARTESIAN_POINT('Ctrl Pts',(22.3470158953207,15.0528309748598,38.389448258535));
#54922=CARTESIAN_POINT('Ctrl Pts',(22.3346938026217,15.0486043139337,38.4676891199095));
#54923=CARTESIAN_POINT('Ctrl Pts',(22.3223794880116,15.0443803210077,38.5458805932142));
#54924=CARTESIAN_POINT('Ctrl Pts',(22.306123815899,15.0401563280817,38.6235098313147));
#54925=CARTESIAN_POINT('Ctrl Pts',(22.2860021917214,15.0359323351557,38.7001536639435));
#54926=CARTESIAN_POINT('Ctrl Pts',(22.2658870039,15.0317096933692,38.776772980311));
#54927=CARTESIAN_POINT('Ctrl Pts',(22.2419084386302,15.0274870515827,38.8524070640585));
#54928=CARTESIAN_POINT('Ctrl Pts',(22.214192617479,15.0232644097963,38.926644720301));
#54929=CARTESIAN_POINT('Ctrl Pts',(22.186477032513,15.0190418039938,39.0008817439143));
#54930=CARTESIAN_POINT('Ctrl Pts',(22.155024420285,15.0148191981913,39.0737219250184));
#54931=CARTESIAN_POINT('Ctrl Pts',(22.1200096958296,15.0105965923888,39.1447723821428));
#54932=CARTESIAN_POINT('Ctrl Pts',(22.0849601537249,15.0063697877468,39.2158934898276));
#54933=CARTESIAN_POINT('Ctrl Pts',(22.0463416318082,15.0021429831049,39.2852208972095));
#54934=CARTESIAN_POINT('Ctrl Pts',(22.0043755801985,14.9979161784629,39.3523853138727));
#54935=CARTESIAN_POINT('Ctrl Pts',(21.9623891925755,14.9936873255854,39.4195822772354));
#54936=CARTESIAN_POINT('Ctrl Pts',(21.9170523121701,14.989458472708,39.4846137768073));
#54937=CARTESIAN_POINT('Ctrl Pts',(21.8686289657637,14.9852296198305,39.5471407081584));
#54938=CARTESIAN_POINT('Ctrl Pts',(21.8201185919922,14.9809931667777,39.6097800141072));
#54939=CARTESIAN_POINT('Ctrl Pts',(21.7685109747064,14.976756713725,39.6699054013311));
#54940=CARTESIAN_POINT('Ctrl Pts',(21.714109398934,14.9725202606722,39.7272121586893));
#54941=CARTESIAN_POINT('Ctrl Pts',(21.664665305879,14.968669865238,39.7792966912284));
#54942=CARTESIAN_POINT('Ctrl Pts',(21.6129139293989,14.9648194698039,39.829053185278));
#54943=CARTESIAN_POINT('Ctrl Pts',(21.5591063425391,14.9609690743697,39.8762820309721));
#54944=CARTESIAN_POINT('Ctrl Pts',(21.4998871495476,14.9567314319922,39.9282608371432));
#54945=CARTESIAN_POINT('Ctrl Pts',(21.437954583786,14.9524937896147,39.9773725242892));
#54946=CARTESIAN_POINT('Ctrl Pts',(21.3736176294146,14.9482561472372,40.0233213587597));
#54947=CARTESIAN_POINT('Ctrl Pts',(21.3093731941084,14.9440245987557,40.0692041170032));
#54948=CARTESIAN_POINT('Ctrl Pts',(21.2427316149981,14.9397930502743,40.1119327848922));
#54949=CARTESIAN_POINT('Ctrl Pts',(21.1740362093125,14.9355615017928,40.1512506965564));
#54950=CARTESIAN_POINT('Ctrl Pts',(21.1054201487175,14.9313348408667,40.1905231949468));
#54951=CARTESIAN_POINT('Ctrl Pts',(21.0347553805461,14.9271081799406,40.2263925342439));
#54952=CARTESIAN_POINT('Ctrl Pts',(20.9624143050223,14.9228815190145,40.2586452108646));
#54953=CARTESIAN_POINT('Ctrl Pts',(20.8901188934396,14.9186575260884,40.2908775285907));
#54954=CARTESIAN_POINT('Ctrl Pts',(20.8161497018186,14.9144335331624,40.3194975246576));
#54955=CARTESIAN_POINT('Ctrl Pts',(20.7409027598398,14.9102095402364,40.3443381076304));
#54956=CARTESIAN_POINT('Ctrl Pts',(20.6656798872951,14.9059868984499,40.3691707447816));
#54957=CARTESIAN_POINT('Ctrl Pts',(20.5891805208482,14.9017642566634,40.3902262226906));
#54958=CARTESIAN_POINT('Ctrl Pts',(20.5118182510104,14.897541614877,40.4073865126659));
#54959=CARTESIAN_POINT('Ctrl Pts',(20.4344566404286,14.8933190090745,40.4245466564069));
#54960=CARTESIAN_POINT('Ctrl Pts',(20.3562325990354,14.889096403272,40.4378115780941));
#54961=CARTESIAN_POINT('Ctrl Pts',(20.27757091483,14.8848737974695,40.447114148937));
#54962=CARTESIAN_POINT('Ctrl Pts',(20.1988310116759,14.8806469928275,40.4564259699927));
#54963=CARTESIAN_POINT('Ctrl Pts',(20.1196530630481,14.8764201881855,40.461767514756));
#54964=CARTESIAN_POINT('Ctrl Pts',(20.040467397875,14.8721933835435,40.4631235326595));
#54965=CARTESIAN_POINT('Ctrl Pts',(19.9612433607161,14.867964530666,40.4644802076656));
#54966=CARTESIAN_POINT('Ctrl Pts',(19.8820120686772,14.8637356777886,40.4618475239913));
#54967=CARTESIAN_POINT('Ctrl Pts',(19.8032017046315,14.8595068249111,40.4552623785558));
#54968=CARTESIAN_POINT('Ctrl Pts',(19.7242497010912,14.8552703718583,40.4486653981708));
#54969=CARTESIAN_POINT('Ctrl Pts',(19.6457206027955,14.8510339188055,40.4381018253066));
#54970=CARTESIAN_POINT('Ctrl Pts',(19.5680351108609,14.8467974657527,40.4236602108422));
#54971=CARTESIAN_POINT('Ctrl Pts',(19.497428908052,14.8429470703187,40.4105346254289));
#54972=CARTESIAN_POINT('Ctrl Pts',(19.4275196849273,14.8390966748847,40.3942063006677));
#54973=CARTESIAN_POINT('Ctrl Pts',(19.3586115557134,14.8352462794506,40.3747771988561));
#54974=CARTESIAN_POINT('Ctrl Pts',(19.2827731091141,14.8310086370731,40.3533940483191));
#54975=CARTESIAN_POINT('Ctrl Pts',(19.2078628105288,14.8267709946956,40.3281740625552));
#54976=CARTESIAN_POINT('Ctrl Pts',(19.1342969323881,14.8225333523182,40.2992154600283));
#54977=CARTESIAN_POINT('Ctrl Pts',(19.0608368448671,14.8183018038367,40.2702985011082));
#54978=CARTESIAN_POINT('Ctrl Pts',(18.9887177709689,14.8140702553553,40.2376537725005));
#54979=CARTESIAN_POINT('Ctrl Pts',(18.9183418991389,14.8098387068738,40.2014295595479));
#54980=CARTESIAN_POINT('Ctrl Pts',(18.8480473133843,14.8056120459477,40.1652471865615));
#54981=CARTESIAN_POINT('Ctrl Pts',(18.7794923431636,14.8013853850216,40.125493758781));
#54982=CARTESIAN_POINT('Ctrl Pts',(18.7130588003859,14.7971587240956,40.0823654530979));
#54983=CARTESIAN_POINT('Ctrl Pts',(18.6466671925307,14.7929347311695,40.0392643713453));
#54984=CARTESIAN_POINT('Ctrl Pts',(18.582394746287,14.7887107382435,39.9927928947417));
#54985=CARTESIAN_POINT('Ctrl Pts',(18.5205972022698,14.7844867453175,39.9431922859453));
#54986=CARTESIAN_POINT('Ctrl Pts',(18.4588194255931,14.7802641035311,39.893607543024));
#54987=CARTESIAN_POINT('Ctrl Pts',(18.3995153443931,14.7760414617446,39.8408959487613));
#54988=CARTESIAN_POINT('Ctrl Pts',(18.3430091011241,14.7718188199582,39.7853402036214));
#54989=CARTESIAN_POINT('Ctrl Pts',(18.2865033393828,14.7675962141557,39.7297849319094));
#54990=CARTESIAN_POINT('Ctrl Pts',(18.2327957014365,14.7633736083532,39.6713858871789));
#54991=CARTESIAN_POINT('Ctrl Pts',(18.1821737266528,14.7591510025508,39.6104628697286));
#54992=CARTESIAN_POINT('Ctrl Pts',(18.1315014148125,14.7549241979088,39.5494792721569));
#54993=CARTESIAN_POINT('Ctrl Pts',(18.0839211953534,14.7506973932668,39.4859670499826));
#54994=CARTESIAN_POINT('Ctrl Pts',(18.0396801048077,14.7464705886248,39.4202788907702));
#54995=CARTESIAN_POINT('Ctrl Pts',(17.9954175758047,14.7422417357474,39.3545589002268));
#54996=CARTESIAN_POINT('Ctrl Pts',(17.9544976414061,14.73801288287,39.2866612741251));
#54997=CARTESIAN_POINT('Ctrl Pts',(17.9171224251338,14.7337840299925,39.2169652855034));
#54998=CARTESIAN_POINT('Ctrl Pts',(17.8796800374076,14.7295475769398,39.1471440379171));
#54999=CARTESIAN_POINT('Ctrl Pts',(17.8457952978973,14.725311123887,39.0755183946107));
#55000=CARTESIAN_POINT('Ctrl Pts',(17.815622926706,14.7210746708342,39.0024894695051));
#55001=CARTESIAN_POINT('Ctrl Pts',(17.788200090001,14.7172242754,38.9361154919606));
#55002=CARTESIAN_POINT('Ctrl Pts',(17.7638433183341,14.7133738799658,38.8685828232599));
#55003=CARTESIAN_POINT('Ctrl Pts',(17.7426326190174,14.7095234845316,38.8002020766719));
#55004=CARTESIAN_POINT('Ctrl Pts',(17.7143095978416,14.7043819835471,38.7088920588025));
#55005=CARTESIAN_POINT('Ctrl Pts',(17.691509480421,14.6992404825626,38.6157933314888));
#55006=CARTESIAN_POINT('Ctrl Pts',(17.6744210927045,14.6940989815781,38.5215129735158));
#55007=CARTESIAN_POINT('Ctrl Pts',(17.6575525340282,14.6890236220721,38.4284454602508));
#55008=CARTESIAN_POINT('Ctrl Pts',(17.6462497389265,14.683948262566,38.3342265316659));
#55009=CARTESIAN_POINT('Ctrl Pts',(17.6406481563961,14.6788729030599,38.2394608152235));
#55010=CARTESIAN_POINT('Ctrl Pts',(17.6379455876605,14.6764242186304,38.1937396531996));
#55011=CARTESIAN_POINT('Ctrl Pts',(17.6365694097498,14.6739755342008,38.1478915231381));
#55012=CARTESIAN_POINT('Ctrl Pts',(17.6365308344677,14.6715268497713,38.1019860710541));
#55013=CARTESIAN_POINT('',(17.6365303963904,13.8777768497283,38.0986311634849));
#55014=CARTESIAN_POINT('Ctrl Pts',(17.6365308344671,14.6715268497283,38.1019860702482));
#55015=CARTESIAN_POINT('Ctrl Pts',(17.6364646605814,14.6673262575168,38.0232376279563));
#55016=CARTESIAN_POINT('Ctrl Pts',(17.6403385060611,14.6631256653054,37.9444216968236));
#55017=CARTESIAN_POINT('Ctrl Pts',(17.6481459042837,14.6589250730939,37.8659642049545));
#55018=CARTESIAN_POINT('Ctrl Pts',(17.6559505594527,14.6547259567198,37.7875342783647));
#55019=CARTESIAN_POINT('Ctrl Pts',(17.6676859771048,14.6505268403457,37.7094630126979));
#55020=CARTESIAN_POINT('Ctrl Pts',(17.683293711496,14.6463277239716,37.632172666782));
#55021=CARTESIAN_POINT('Ctrl Pts',(17.6989009574053,14.642128739019,37.5548847398548));
#55022=CARTESIAN_POINT('Ctrl Pts',(17.7183801840557,14.6379297540664,37.4783781488536));
#55023=CARTESIAN_POINT('Ctrl Pts',(17.7416218588689,14.6337307691138,37.4030648433597));
#55024=CARTESIAN_POINT('Ctrl Pts',(17.7648867551708,14.6295275888232,37.3276762899725));
#55025=CARTESIAN_POINT('Ctrl Pts',(17.7919214685464,14.6253244085327,37.25348385805));
#55026=CARTESIAN_POINT('Ctrl Pts',(17.8225667841824,14.6211212282421,37.180883559306));
#55027=CARTESIAN_POINT('Ctrl Pts',(17.8532267747405,14.616916035202,37.1082484949309));
#55028=CARTESIAN_POINT('Ctrl Pts',(17.8875006042114,14.6127108421619,37.0372075097695));
#55029=CARTESIAN_POINT('Ctrl Pts',(17.9251822807059,14.6085056491219,36.9681334563637));
#55030=CARTESIAN_POINT('Ctrl Pts',(17.962933700464,14.6042926728854,36.8989315570028));
#55031=CARTESIAN_POINT('Ctrl Pts',(18.0041053208906,14.600079696649,36.8317042684717));
#55032=CARTESIAN_POINT('Ctrl Pts',(18.0484470026627,14.5958667204126,36.7667965873567));
#55033=CARTESIAN_POINT('Ctrl Pts',(18.0907787627588,14.5918447101459,36.7048310444285));
#55034=CARTESIAN_POINT('Ctrl Pts',(18.135999166347,14.5878226998792,36.6449796362851));
#55035=CARTESIAN_POINT('Ctrl Pts',(18.1838579015468,14.5838006896125,36.5875125391838));
#55036=CARTESIAN_POINT('Ctrl Pts',(18.2342824880017,14.579563047235,36.5269644575433));
#55037=CARTESIAN_POINT('Ctrl Pts',(18.2878329422262,14.5753254048575,36.4688271255746));
#55038=CARTESIAN_POINT('Ctrl Pts',(18.344249977709,14.57108776248,36.4134406904638));
#55039=CARTESIAN_POINT('Ctrl Pts',(18.4005858832808,14.5668562139985,36.3581339032201));
#55040=CARTESIAN_POINT('Ctrl Pts',(18.4597798519412,14.5626246655171,36.3055704824781));
#55041=CARTESIAN_POINT('Ctrl Pts',(18.5215326113407,14.5583931170356,36.256057316083));
#55042=CARTESIAN_POINT('Ctrl Pts',(18.5832140445977,14.5541664561095,36.2066013387624));
#55043=CARTESIAN_POINT('Ctrl Pts',(18.6474480314449,14.5499397951834,36.1601889062038));
#55044=CARTESIAN_POINT('Ctrl Pts',(18.7138998638877,14.5457131342573,36.1170887864577));
#55045=CARTESIAN_POINT('Ctrl Pts',(18.780309749863,14.5414891413313,36.0740158728503));
#55046=CARTESIAN_POINT('Ctrl Pts',(18.8489343103774,14.5372651484053,36.0342513763981));
#55047=CARTESIAN_POINT('Ctrl Pts',(18.9194082842053,14.5330411554793,35.998021887684));
#55048=CARTESIAN_POINT('Ctrl Pts',(18.9898597153405,14.5288185136928,35.9618039877903));
#55049=CARTESIAN_POINT('Ctrl Pts',(19.0621589684265,14.5245958719063,35.9291190643558));
#55050=CARTESIAN_POINT('Ctrl Pts',(19.1359158121418,14.5203732301199,35.9001479692503));
#55051=CARTESIAN_POINT('Ctrl Pts',(19.2096720273254,14.5161506243174,35.8711771210271));
#55052=CARTESIAN_POINT('Ctrl Pts',(19.2848853715982,14.5119280185149,35.8459202082597));
#55053=CARTESIAN_POINT('Ctrl Pts',(19.3611466441945,14.5077054127125,35.8245095406317));
#55054=CARTESIAN_POINT('Ctrl Pts',(19.4374837488383,14.5034786080705,35.8030775828429));
#55055=CARTESIAN_POINT('Ctrl Pts',(19.514870410893,14.4992518034285,35.785499636849));
#55056=CARTESIAN_POINT('Ctrl Pts',(19.5928838960292,14.4950249987865,35.771857624889));
#55057=CARTESIAN_POINT('Ctrl Pts',(19.6709351851333,14.4907961459091,35.758209002249));
#55058=CARTESIAN_POINT('Ctrl Pts',(19.7496134365798,14.4865672930316,35.7485001706613));
#55059=CARTESIAN_POINT('Ctrl Pts',(19.8284899342873,14.4823384401542,35.7427612046593));
#55060=CARTESIAN_POINT('Ctrl Pts',(19.9075081903462,14.4781019871014,35.7370119244778));
#55061=CARTESIAN_POINT('Ctrl Pts',(19.9867249348031,14.4738655340486,35.7352467762091));
#55062=CARTESIAN_POINT('Ctrl Pts',(20.0657108174142,14.4696290809959,35.7374436452489));
#55063=CARTESIAN_POINT('Ctrl Pts',(20.1374989094757,14.4657786855617,35.7394403189792));
#55064=CARTESIAN_POINT('Ctrl Pts',(20.2090960695186,14.4619282901276,35.7447091273303));
#55065=CARTESIAN_POINT('Ctrl Pts',(20.2801860349142,14.4580778946935,35.7531965939306));
#55066=CARTESIAN_POINT('Ctrl Pts',(20.3584257521403,14.453840252316,35.7625376729855));
#55067=CARTESIAN_POINT('Ctrl Pts',(20.4363446904957,14.4496026099385,35.7758131978984));
#55068=CARTESIAN_POINT('Ctrl Pts',(20.5135163726699,14.445364967561,35.792990815818));
#55069=CARTESIAN_POINT('Ctrl Pts',(20.5905770789364,14.4411334190795,35.8101437316489));
#55070=CARTESIAN_POINT('Ctrl Pts',(20.6668922092512,14.436901870598,35.8311874958296));
#55071=CARTESIAN_POINT('Ctrl Pts',(20.7420414207746,14.4326703221166,35.8560381084442));
#55072=CARTESIAN_POINT('Ctrl Pts',(20.8171038328835,14.4284436611905,35.880860017915));
#55073=CARTESIAN_POINT('Ctrl Pts',(20.8910025595526,14.4242170002644,35.9094798914121));
#55074=CARTESIAN_POINT('Ctrl Pts',(20.9633299465217,14.4199903393382,35.9417632532471));
#55075=CARTESIAN_POINT('Ctrl Pts',(21.0356116781902,14.4157663464122,35.974026236818));
#55076=CARTESIAN_POINT('Ctrl Pts',(21.1063236119807,14.4115423534862,36.0099479280856));
#55077=CARTESIAN_POINT('Ctrl Pts',(21.1750768437342,14.4073183605602,36.0493452625516));
#55078=CARTESIAN_POINT('Ctrl Pts',(21.2438080832135,14.4030957187737,36.0887299948902));
#55079=CARTESIAN_POINT('Ctrl Pts',(21.3105814583948,14.3988730769872,36.1315879297875));
#55080=CARTESIAN_POINT('Ctrl Pts',(21.3750328417326,14.3946504352008,36.1776901589346));
#55081=CARTESIAN_POINT('Ctrl Pts',(21.4394836758367,14.3904278293983,36.2237919952136));
#55082=CARTESIAN_POINT('Ctrl Pts',(21.5016121769995,14.3862052235958,36.2731377968842));
#55083=CARTESIAN_POINT('Ctrl Pts',(21.5610846124,14.3819826177933,36.3254563195492));
#55084=CARTESIAN_POINT('Ctrl Pts',(21.6206161855042,14.3777558131513,36.3778268662698));
#55085=CARTESIAN_POINT('Ctrl Pts',(21.6774860644205,14.3735290085093,36.43317572824));
#55086=CARTESIAN_POINT('Ctrl Pts',(21.7313954179226,14.3693022038673,36.4911928805178));
#55087=CARTESIAN_POINT('Ctrl Pts',(21.7853308949528,14.3650733509898,36.549238146891));
#55088=CARTESIAN_POINT('Ctrl Pts',(21.8363026868455,14.3608444981124,36.6099539199054));
#55089=CARTESIAN_POINT('Ctrl Pts',(21.884052199654,14.3566156452349,36.6729969341732));
#55090=CARTESIAN_POINT('Ctrl Pts',(21.9318875288007,14.3523791921821,36.7361532505528));
#55091=CARTESIAN_POINT('Ctrl Pts',(21.9764887431074,14.3481427391293,36.8016447769754));
#55092=CARTESIAN_POINT('Ctrl Pts',(22.0176406832059,14.3439062860765,36.8690993076725));
#55093=CARTESIAN_POINT('Ctrl Pts',(22.0550425475214,14.3400558906425,36.9304068717522));
#55094=CARTESIAN_POINT('Ctrl Pts',(22.0895955930787,14.3362054952084,36.9933354082853));
#55095=CARTESIAN_POINT('Ctrl Pts',(22.1211725264869,14.3323550997743,37.0575905057143));
#55096=CARTESIAN_POINT('Ctrl Pts',(22.1559252560319,14.3281174573968,37.1283079498045));
#55097=CARTESIAN_POINT('Ctrl Pts',(22.1872028951335,14.3238798150193,37.2008979615713));
#55098=CARTESIAN_POINT('Ctrl Pts',(22.214800436797,14.3196421726418,37.2749851722157));
#55099=CARTESIAN_POINT('Ctrl Pts',(22.2423582921125,14.3154106241604,37.3489658425438));
#55100=CARTESIAN_POINT('Ctrl Pts',(22.2662463973767,14.3111790756789,37.4244390003731));
#55101=CARTESIAN_POINT('Ctrl Pts',(22.2863064098537,14.3069475271975,37.501006309581));
#55102=CARTESIAN_POINT('Ctrl Pts',(22.3063432524623,14.3027208662714,37.5774851814321));
#55103=CARTESIAN_POINT('Ctrl Pts',(22.3225606708177,14.2984942053453,37.6550552420493));
#55104=CARTESIAN_POINT('Ctrl Pts',(22.3348495715185,14.2942675444192,37.7333013235912));
#55105=CARTESIAN_POINT('Ctrl Pts',(22.3471307150821,14.2900435514932,37.811498013768));
#55106=CARTESIAN_POINT('Ctrl Pts',(22.3554881905846,14.2858195585672,37.8903694159813));
#55107=CARTESIAN_POINT('Ctrl Pts',(22.3598638705481,14.2815955656412,37.9694896426265));
#55108=CARTESIAN_POINT('Ctrl Pts',(22.3642381508515,14.2773729238547,38.04858456088));
#55109=CARTESIAN_POINT('Ctrl Pts',(22.3646331390006,14.2731502820683,38.1279276777905));
#55110=CARTESIAN_POINT('Ctrl Pts',(22.3610426511955,14.2689276402818,38.2070889356365));
#55111=CARTESIAN_POINT('Ctrl Pts',(22.3574521939874,14.2647050344794,38.2862495188959));
#55112=CARTESIAN_POINT('Ctrl Pts',(22.3498763510219,14.2604824286769,38.3652277779459));
#55113=CARTESIAN_POINT('Ctrl Pts',(22.3383609978002,14.2562598228744,38.4435961071766));
#55114=CARTESIAN_POINT('Ctrl Pts',(22.3268341940376,14.2520330182324,38.5220423636523));
#55115=CARTESIAN_POINT('Ctrl Pts',(22.3113601234275,14.2478062135905,38.5998770139571));
#55116=CARTESIAN_POINT('Ctrl Pts',(22.2920361913906,14.2435794089485,38.6766806206694));
#55117=CARTESIAN_POINT('Ctrl Pts',(22.2727028953148,14.239350556071,38.7535214450639));
#55118=CARTESIAN_POINT('Ctrl Pts',(22.2495161586525,14.2351217031936,38.8293297817057));
#55119=CARTESIAN_POINT('Ctrl Pts',(22.2226231737379,14.2308928503162,38.9037018529674));
#55120=CARTESIAN_POINT('Ctrl Pts',(22.1956818562362,14.2266563972634,38.9782075871389));
#55121=CARTESIAN_POINT('Ctrl Pts',(22.1650211631008,14.2224199442106,39.0512714649937));
#55122=CARTESIAN_POINT('Ctrl Pts',(22.1308362067978,14.2181834911578,39.1225103914873));
#55123=CARTESIAN_POINT('Ctrl Pts',(22.0997664420612,14.2143330957237,39.1872574886205));
#55124=CARTESIAN_POINT('Ctrl Pts',(22.0657861828018,14.2104827002895,39.2504971569346));
#55125=CARTESIAN_POINT('Ctrl Pts',(22.0290731110171,14.2066323048553,39.311962355458));
#55126=CARTESIAN_POINT('Ctrl Pts',(21.9886676847534,14.2023946624778,39.379609311324));
#55127=CARTESIAN_POINT('Ctrl Pts',(21.9447998069588,14.1981570201003,39.4453604315721));
#55128=CARTESIAN_POINT('Ctrl Pts',(21.8976727697612,14.1939193777228,39.5088394159048));
#55129=CARTESIAN_POINT('Ctrl Pts',(21.8506135030923,14.1896878292413,39.5722271149671));
#55130=CARTESIAN_POINT('Ctrl Pts',(21.8003046616916,14.1854562807599,39.6333487936316));
#55131=CARTESIAN_POINT('Ctrl Pts',(21.7469942052441,14.1812247322784,39.6918547948049));
#55132=CARTESIAN_POINT('Ctrl Pts',(21.6937453238462,14.1769980713523,39.7502932199311));
#55133=CARTESIAN_POINT('Ctrl Pts',(21.6375020312322,14.1727714104262,39.8061216266631));
#55134=CARTESIAN_POINT('Ctrl Pts',(21.5785532148333,14.1685447495001,39.859022509475));
#55135=CARTESIAN_POINT('Ctrl Pts',(21.5196416087641,14.1643207565741,39.9118899996011));
#55136=CARTESIAN_POINT('Ctrl Pts',(21.4580282167,14.1600967636481,39.9618333214996));
#55137=CARTESIAN_POINT('Ctrl Pts',(21.3940386610968,14.155872770722,40.0085718881581));
#55138=CARTESIAN_POINT('Ctrl Pts',(21.3300695739986,14.1516501289356,40.0552955044302));
#55139=CARTESIAN_POINT('Ctrl Pts',(21.2637262109849,14.1474274871491,40.098816124839));
#55140=CARTESIAN_POINT('Ctrl Pts',(21.1953659674773,14.1432048453627,40.1388944662972));
#55141=CARTESIAN_POINT('Ctrl Pts',(21.1270063065133,14.1389822395602,40.1789724662208));
#55142=CARTESIAN_POINT('Ctrl Pts',(21.0566302043478,14.1347596337577,40.215608009662));
#55143=CARTESIAN_POINT('Ctrl Pts',(20.9846213371323,14.1305370279552,40.2486068191653));
#55144=CARTESIAN_POINT('Ctrl Pts',(20.9125408663408,14.1263102233132,40.2816384417492));
#55145=CARTESIAN_POINT('Ctrl Pts',(20.8388248145482,14.1220834186712,40.3110259111443));
#55146=CARTESIAN_POINT('Ctrl Pts',(20.7638780554441,14.1178566140293,40.3366226229096));
#55147=CARTESIAN_POINT('Ctrl Pts',(20.6888949784536,14.1136277611518,40.3622317383929));
#55148=CARTESIAN_POINT('Ctrl Pts',(20.6126804573469,14.1093989082743,40.3840463076975));
#55149=CARTESIAN_POINT('Ctrl Pts',(20.5356533301059,14.1051700553969,40.4019700151928));
#55150=CARTESIAN_POINT('Ctrl Pts',(20.4584877682375,14.1009336023441,40.4199259355182));
#55151=CARTESIAN_POINT('Ctrl Pts',(20.3805071445901,14.0966971492913,40.4339769385539));
#55152=CARTESIAN_POINT('Ctrl Pts',(20.3021390318273,14.0924606962386,40.4440781655795));
#55153=CARTESIAN_POINT('Ctrl Pts',(20.2309124137566,14.0886103008044,40.4532588924598));
#55154=CARTESIAN_POINT('Ctrl Pts',(20.1593660432827,14.0847599053703,40.4591775527539));
#55155=CARTESIAN_POINT('Ctrl Pts',(20.0878206510454,14.0809095099361,40.4618378382416));
#55156=CARTESIAN_POINT('Ctrl Pts',(20.0090797032014,14.0766718675586,40.4647656773979));
#55157=CARTESIAN_POINT('Ctrl Pts',(19.9300443750174,14.0724342251811,40.4637570075032));
#55158=CARTESIAN_POINT('Ctrl Pts',(19.8511409917448,14.0681965828037,40.458777530112));
#55159=CARTESIAN_POINT('Ctrl Pts',(19.7723510746336,14.0639650343222,40.4538052134047));
#55160=CARTESIAN_POINT('Ctrl Pts',(19.6936931896012,14.0597334858407,40.4448734583647));
#55161=CARTESIAN_POINT('Ctrl Pts',(19.6155956259171,14.0555019373593,40.4319999395553));
#55162=CARTESIAN_POINT('Ctrl Pts',(19.5375882670758,14.0512752764332,40.4191412900157));
#55163=CARTESIAN_POINT('Ctrl Pts',(19.4601404036507,14.047048615507,40.4023500002143));
#55164=CARTESIAN_POINT('Ctrl Pts',(19.3836756324295,14.0428219545809,40.3816955789147));
#55165=CARTESIAN_POINT('Ctrl Pts',(19.3072591281547,14.0385979616549,40.3610541953295));
#55166=CARTESIAN_POINT('Ctrl Pts',(19.231824935714,14.0343739687289,40.3365546423794));
#55167=CARTESIAN_POINT('Ctrl Pts',(19.1577856783303,14.0301499758029,40.3083173407086));
#55168=CARTESIAN_POINT('Ctrl Pts',(19.0837701040756,14.0259273340164,40.2800890713767));
#55169=CARTESIAN_POINT('Ctrl Pts',(19.0111490164942,14.0217046922299,40.2481255944814));
#55170=CARTESIAN_POINT('Ctrl Pts',(18.9403176854388,14.0174820504435,40.2125964671717));
#55171=CARTESIAN_POINT('Ctrl Pts',(18.8694869579849,14.013259444641,40.1770676426296));
#55172=CARTESIAN_POINT('Ctrl Pts',(18.8004463751051,14.0090368388385,40.1379734395443));
#55173=CARTESIAN_POINT('Ctrl Pts',(18.7335677584216,14.004814233036,40.0955299592817));
#55174=CARTESIAN_POINT('Ctrl Pts',(18.6666226395377,14.000587428394,40.0530442744256));
#55175=CARTESIAN_POINT('Ctrl Pts',(18.6018441777969,13.996360623752,40.0072029116203));
#55176=CARTESIAN_POINT('Ctrl Pts',(18.5395757420476,13.99213381911,39.9582657042749));
#55177=CARTESIAN_POINT('Ctrl Pts',(18.4772771321055,13.9879049662326,39.9093047828163));
#55178=CARTESIAN_POINT('Ctrl Pts',(18.4174913251768,13.9836761133551,39.8572453364943));
#55179=CARTESIAN_POINT('Ctrl Pts',(18.3605271057175,13.9794472604777,39.8023862868964));
#55180=CARTESIAN_POINT('Ctrl Pts',(18.3034605090727,13.9752108074249,39.7474286435647));
#55181=CARTESIAN_POINT('Ctrl Pts',(18.2492259538894,13.9709743543721,39.689661686099));
#55182=CARTESIAN_POINT('Ctrl Pts',(18.1980938136872,13.9667379013193,39.629419673153));
#55183=CARTESIAN_POINT('Ctrl Pts',(18.1516212205255,13.9628875058852,39.574667367699));
#55184=CARTESIAN_POINT('Ctrl Pts',(18.1077110166983,13.9590371104512,39.5178711735712));
#55185=CARTESIAN_POINT('Ctrl Pts',(18.0665346903742,13.9551867150171,39.4593021508751));
#55186=CARTESIAN_POINT('Ctrl Pts',(18.0207442084218,13.9509048502085,39.3941699738172));
#55187=CARTESIAN_POINT('Ctrl Pts',(17.9781648846182,13.9466229853999,39.326602749622));
#55188=CARTESIAN_POINT('Ctrl Pts',(17.9390618242376,13.9423411205913,39.2569460992567));
#55189=CARTESIAN_POINT('Ctrl Pts',(17.9000177586572,13.9380657158335,39.1873945399028));
#55190=CARTESIAN_POINT('Ctrl Pts',(17.864439760251,13.9337903110758,39.1157602097527));
#55191=CARTESIAN_POINT('Ctrl Pts',(17.8325504845345,13.929514906318,39.0424187173484));
#55192=CARTESIAN_POINT('Ctrl Pts',(17.8003919474075,13.9252034016022,38.968457956138));
#55193=CARTESIAN_POINT('Ctrl Pts',(17.7719850048456,13.9208918968864,38.8927614434773));
#55194=CARTESIAN_POINT('Ctrl Pts',(17.7475113669798,13.9165803921706,38.8157411536406));
#55195=CARTESIAN_POINT('Ctrl Pts',(17.7232972902773,13.9123146141745,38.7395377213607));
#55196=CARTESIAN_POINT('Ctrl Pts',(17.7029336313327,13.9080488361785,38.662038900109));
#55197=CARTESIAN_POINT('Ctrl Pts',(17.6865480274974,13.9037830581824,38.5836635316247));
#55198=CARTESIAN_POINT('Ctrl Pts',(17.6698989570979,13.8994486901067,38.5040279539194));
#55199=CARTESIAN_POINT('Ctrl Pts',(17.6573571699985,13.895114322031,38.4234878417123));
#55200=CARTESIAN_POINT('Ctrl Pts',(17.6490032228322,13.8907799539554,38.3424965868764));
#55201=CARTESIAN_POINT('Ctrl Pts',(17.6406492756659,13.8864455858797,38.2615053320404));
#55202=CARTESIAN_POINT('Ctrl Pts',(17.6364832337555,13.882111217804,38.1800634256563));
#55203=CARTESIAN_POINT('Ctrl Pts',(17.6365303963904,13.8777768497283,38.0986311634849));
#55204=CARTESIAN_POINT('',(17.6331851034168,13.0840268497283,38.0990226178629));
#55205=CARTESIAN_POINT('Ctrl Pts',(17.6395267864659,13.8777759447365,38.0986159178374));
#55206=CARTESIAN_POINT('Ctrl Pts',(17.637928747162,13.8616719365237,37.7964432487494));
#55207=CARTESIAN_POINT('Ctrl Pts',(17.8318962804384,13.8036603300046,36.7099019745982));
#55208=CARTESIAN_POINT('Ctrl Pts',(19.4641824064282,13.7037411251789,35.3606306468454));
#55209=CARTESIAN_POINT('Ctrl Pts',(22.0063036074145,13.5780183302599,36.1593839170346));
#55210=CARTESIAN_POINT('Ctrl Pts',(22.7200222714505,13.4522955353407,38.7266767822465));
#55211=CARTESIAN_POINT('Ctrl Pts',(20.9549059260135,13.3265727404216,40.7228609606787));
#55212=CARTESIAN_POINT('Ctrl Pts',(18.3817401264292,13.2038165118843,40.3380553789342));
#55213=CARTESIAN_POINT('Ctrl Pts',(17.6369894458825,13.1229678816531,38.8246886382043));
#55214=CARTESIAN_POINT('Ctrl Pts',(17.6331851034168,13.0840268497283,38.0990226178629));
#55215=CARTESIAN_POINT('',(17.6367489926442,12.2902768497283,38.1021344623069));
#55216=CARTESIAN_POINT('Ctrl Pts',(17.6331851034168,13.0840268497283,38.0990226178629));
#55217=CARTESIAN_POINT('Ctrl Pts',(17.6328952848397,13.0810602833467,38.0437406616896));
#55218=CARTESIAN_POINT('Ctrl Pts',(17.6596679510084,13.0361861186589,37.2077962582566));
#55219=CARTESIAN_POINT('Ctrl Pts',(18.6491954913026,12.9494043556642,35.657343223885));
#55220=CARTESIAN_POINT('Ctrl Pts',(21.3137747086376,12.8236815607454,35.6372290074956));
#55221=CARTESIAN_POINT('Ctrl Pts',(22.7810730152558,12.6979587658264,37.8615092655836));
#55222=CARTESIAN_POINT('Ctrl Pts',(21.713899002855,12.5722359709072,40.3031330315278));
#55223=CARTESIAN_POINT('Ctrl Pts',(19.0847992314011,12.4465131759882,40.7369779103628));
#55224=CARTESIAN_POINT('Ctrl Pts',(17.742876170108,12.3525268022618,39.2647846658353));
#55225=CARTESIAN_POINT('Ctrl Pts',(17.6350286938508,12.3004480268419,38.2924174207486));
#55226=CARTESIAN_POINT('Ctrl Pts',(17.6367489926442,12.2902768497283,38.1021344623069));
#55227=CARTESIAN_POINT('',(17.640153963339,11.4965268497283,38.0992943844365));
#55228=CARTESIAN_POINT('Ctrl Pts',(17.6367489926442,12.2902768497283,38.1021344623069));
#55229=CARTESIAN_POINT('Ctrl Pts',(17.6421167221093,12.2585404285355,37.5084076942567));
#55230=CARTESIAN_POINT('Ctrl Pts',(18.1692910103586,12.1848964090363,36.1221756123481));
#55231=CARTESIAN_POINT('Ctrl Pts',(20.4944013127005,12.0693447912309,35.3528537919161));
#55232=CARTESIAN_POINT('Ctrl Pts',(22.5736121140596,11.9436219963119,37.0193679474702));
#55233=CARTESIAN_POINT('Ctrl Pts',(22.307415719276,11.8178992013927,39.6706933644183));
#55234=CARTESIAN_POINT('Ctrl Pts',(19.9384046062531,11.6921764064736,40.8906004647851));
#55235=CARTESIAN_POINT('Ctrl Pts',(17.9676804027266,11.5850522892521,39.7631059729174));
#55236=CARTESIAN_POINT('Ctrl Pts',(17.641330657499,11.5198357703371,38.5369497808051));
#55237=CARTESIAN_POINT('Ctrl Pts',(17.640153963339,11.4965268497283,38.0992943844365));
#55238=CARTESIAN_POINT('',(17.6341963774677,10.7027768497283,38.0983734632106));
#55239=CARTESIAN_POINT('Ctrl Pts',(17.640153963339,11.4965268497283,38.0992943844365));
#55240=CARTESIAN_POINT('Ctrl Pts',(17.6392150543351,11.4779281720307,37.7500799443385));
#55241=CARTESIAN_POINT('Ctrl Pts',(17.8753171992425,11.4174218960267,36.615203052934));
#55242=CARTESIAN_POINT('Ctrl Pts',(19.6272936397288,11.3150080217165,35.3337145997561));
#55243=CARTESIAN_POINT('Ctrl Pts',(22.1176698466579,11.1892852267973,36.2815612830932));
#55244=CARTESIAN_POINT('Ctrl Pts',(22.6781522400348,11.0635624318782,38.8866037921257));
#55245=CARTESIAN_POINT('Ctrl Pts',(20.797956995228,10.9378396369591,40.7747915022213));
#55246=CARTESIAN_POINT('Ctrl Pts',(18.3038161317269,10.8175777762425,40.2492294011243));
#55247=CARTESIAN_POINT('Ctrl Pts',(17.6395514888341,10.7392235138322,38.7783215464619));
#55248=CARTESIAN_POINT('Ctrl Pts',(17.6341963774677,10.7027768497283,38.0983734632106));
#55249=CARTESIAN_POINT('',(17.6353503215415,9.9090268497283,38.1019939141643));
#55250=CARTESIAN_POINT('Ctrl Pts',(17.6341963774677,10.7027768497283,38.0983734632106));
#55251=CARTESIAN_POINT('Ctrl Pts',(17.6333940019544,10.6973159155259,37.9964944069241));
#55252=CARTESIAN_POINT('Ctrl Pts',(17.6855609843329,10.6499473830165,37.1136154527935));
#55253=CARTESIAN_POINT('Ctrl Pts',(18.7961706379081,10.5606712522025,35.581659313446));
#55254=CARTESIAN_POINT('Ctrl Pts',(21.4572672824637,10.4349484572826,35.7193242526437));
#55255=CARTESIAN_POINT('Ctrl Pts',(22.7903140813097,10.3092256623639,38.0265678937093));
#55256=CARTESIAN_POINT('Ctrl Pts',(21.5804669102173,10.1835028674447,40.400732338256));
#55257=CARTESIAN_POINT('Ctrl Pts',(18.9302945074246,10.0577800725256,40.6781728230947));
#55258=CARTESIAN_POINT('Ctrl Pts',(17.711117980681,9.96628806662015,39.1702307552347));
#55259=CARTESIAN_POINT('Ctrl Pts',(17.6340610761295,9.91670365902104,38.2453939776618));
#55260=CARTESIAN_POINT('Ctrl Pts',(17.6353503215415,9.9090268497283,38.1019939141643));
#55261=CARTESIAN_POINT('',(17.6403527334675,9.11527684972829,38.100042490769));
#55262=CARTESIAN_POINT('Ctrl Pts',(17.6353503215415,9.9090268497283,38.1019939141643));
#55263=CARTESIAN_POINT('Ctrl Pts',(17.6410990494308,9.87479606071468,37.4625749666653));
#55264=CARTESIAN_POINT('Ctrl Pts',(18.238503270141,9.79865767339471,36.0308725437426));
#55265=CARTESIAN_POINT('Ctrl Pts',(20.6561660623633,9.68061168776838,35.3869406484207));
#55266=CARTESIAN_POINT('Ctrl Pts',(22.6330720558258,9.55488889284928,37.1736218399495));
#55267=CARTESIAN_POINT('Ctrl Pts',(22.2103832875294,9.42916609793023,39.8045382567722));
#55268=CARTESIAN_POINT('Ctrl Pts',(19.7733082640224,9.30344330301114,40.8820596333343));
#55269=CARTESIAN_POINT('Ctrl Pts',(17.9170417702093,9.1988135536105,39.6687992359617));
#55270=CARTESIAN_POINT('Ctrl Pts',(17.6402897602495,9.13609140251621,38.4909451107544));
#55271=CARTESIAN_POINT('Ctrl Pts',(17.6403527334675,9.11527684972829,38.100042490769));
#55272=CARTESIAN_POINT('',(17.6355044646775,8.3215268497283,38.0979757353713));
#55273=CARTESIAN_POINT('Ctrl Pts',(17.6403527334675,9.11527684972829,38.100042490769));
#55274=CARTESIAN_POINT('Ctrl Pts',(17.640416549249,9.09418380420986,37.7039097061427));
#55275=CARTESIAN_POINT('Ctrl Pts',(17.9225004294726,9.03118316038505,36.5206561174594));
#55276=CARTESIAN_POINT('Ctrl Pts',(19.7917122341746,8.9262749182539,35.316501993319));
#55277=CARTESIAN_POINT('Ctrl Pts',(22.2216078271693,8.80055212333482,36.4101172795579));
#55278=CARTESIAN_POINT('Ctrl Pts',(22.6268879171577,8.67482932841574,39.0437715916894));
#55279=CARTESIAN_POINT('Ctrl Pts',(20.6382090299156,8.54910653349668,40.8173395409341));
#55280=CARTESIAN_POINT('Ctrl Pts',(18.2305512719002,8.43133904060083,40.1589894803223));
#55281=CARTESIAN_POINT('Ctrl Pts',(17.641248927774,8.35547914601139,38.7322993073621));
#55282=CARTESIAN_POINT('Ctrl Pts',(17.6355044646775,8.3215268497283,38.0979757353713));
#55283=CARTESIAN_POINT('',(17.6340647533427,7.52777684972829,38.1015653822901));
#55284=CARTESIAN_POINT('Ctrl Pts',(17.6355044646775,8.3215268497283,38.0979757353713));
#55285=CARTESIAN_POINT('Ctrl Pts',(17.6341584897687,8.31357154770503,37.9493485098786));
#55286=CARTESIAN_POINT('Ctrl Pts',(17.7145046251406,8.26370864737542,37.0192206278211));
#55287=CARTESIAN_POINT('Ctrl Pts',(18.9473685182804,8.17193814873941,35.5148091153107));
#55288=CARTESIAN_POINT('Ctrl Pts',(21.5956481253796,8.04621535382035,35.8097703157627));
#55289=CARTESIAN_POINT('Ctrl Pts',(22.789767420079,7.92049255890126,38.1918841033843));
#55290=CARTESIAN_POINT('Ctrl Pts',(21.4414909330391,7.79476976398219,40.4902612485993));
#55291=CARTESIAN_POINT('Ctrl Pts',(18.7795420440647,7.6690469690631,40.6103241472732));
#55292=CARTESIAN_POINT('Ctrl Pts',(17.6825210085457,7.58004933097848,39.07585822244));
#55293=CARTESIAN_POINT('Ctrl Pts',(17.6333245476966,7.53295929120021,38.1982348102183));
#55294=CARTESIAN_POINT('Ctrl Pts',(17.6340647533427,7.52777684972829,38.1015653822901));
#55295=CARTESIAN_POINT('',(17.6367873258724,6.73402689228867,38.100787309117));
#55296=CARTESIAN_POINT('Ctrl Pts',(17.6340647533427,7.52777684972829,38.1015653822901));
#55297=CARTESIAN_POINT('Ctrl Pts',(17.6393101899942,7.49105169289384,37.4165214853157));
#55298=CARTESIAN_POINT('Ctrl Pts',(18.3122833940378,7.41241893775303,35.9407788034475));
#55299=CARTESIAN_POINT('Ctrl Pts',(20.8156291448001,7.29187858430588,35.4305442418459));
#55300=CARTESIAN_POINT('Ctrl Pts',(22.6832958361958,7.16615578938679,37.3311252364372));
#55301=CARTESIAN_POINT('Ctrl Pts',(22.1055973813781,7.04043299446771,39.9324040531833));
#55302=CARTESIAN_POINT('Ctrl Pts',(19.6090070999777,6.91471019954863,40.863760029149));
#55303=CARTESIAN_POINT('Ctrl Pts',(17.8702883666026,6.81257501512464,39.5742316475738));
#55304=CARTESIAN_POINT('Ctrl Pts',(17.6390752763342,6.75234742900701,38.4447601330821));
#55305=CARTESIAN_POINT('Ctrl Pts',(17.6401044046334,6.73402744119574,38.1007965110423));
#55306=CARTESIAN_POINT('',(17.6365309617442,5.94027684968202,38.0978678400331));
#55307=CARTESIAN_POINT('Ctrl Pts',(17.636530130895,6.73402684972829,38.1007865956311));
#55308=CARTESIAN_POINT('Ctrl Pts',(17.6365030726185,6.72970315999644,38.0194850745859));
#55309=CARTESIAN_POINT('Ctrl Pts',(17.6406754204681,6.7253794702646,37.9382157103641));
#55310=CARTESIAN_POINT('Ctrl Pts',(17.6490110348502,6.72105578053275,37.8574276878044));
#55311=CARTESIAN_POINT('Ctrl Pts',(17.6573525203997,6.71672904542176,37.7765827624198));
#55312=CARTESIAN_POINT('Ctrl Pts',(17.6698630616553,6.71240231031076,37.6962202870288));
#55313=CARTESIAN_POINT('Ctrl Pts',(17.6864549718565,6.70807557519977,37.6167817846434));
#55314=CARTESIAN_POINT('Ctrl Pts',(17.7030761246116,6.70374121439748,37.5372032751902));
#55315=CARTESIAN_POINT('Ctrl Pts',(17.7237929189623,6.69940685359519,37.4585524180726));
#55316=CARTESIAN_POINT('Ctrl Pts',(17.7484670911131,6.6950724927929,37.3812580427585));
#55317=CARTESIAN_POINT('Ctrl Pts',(17.7731654827171,6.6907338775075,37.3038877975228));
#55318=CARTESIAN_POINT('Ctrl Pts',(17.8018288365831,6.6863952622221,37.2278770944096));
#55319=CARTESIAN_POINT('Ctrl Pts',(17.8342706913796,6.6820566469367,37.1536348470687));
#55320=CARTESIAN_POINT('Ctrl Pts',(17.86677938582,6.67770909284362,37.0792396391339));
#55321=CARTESIAN_POINT('Ctrl Pts',(17.9030819344239,6.67336153875053,37.0066205541054));
#55322=CARTESIAN_POINT('Ctrl Pts',(17.9429459095411,6.66901398465745,36.9361619915872));
#55323=CARTESIAN_POINT('Ctrl Pts',(17.9605184675755,6.66709752634179,36.905102942026));
#55324=CARTESIAN_POINT('Ctrl Pts',(17.9787825054123,6.66518106802613,36.8744633307563));
#55325=CARTESIAN_POINT('Ctrl Pts',(17.9977155506846,6.66326460971047,36.8442741441979));
#55326=CARTESIAN_POINT('Ctrl Pts',(18.0395800015446,6.65902696733297,36.7775202913974));
#55327=CARTESIAN_POINT('Ctrl Pts',(18.0848649312771,6.65478932495548,36.712736993741));
#55328=CARTESIAN_POINT('Ctrl Pts',(18.1333589265657,6.65055168257798,36.6502960495784));
#55329=CARTESIAN_POINT('Ctrl Pts',(18.1817831855859,6.64632013409652,36.5879448979439));
#55330=CARTESIAN_POINT('Ctrl Pts',(18.2334070605116,6.64208858561506,36.5279297776531));
#55331=CARTESIAN_POINT('Ctrl Pts',(18.2879750593924,6.6378570371336,36.4705948804433));
#55332=CARTESIAN_POINT('Ctrl Pts',(18.3424800307276,6.6336303762075,36.4133262066231));
#55333=CARTESIAN_POINT('Ctrl Pts',(18.3999220467381,6.6294037152814,36.3587319417326));
#55334=CARTESIAN_POINT('Ctrl Pts',(18.4600053953514,6.62517705435529,36.3071232450184));
#55335=CARTESIAN_POINT('Ctrl Pts',(18.5200508174828,6.62095306142927,36.2555471253219));
#55336=CARTESIAN_POINT('Ctrl Pts',(18.5827339081565,6.61672906850325,36.2069531377565));
#55337=CARTESIAN_POINT('Ctrl Pts',(18.6477230303954,6.61250507557723,36.1616147342757));
#55338=CARTESIAN_POINT('Ctrl Pts',(18.7126913643955,6.60828243379077,36.1162908333075));
#55339=CARTESIAN_POINT('Ctrl Pts',(18.7799638809766,6.60405979200431,36.0742207164835));
#55340=CARTESIAN_POINT('Ctrl Pts',(18.8491780743503,6.59983715021784,36.0356358518072));
#55341=CARTESIAN_POINT('Ctrl Pts',(18.9183916779033,6.59561454441536,35.9970513159385));
#55342=CARTESIAN_POINT('Ctrl Pts',(18.9895465152061,6.59139193861287,35.9619522001709));
#55343=CARTESIAN_POINT('Ctrl Pts',(19.0622547829605,6.58716933281038,35.9305244069547));
#55344=CARTESIAN_POINT('Ctrl Pts',(19.1350353497551,6.5829425281684,35.8990653628318));
#55345=CARTESIAN_POINT('Ctrl Pts',(19.2093720012243,6.57871572352641,35.8712851198941));
#55346=CARTESIAN_POINT('Ctrl Pts',(19.2848567764607,6.57448891888443,35.8473214586351));
#55347=CARTESIAN_POINT('Ctrl Pts',(19.3603781302965,6.57026006600698,35.8233461850058));
#55348=CARTESIAN_POINT('Ctrl Pts',(19.4370482622848,6.56603121312953,35.8031912967065));
#55349=CARTESIAN_POINT('Ctrl Pts',(19.5144463422357,6.56180236025208,35.7869439941213));
#55350=CARTESIAN_POINT('Ctrl Pts',(19.5919835234973,6.5575659071993,35.7706674915729));
#55351=CARTESIAN_POINT('Ctrl Pts',(19.6702508026572,6.55332945414652,35.758312680216));
#55352=CARTESIAN_POINT('Ctrl Pts',(19.7488197339795,6.54909300109374,35.7499151260302));
#55353=CARTESIAN_POINT('Ctrl Pts',(19.8202288705043,6.54524260565962,35.7422828204453));
#55354=CARTESIAN_POINT('Ctrl Pts',(19.8918868679174,6.54139221022551,35.737918754183));
#55355=CARTESIAN_POINT('Ctrl Pts',(19.9634731513095,6.53754181479139,35.7368122735964));
#55356=CARTESIAN_POINT('Ctrl Pts',(20.042259102867,6.5333041724139,35.7355945106149));
#55357=CARTESIAN_POINT('Ctrl Pts',(20.1212539077664,6.5290665300364,35.7383187196748));
#55358=CARTESIAN_POINT('Ctrl Pts',(20.2000305966432,6.52482888765891,35.7450099360493));
#55359=CARTESIAN_POINT('Ctrl Pts',(20.27869400155,6.52059733917745,35.751691530192));
#55360=CARTESIAN_POINT('Ctrl Pts',(20.3571394501003,6.51636579069598,35.7623287632727));
#55361=CARTESIAN_POINT('Ctrl Pts',(20.4349391376553,6.51213424221452,35.7768946671673));
#55362=CARTESIAN_POINT('Ctrl Pts',(20.5126489644227,6.50790758128842,35.7914437470407));
#55363=CARTESIAN_POINT('Ctrl Pts',(20.5897140539943,6.50368092036231,35.8099123943005));
#55364=CARTESIAN_POINT('Ctrl Pts',(20.6657124183755,6.49945425943621,35.8322219207073));
#55365=CARTESIAN_POINT('Ctrl Pts',(20.7416628102208,6.4952302665102,35.8545173646458));
#55366=CARTESIAN_POINT('Ctrl Pts',(20.8165473647843,6.49100627358418,35.8806487437084));
#55367=CARTESIAN_POINT('Ctrl Pts',(20.8899561702956,6.48678228065817,35.9104867079982));
#55368=CARTESIAN_POINT('Ctrl Pts',(20.9633414943422,6.48255963887172,35.9403151279411));
#55369=CARTESIAN_POINT('Ctrl Pts',(21.0352515727803,6.47833699708526,35.9738476022866));
#55370=CARTESIAN_POINT('Ctrl Pts',(21.1052949098236,6.47411435529881,36.0109060329372));
#55371=CARTESIAN_POINT('Ctrl Pts',(21.1753376499804,6.46989174949633,36.047964147788));
#55372=CARTESIAN_POINT('Ctrl Pts',(21.2435132666876,6.46566914369385,36.0885479387124));
#55373=CARTESIAN_POINT('Ctrl Pts',(21.3094547172913,6.46144653789137,36.1324332834022));
#55374=CARTESIAN_POINT('Ctrl Pts',(21.3754617382042,6.45721973324939,36.1763622664347));
#55375=CARTESIAN_POINT('Ctrl Pts',(21.4392297642179,6.45299292860741,36.2235991006603));
#55376=CARTESIAN_POINT('Ctrl Pts',(21.5004211481249,6.44876612396542,36.2738765597147));
#55377=CARTESIAN_POINT('Ctrl Pts',(21.5616421843044,6.44453727108797,36.3241783823448));
#55378=CARTESIAN_POINT('Ctrl Pts',(21.6202837438227,6.44030841821051,36.3775234492089));
#55379=CARTESIAN_POINT('Ctrl Pts',(21.6760436042791,6.43607956533306,36.433606205768));
#55380=CARTESIAN_POINT('Ctrl Pts',(21.731903677424,6.43184311228028,36.4897897553305));
#55381=CARTESIAN_POINT('Ctrl Pts',(21.7848713891656,6.4276066592275,36.5487204762121));
#55382=CARTESIAN_POINT('Ctrl Pts',(21.8346836861194,6.42337020617472,36.6100583189979));
#55383=CARTESIAN_POINT('Ctrl Pts',(21.8799567101245,6.41951981074058,36.6658065939959));
#55384=CARTESIAN_POINT('Ctrl Pts',(21.9226235779161,6.41566941530645,36.7235426491132));
#55385=CARTESIAN_POINT('Ctrl Pts',(21.9625187261799,6.41181901987231,36.7829917652903));
#55386=CARTESIAN_POINT('Ctrl Pts',(22.0064262608295,6.40758137749482,36.8484198747731));
#55387=CARTESIAN_POINT('Ctrl Pts',(22.047140689196,6.40334373511733,36.9161689399982));
#55388=CARTESIAN_POINT('Ctrl Pts',(22.0844085954045,6.39910609273984,36.9858944177935));
#55389=CARTESIAN_POINT('Ctrl Pts',(22.1216229089014,6.39487454425839,37.0555196276154));
#55390=CARTESIAN_POINT('Ctrl Pts',(22.1554003237148,6.39064299577694,37.1271151957349));
#55391=CARTESIAN_POINT('Ctrl Pts',(22.185530593265,6.38641144729549,37.2003075709984));
#55392=CARTESIAN_POINT('Ctrl Pts',(22.2156260615218,6.38218478636939,37.2734154070474));
#55393=CARTESIAN_POINT('Ctrl Pts',(22.2420825783761,6.37795812544329,37.3481159537538));
#55394=CARTESIAN_POINT('Ctrl Pts',(22.2647364497823,6.37373146451718,37.4240123862617));
#55395=CARTESIAN_POINT('Ctrl Pts',(22.2873760213589,6.36950747159117,37.4998609105762));
#55396=CARTESIAN_POINT('Ctrl Pts',(22.3062175781883,6.36528347866516,37.5769033743228));
#55397=CARTESIAN_POINT('Ctrl Pts',(22.3211464981653,6.36105948573914,37.6547255060584));
#55398=CARTESIAN_POINT('Ctrl Pts',(22.33607064279,6.35683684395268,37.7325227446273));
#55399=CARTESIAN_POINT('Ctrl Pts',(22.3470845476314,6.35261420216622,37.8110986958902));
#55400=CARTESIAN_POINT('Ctrl Pts',(22.3541245083443,6.34839156037976,37.8900280015987));
#55401=CARTESIAN_POINT('Ctrl Pts',(22.361164409065,6.34416895457728,37.9689566346973));
#55402=CARTESIAN_POINT('Ctrl Pts',(22.3642303927682,6.3399463487748,38.0482381492084));
#55403=CARTESIAN_POINT('Ctrl Pts',(22.3633106740363,6.33572374297231,38.1274426472103));
#55404=CARTESIAN_POINT('Ctrl Pts',(22.3623900407622,6.33149693833033,38.2067259039196));
#55405=CARTESIAN_POINT('Ctrl Pts',(22.3574757938599,6.32727013368835,38.2859315213133));
#55406=CARTESIAN_POINT('Ctrl Pts',(22.3486083074933,6.32304332904637,38.3646307972881));
#55407=CARTESIAN_POINT('Ctrl Pts',(22.3397365240982,6.31881447616892,38.443368209553));
#55408=CARTESIAN_POINT('Ctrl Pts',(22.3269077609558,6.31458562329147,38.5215983284183));
#55409=CARTESIAN_POINT('Ctrl Pts',(22.3102138274744,6.31035677041402,38.5989013051158));
#55410=CARTESIAN_POINT('Ctrl Pts',(22.2934898913362,6.30612031736125,38.6763432122026));
#55411=CARTESIAN_POINT('Ctrl Pts',(22.2728870271406,6.30188386430847,38.7528541940136));
#55412=CARTESIAN_POINT('Ctrl Pts',(22.2485473020164,6.29764741125569,38.8280284826122));
#55413=CARTESIAN_POINT('Ctrl Pts',(22.2264255965899,6.29379701582154,38.8963523219136));
#55414=CARTESIAN_POINT('Ctrl Pts',(22.2012177834238,6.28994662038738,38.9635719605848));
#55415=CARTESIAN_POINT('Ctrl Pts',(22.1730641934383,6.28609622495323,39.0293989735827));
#55416=CARTESIAN_POINT('Ctrl Pts',(22.1420791042334,6.28185858257573,39.1018464259636));
#55417=CARTESIAN_POINT('Ctrl Pts',(22.1074089192801,6.27762094019822,39.1728786636548));
#55418=CARTESIAN_POINT('Ctrl Pts',(22.0692047214133,6.27338329782073,39.2420955572021));
#55419=CARTESIAN_POINT('Ctrl Pts',(22.0310554626825,6.26915174933927,39.31121291414));
#55420=CARTESIAN_POINT('Ctrl Pts',(21.9893825081704,6.26492020085782,39.3785197041992));
#55421=CARTESIAN_POINT('Ctrl Pts',(21.9443847731485,6.26068865237637,39.443636221173));
#55422=CARTESIAN_POINT('Ctrl Pts',(21.8994390117532,6.25646199145027,39.5086775267716));
#55423=CARTESIAN_POINT('Ctrl Pts',(21.8511763664676,6.25223533052416,39.5715332029856));
#55424=CARTESIAN_POINT('Ctrl Pts',(21.7998406163161,6.24800866959806,39.6318499263175));
#55425=CARTESIAN_POINT('Ctrl Pts',(21.7485372708899,6.24378467667204,39.692128575854));
#55426=CARTESIAN_POINT('Ctrl Pts',(21.6941649739992,6.23956068374603,39.7498710975752));
#55427=CARTESIAN_POINT('Ctrl Pts',(21.6370088516455,6.23533669082002,39.8047558360464));
#55428=CARTESIAN_POINT('Ctrl Pts',(21.5798710119687,6.23111404903355,39.8596230183942));
#55429=CARTESIAN_POINT('Ctrl Pts',(21.5199514530048,6.22689140724709,39.9116339083146));
#55430=CARTESIAN_POINT('Ctrl Pts',(21.4575723174632,6.22266876546063,39.9605035286892));
#55431=CARTESIAN_POINT('Ctrl Pts',(21.3951937134964,6.21844615965815,40.0093727326128));
#55432=CARTESIAN_POINT('Ctrl Pts',(21.3303559445216,6.21422355385566,40.0551004322445));
#55433=CARTESIAN_POINT('Ctrl Pts',(21.2634132227497,6.21000094805318,40.097442732466));
#55434=CARTESIAN_POINT('Ctrl Pts',(21.196403935033,6.2057741434112,40.1398271366706));
#55435=CARTESIAN_POINT('Ctrl Pts',(21.127285910628,6.20154733876921,40.1788191660058));
#55436=CARTESIAN_POINT('Ctrl Pts',(21.0564407509257,6.19732053412722,40.2142193312624));
#55437=CARTESIAN_POINT('Ctrl Pts',(20.9855612609005,6.19309168124977,40.2496366508187));
#55438=CARTESIAN_POINT('Ctrl Pts',(20.9129533981948,6.18886282837232,40.2814584504973));
#55439=CARTESIAN_POINT('Ctrl Pts',(20.8390193354553,6.18463397549487,40.3095332076328));
#55440=CARTESIAN_POINT('Ctrl Pts',(20.7649523970032,6.18039752244209,40.3376584212592));
#55441=CARTESIAN_POINT('Ctrl Pts',(20.6895549432289,6.17616106938931,40.3620229921586));
#55442=CARTESIAN_POINT('Ctrl Pts',(20.6132446918886,6.17192461633653,40.3825252219352));
#55443=CARTESIAN_POINT('Ctrl Pts',(20.543888407356,6.16807422090241,40.4011591335915));
#55444=CARTESIAN_POINT('Ctrl Pts',(20.4737785228483,6.16422382546828,40.4166031538563));
#55445=CARTESIAN_POINT('Ctrl Pts',(20.4032333758916,6.16037343003415,40.4288180017913));
#55446=CARTESIAN_POINT('Ctrl Pts',(20.3255932712882,6.15613578765666,40.4422613371914));
#55447=CARTESIAN_POINT('Ctrl Pts',(20.2471344158678,6.15189814527916,40.4518430135706));
#55448=CARTESIAN_POINT('Ctrl Pts',(20.1682747050158,6.14766050290166,40.4574719647436));
#55449=CARTESIAN_POINT('Ctrl Pts',(20.089528397523,6.14342895442022,40.4630928212639));
#55450=CARTESIAN_POINT('Ctrl Pts',(20.0103828430872,6.13919740593877,40.4647722077209));
#55451=CARTESIAN_POINT('Ctrl Pts',(19.931264841588,6.13496585745733,40.4624703001092));
#55452=CARTESIAN_POINT('Ctrl Pts',(19.8522382235653,6.13073919653123,40.4601710512644));
#55453=CARTESIAN_POINT('Ctrl Pts',(19.7732395614395,6.12651253560512,40.4538996603001));
#55454=CARTESIAN_POINT('Ctrl Pts',(19.6946979444256,6.12228587467902,40.4436682990052));
#55455=CARTESIAN_POINT('Ctrl Pts',(19.6162059053278,6.118061881753,40.4334433960644));
#55456=CARTESIAN_POINT('Ctrl Pts',(19.5381708023289,6.11383788882699,40.419263544731));
#55457=CARTESIAN_POINT('Ctrl Pts',(19.4610176659607,6.10961389590098,40.4011928394842));
#55458=CARTESIAN_POINT('Ctrl Pts',(19.3838892087661,6.10539125411452,40.3831279145608));
#55459=CARTESIAN_POINT('Ctrl Pts',(19.3076426140659,6.10116861232806,40.3611747140345));
#55460=CARTESIAN_POINT('Ctrl Pts',(19.2326922936507,6.09694597054161,40.335448349812));
#55461=CARTESIAN_POINT('Ctrl Pts',(19.1577426119376,6.09272336473912,40.3097222048211));
#55462=CARTESIAN_POINT('Ctrl Pts',(19.0840896254625,6.08850075893664,40.2802231136058));
#55463=CARTESIAN_POINT('Ctrl Pts',(19.0121307402265,6.08427815313415,40.2471154525304));
#55464=CARTESIAN_POINT('Ctrl Pts',(18.9401003011151,6.08005134849217,40.2139748701354));
#55465=CARTESIAN_POINT('Ctrl Pts',(18.8697677550231,6.07582454385019,40.1772187467062));
#55466=CARTESIAN_POINT('Ctrl Pts',(18.8015081661781,6.07159773920821,40.1370586062169));
#55467=CARTESIAN_POINT('Ctrl Pts',(18.7332154999324,6.06736888633076,40.0968790048271));
#55468=CARTESIAN_POINT('Ctrl Pts',(18.6669981841135,6.06314003345332,40.0532923583951));
#55469=CARTESIAN_POINT('Ctrl Pts',(18.6032022430351,6.05891118057588,40.0065535573484));
#55470=CARTESIAN_POINT('Ctrl Pts',(18.5392916466703,6.0546747275231,39.9597307564339));
#55471=CARTESIAN_POINT('Ctrl Pts',(18.4778114848346,6.05043827447032,39.9097447778856));
#55472=CARTESIAN_POINT('Ctrl Pts',(18.4190744476327,6.04620182141754,39.8568906735401));
#55473=CARTESIAN_POINT('Ctrl Pts',(18.3656899731583,6.04235142598338,39.8088530346207));
#55474=CARTESIAN_POINT('Ctrl Pts',(18.3145711839386,6.03850103054923,39.7584468538845));
#55475=CARTESIAN_POINT('Ctrl Pts',(18.2659243139061,6.03465063511508,39.7059177923536));
#55476=CARTESIAN_POINT('Ctrl Pts',(18.2130172211904,6.03046304343466,39.6487885273707));
#55477=CARTESIAN_POINT('Ctrl Pts',(18.1628255204444,6.02627545175425,39.5889219903604));
#55478=CARTESIAN_POINT('Ctrl Pts',(18.1156500699753,6.02208786007384,39.5266098913564));
#55479=CARTESIAN_POINT('Ctrl Pts',(18.0685365912465,6.01790576939746,39.4643796482579));
#55480=CARTESIAN_POINT('Ctrl Pts',(18.0244317920978,6.01372367872109,39.3997105934865));
#55481=CARTESIAN_POINT('Ctrl Pts',(17.9835989233411,6.00954158804471,39.3329303057954));
#55482=CARTESIAN_POINT('Ctrl Pts',(17.9428062547143,6.00536361465408,39.2662157635766));
#55483=CARTESIAN_POINT('Ctrl Pts',(17.9052793751211,6.00118564126344,39.1973945197397));
#55484=CARTESIAN_POINT('Ctrl Pts',(17.8712395298754,5.99700766787281,39.1268248641979));
#55485=CARTESIAN_POINT('Ctrl Pts',(17.8372219986205,5.99283243325079,39.0563014688735));
#55486=CARTESIAN_POINT('Ctrl Pts',(17.8066871724102,5.98865719862876,38.9840323687656));
#55487=CARTESIAN_POINT('Ctrl Pts',(17.7798106199974,5.98448196400674,38.9104008624277));
#55488=CARTESIAN_POINT('Ctrl Pts',(17.7529350517411,5.98030688227206,38.8367720523035));
#55489=CARTESIAN_POINT('Ctrl Pts',(17.7297176706244,5.97613180053737,38.7617813810599));
#55490=CARTESIAN_POINT('Ctrl Pts',(17.7102855957909,5.97195671880268,38.6858313648631));
#55491=CARTESIAN_POINT('Ctrl Pts',(17.690854232713,5.96778178999237,38.609884130554));
#55492=CARTESIAN_POINT('Ctrl Pts',(17.6752080112612,5.96360686118205,38.5329780891183));
#55493=CARTESIAN_POINT('Ctrl Pts',(17.6634234014289,5.95943193237174,38.4555281140923));
#55494=CARTESIAN_POINT('Ctrl Pts',(17.6516296863262,5.95525377784107,38.3780182980553));
#55495=CARTESIAN_POINT('Ctrl Pts',(17.6437036009049,5.95107562331041,38.2999641866128));
#55496=CARTESIAN_POINT('Ctrl Pts',(17.6396698565796,5.94689746877974,38.2217869244251));
#55497=CARTESIAN_POINT('Ctrl Pts',(17.637539260058,5.94469059576259,38.1804942222977));
#55498=CARTESIAN_POINT('Ctrl Pts',(17.6364937042972,5.94248372274543,38.1391672076312));
#55499=CARTESIAN_POINT('Ctrl Pts',(17.6365309617434,5.94027684972828,38.0978678408989));
#55500=CARTESIAN_POINT('',(17.6365301680466,5.14652684968129,38.1008912610287));
#55501=CARTESIAN_POINT('Ctrl Pts',(17.6365309617442,5.94027684968202,38.0978678400331));
#55502=CARTESIAN_POINT('Ctrl Pts',(17.6366235326623,5.93479359199753,37.9952542921597));
#55503=CARTESIAN_POINT('Ctrl Pts',(17.6434025454018,5.92931033431303,37.8929359218963));
#55504=CARTESIAN_POINT('Ctrl Pts',(17.6567308745933,5.92382707662854,37.7916491498052));
#55505=CARTESIAN_POINT('Ctrl Pts',(17.6688028908594,5.91886066448436,37.6999095519417));
#55506=CARTESIAN_POINT('Ctrl Pts',(17.6862470647488,5.91389425234017,37.6090156628067));
#55507=CARTESIAN_POINT('Ctrl Pts',(17.7089286062922,5.90892784019599,37.5194982258133));
#55508=CARTESIAN_POINT('Ctrl Pts',(17.7282818655146,5.90469019781849,37.4431165495617));
#55509=CARTESIAN_POINT('Ctrl Pts',(17.751495345354,5.900452555441,37.3675603792653));
#55510=CARTESIAN_POINT('Ctrl Pts',(17.778481962481,5.8962149130635,37.2932484583978));
#55511=CARTESIAN_POINT('Ctrl Pts',(17.8054297717935,5.89198336458204,37.2190434009888));
#55512=CARTESIAN_POINT('Ctrl Pts',(17.83613978433,5.88775181610058,37.1460794766435));
#55513=CARTESIAN_POINT('Ctrl Pts',(17.8704744921261,5.88352026761912,37.0747626849288));
#55514=CARTESIAN_POINT('Ctrl Pts',(17.9047695423865,5.87929360669301,37.003528266078));
#55515=CARTESIAN_POINT('Ctrl Pts',(17.9426807657155,5.8750669457669,36.9339376193788));
#55516=CARTESIAN_POINT('Ctrl Pts',(17.9840222362744,5.87084028484079,36.8663776521708));
#55517=CARTESIAN_POINT('Ctrl Pts',(18.0253376108088,5.86661629191477,36.7988603309193));
#55518=CARTESIAN_POINT('Ctrl Pts',(18.0700786906955,5.86239229898875,36.7333715436769));
#55519=CARTESIAN_POINT('Ctrl Pts',(18.1180137851516,5.85816830606273,36.6702733380046));
#55520=CARTESIAN_POINT('Ctrl Pts',(18.1659335464848,5.85394566427627,36.6071953157188));
#55521=CARTESIAN_POINT('Ctrl Pts',(18.2170450101681,5.84972302248981,36.5465067295028));
#55522=CARTESIAN_POINT('Ctrl Pts',(18.2710742197591,5.84550038070334,36.4885391449624));
#55523=CARTESIAN_POINT('Ctrl Pts',(18.3251029689308,5.84127777490085,36.4305720544029));
#55524=CARTESIAN_POINT('Ctrl Pts',(18.3820490939087,5.83705516909836,36.3753262613571));
#55525=CARTESIAN_POINT('Ctrl Pts',(18.4416005755605,5.83283256329587,36.3230977306541));
#55526=CARTESIAN_POINT('Ctrl Pts',(18.5012112735172,5.82860575865388,36.270817265381));
#55527=CARTESIAN_POINT('Ctrl Pts',(18.5634321498163,5.8243789540119,36.2215603653372));
#55528=CARTESIAN_POINT('Ctrl Pts',(18.6279172297163,5.82015214936991,36.1755833838821));
#55529=CARTESIAN_POINT('Ctrl Pts',(18.6924335579561,5.81592329649245,36.1295841227874));
#55530=CARTESIAN_POINT('Ctrl Pts',(18.7592158801282,5.811694443615,36.0868681994476));
#55531=CARTESIAN_POINT('Ctrl Pts',(18.827890447833,5.80746559073754,36.0476477791035));
#55532=CARTESIAN_POINT('Ctrl Pts',(18.8966884387851,5.80322913768476,36.0083568710694));
#55533=CARTESIAN_POINT('Ctrl Pts',(18.9673850511148,5.79899268463198,35.972574230643));
#55534=CARTESIAN_POINT('Ctrl Pts',(19.0395834392595,5.79475623157919,35.9404652189058));
#55535=CARTESIAN_POINT('Ctrl Pts',(19.1052025646453,5.7909058361451,35.9112822229784));
#55536=CARTESIAN_POINT('Ctrl Pts',(19.1720617280285,5.78705544071101,35.8851333044687));
#55537=CARTESIAN_POINT('Ctrl Pts',(19.2398525600461,5.78320504527692,35.8621067249684));
#55538=CARTESIAN_POINT('Ctrl Pts',(19.3144613391911,5.77896740289943,35.8367642865698));
#55539=CARTESIAN_POINT('Ctrl Pts',(19.3904788833851,5.77472976052194,35.815109414351));
#55540=CARTESIAN_POINT('Ctrl Pts',(19.4675065197498,5.77049211814445,35.7972969938807));
#55541=CARTESIAN_POINT('Ctrl Pts',(19.5444233873506,5.76626056966299,35.77951018837));
#55542=CARTESIAN_POINT('Ctrl Pts',(19.6223470095406,5.76202902118154,35.7655549660279));
#55543=CARTESIAN_POINT('Ctrl Pts',(19.7008619559717,5.75779747270009,35.7555369758695));
#55544=CARTESIAN_POINT('Ctrl Pts',(19.7792862154715,5.75357081177399,35.7455305567665));
#55545=CARTESIAN_POINT('Ctrl Pts',(19.8582999792779,5.74934415084789,35.7394523916293));
#55546=CARTESIAN_POINT('Ctrl Pts',(19.9374774773243,5.74511748992178,35.7373571207103));
#55547=CARTESIAN_POINT('Ctrl Pts',(20.0166049960666,5.74089349699577,35.7352631723916));
#55548=CARTESIAN_POINT('Ctrl Pts',(20.0958955765188,5.73666950406976,35.737147140395));
#55549=CARTESIAN_POINT('Ctrl Pts',(20.1749193911915,5.73244551114374,35.7430117421834));
#55550=CARTESIAN_POINT('Ctrl Pts',(20.2539179283118,5.72822286935729,35.7488744680465));
#55551=CARTESIAN_POINT('Ctrl Pts',(20.3326494019525,5.72400022757083,35.7587152645124));
#55552=CARTESIAN_POINT('Ctrl Pts',(20.4106865482482,5.71977758578438,35.7724848013412));
#55553=CARTESIAN_POINT('Ctrl Pts',(20.4887230295368,5.71555497998189,35.7862542208304));
#55554=CARTESIAN_POINT('Ctrl Pts',(20.5660647338519,5.71133237417941,35.8039522312514));
#55555=CARTESIAN_POINT('Ctrl Pts',(20.6422935427912,5.70710976837693,35.8254781940398));
#55556=CARTESIAN_POINT('Ctrl Pts',(20.7185981514971,5.70288296373495,35.8470255616352));
#55557=CARTESIAN_POINT('Ctrl Pts',(20.7937872021454,5.69865615909297,35.8724083572244));
#55558=CARTESIAN_POINT('Ctrl Pts',(20.8674573218677,5.69442935445099,35.9014758960525));
#55559=CARTESIAN_POINT('Ctrl Pts',(20.9411631408391,5.69020050157354,35.9305575205005));
#55560=CARTESIAN_POINT('Ctrl Pts',(21.0133481351976,5.6859716486961,35.9633272512121));
#55561=CARTESIAN_POINT('Ctrl Pts',(21.083630881866,5.68174279581865,35.9995870518476));
#55562=CARTESIAN_POINT('Ctrl Pts',(21.1540399420318,5.67750634276588,36.0359120192907));
#55563=CARTESIAN_POINT('Ctrl Pts',(21.222539517287,5.6732698897131,36.0757393533793));
#55564=CARTESIAN_POINT('Ctrl Pts',(21.2887748744403,5.66903343666033,36.1188261651457));
#55565=CARTESIAN_POINT('Ctrl Pts',(21.3489743652848,5.66518304122616,36.1579865810009));
#55566=CARTESIAN_POINT('Ctrl Pts',(21.4073036636659,5.66133264579199,36.1998387806815));
#55567=CARTESIAN_POINT('Ctrl Pts',(21.463520873394,5.65748225035783,36.2441721270441));
#55568=CARTESIAN_POINT('Ctrl Pts',(21.5253920329571,5.65324460798033,36.2929642239843));
#55569=CARTESIAN_POINT('Ctrl Pts',(21.5849366536444,5.64900696560284,36.3449453615566));
#55570=CARTESIAN_POINT('Ctrl Pts',(21.6418077951597,5.64476932322535,36.3998654157236));
#55571=CARTESIAN_POINT('Ctrl Pts',(21.6985971537418,5.64053777474389,36.4547064926974));
#55572=CARTESIAN_POINT('Ctrl Pts',(21.7527203336871,5.63630622626243,36.5124777703227));
#55573=CARTESIAN_POINT('Ctrl Pts',(21.8038625759622,5.63207467778097,36.5728882660581));
#55574=CARTESIAN_POINT('Ctrl Pts',(21.8549457475351,5.62784801685487,36.6332289860026));
#55575=CARTESIAN_POINT('Ctrl Pts',(21.9030545223185,5.62362135592877,36.6962025102102));
#55576=CARTESIAN_POINT('Ctrl Pts',(21.9479113026009,5.61939469500266,36.7614814166028));
#55577=CARTESIAN_POINT('Ctrl Pts',(21.9927397678858,5.61517070207664,36.8267191169155));
#55578=CARTESIAN_POINT('Ctrl Pts',(22.0343200483831,5.61094670915063,36.8942589256039));
#55579=CARTESIAN_POINT('Ctrl Pts',(22.0724158941268,5.60672271622461,36.9637417535302));
#55580=CARTESIAN_POINT('Ctrl Pts',(22.1104995540536,5.60250007443815,37.0332023558044));
#55581=CARTESIAN_POINT('Ctrl Pts',(22.1451007673485,5.59827743265169,37.1046043323545));
#55582=CARTESIAN_POINT('Ctrl Pts',(22.1760283406479,5.59405479086523,37.1775624131699));
#55583=CARTESIAN_POINT('Ctrl Pts',(22.2069556503927,5.58983218506275,37.2505198722603));
#55584=CARTESIAN_POINT('Ctrl Pts',(22.2342092007462,5.58560957926027,37.3250329770968));
#55585=CARTESIAN_POINT('Ctrl Pts',(22.2576458174357,5.58138697345778,37.4006962005573));
#55586=CARTESIAN_POINT('Ctrl Pts',(22.2811057388325,5.5771601688158,37.4764346613822));
#55587=CARTESIAN_POINT('Ctrl Pts',(22.3007410061124,5.57293336417381,37.5533250764427));
#55588=CARTESIAN_POINT('Ctrl Pts',(22.3164584536478,5.56870655953183,37.6309470462476));
#55589=CARTESIAN_POINT('Ctrl Pts',(22.3321835175828,5.56447770665438,37.708606630299));
#55590=CARTESIAN_POINT('Ctrl Pts',(22.34398690984,5.56024885377693,37.7869980111561));
#55591=CARTESIAN_POINT('Ctrl Pts',(22.3518271345525,5.55602000089948,37.8656934271461));
#55592=CARTESIAN_POINT('Ctrl Pts',(22.359681449867,5.5517835478467,37.9445302760439));
#55593=CARTESIAN_POINT('Ctrl Pts',(22.3635583428394,5.54754709479392,38.0236717825474));
#55594=CARTESIAN_POINT('Ctrl Pts',(22.3634684712725,5.54331064174114,38.1026881593849));
#55595=CARTESIAN_POINT('Ctrl Pts',(22.3633867894819,5.53946024630701,38.1745039668083));
#55596=CARTESIAN_POINT('Ctrl Pts',(22.3600290452797,5.53560985087289,38.2462161639682));
#55597=CARTESIAN_POINT('Ctrl Pts',(22.3534402626473,5.53175945543876,38.3175071747104));
#55598=CARTESIAN_POINT('Ctrl Pts',(22.346188824457,5.52752181306127,38.3959681570753));
#55599=CARTESIAN_POINT('Ctrl Pts',(22.3349957856703,5.52328417068377,38.4742133895104));
#55600=CARTESIAN_POINT('Ctrl Pts',(22.319882115305,5.51904652830628,38.5518156836456));
#55601=CARTESIAN_POINT('Ctrl Pts',(22.3047901789907,5.51481497982482,38.6293063826365));
#55602=CARTESIAN_POINT('Ctrl Pts',(22.2857888965608,5.51058343134337,38.7061555231122));
#55603=CARTESIAN_POINT('Ctrl Pts',(22.2629510293121,5.50635188286191,38.7819406717855));
#55604=CARTESIAN_POINT('Ctrl Pts',(22.2401395404308,5.50212522193581,38.8576382865193));
#55605=CARTESIAN_POINT('Ctrl Pts',(22.213500407533,5.4978985610097,38.9322739050989));
#55606=CARTESIAN_POINT('Ctrl Pts',(22.1831571880899,5.4936719000836,39.0054364323306));
#55607=CARTESIAN_POINT('Ctrl Pts',(22.1528331222324,5.48944790715758,39.0785527770953));
#55608=CARTESIAN_POINT('Ctrl Pts',(22.1188097898846,5.48522391423156,39.1501974443069));
#55609=CARTESIAN_POINT('Ctrl Pts',(22.0812598200345,5.48099992130555,39.2199767865495));
#55610=CARTESIAN_POINT('Ctrl Pts',(22.0437218613905,5.47677727951909,39.2897338082933));
#55611=CARTESIAN_POINT('Ctrl Pts',(22.002659727355,5.47255463773263,39.3576262774278));
#55612=CARTESIAN_POINT('Ctrl Pts',(21.9582925351113,5.46833199594617,39.4232840918817));
#55613=CARTESIAN_POINT('Ctrl Pts',(21.9139257209504,5.46410939014368,39.4889413468213));
#55614=CARTESIAN_POINT('Ctrl Pts',(21.8662541682268,5.4598867843412,39.5523635973345));
#55615=CARTESIAN_POINT('Ctrl Pts',(21.8155401256557,5.45566417853871,39.6132099963436));
#55616=CARTESIAN_POINT('Ctrl Pts',(21.7647756544783,5.45143737389673,39.6741168992869));
#55617=CARTESIAN_POINT('Ctrl Pts',(21.7109629511014,5.44721056925474,39.732442473477));
#55618=CARTESIAN_POINT('Ctrl Pts',(21.6544039616708,5.44298376461276,39.7878797269083));
#55619=CARTESIAN_POINT('Ctrl Pts',(21.5978175647449,5.43875491173531,39.8433438442612));
#55620=CARTESIAN_POINT('Ctrl Pts',(21.5384825819637,5.43452605885786,39.8959165413559));
#55621=CARTESIAN_POINT('Ctrl Pts',(21.4767352610551,5.43029720598041,39.9453301627775));
#55622=CARTESIAN_POINT('Ctrl Pts',(21.4148769666796,5.42606075292763,39.9948325913053));
#55623=CARTESIAN_POINT('Ctrl Pts',(21.3505980526119,5.42182429987485,40.0411643251066));
#55624=CARTESIAN_POINT('Ctrl Pts',(21.2842648548844,5.41758784682207,40.0841003561838));
#55625=CARTESIAN_POINT('Ctrl Pts',(21.2239764394388,5.41373745138794,40.1231237316256));
#55626=CARTESIAN_POINT('Ctrl Pts',(21.1619916621134,5.4098870559538,40.1593425257466));
#55627=CARTESIAN_POINT('Ctrl Pts',(21.0986014354038,5.40603666051967,40.1926216397211));
#55628=CARTESIAN_POINT('Ctrl Pts',(21.028835844929,5.40179901814217,40.2292477437346));
#55629=CARTESIAN_POINT('Ctrl Pts',(20.9571056868249,5.39756137576468,40.2624499264109));
#55630=CARTESIAN_POINT('Ctrl Pts',(20.8837807297505,5.39332373338719,40.2920132441712));
#55631=CARTESIAN_POINT('Ctrl Pts',(20.8105612168419,5.38909218490573,40.3215340487203));
#55632=CARTESIAN_POINT('Ctrl Pts',(20.7357518905846,5.38486063642427,40.3474262064284));
#55633=CARTESIAN_POINT('Ctrl Pts',(20.6597467231307,5.38062908794282,40.3695208089415));
#55634=CARTESIAN_POINT('Ctrl Pts',(20.5838293437441,5.37640242701671,40.3915898915785));
#55635=CARTESIAN_POINT('Ctrl Pts',(20.5067193158726,5.37217576609061,40.4098700054719));
#55636=CARTESIAN_POINT('Ctrl Pts',(20.4288287506712,5.36794910516451,40.4242410252592));
#55637=CARTESIAN_POINT('Ctrl Pts',(20.3509873524219,5.36372511223849,40.4386029736109));
#55638=CARTESIAN_POINT('Ctrl Pts',(20.2723668545833,5.35950111931247,40.4490606408231));
#55639=CARTESIAN_POINT('Ctrl Pts',(20.1933914433055,5.35527712638646,40.4555445634834));
#55640=CARTESIAN_POINT('Ctrl Pts',(20.114441294097,5.3510544846,40.4620264121146));
#55641=CARTESIAN_POINT('Ctrl Pts',(20.0351369237563,5.34683184281354,40.4645370020018));
#55642=CARTESIAN_POINT('Ctrl Pts',(19.9559080721833,5.34260920102708,40.4630586837405));
#55643=CARTESIAN_POINT('Ctrl Pts',(19.8766798957726,5.3383865952246,40.461580378077));
#55644=CARTESIAN_POINT('Ctrl Pts',(19.7975277055146,5.33416398942211,40.4561132420264));
#55645=CARTESIAN_POINT('Ctrl Pts',(19.7188801782686,5.32994138361963,40.4466917323606));
#55646=CARTESIAN_POINT('Ctrl Pts',(19.6401544461512,5.32571457897764,40.4372608542128));
#55647=CARTESIAN_POINT('Ctrl Pts',(19.5619348459664,5.32148777433566,40.4238678039155));
#55648=CARTESIAN_POINT('Ctrl Pts',(19.484643263373,5.31726096969368,40.4065987676475));
#55649=CARTESIAN_POINT('Ctrl Pts',(19.4073142266329,5.31303211681622,40.3893213631072));
#55650=CARTESIAN_POINT('Ctrl Pts',(19.3309145556901,5.30880326393877,40.3681643561995));
#55651=CARTESIAN_POINT('Ctrl Pts',(19.2558518095822,5.30457441106132,40.3432641198927));
#55652=CARTESIAN_POINT('Ctrl Pts',(19.1806541592704,5.30033795800854,40.3183191324046));
#55653=CARTESIAN_POINT('Ctrl Pts',(19.1067986726909,5.29610150495576,40.2896176437174));
#55654=CARTESIAN_POINT('Ctrl Pts',(19.0346735114784,5.29186505190298,40.2573444814073));
#55655=CARTESIAN_POINT('Ctrl Pts',(18.9691209400327,5.28801465646886,40.2280122935474));
#55656=CARTESIAN_POINT('Ctrl Pts',(18.9049976509105,5.28416426103473,40.1957304494275));
#55657=CARTESIAN_POINT('Ctrl Pts',(18.8425753281453,5.2803138656006,40.1606694470201));
#55658=CARTESIAN_POINT('Ctrl Pts',(18.7738749869007,5.27607622322311,40.1220822441884));
#55659=CARTESIAN_POINT('Ctrl Pts',(18.7069774783263,5.27183858084562,40.07998326721));
#55660=CARTESIAN_POINT('Ctrl Pts',(18.6422643898427,5.26760093846813,40.0345657016009));
#55661=CARTESIAN_POINT('Ctrl Pts',(18.5776443613199,5.26336938998668,39.9892134482336));
#55662=CARTESIAN_POINT('Ctrl Pts',(18.515202895127,5.25913784150523,39.9405523505732));
#55663=CARTESIAN_POINT('Ctrl Pts',(18.4552961360479,5.25490629302378,39.8888209562703));
#55664=CARTESIAN_POINT('Ctrl Pts',(18.3954585709299,5.25067963209768,39.8371493131562));
#55665=CARTESIAN_POINT('Ctrl Pts',(18.3381502479364,5.24645297117158,39.7824147255725));
#55666=CARTESIAN_POINT('Ctrl Pts',(18.2836962630847,5.24222631024548,39.7248975117067));
#55667=CARTESIAN_POINT('Ctrl Pts',(18.2292766512852,5.23800231731946,39.6674166044986));
#55668=CARTESIAN_POINT('Ctrl Pts',(18.1777081227993,5.23377832439344,39.6071568969513));
#55669=CARTESIAN_POINT('Ctrl Pts',(18.129279847825,5.22955433146743,39.5444364136737));
#55670=CARTESIAN_POINT('Ctrl Pts',(18.0808670637285,5.22533168968097,39.4817359929595));
#55671=CARTESIAN_POINT('Ctrl Pts',(18.0355928247275,5.22110904789452,39.4165767303823));
#55672=CARTESIAN_POINT('Ctrl Pts',(17.9937058590316,5.21688640610806,39.3493095136178));
#55673=CARTESIAN_POINT('Ctrl Pts',(17.9518192502828,5.21266380030557,39.2820428700825));
#55674=CARTESIAN_POINT('Ctrl Pts',(17.9133201040219,5.20844119450308,39.2126687067619));
#55675=CARTESIAN_POINT('Ctrl Pts',(17.8784128596257,5.2042185887006,39.1415653828245));
#55676=CARTESIAN_POINT('Ctrl Pts',(17.8434709044553,5.19999178405862,39.0703913557576));
#55677=CARTESIAN_POINT('Ctrl Pts',(17.8121281926727,5.19576497941664,38.9974851552844));
#55678=CARTESIAN_POINT('Ctrl Pts',(17.7845420728401,5.19153817477466,38.9232476018091));
#55679=CARTESIAN_POINT('Ctrl Pts',(17.7569425852572,5.18730932189721,38.8489740741162));
#55680=CARTESIAN_POINT('Ctrl Pts',(17.7331034571786,5.18308046901976,38.7733683558542));
#55681=CARTESIAN_POINT('Ctrl Pts',(17.7131321386065,5.17885161614231,38.6968465677422));
#55682=CARTESIAN_POINT('Ctrl Pts',(17.6931249271985,5.17461516308954,38.620187253208));
#55683=CARTESIAN_POINT('Ctrl Pts',(17.6769995102976,5.17037871003676,38.5426090392524));
#55684=CARTESIAN_POINT('Ctrl Pts',(17.6648121322106,5.16614225698399,38.4645381503067));
#55685=CARTESIAN_POINT('Ctrl Pts',(17.6537353601193,5.16229186154983,38.3935816707724));
#55686=CARTESIAN_POINT('Ctrl Pts',(17.6459109682121,5.15844146611567,38.3222185671474));
#55687=CARTESIAN_POINT('Ctrl Pts',(17.6413438185386,5.15459107068152,38.250769554466));
#55688=CARTESIAN_POINT('Ctrl Pts',(17.6381553577927,5.15190299703044,38.200888909304));
#55689=CARTESIAN_POINT('Ctrl Pts',(17.6365490285732,5.14921492337936,38.1509060607469));
#55690=CARTESIAN_POINT('Ctrl Pts',(17.6365301680469,5.14652684972828,38.100891261903));
#55691=CARTESIAN_POINT('',(17.6365304347554,4.35277684975661,38.1014335489659));
#55692=CARTESIAN_POINT('Ctrl Pts',(17.6365301680466,5.14652684968129,38.1008912610287));
#55693=CARTESIAN_POINT('Ctrl Pts',(17.6365007172957,5.14232941297597,38.0227929721683));
#55694=CARTESIAN_POINT('Ctrl Pts',(17.6403465262968,5.13813197627065,37.944538778742));
#55695=CARTESIAN_POINT('Ctrl Pts',(17.6480877422875,5.13393453956532,37.8665494208153));
#55696=CARTESIAN_POINT('Ctrl Pts',(17.6561615253538,5.12955677857354,37.7852095953753));
#55697=CARTESIAN_POINT('Ctrl Pts',(17.6684730614319,5.12517901758175,37.7041583895631));
#55698=CARTESIAN_POINT('Ctrl Pts',(17.6849847219665,5.12080125658996,37.6238753279115));
#55699=CARTESIAN_POINT('Ctrl Pts',(17.7007772898864,5.11661414968722,37.5470886412364));
#55700=CARTESIAN_POINT('Ctrl Pts',(17.7204116738816,5.11242704278448,37.4710051167982));
#55701=CARTESIAN_POINT('Ctrl Pts',(17.7438020749889,5.10823993588174,37.3960388049932));
#55702=CARTESIAN_POINT('Ctrl Pts',(17.7671799540606,5.10405507054387,37.321112626353));
#55703=CARTESIAN_POINT('Ctrl Pts',(17.7943097185199,5.09987020520601,37.2473029294767));
#55704=CARTESIAN_POINT('Ctrl Pts',(17.8250551809499,5.09568533986814,37.1750105541211));
#55705=CARTESIAN_POINT('Ctrl Pts',(17.8557942006474,5.09150135147166,37.102733327682));
#55706=CARTESIAN_POINT('Ctrl Pts',(17.8901472264574,5.08731736307517,37.03197323143));
#55707=CARTESIAN_POINT('Ctrl Pts',(17.927929795733,5.08313337467868,36.9631114788649));
#55708=CARTESIAN_POINT('Ctrl Pts',(17.9657167571783,5.07894889989951,36.8942417212192));
#55709=CARTESIAN_POINT('Ctrl Pts',(18.0069338210219,5.07476442512034,36.8272711634052));
#55710=CARTESIAN_POINT('Ctrl Pts',(18.0513511975692,5.07057995034116,36.7625553149064));
#55711=CARTESIAN_POINT('Ctrl Pts',(18.0958154486267,5.06639105960543,36.6977711705304));
#55712=CARTESIAN_POINT('Ctrl Pts',(18.1434864789077,5.06220216886969,36.6352468772897));
#55713=CARTESIAN_POINT('Ctrl Pts',(18.194092390071,5.05801327813396,36.5753071964161));
#55714=CARTESIAN_POINT('Ctrl Pts',(18.244729818509,5.05382177856426,36.515330185212));
#55715=CARTESIAN_POINT('Ctrl Pts',(18.2983054368241,5.04963027899456,36.4579413368638));
#55716=CARTESIAN_POINT('Ctrl Pts',(18.3545102414385,5.04543877942486,36.4034287827005));
#55717=CARTESIAN_POINT('Ctrl Pts',(18.4108053900339,5.04124054241054,36.3488286046909));
#55718=CARTESIAN_POINT('Ctrl Pts',(18.4697377955761,5.03704230539623,36.2971142568638));
#55719=CARTESIAN_POINT('Ctrl Pts',(18.5309657889771,5.03284406838192,36.2485333036362));
#55720=CARTESIAN_POINT('Ctrl Pts',(18.5502937277793,5.03151880417543,36.233197676274));
#55721=CARTESIAN_POINT('Ctrl Pts',(18.569850209863,5.03019353996893,36.2181739573338));
#55722=CARTESIAN_POINT('Ctrl Pts',(18.5896239431852,5.02886827576244,36.2034690038748));
#55723=CARTESIAN_POINT('Ctrl Pts',(18.6528520979012,5.02463063338495,36.1564486937875));
#55724=CARTESIAN_POINT('Ctrl Pts',(18.7185529135914,5.02039299100746,36.1125055107695));
#55725=CARTESIAN_POINT('Ctrl Pts',(18.7863945055933,5.01615534862996,36.0719092365365));
#55726=CARTESIAN_POINT('Ctrl Pts',(18.8541385387237,5.0119238001485,36.031371341339));
#55727=CARTESIAN_POINT('Ctrl Pts',(18.9240168355792,5.00769225166704,35.994171035501));
#55728=CARTESIAN_POINT('Ctrl Pts',(18.9956664497596,5.00346070318558,35.9605363848007));
#55729=CARTESIAN_POINT('Ctrl Pts',(19.0672333066569,4.99923404225947,35.9269405830509));
#55730=CARTESIAN_POINT('Ctrl Pts',(19.1405669929246,4.99500738133337,35.8969024502745));
#55731=CARTESIAN_POINT('Ctrl Pts',(19.215279064378,4.99078072040726,35.8706046797177));
#55732=CARTESIAN_POINT('Ctrl Pts',(19.2899439752438,4.98655672748124,35.8443235091332));
#55733=CARTESIAN_POINT('Ctrl Pts',(19.3659851032591,4.98233273455522,35.8217781696134));
#55734=CARTESIAN_POINT('Ctrl Pts',(19.442994204912,4.9781087416292,35.8031031836109));
#55735=CARTESIAN_POINT('Ctrl Pts',(19.519978673464,4.97388609984274,35.7844341712246));
#55736=CARTESIAN_POINT('Ctrl Pts',(19.5979300455523,4.96966345805628,35.76963316429));
#55737=CARTESIAN_POINT('Ctrl Pts',(19.6764265414123,4.96544081626982,35.7587843632426));
#55738=CARTESIAN_POINT('Ctrl Pts',(19.7549223683509,4.96121821046733,35.747935654645));
#55739=CARTESIAN_POINT('Ctrl Pts',(19.8339628452702,4.95699560466484,35.7410391477315));
#55740=CARTESIAN_POINT('Ctrl Pts',(19.9131191472081,4.95277299886236,35.7381274043001));
#55741=CARTESIAN_POINT('Ctrl Pts',(19.9923541599286,4.94854619422037,35.7352127655136));
#55742=CARTESIAN_POINT('Ctrl Pts',(20.0717047581808,4.94431938957838,35.7362908222652));
#55743=CARTESIAN_POINT('Ctrl Pts',(20.1507407889469,4.9400925849364,35.7413419799709));
#55744=CARTESIAN_POINT('Ctrl Pts',(20.2298151191886,4.93586373205895,35.7463955853791));
#55745=CARTESIAN_POINT('Ctrl Pts',(20.3085741119602,4.9316348791815,35.7554260736865));
#55746=CARTESIAN_POINT('Ctrl Pts',(20.3865939697747,4.92740602630405,35.7683620470935));
#55747=CARTESIAN_POINT('Ctrl Pts',(20.4647540463709,4.92316957325127,35.7813212692796));
#55748=CARTESIAN_POINT('Ctrl Pts',(20.5421718746618,4.91893312019849,35.7981999011402));
#55749=CARTESIAN_POINT('Ctrl Pts',(20.6184352910172,4.91469666714571,35.818875665001));
#55750=CARTESIAN_POINT('Ctrl Pts',(20.6877490085225,4.91084627171159,35.8376672970043));
#55751=CARTESIAN_POINT('Ctrl Pts',(20.7561090637551,4.90699587627747,35.8595948257343));
#55752=CARTESIAN_POINT('Ctrl Pts',(20.8232205826439,4.90314548084336,35.8845320329079));
#55753=CARTESIAN_POINT('Ctrl Pts',(20.8970817279021,4.89890783846587,35.9119772570941));
#55754=CARTESIAN_POINT('Ctrl Pts',(20.9697075282217,4.89467019608838,35.9431717060236));
#55755=CARTESIAN_POINT('Ctrl Pts',(21.0406910158519,4.89043255371089,35.9779838241839));
#55756=CARTESIAN_POINT('Ctrl Pts',(21.1115724264413,4.88620100522944,36.0127458811522));
#55757=CARTESIAN_POINT('Ctrl Pts',(21.1808157970728,4.88196945674798,36.0511150712587));
#55758=CARTESIAN_POINT('Ctrl Pts',(21.2480322461359,4.87773790826653,36.0929110748387));
#55759=CARTESIAN_POINT('Ctrl Pts',(21.3151710583441,4.87351124734042,36.1346588028804));
#55760=CARTESIAN_POINT('Ctrl Pts',(21.3802872053651,4.86928458641432,36.179825232443));
#55761=CARTESIAN_POINT('Ctrl Pts',(21.4430159877848,4.86505792548821,36.2281839567154));
#55762=CARTESIAN_POINT('Ctrl Pts',(21.5057051738423,4.8608339325622,36.2765121554541));
#55763=CARTESIAN_POINT('Ctrl Pts',(21.5660096161983,4.85660993963618,36.3280283637388));
#55764=CARTESIAN_POINT('Ctrl Pts',(21.6235942468787,4.85238594671016,36.3824633446699));
#55765=CARTESIAN_POINT('Ctrl Pts',(21.6811604578141,4.8481633049237,36.4368809133427));
#55766=CARTESIAN_POINT('Ctrl Pts',(21.7360082442959,4.84394066313724,36.494215078853));
#55767=CARTESIAN_POINT('Ctrl Pts',(21.787837383596,4.83971802135078,36.5541578571159));
#55768=CARTESIAN_POINT('Ctrl Pts',(21.8396660812251,4.8354954155483,36.614100124566));
#55769=CARTESIAN_POINT('Ctrl Pts',(21.888475877297,4.83127280974582,36.6766506050328));
#55770=CARTESIAN_POINT('Ctrl Pts',(21.9340060321114,4.82705020394334,36.7414672956985));
#55771=CARTESIAN_POINT('Ctrl Pts',(21.979581460821,4.82282339930136,36.8063484382439));
#55772=CARTESIAN_POINT('Ctrl Pts',(22.0218704639672,4.81859659465938,36.8734999077903));
#55773=CARTESIAN_POINT('Ctrl Pts',(22.0606553312402,4.81436979001739,36.9425501968848));
#55774=CARTESIAN_POINT('Ctrl Pts',(22.0994589929802,4.81014093713994,37.0116339465395));
#55775=CARTESIAN_POINT('Ctrl Pts',(22.1347549271662,4.80591208426249,37.0826179284749));
#55776=CARTESIAN_POINT('Ctrl Pts',(22.166372339068,4.80168323138504,37.1551077683561));
#55777=CARTESIAN_POINT('Ctrl Pts',(22.1980465743876,4.79744677833226,37.2277278883651));
#55778=CARTESIAN_POINT('Ctrl Pts',(22.2260289118425,4.79321032527948,37.3018588342739));
#55779=CARTESIAN_POINT('Ctrl Pts',(22.2501975709019,4.7889738722267,37.3770882952895));
#55780=CARTESIAN_POINT('Ctrl Pts',(22.272163799096,4.78512347679256,37.4454622792801));
#55781=CARTESIAN_POINT('Ctrl Pts',(22.2909803129078,4.78127308135842,37.5147432469093));
#55782=CARTESIAN_POINT('Ctrl Pts',(22.3065924823299,4.77742268592428,37.5846151327803));
#55783=CARTESIAN_POINT('Ctrl Pts',(22.3237748190222,4.77318504354679,37.6615142642142));
#55784=CARTESIAN_POINT('Ctrl Pts',(22.3371396104549,4.7689474011693,37.7394179410598));
#55785=CARTESIAN_POINT('Ctrl Pts',(22.3465756872768,4.76470975879181,37.8179131609216));
#55786=CARTESIAN_POINT('Ctrl Pts',(22.35599819465,4.76047821031035,37.8962955015771));
#55787=CARTESIAN_POINT('Ctrl Pts',(22.3615031515985,4.75624666182888,37.9752672343355));
#55788=CARTESIAN_POINT('Ctrl Pts',(22.3630301403667,4.75201511334742,38.0544039846177));
#55789=CARTESIAN_POINT('Ctrl Pts',(22.3645553654206,4.74778845242132,38.1334493297678));
#55790=CARTESIAN_POINT('Ctrl Pts',(22.3621117440479,4.74356179149521,38.2126588473581));
#55791=CARTESIAN_POINT('Ctrl Pts',(22.3556906827349,4.73933513056911,38.291603361599));
#55792=CARTESIAN_POINT('Ctrl Pts',(22.3492736745959,4.73511113764309,38.3704980436024));
#55793=CARTESIAN_POINT('Ctrl Pts',(22.3388842478505,4.73088714471707,38.4491275882775));
#55794=CARTESIAN_POINT('Ctrl Pts',(22.3245658672038,4.72666315179105,38.5270643627503));
#55795=CARTESIAN_POINT('Ctrl Pts',(22.3102520666145,4.7224405100046,38.6049762073851));
#55796=CARTESIAN_POINT('Ctrl Pts',(22.2920118924536,4.71821786821814,38.6821952611433));
#55797=CARTESIAN_POINT('Ctrl Pts',(22.2699402806896,4.71399522643168,38.7583020302285));
#55798=CARTESIAN_POINT('Ctrl Pts',(22.2478688570126,4.7097726206292,38.8344081507568));
#55799=CARTESIAN_POINT('Ctrl Pts',(22.2219661925922,4.70555001482671,38.9094015556345));
#55800=CARTESIAN_POINT('Ctrl Pts',(22.1923772526242,4.70132740902423,38.9828773544928));
#55801=CARTESIAN_POINT('Ctrl Pts',(22.1627588902531,4.69710060438224,39.0564262156023));
#55802=CARTESIAN_POINT('Ctrl Pts',(22.1294471059438,4.69287379974026,39.1284540204798));
#55803=CARTESIAN_POINT('Ctrl Pts',(22.0926350378,4.68864699509828,39.1985759142962));
#55804=CARTESIAN_POINT('Ctrl Pts',(22.0558051311731,4.68441814222083,39.2687317879535));
#55805=CARTESIAN_POINT('Ctrl Pts',(22.0154718005368,4.68018928934339,39.3369795066057));
#55806=CARTESIAN_POINT('Ctrl Pts',(21.9718729040978,4.67596043646594,39.4029611241265));
#55807=CARTESIAN_POINT('Ctrl Pts',(21.9281956508876,4.67172398341317,39.4690613250733));
#55808=CARTESIAN_POINT('Ctrl Pts',(21.8812413836156,4.66748753036039,39.5328869087816));
#55809=CARTESIAN_POINT('Ctrl Pts',(21.8312896869721,4.66325107730761,39.594111282097));
#55810=CARTESIAN_POINT('Ctrl Pts',(21.7858899664306,4.65940068187347,39.6497564278203));
#55811=CARTESIAN_POINT('Ctrl Pts',(21.7380149052619,4.65555028643934,39.7032530836573));
#55812=CARTESIAN_POINT('Ctrl Pts',(21.6878999034291,4.6516998910052,39.7543833766404));
#55813=CARTESIAN_POINT('Ctrl Pts',(21.6327446708958,4.6474622486277,39.810656011497));
#55814=CARTESIAN_POINT('Ctrl Pts',(21.5746687322511,4.64322460625021,39.8642730411299));
#55815=CARTESIAN_POINT('Ctrl Pts',(21.5139580283905,4.63898696387271,39.9149163972955));
#55816=CARTESIAN_POINT('Ctrl Pts',(21.4533346289045,4.63475541539125,39.9654869263275));
#55817=CARTESIAN_POINT('Ctrl Pts',(21.3900843455973,4.6305238669098,40.0130919763475));
#55818=CARTESIAN_POINT('Ctrl Pts',(21.3245302850174,4.62629231842834,40.0574498626968));
#55819=CARTESIAN_POINT('Ctrl Pts',(21.2590519411876,4.62206565750224,40.1017565144625));
#55820=CARTESIAN_POINT('Ctrl Pts',(21.191275494293,4.61783899657613,40.1428231944919));
#55821=CARTESIAN_POINT('Ctrl Pts',(21.121556288238,4.61361233565003,40.1804090783338));
#55822=CARTESIAN_POINT('Ctrl Pts',(21.0518810911186,4.60938834272402,40.2179712367946));
#55823=CARTESIAN_POINT('Ctrl Pts',(20.9802659805198,4.605164349798,40.2520567383726));
#55824=CARTESIAN_POINT('Ctrl Pts',(20.9070933431826,4.60094035687199,40.2824692684329));
#55825=CARTESIAN_POINT('Ctrl Pts',(20.8339441117663,4.59671771508553,40.3128720703584));
#55826=CARTESIAN_POINT('Ctrl Pts',(20.7592387755196,4.59249507329907,40.3396040540671));
#55827=CARTESIAN_POINT('Ctrl Pts',(20.6833809112124,4.58827243151261,40.3625165128879));
#55828=CARTESIAN_POINT('Ctrl Pts',(20.607523693341,4.58404982571011,40.3854287764563));
#55829=CARTESIAN_POINT('Ctrl Pts',(20.5305144160999,4.57982721990762,40.4045214456795));
#55830=CARTESIAN_POINT('Ctrl Pts',(20.4527716386031,4.57560461410512,40.4196957309476));
#55831=CARTESIAN_POINT('Ctrl Pts',(20.3749515558925,4.57137780946314,40.4348851050949));
#55832=CARTESIAN_POINT('Ctrl Pts',(20.2963969771635,4.56715100482115,40.4461482223384));
#55833=CARTESIAN_POINT('Ctrl Pts',(20.2175358765903,4.56292420017917,40.4534376098159));
#55834=CARTESIAN_POINT('Ctrl Pts',(20.1386365613096,4.55869534730172,40.4607305296029));
#55835=CARTESIAN_POINT('Ctrl Pts',(20.0594308972479,4.55446649442428,40.4640458639742));
#55836=CARTESIAN_POINT('Ctrl Pts',(19.9803486284817,4.55023764154683,40.4633883016757));
#55837=CARTESIAN_POINT('Ctrl Pts',(19.9011242315485,4.54600118849405,40.4627295575936));
#55838=CARTESIAN_POINT('Ctrl Pts',(19.8220241421029,4.54176473544127,40.4580836776483));
#55839=CARTESIAN_POINT('Ctrl Pts',(19.7434745164375,4.53752828238849,40.4495074201166));
#55840=CARTESIAN_POINT('Ctrl Pts',(19.6720829262921,4.53367788695437,40.4417126959853));
#55841=CARTESIAN_POINT('Ctrl Pts',(19.6011462188211,4.52982749152024,40.4306719894504));
#55842=CARTESIAN_POINT('Ctrl Pts',(19.5309752971593,4.52597709608612,40.4164641739136));
#55843=CARTESIAN_POINT('Ctrl Pts',(19.4537470549203,4.52173945370862,40.4008274315996));
#55844=CARTESIAN_POINT('Ctrl Pts',(19.3771566697186,4.51750181133113,40.3812950633162));
#55845=CARTESIAN_POINT('Ctrl Pts',(19.3016266064833,4.51326416895363,40.3579337997665));
#55846=CARTESIAN_POINT('Ctrl Pts',(19.2262051584429,4.50903262047217,40.3346061306305));
#55847=CARTESIAN_POINT('Ctrl Pts',(19.1518414484292,4.50480107199071,40.3074606382079));
#55848=CARTESIAN_POINT('Ctrl Pts',(19.0789476509468,4.50056952350924,40.2766150351414));
#55849=CARTESIAN_POINT('Ctrl Pts',(19.0061380478138,4.49634286258314,40.2458050595984));
#55850=CARTESIAN_POINT('Ctrl Pts',(18.9347954128044,4.49211620165704,40.211303648146));
#55851=CARTESIAN_POINT('Ctrl Pts',(18.865315192058,4.48788954073094,40.1732777979629));
#55852=CARTESIAN_POINT('Ctrl Pts',(18.7958788293922,4.48366554780492,40.1352759508813));
#55853=CARTESIAN_POINT('Ctrl Pts',(18.7283029576661,4.47944155487891,40.0937543053894));
#55854=CARTESIAN_POINT('Ctrl Pts',(18.6629604055536,4.47521756195289,40.0489267722987));
#55855=CARTESIAN_POINT('Ctrl Pts',(18.5976387547325,4.47099492016643,40.0041135783071));
#55856=CARTESIAN_POINT('Ctrl Pts',(18.5345493911858,4.46677227837997,39.9559968616279));
#55857=CARTESIAN_POINT('Ctrl Pts',(18.4740367412951,4.46254963659351,39.9048342234074));
#55858=CARTESIAN_POINT('Ctrl Pts',(18.4135246070734,4.45832703079102,39.8536720211782));
#55859=CARTESIAN_POINT('Ctrl Pts',(18.3555894998982,4.45410442498852,39.7994642527695));
#55860=CARTESIAN_POINT('Ctrl Pts',(18.3005421277688,4.44988181918603,39.7425082591608));
#55861=CARTESIAN_POINT('Ctrl Pts',(18.2454400180932,4.44565501454405,39.6854956301268));
#55862=CARTESIAN_POINT('Ctrl Pts',(18.1932317057957,4.44142820990206,39.6257296550541));
#55863=CARTESIAN_POINT('Ctrl Pts',(18.1441899758712,4.43720140526008,39.5635435064402));
#55864=CARTESIAN_POINT('Ctrl Pts',(18.0951244811839,4.43297255238264,39.5013272235084));
#55865=CARTESIAN_POINT('Ctrl Pts',(18.0492288974533,4.42874369950519,39.4366888134454));
#55866=CARTESIAN_POINT('Ctrl Pts',(18.0067332164128,4.42451484662775,39.369991326879));
#55867=CARTESIAN_POINT('Ctrl Pts',(17.964161161321,4.42027839357497,39.3031739703132));
#55868=CARTESIAN_POINT('Ctrl Pts',(17.9250014502555,4.4160419405222,39.2342905515535));
#55869=CARTESIAN_POINT('Ctrl Pts',(17.8894384425492,4.41180548746942,39.1637294548478));
#55870=CARTESIAN_POINT('Ctrl Pts',(17.8571162048682,4.40795509203529,39.0995984185309));
#55871=CARTESIAN_POINT('Ctrl Pts',(17.8277645254185,4.40410469660117,39.0340820649915));
#55872=CARTESIAN_POINT('Ctrl Pts',(17.8014864754825,4.40025430116704,38.9674841343872));
#55873=CARTESIAN_POINT('Ctrl Pts',(17.7688461216759,4.39547166814932,38.8847618615015));
#55874=CARTESIAN_POINT('Ctrl Pts',(17.7408451901343,4.3906890351316,38.8001111929199));
#55875=CARTESIAN_POINT('Ctrl Pts',(17.7176868255926,4.38590640211389,38.7140333987874));
#55876=CARTESIAN_POINT('Ctrl Pts',(17.6946140719736,4.38114144934406,38.6282738136273));
#55877=CARTESIAN_POINT('Ctrl Pts',(17.6763482843133,4.37637649657422,38.5410978479686));
#55878=CARTESIAN_POINT('Ctrl Pts',(17.6630436254456,4.37161154380439,38.4530231498492));
#55879=CARTESIAN_POINT('Ctrl Pts',(17.6498224692232,4.36687649681154,38.365501225788));
#55880=CARTESIAN_POINT('Ctrl Pts',(17.6415004770565,4.36214144981869,38.2770920449245));
#55881=CARTESIAN_POINT('Ctrl Pts',(17.6381808545965,4.35740640282584,38.1883219412461));
#55882=CARTESIAN_POINT('Ctrl Pts',(17.6370989668228,4.35586321846943,38.159391154388));
#55883=CARTESIAN_POINT('Ctrl Pts',(17.6365480176339,4.35432003411302,38.1304221633823));
#55884=CARTESIAN_POINT('Ctrl Pts',(17.6365304347554,4.35277684975661,38.1014335489659));
#55885=CARTESIAN_POINT('',(17.6365308065437,3.55902684968247,38.098047441927));
#55886=CARTESIAN_POINT('Ctrl Pts',(17.6365304347551,4.35277684972829,38.1014335484339));
#55887=CARTESIAN_POINT('Ctrl Pts',(17.6364819365156,4.34852033665357,38.0214752364084));
#55888=CARTESIAN_POINT('Ctrl Pts',(17.6404953682683,4.34426382357884,37.941502555969));
#55889=CARTESIAN_POINT('Ctrl Pts',(17.6485485953399,4.34000731050412,37.8619522476012));
#55890=CARTESIAN_POINT('Ctrl Pts',(17.6566030235322,4.33575016258004,37.7823900744838));
#55891=CARTESIAN_POINT('Ctrl Pts',(17.6686983974036,4.33149301465597,37.7032508543268));
#55892=CARTESIAN_POINT('Ctrl Pts',(17.6847607875601,4.32723586673189,37.6249654432773));
#55893=CARTESIAN_POINT('Ctrl Pts',(17.7013320933604,4.32284383669156,37.5441996622471));
#55894=CARTESIAN_POINT('Ctrl Pts',(17.7221259304715,4.31845180665124,37.4643432170031));
#55895=CARTESIAN_POINT('Ctrl Pts',(17.7470048447539,4.31405977661091,37.385854866755));
#55896=CARTESIAN_POINT('Ctrl Pts',(17.771164415336,4.30979473680437,37.3096359121751));
#55897=CARTESIAN_POINT('Ctrl Pts',(17.7991758114773,4.30552969699783,37.2347074253263));
#55898=CARTESIAN_POINT('Ctrl Pts',(17.8308639407526,4.30126465719129,37.1614696609206));
#55899=CARTESIAN_POINT('Ctrl Pts',(17.8639673263188,4.29680913203407,37.0849609490282));
#55900=CARTESIAN_POINT('Ctrl Pts',(17.9010832925184,4.29235360687685,37.0102980217581));
#55901=CARTESIAN_POINT('Ctrl Pts',(17.9419595175657,4.28789808171962,36.937907140732));
#55902=CARTESIAN_POINT('Ctrl Pts',(17.9828357426131,4.2834425565624,36.8655162597058));
#55903=CARTESIAN_POINT('Ctrl Pts',(18.0274718595266,4.27898703140518,36.7953978564748));
#55904=CARTESIAN_POINT('Ctrl Pts',(18.0755666504899,4.27453150624796,36.7279406994618));
#55905=CARTESIAN_POINT('Ctrl Pts',(18.1213095241425,4.27029386387047,36.6637823124848));
#55906=CARTESIAN_POINT('Ctrl Pts',(18.170350220126,4.26605622149298,36.6017935179042));
#55907=CARTESIAN_POINT('Ctrl Pts',(18.2224556853443,4.26181857911549,36.542332946251));
#55908=CARTESIAN_POINT('Ctrl Pts',(18.2744862208587,4.25758703063405,36.4829578812334));
#55909=CARTESIAN_POINT('Ctrl Pts',(18.3295724668039,4.25335548215261,36.4261041686591));
#55910=CARTESIAN_POINT('Ctrl Pts',(18.3874390030781,4.24912393367117,36.372100271397));
#55911=CARTESIAN_POINT('Ctrl Pts',(18.445238701905,4.24489727274507,36.3181587501275));
#55912=CARTESIAN_POINT('Ctrl Pts',(18.5058119683969,4.24067061181897,36.2670608211206));
#55913=CARTESIAN_POINT('Ctrl Pts',(18.5688451884037,4.23644395089287,36.2190995916464));
#55914=CARTESIAN_POINT('Ctrl Pts',(18.6318386198778,4.23221995796685,36.1711686367948));
#55915=CARTESIAN_POINT('Ctrl Pts',(18.6972885506477,4.22799596504084,36.1263707345436));
#55916=CARTESIAN_POINT('Ctrl Pts',(18.7648477369498,4.22377197211483,36.0849592242384));
#55917=CARTESIAN_POINT('Ctrl Pts',(18.83238531292,4.21954933032837,36.0435609603402));
#55918=CARTESIAN_POINT('Ctrl Pts',(18.9020304052379,4.21532668854191,36.0055471821441));
#55919=CARTESIAN_POINT('Ctrl Pts',(18.9734074409312,4.21110404675546,35.9711274912376));
#55920=CARTESIAN_POINT('Ctrl Pts',(19.0447838683725,4.20688144095298,35.9367080936444));
#55921=CARTESIAN_POINT('Ctrl Pts',(19.1178917869802,4.20265883515051,35.9058829247715));
#55922=CARTESIAN_POINT('Ctrl Pts',(19.1923330681351,4.19843622934803,35.8788146029492));
#55923=CARTESIAN_POINT('Ctrl Pts',(19.2668483715896,4.19420942470606,35.851719365155));
#55924=CARTESIAN_POINT('Ctrl Pts',(19.3426992444218,4.18998262006408,35.8283885970594));
#55925=CARTESIAN_POINT('Ctrl Pts',(19.4194702845906,4.1857558154221,35.8089356860999));
#55926=CARTESIAN_POINT('Ctrl Pts',(19.4962785266604,4.18152696254465,35.7894733486005));
#55927=CARTESIAN_POINT('Ctrl Pts',(19.5740073641273,4.1772981096672,35.7738927039572));
#55928=CARTESIAN_POINT('Ctrl Pts',(19.6522315425966,4.17306925678975,35.7622558863436));
#55929=CARTESIAN_POINT('Ctrl Pts',(19.7305963070566,4.16883280373698,35.7505981548186));
#55930=CARTESIAN_POINT('Ctrl Pts',(19.8094577236358,4.1645963506842,35.7428984583384));
#55931=CARTESIAN_POINT('Ctrl Pts',(19.8883859925219,4.16035989763142,35.7391669363899));
#55932=CARTESIAN_POINT('Ctrl Pts',(19.9601217210574,4.15650950219724,35.7357754589218));
#55933=CARTESIAN_POINT('Ctrl Pts',(20.0319123932756,4.15265910676306,35.7356612213296));
#55934=CARTESIAN_POINT('Ctrl Pts',(20.1034386272148,4.14880871132888,35.738794610522));
#55935=CARTESIAN_POINT('Ctrl Pts',(20.1821584899466,4.1445710689514,35.7422431349798));
#55936=CARTESIAN_POINT('Ctrl Pts',(20.2608534738069,4.14033342657392,35.7496390819302));
#55937=CARTESIAN_POINT('Ctrl Pts',(20.3390958761865,4.13609578419645,35.760982166025));
#55938=CARTESIAN_POINT('Ctrl Pts',(20.4172257629209,4.13186423571501,35.7723089383196));
#55939=CARTESIAN_POINT('Ctrl Pts',(20.4949039005721,4.12763268723357,35.787571508773));
#55940=CARTESIAN_POINT('Ctrl Pts',(20.5717048313383,4.12340113875213,35.8067176303986));
#55941=CARTESIAN_POINT('Ctrl Pts',(20.6484170549086,4.11917447782605,35.8258416377251));
#55942=CARTESIAN_POINT('Ctrl Pts',(20.7242536325234,4.11494781689996,35.8488401693719));
#55943=CARTESIAN_POINT('Ctrl Pts',(20.7987979746695,4.11072115597388,35.8756096932948));
#55944=CARTESIAN_POINT('Ctrl Pts',(20.8732952621039,4.10649716304788,35.9023623194601));
#55945=CARTESIAN_POINT('Ctrl Pts',(20.9465014931087,4.10227317012188,35.9328810551143));
#55946=CARTESIAN_POINT('Ctrl Pts',(21.0180151323997,4.09804917719588,35.9670125103261));
#55947=CARTESIAN_POINT('Ctrl Pts',(21.0895058964376,4.09382653540944,36.001133047821));
#55948=CARTESIAN_POINT('Ctrl Pts',(21.1593047211482,4.089603893623,36.0388638082917));
#55949=CARTESIAN_POINT('Ctrl Pts',(21.2270313408399,4.08538125183656,36.0800038293361));
#55950=CARTESIAN_POINT('Ctrl Pts',(21.2947573833875,4.0811586460341,36.1211434997988));
#55951=CARTESIAN_POINT('Ctrl Pts',(21.3604108561213,4.07693604023163,36.1656921284776));
#55952=CARTESIAN_POINT('Ctrl Pts',(21.4236386282416,4.07271343442917,36.2134042571133));
#55953=CARTESIAN_POINT('Ctrl Pts',(21.4869292722659,4.0684866297872,36.261163829337));
#55954=CARTESIAN_POINT('Ctrl Pts',(21.5477890225405,4.06425982514524,36.3120929020342));
#55955=CARTESIAN_POINT('Ctrl Pts',(21.6058966439289,4.06003302050328,36.3659047287078));
#55956=CARTESIAN_POINT('Ctrl Pts',(21.6640324232525,4.05580416762584,36.4197426316498));
#55957=CARTESIAN_POINT('Ctrl Pts',(21.7194130890371,4.05157531474841,36.4764657355728));
#55958=CARTESIAN_POINT('Ctrl Pts',(21.7717550378619,4.04734646187097,36.5357511301871));
#55959=CARTESIAN_POINT('Ctrl Pts',(21.8241910566387,4.04311000881822,36.5951430736471));
#55960=CARTESIAN_POINT('Ctrl Pts',(21.8735771534998,4.03887355576546,36.657106141579));
#55961=CARTESIAN_POINT('Ctrl Pts',(21.9196708674492,4.0346371027127,36.7212853081341));
#55962=CARTESIAN_POINT('Ctrl Pts',(21.961564173838,4.0307867072784,36.7796159840094));
#55963=CARTESIAN_POINT('Ctrl Pts',(22.0007382177158,4.0269363118441,36.8397766684666));
#55964=CARTESIAN_POINT('Ctrl Pts',(22.0370439895952,4.0230859164098,36.901483322872));
#55965=CARTESIAN_POINT('Ctrl Pts',(22.077001152461,4.01884827403225,36.9693960186319));
#55966=CARTESIAN_POINT('Ctrl Pts',(22.1136334080881,4.01461063165471,37.0394365666303));
#55967=CARTESIAN_POINT('Ctrl Pts',(22.1467081821194,4.01037298927716,37.1112460256861));
#55968=CARTESIAN_POINT('Ctrl Pts',(22.1797353933276,4.00614144079566,37.1829522199216));
#55969=CARTESIAN_POINT('Ctrl Pts',(22.2092150879509,4.00190989231416,37.2564218512728));
#55970=CARTESIAN_POINT('Ctrl Pts',(22.2349595024946,3.99767834383266,37.3312695770889));
#55971=CARTESIAN_POINT('Ctrl Pts',(22.2606741815285,3.9934516829065,37.4060308517147));
#55972=CARTESIAN_POINT('Ctrl Pts',(22.2826620024857,3.98922502198035,37.4821666165824));
#55973=CARTESIAN_POINT('Ctrl Pts',(22.3007830505684,3.98499836105419,37.5592710520814));
#55974=CARTESIAN_POINT('Ctrl Pts',(22.3188926600809,3.98077436812812,37.6363268168581));
#55975=CARTESIAN_POINT('Ctrl Pts',(22.3331402345238,3.97655037520206,37.7143495834492));
#55976=CARTESIAN_POINT('Ctrl Pts',(22.3434358778168,3.97232638227599,37.7929190213299));
#55977=CARTESIAN_POINT('Ctrl Pts',(22.3537282278157,3.96810374048948,37.8714633270011));
#55978=CARTESIAN_POINT('Ctrl Pts',(22.3600710960833,3.96388109870296,37.9505534922494));
#55979=CARTESIAN_POINT('Ctrl Pts',(22.3624260713381,3.95965845691644,38.0297611335359));
#55980=CARTESIAN_POINT('Ctrl Pts',(22.3647810265245,3.95543585111392,38.1089680998404));
#55981=CARTESIAN_POINT('Ctrl Pts',(22.3631481437654,3.95121324531139,38.1882920715844));
#55982=CARTESIAN_POINT('Ctrl Pts',(22.3575411083972,3.94699063950886,38.2673032071336));
#55983=CARTESIAN_POINT('Ctrl Pts',(22.3519284975521,3.94276383486683,38.3463929091162));
#55984=CARTESIAN_POINT('Ctrl Pts',(22.3423338736503,3.9385370302248,38.4251686848449));
#55985=CARTESIAN_POINT('Ctrl Pts',(22.328822919336,3.93431022558277,38.5032049742689));
#55986=CARTESIAN_POINT('Ctrl Pts',(22.31530541785,3.93008137270527,38.5812790787115));
#55987=CARTESIAN_POINT('Ctrl Pts',(22.2978679085859,3.92585251982777,38.6586125251126));
#55988=CARTESIAN_POINT('Ctrl Pts',(22.276626895101,3.92162366695026,38.7347916362105));
#55989=CARTESIAN_POINT('Ctrl Pts',(22.2553477068602,3.91738721389744,38.8111076578648));
#55990=CARTESIAN_POINT('Ctrl Pts',(22.2302515047706,3.91315076084461,38.8862647532822));
#55991=CARTESIAN_POINT('Ctrl Pts',(22.2015041283749,3.90891430779179,38.9598662766083));
#55992=CARTESIAN_POINT('Ctrl Pts',(22.1753764301744,3.9050639123581,39.026760672886));
#55993=CARTESIAN_POINT('Ctrl Pts',(22.1462334058879,3.90121351692441,39.0923701066734));
#55994=CARTESIAN_POINT('Ctrl Pts',(22.1142322151604,3.89736312149072,39.1564149664209));
#55995=CARTESIAN_POINT('Ctrl Pts',(22.0790125593376,3.89312547911326,39.2269010285406));
#55996=CARTESIAN_POINT('Ctrl Pts',(22.040198052094,3.88888783673581,39.2957561993228));
#55997=CARTESIAN_POINT('Ctrl Pts',(21.997963199066,3.88465019435835,39.3625899952391));
#55998=CARTESIAN_POINT('Ctrl Pts',(21.9557890814143,3.88041864587694,39.429327681534));
#55999=CARTESIAN_POINT('Ctrl Pts',(21.9102046341999,3.87618709739552,39.4940493726268));
#56000=CARTESIAN_POINT('Ctrl Pts',(21.8614309025415,3.8719555489141,39.5563878041111));
#56001=CARTESIAN_POINT('Ctrl Pts',(21.8127135058901,3.86772888798804,39.6186542329856));
#56002=CARTESIAN_POINT('Ctrl Pts',(21.7608144326559,3.86350222706197,39.6785425052902));
#56003=CARTESIAN_POINT('Ctrl Pts',(21.7059979511609,3.8592755661359,39.7357143490031));
#56004=CARTESIAN_POINT('Ctrl Pts',(21.6512160715373,3.85505157320992,39.7928501040667));
#56005=CARTESIAN_POINT('Ctrl Pts',(21.593520762525,3.85082758028395,39.8472724965332));
#56006=CARTESIAN_POINT('Ctrl Pts',(21.5332156921468,3.84660358735797,39.8986773146551));
#56007=CARTESIAN_POINT('Ctrl Pts',(21.4729299117075,3.84238094557154,39.9500656897848));
#56008=CARTESIAN_POINT('Ctrl Pts',(21.4100363841272,3.83815830378511,39.998438103464));
#56009=CARTESIAN_POINT('Ctrl Pts',(21.3448735578467,3.83393566199869,40.0435291493324));
#56010=CARTESIAN_POINT('Ctrl Pts',(21.2797112868624,3.82971305619623,40.0886198109498));
#56011=CARTESIAN_POINT('Ctrl Pts',(21.2122801419229,3.82549045039378,40.1304288947869));
#56012=CARTESIAN_POINT('Ctrl Pts',(21.1429481526579,3.82126784459132,40.1687339029551));
#56013=CARTESIAN_POINT('Ctrl Pts',(21.0735472216284,3.81704103994938,40.2070770005374));
#56014=CARTESIAN_POINT('Ctrl Pts',(21.0022420819679,3.81281423530743,40.2419088352182));
#56015=CARTESIAN_POINT('Ctrl Pts',(20.9294254756064,3.80858743066548,40.2730528585825));
#56016=CARTESIAN_POINT('Ctrl Pts',(20.8565735835934,3.80435857778806,40.3042119737949));
#56017=CARTESIAN_POINT('Ctrl Pts',(20.7822092060908,3.80012972491065,40.33167955505));
#56018=CARTESIAN_POINT('Ctrl Pts',(20.706742780571,3.79590087203323,40.3553281541742));
#56019=CARTESIAN_POINT('Ctrl Pts',(20.6311407253468,3.79166441898049,40.3790192550134));
#56020=CARTESIAN_POINT('Ctrl Pts',(20.5544331195204,3.78742796592774,40.3988775419244));
#56021=CARTESIAN_POINT('Ctrl Pts',(20.4770429687982,3.783191512875,40.4148262238925));
#56022=CARTESIAN_POINT('Ctrl Pts',(20.40670519347,3.77934111744054,40.4293215414307));
#56023=CARTESIAN_POINT('Ctrl Pts',(20.3358039824011,3.77549072200609,40.4405879489081));
#56024=CARTESIAN_POINT('Ctrl Pts',(20.2646594402364,3.77164032657164,40.4486050799557));
#56025=CARTESIAN_POINT('Ctrl Pts',(20.1863596572844,3.76740268419425,40.4574285202623));
#56026=CARTESIAN_POINT('Ctrl Pts',(20.1074711708587,3.76316504181687,40.462348604127));
#56027=CARTESIAN_POINT('Ctrl Pts',(20.0284165345531,3.75892739943948,40.4632991646137));
#56028=CARTESIAN_POINT('Ctrl Pts',(19.9494755819169,3.75469585095813,40.4642483581572));
#56029=CARTESIAN_POINT('Ctrl Pts',(19.8703694187606,3.75046430247677,40.4612393589484));
#56030=CARTESIAN_POINT('Ctrl Pts',(19.7915264540029,3.74623275399542,40.4542576795074));
#56031=CARTESIAN_POINT('Ctrl Pts',(19.7127745550468,3.74200609306943,40.4472840640989));
#56032=CARTESIAN_POINT('Ctrl Pts',(19.6342857149448,3.73777943214344,40.4363469282115));
#56033=CARTESIAN_POINT('Ctrl Pts',(19.5564875497691,3.73355277121744,40.4214838244946));
#56034=CARTESIAN_POINT('Ctrl Pts',(19.4787384932196,3.72932877829153,40.406630102832));
#56035=CARTESIAN_POINT('Ctrl Pts',(19.4016797054743,3.72510478536563,40.3878554200163));
#56036=CARTESIAN_POINT('Ctrl Pts',(19.3257316772024,3.72088079243972,40.3652489200465));
#56037=CARTESIAN_POINT('Ctrl Pts',(19.2498079426231,3.71665815065337,40.3426496512764));
#56038=CARTESIAN_POINT('Ctrl Pts',(19.1749947109268,3.71243550886702,40.3162211329756));
#56039=CARTESIAN_POINT('Ctrl Pts',(19.1016988524184,3.70821286708068,40.2861028084593));
#56040=CARTESIAN_POINT('Ctrl Pts',(19.0284036185131,3.70399026127829,40.2559847406015));
#56041=CARTESIAN_POINT('Ctrl Pts',(18.9566261651361,3.69976765547591,40.2221771085391));
#56042=CARTESIAN_POINT('Ctrl Pts',(18.8867534701583,3.69554504967352,40.1848675268936));
#56043=CARTESIAN_POINT('Ctrl Pts',(18.8168112957537,3.69131824503165,40.147520845658));
#56044=CARTESIAN_POINT('Ctrl Pts',(18.7487780775739,3.68709144038978,40.1066654803662));
#56045=CARTESIAN_POINT('Ctrl Pts',(18.6830156997487,3.68286463574791,40.0625347879189));
#56046=CARTESIAN_POINT('Ctrl Pts',(18.6172214546275,3.67863578287057,40.0183827105111));
#56047=CARTESIAN_POINT('Ctrl Pts',(18.5537006181006,3.67440692999322,39.9709524249533));
#56048=CARTESIAN_POINT('Ctrl Pts',(18.4927835180097,3.67017807711588,39.9205188593686));
#56049=CARTESIAN_POINT('Ctrl Pts',(18.4317569365406,3.66594162406321,39.8699946536146));
#56050=CARTESIAN_POINT('Ctrl Pts',(18.3733437879723,3.66170517101055,39.81645670049));
#56051=CARTESIAN_POINT('Ctrl Pts',(18.3178387468338,3.65746871795788,39.7602180456935));
#56052=CARTESIAN_POINT('Ctrl Pts',(18.2673917445024,3.65361832252277,39.7091042821246));
#56053=CARTESIAN_POINT('Ctrl Pts',(18.2193466720729,3.64976792708767,39.6557602601024));
#56054=CARTESIAN_POINT('Ctrl Pts',(18.1738948585642,3.64591753165256,39.6004434189005));
#56055=CARTESIAN_POINT('Ctrl Pts',(18.1241097958789,3.64170005025189,39.5398528242862));
#56056=CARTESIAN_POINT('Ctrl Pts',(18.0772440232761,3.63748256885122,39.4766604032495));
#56057=CARTESIAN_POINT('Ctrl Pts',(18.0335827029836,3.63326508745055,39.4111801763659));
#56058=CARTESIAN_POINT('Ctrl Pts',(17.9899812417688,3.62905338815965,39.3457897219848));
#56059=CARTESIAN_POINT('Ctrl Pts',(17.9495757753076,3.62484168886876,39.2781180754439));
#56060=CARTESIAN_POINT('Ctrl Pts',(17.9126116513043,3.62062998957786,39.2085126623677));
#56061=CARTESIAN_POINT('Ctrl Pts',(17.8756864262643,3.61642272244221,39.1389804981099));
#56062=CARTESIAN_POINT('Ctrl Pts',(17.8421955755532,3.61221545530655,39.0675190224678));
#56063=CARTESIAN_POINT('Ctrl Pts',(17.8123406269042,3.6080081881709,38.9945037217397));
#56064=CARTESIAN_POINT('Ctrl Pts',(17.7825040763327,3.60380351375873,38.9215334166059));
#56065=CARTESIAN_POINT('Ctrl Pts',(17.7562991624995,3.59959883934656,38.8470116224974));
#56066=CARTESIAN_POINT('Ctrl Pts',(17.7338803767706,3.59539416493439,38.7713362005097));
#56067=CARTESIAN_POINT('Ctrl Pts',(17.7114705086883,3.59119116303922,38.6956908803603));
#56068=CARTESIAN_POINT('Ctrl Pts',(17.6928439091955,3.58698816114405,38.6188932980639));
#56069=CARTESIAN_POINT('Ctrl Pts',(17.6781054904817,3.58278515924888,38.5413573694509));
#56070=CARTESIAN_POINT('Ctrl Pts',(17.6633617670978,3.57858064460402,38.4637935340098));
#56071=CARTESIAN_POINT('Ctrl Pts',(17.6525091147608,3.57437612995915,38.385491285794));
#56072=CARTESIAN_POINT('Ctrl Pts',(17.6456012848616,3.57017161531429,38.3068746747539));
#56073=CARTESIAN_POINT('Ctrl Pts',(17.6394978340523,3.56645669345229,38.2374125389932));
#56074=CARTESIAN_POINT('Ctrl Pts',(17.6364732593455,3.56274177159029,38.1677053393348));
#56075=CARTESIAN_POINT('Ctrl Pts',(17.636530806543,3.55902684972829,38.0980474427862));
#56076=CARTESIAN_POINT('',(17.6365300009389,2.76527684969598,38.1000666180705));
#56077=CARTESIAN_POINT('Ctrl Pts',(17.6365308065437,3.55902684968247,38.098047441927));
#56078=CARTESIAN_POINT('Ctrl Pts',(17.6366087562975,3.55399485629477,38.0036933510878));
#56079=CARTESIAN_POINT('Ctrl Pts',(17.6423407577314,3.54896286290708,37.9095808518187));
#56080=CARTESIAN_POINT('Ctrl Pts',(17.6536172651267,3.54393086951938,37.8163126679098));
#56081=CARTESIAN_POINT('Ctrl Pts',(17.6650358770517,3.53883546385085,37.7218691350258));
#56082=CARTESIAN_POINT('Ctrl Pts',(17.6821395347456,3.53374005818232,37.6282913753209));
#56083=CARTESIAN_POINT('Ctrl Pts',(17.7047654113372,3.5286446525138,37.5361838740284));
#56084=CARTESIAN_POINT('Ctrl Pts',(17.7172725445006,3.52582801392036,37.4852686849811));
#56085=CARTESIAN_POINT('Ctrl Pts',(17.7314662234869,3.52301137532692,37.4348023773383));
#56086=CARTESIAN_POINT('Ctrl Pts',(17.7473127371145,3.52019473673349,37.3848842495559));
#56087=CARTESIAN_POINT('Ctrl Pts',(17.7711538709519,3.51595709435636,37.3097822559346));
#56088=CARTESIAN_POINT('Ctrl Pts',(17.7987995848625,3.51171945197924,37.2357328466356));
#56089=CARTESIAN_POINT('Ctrl Pts',(17.8301381585128,3.50748180960211,37.16314887535));
#56090=CARTESIAN_POINT('Ctrl Pts',(17.8614316660644,3.50325026112103,37.0906692826637));
#56091=CARTESIAN_POINT('Ctrl Pts',(17.8964073029588,3.49901871263994,37.0196513697913));
#56092=CARTESIAN_POINT('Ctrl Pts',(17.9349037671089,3.49478716415886,36.950492283715));
#56093=CARTESIAN_POINT('Ctrl Pts',(17.9733557667798,3.49056050323311,36.8814130782928));
#56094=CARTESIAN_POINT('Ctrl Pts',(18.0153202854038,3.48633384230737,36.8141888405654));
#56095=CARTESIAN_POINT('Ctrl Pts',(18.0605888182041,3.48210718138163,36.7491947924201));
#56096=CARTESIAN_POINT('Ctrl Pts',(18.1058287760958,3.47788318845598,36.6842417705434));
#56097=CARTESIAN_POINT('Ctrl Pts',(18.1543683412653,3.47365919553032,36.6215165276491));
#56098=CARTESIAN_POINT('Ctrl Pts',(18.2059547959636,3.46943520260466,36.5613667601491));
#56099=CARTESIAN_POINT('Ctrl Pts',(18.2575247495691,3.46521256081856,36.501236232911));
#56100=CARTESIAN_POINT('Ctrl Pts',(18.3121393523534,3.46098991903246,36.443679900692));
#56101=CARTESIAN_POINT('Ctrl Pts',(18.369505499578,3.45676727724635,36.3890125292705));
#56102=CARTESIAN_POINT('Ctrl Pts',(18.4268711579469,3.45254467144422,36.3343456237064));
#56103=CARTESIAN_POINT('Ctrl Pts',(18.4869879737899,3.44832206564209,36.282567952349));
#56104=CARTESIAN_POINT('Ctrl Pts',(18.549526954012,3.44409945983996,36.233956489317));
#56105=CARTESIAN_POINT('Ctrl Pts',(18.6121281212232,3.43987265519832,36.1852966884241));
#56106=CARTESIAN_POINT('Ctrl Pts',(18.6771558928925,3.43564585055668,36.1398096731329));
#56107=CARTESIAN_POINT('Ctrl Pts',(18.7442497248806,3.43141904591504,36.0977308653836));
#56108=CARTESIAN_POINT('Ctrl Pts',(18.8113760693641,3.42719019303793,36.0556316669813));
#56109=CARTESIAN_POINT('Ctrl Pts',(18.8805700589422,3.42296134016082,36.0169441952786));
#56110=CARTESIAN_POINT('Ctrl Pts',(18.9514460404782,3.41873248728371,35.9818581173889));
#56111=CARTESIAN_POINT('Ctrl Pts',(19.022449401685,3.41449603423126,35.9467089821285));
#56112=CARTESIAN_POINT('Ctrl Pts',(19.0951403638434,3.41025958117881,35.9151743603576));
#56113=CARTESIAN_POINT('Ctrl Pts',(19.169112987984,3.40602312812636,35.8873958297601));
#56114=CARTESIAN_POINT('Ctrl Pts',(19.2363446676346,3.40217273268904,35.8621486887806));
#56115=CARTESIAN_POINT('Ctrl Pts',(19.3046345921318,3.39832233725172,35.840003714446));
#56116=CARTESIAN_POINT('Ctrl Pts',(19.3736697078406,3.3944719418144,35.8210307579909));
#56117=CARTESIAN_POINT('Ctrl Pts',(19.4496479123088,3.39023429943751,35.8001496288712));
#56118=CARTESIAN_POINT('Ctrl Pts',(19.526814106019,3.38599665706063,35.7830329977053));
#56119=CARTESIAN_POINT('Ctrl Pts',(19.604761146044,3.38175901468375,35.7698118768598));
#56120=CARTESIAN_POINT('Ctrl Pts',(19.6825960951665,3.37752746620291,35.756609768505));
#56121=CARTESIAN_POINT('Ctrl Pts',(19.7612092022994,3.37329591772207,35.7472921233669));
#56122=CARTESIAN_POINT('Ctrl Pts',(19.8401795112546,3.36906436924124,35.7419398115661));
#56123=CARTESIAN_POINT('Ctrl Pts',(19.919058607322,3.36483770831576,35.7365936818332));
#56124=CARTESIAN_POINT('Ctrl Pts',(19.9982936199824,3.36061104739028,35.7352038152258));
#56125=CARTESIAN_POINT('Ctrl Pts',(20.077456291198,3.3563843864648,35.7377995504501));
#56126=CARTESIAN_POINT('Ctrl Pts',(20.1565689924686,3.35216039353941,35.7403936471654));
#56127=CARTESIAN_POINT('Ctrl Pts',(20.2356089756367,3.34793640061402,35.746968336733));
#56128=CARTESIAN_POINT('Ctrl Pts',(20.3141470062023,3.34371240768863,35.7575008859353));
#56129=CARTESIAN_POINT('Ctrl Pts',(20.3926599146046,3.33948976590281,35.7680300660637));
#56130=CARTESIAN_POINT('Ctrl Pts',(20.4706707249675,3.33526712411698,35.7825145295162));
#56131=CARTESIAN_POINT('Ctrl Pts',(20.5477558431582,3.33104448233115,35.8008797384247));
#56132=CARTESIAN_POINT('Ctrl Pts',(20.6248403044547,3.3268218765293,35.8192447908309));
#56133=CARTESIAN_POINT('Ctrl Pts',(20.7009986335855,3.32259927072744,35.8414904129059));
#56134=CARTESIAN_POINT('Ctrl Pts',(20.7758194033088,3.31837666492559,35.8674913898599));
#56135=CARTESIAN_POINT('Ctrl Pts',(20.8507145726844,3.31414986028424,35.8935182214483));
#56136=CARTESIAN_POINT('Ctrl Pts',(20.9242690820816,3.30992305564289,35.9233077127991));
#56137=CARTESIAN_POINT('Ctrl Pts',(20.9960891866796,3.30569625100154,35.9566855636468));
#56138=CARTESIAN_POINT('Ctrl Pts',(21.0679440940418,3.30146739812472,35.9900795888162));
#56139=CARTESIAN_POINT('Ctrl Pts',(21.1380625071475,3.2972385452479,36.0270652185019));
#56140=CARTESIAN_POINT('Ctrl Pts',(21.2060753956977,3.29300969237108,36.0674221833365));
#56141=CARTESIAN_POINT('Ctrl Pts',(21.2742105183131,3.28877323931893,36.1078516784808));
#56142=CARTESIAN_POINT('Ctrl Pts',(21.3402321638762,3.28453678626677,36.1516643554831));
#56143=CARTESIAN_POINT('Ctrl Pts',(21.4038006004526,3.28030033321462,36.1985967510628));
#56144=CARTESIAN_POINT('Ctrl Pts',(21.4615762007705,3.27644993777486,36.2412523121402));
#56145=CARTESIAN_POINT('Ctrl Pts',(21.5173255343056,3.27259954233509,36.2864842200498));
#56146=CARTESIAN_POINT('Ctrl Pts',(21.5708195989041,3.26874914689532,36.3340678867525));
#56147=CARTESIAN_POINT('Ctrl Pts',(21.6296937376197,3.26451150451514,36.3864371994057));
#56148=CARTESIAN_POINT('Ctrl Pts',(21.6860566257664,3.26027386213496,36.4418522277241));
#56149=CARTESIAN_POINT('Ctrl Pts',(21.7395767389552,3.25603621975477,36.5000427473879));
#56150=CARTESIAN_POINT('Ctrl Pts',(21.793019888121,3.25180467127062,36.558149586801));
#56151=CARTESIAN_POINT('Ctrl Pts',(21.8436280660461,3.24757312278648,36.6190236490969));
#56152=CARTESIAN_POINT('Ctrl Pts',(21.8911042919975,3.24334157430233,36.6823558282529));
#56153=CARTESIAN_POINT('Ctrl Pts',(21.9385256815969,3.23911491337353,36.7456148569931));
#56154=CARTESIAN_POINT('Ctrl Pts',(21.9828220283333,3.23488825244474,36.8113259872177));
#56155=CARTESIAN_POINT('Ctrl Pts',(22.0237356048506,3.23066159151594,36.879145937239));
#56156=CARTESIAN_POINT('Ctrl Pts',(22.0646233554434,3.22643759858724,36.9469230771944));
#56157=CARTESIAN_POINT('Ctrl Pts',(22.1021323326594,3.22221360565854,37.0168059944153));
#56158=CARTESIAN_POINT('Ctrl Pts',(22.1360479590686,3.21798961272984,37.0884222434933));
#56159=CARTESIAN_POINT('Ctrl Pts',(22.1699527367984,3.2137669709407,37.1600155844961));
#56160=CARTESIAN_POINT('Ctrl Pts',(22.2002662457384,3.20954432915156,37.2333407329763));
#56161=CARTESIAN_POINT('Ctrl Pts',(22.226820435953,3.20532168736243,37.308001775935));
#56162=CARTESIAN_POINT('Ctrl Pts',(22.2533743998814,3.20109908155728,37.3826621826565));
#56163=CARTESIAN_POINT('Ctrl Pts',(22.2761689530424,3.19687647575212,37.4586580190729));
#56164=CARTESIAN_POINT('Ctrl Pts',(22.2950851795987,3.19265386994697,37.5355759933468));
#56165=CARTESIAN_POINT('Ctrl Pts',(22.3140202159142,3.18842706530236,37.612570452673));
#56166=CARTESIAN_POINT('Ctrl Pts',(22.3290691100442,3.18420026065775,37.6904884251957));
#56167=CARTESIAN_POINT('Ctrl Pts',(22.3401637475359,3.17997345601313,37.7689047333189));
#56168=CARTESIAN_POINT('Ctrl Pts',(22.3512637612945,3.17574460313307,37.8473590406107));
#56169=CARTESIAN_POINT('Ctrl Pts',(22.3584056589073,3.171515750253,37.9263116971043));
#56170=CARTESIAN_POINT('Ctrl Pts',(22.3615733409036,3.16728689737293,38.0053332347993));
#56171=CARTESIAN_POINT('Ctrl Pts',(22.3647467159185,3.1630504443176,38.0844967915132));
#56172=CARTESIAN_POINT('Ctrl Pts',(22.3639316086702,3.15881399126226,38.1637290069214));
#56173=CARTESIAN_POINT('Ctrl Pts',(22.3591641018022,3.15457753820693,38.2426014784904));
#56174=CARTESIAN_POINT('Ctrl Pts',(22.3548310462195,3.1507271427967,38.3142864938926));
#56175=CARTESIAN_POINT('Ctrl Pts',(22.3472338078296,3.14687674738647,38.3856741368903));
#56176=CARTESIAN_POINT('Ctrl Pts',(22.3364361322485,3.14302635197624,38.4564500537572));
#56177=CARTESIAN_POINT('Ctrl Pts',(22.3245524988267,3.13878870960212,38.5343441379816));
#56178=CARTESIAN_POINT('Ctrl Pts',(22.3087469503506,3.13455106722801,38.6117895067555));
#56179=CARTESIAN_POINT('Ctrl Pts',(22.2890657087384,3.13031342485389,38.6883609623164));
#56180=CARTESIAN_POINT('Ctrl Pts',(22.269412769524,3.1260818763758,38.7648223051195));
#56181=CARTESIAN_POINT('Ctrl Pts',(22.2458953211595,3.12185032789771,38.8404117801773));
#56182=CARTESIAN_POINT('Ctrl Pts',(22.2186110055028,3.11761877941962,38.9147120025886));
#56183=CARTESIAN_POINT('Ctrl Pts',(22.191358203984,3.11339211849684,38.9889264061917));
#56184=CARTESIAN_POINT('Ctrl Pts',(22.1603473421512,3.10916545757407,39.0618540785945));
#56185=CARTESIAN_POINT('Ctrl Pts',(22.1257260977279,3.10493879665129,39.1330919602526));
#56186=CARTESIAN_POINT('Ctrl Pts',(22.0911267073128,3.10071480372859,39.2042848743403));
#56187=CARTESIAN_POINT('Ctrl Pts',(22.0529216622112,3.09649081080588,39.2737896943469));
#56188=CARTESIAN_POINT('Ctrl Pts',(22.0113065926847,3.09226681788317,39.3412236829528));
#56189=CARTESIAN_POINT('Ctrl Pts',(21.969704834678,3.08804417609999,39.4086361012746));
#56190=CARTESIAN_POINT('Ctrl Pts',(21.9246954643149,3.08382153431681,39.4739786049584));
#56191=CARTESIAN_POINT('Ctrl Pts',(21.8765191246263,3.07959889253363,39.5368947128485));
#56192=CARTESIAN_POINT('Ctrl Pts',(21.8283431954803,3.0753762867344,39.5998102845884));
#56193=CARTESIAN_POINT('Ctrl Pts',(21.7770006367988,3.07115368093516,39.6602991303254));
#56194=CARTESIAN_POINT('Ctrl Pts',(21.7227734155927,3.06693107513593,39.7180365259867));
#56195=CARTESIAN_POINT('Ctrl Pts',(21.6684922723741,3.06270427049713,39.7758313340785));
#56196=CARTESIAN_POINT('Ctrl Pts',(21.611321058605,3.05847746585832,39.830868884503));
#56197=CARTESIAN_POINT('Ctrl Pts',(21.5515793648724,3.05425066121952,39.8828605989819));
#56198=CARTESIAN_POINT('Ctrl Pts',(21.4918087213613,3.05002180834521,39.9348775077352));
#56199=CARTESIAN_POINT('Ctrl Pts',(21.4294654856099,3.04579295547091,39.9838453503306));
#56200=CARTESIAN_POINT('Ctrl Pts',(21.3649011608889,3.0415641025966,40.0295168467531));
#56201=CARTESIAN_POINT('Ctrl Pts',(21.3002207999264,3.03732764954688,40.0752704248642));
#56202=CARTESIAN_POINT('Ctrl Pts',(21.2333117708055,3.03309119649715,40.117715567856));
#56203=CARTESIAN_POINT('Ctrl Pts',(21.1645530875906,3.02885474344742,40.1566493495692));
#56204=CARTESIAN_POINT('Ctrl Pts',(21.1020602147053,3.02500434798401,40.1920351911499));
#56205=CARTESIAN_POINT('Ctrl Pts',(21.0380399871679,3.02115395252059,40.2245209451278));
#56206=CARTESIAN_POINT('Ctrl Pts',(20.9727908051473,3.01730355705717,40.2539889717269));
#56207=CARTESIAN_POINT('Ctrl Pts',(20.9009792987033,3.01306591468266,40.286420694493));
#56208=CARTESIAN_POINT('Ctrl Pts',(20.827409367394,3.00882827230814,40.3153181980759));
#56209=CARTESIAN_POINT('Ctrl Pts',(20.7524628560726,3.00459062993362,40.3404888062945));
#56210=CARTESIAN_POINT('Ctrl Pts',(20.6776241207765,3.00035908145519,40.3656232181905));
#56211=CARTESIAN_POINT('Ctrl Pts',(20.6014131774329,2.99612753297676,40.3870412300264));
#56212=CARTESIAN_POINT('Ctrl Pts',(20.5242333066394,2.99189598449833,40.4045975529602));
#56213=CARTESIAN_POINT('Ctrl Pts',(20.4471425807292,2.9876693235753,40.4221335978558));
#56214=CARTESIAN_POINT('Ctrl Pts',(20.3690856061609,2.98344266265227,40.4358167142507));
#56215=CARTESIAN_POINT('Ctrl Pts',(20.2904808827541,2.97921600172925,40.4455513845692));
#56216=CARTESIAN_POINT('Ctrl Pts',(20.2119257770988,2.97499200880635,40.4552799100603));
#56217=CARTESIAN_POINT('Ctrl Pts',(20.1328240728952,2.97076801588344,40.461064879115));
#56218=CARTESIAN_POINT('Ctrl Pts',(20.0536033245773,2.96654402296054,40.4628620620964));
#56219=CARTESIAN_POINT('Ctrl Pts',(19.9744079168059,2.96232138117722,40.4646586702082));
#56220=CARTESIAN_POINT('Ctrl Pts',(19.8950940088524,2.9580987393939,40.4624700146794));
#56221=CARTESIAN_POINT('Ctrl Pts',(19.8160916317561,2.95387609761059,40.4563039177894));
#56222=CARTESIAN_POINT('Ctrl Pts',(19.7370899278926,2.94965349181126,40.450137873445));
#56223=CARTESIAN_POINT('Ctrl Pts',(19.6584002168479,2.94543088601194,40.4399944930337));
#56224=CARTESIAN_POINT('Ctrl Pts',(19.5804483837839,2.94120828021262,40.4259335506911));
#56225=CARTESIAN_POINT('Ctrl Pts',(19.5024190376273,2.93698147557381,40.4118586265461));
#56226=CARTESIAN_POINT('Ctrl Pts',(19.4251294974711,2.93275467093501,40.3938584425738));
#56227=CARTESIAN_POINT('Ctrl Pts',(19.3489958067916,2.9285278662962,40.3720440095485));
#56228=CARTESIAN_POINT('Ctrl Pts',(19.2728252230598,2.92429901342194,40.3502190056312));
#56229=CARTESIAN_POINT('Ctrl Pts',(19.1978120487375,2.92007016054768,40.3245762224212));
#56230=CARTESIAN_POINT('Ctrl Pts',(19.1243550547343,2.91584130767342,40.2952759213208));
#56231=CARTESIAN_POINT('Ctrl Pts',(19.0507660424153,2.91160485462381,40.2659229611582));
#56232=CARTESIAN_POINT('Ctrl Pts',(18.9787392258186,2.90736840157421,40.2328995447266));
#56233=CARTESIAN_POINT('Ctrl Pts',(18.9086511439443,2.9031319485246,40.1964131547207));
#56234=CARTESIAN_POINT('Ctrl Pts',(18.8449500172609,2.89928155306243,40.1632516800472));
#56235=CARTESIAN_POINT('Ctrl Pts',(18.782850286663,2.89543115760026,40.1272303363376));
#56236=CARTESIAN_POINT('Ctrl Pts',(18.7226130661596,2.89158076213809,40.0885354063114));
#56237=CARTESIAN_POINT('Ctrl Pts',(18.6563175902903,2.88734311974163,40.0459487999178));
#56238=CARTESIAN_POINT('Ctrl Pts',(18.5920296832405,2.88310547734517,39.9999633067943));
#56239=CARTESIAN_POINT('Ctrl Pts',(18.530118826536,2.87886783494872,39.950794363725));
#56240=CARTESIAN_POINT('Ctrl Pts',(18.4682970000719,2.87463628644825,39.9016961275245));
#56241=CARTESIAN_POINT('Ctrl Pts',(18.4088457995984,2.87040473794778,39.8494238218444));
#56242=CARTESIAN_POINT('Ctrl Pts',(18.3521066231758,2.86617318944731,39.7942366598321));
#56243=CARTESIAN_POINT('Ctrl Pts',(18.2954329820687,2.8619465285022,39.7391132405158));
#56244=CARTESIAN_POINT('Ctrl Pts',(18.2414654743572,2.85771986755709,39.6810819806166));
#56245=CARTESIAN_POINT('Ctrl Pts',(18.1905120309623,2.85349320661199,39.6204419524624));
#56246=CARTESIAN_POINT('Ctrl Pts',(18.1395907509687,2.84926921366698,39.5598402021837));
#56247=CARTESIAN_POINT('Ctrl Pts',(18.091680059675,2.84504522072198,39.4966333101958));
#56248=CARTESIAN_POINT('Ctrl Pts',(18.047049792961,2.84082122777698,39.4311558622965));
#56249=CARTESIAN_POINT('Ctrl Pts',(18.0024338022463,2.83659858597157,39.3656993588386));
#56250=CARTESIAN_POINT('Ctrl Pts',(17.9610964162059,2.83237594416617,39.2979741288062));
#56251=CARTESIAN_POINT('Ctrl Pts',(17.9232651541579,2.82815330236077,39.228345169248));
#56252=CARTESIAN_POINT('Ctrl Pts',(17.8854342144962,2.8239306965394,39.1587168030461));
#56253=CARTESIAN_POINT('Ctrl Pts',(17.8511095619611,2.81970809071804,39.0871851521587));
#56254=CARTESIAN_POINT('Ctrl Pts',(17.8204728783943,2.81548548489668,39.0141400150334));
#56255=CARTESIAN_POINT('Ctrl Pts',(17.7898057305799,2.81125868023606,38.9410222438991));
#56256=CARTESIAN_POINT('Ctrl Pts',(17.7628340587385,2.80703187557543,38.8663884136422));
#56257=CARTESIAN_POINT('Ctrl Pts',(17.7396912067772,2.80280507091481,38.7906479567622));
#56258=CARTESIAN_POINT('Ctrl Pts',(17.716537140196,2.79857621801882,38.714870797386));
#56259=CARTESIAN_POINT('Ctrl Pts',(17.6972157040253,2.79434736512283,38.637986398329));
#56260=CARTESIAN_POINT('Ctrl Pts',(17.6818095253449,2.79011851222684,38.5604165115612));
#56261=CARTESIAN_POINT('Ctrl Pts',(17.6663756583868,2.78588205915591,38.482707214716));
#56262=CARTESIAN_POINT('Ctrl Pts',(17.6548711769025,2.78164560608498,38.4043104334678));
#56263=CARTESIAN_POINT('Ctrl Pts',(17.6473269939418,2.77740915301404,38.3256549743858));
#56264=CARTESIAN_POINT('Ctrl Pts',(17.6404702942772,2.77355875774903,38.2541671986106));
#56265=CARTESIAN_POINT('Ctrl Pts',(17.6368843425059,2.76970836248401,38.1824660538048));
#56266=CARTESIAN_POINT('Ctrl Pts',(17.6365550057291,2.765857967219,38.1108719802996));
#56267=CARTESIAN_POINT('Ctrl Pts',(17.6365384374421,2.76566426138876,38.107270222949));
#56268=CARTESIAN_POINT('Ctrl Pts',(17.6365301024624,2.76547055555852,38.1036684276956));
#56269=CARTESIAN_POINT('Ctrl Pts',(17.6365300009389,2.76527684972828,38.1000666186711));
#56270=CARTESIAN_POINT('',(17.6365307642293,1.97152684977754,38.1019006486528));
#56271=CARTESIAN_POINT('Ctrl Pts',(17.6365300009389,2.76527684969598,38.1000666180705));
#56272=CARTESIAN_POINT('Ctrl Pts',(17.6365277817899,2.7610426970283,38.0213358474423));
#56273=CARTESIAN_POINT('Ctrl Pts',(17.6404638294913,2.75680854436061,37.9424559890261));
#56274=CARTESIAN_POINT('Ctrl Pts',(17.6483568759924,2.75257439169293,37.8638537355627));
#56275=CARTESIAN_POINT('Ctrl Pts',(17.656238569863,2.74834632904014,37.7853645363352));
#56276=CARTESIAN_POINT('Ctrl Pts',(17.6680659139453,2.74411826638735,37.7071526125758));
#56277=CARTESIAN_POINT('Ctrl Pts',(17.6838056298472,2.73989020373455,37.6296447294093));
#56278=CARTESIAN_POINT('Ctrl Pts',(17.6995272028678,2.73566701469187,37.5522261881552));
#56279=CARTESIAN_POINT('Ctrl Pts',(17.7191520931642,2.73144382564918,37.4755105327649));
#56280=CARTESIAN_POINT('Ctrl Pts',(17.7425953940227,2.72722063660649,37.3999179435147));
#56281=CARTESIAN_POINT('Ctrl Pts',(17.7660239611144,2.72300010177547,37.3243728630856));
#56282=CARTESIAN_POINT('Ctrl Pts',(17.7932660368616,2.71877956694445,37.2499498952732));
#56283=CARTESIAN_POINT('Ctrl Pts',(17.8241862410376,2.71455903211343,37.1770563791814));
#56284=CARTESIAN_POINT('Ctrl Pts',(17.8550966835537,2.71033982972592,37.1041858759295));
#56285=CARTESIAN_POINT('Ctrl Pts',(17.8896827653708,2.70612062733841,37.032844297629));
#56286=CARTESIAN_POINT('Ctrl Pts',(17.9277606465776,2.7019014249509,36.963419821118));
#56287=CARTESIAN_POINT('Ctrl Pts',(17.9658384161765,2.69768223493006,36.893995548093));
#56288=CARTESIAN_POINT('Ctrl Pts',(18.0074077376034,2.69346304490922,36.8264887767218));
#56289=CARTESIAN_POINT('Ctrl Pts',(18.0522391338228,2.68924385488838,36.7612625167388));
#56290=CARTESIAN_POINT('Ctrl Pts',(18.0971152043896,2.68502046045775,36.6959712589898));
#56291=CARTESIAN_POINT('Ctrl Pts',(18.1452595758028,2.68079706602713,36.6329654395846));
#56292=CARTESIAN_POINT('Ctrl Pts',(18.1964001430807,2.67657367159651,36.5725779898729));
#56293=CARTESIAN_POINT('Ctrl Pts',(18.2475658828021,2.67234819832392,36.5121608162112));
#56294=CARTESIAN_POINT('Ctrl Pts',(18.3017304344297,2.66812272505133,36.4543649224505));
#56295=CARTESIAN_POINT('Ctrl Pts',(18.358583940748,2.66389725177874,36.3994872063611));
#56296=CARTESIAN_POINT('Ctrl Pts',(18.4155388995487,2.6596642383423,36.3445115634966));
#56297=CARTESIAN_POINT('Ctrl Pts',(18.4751920449262,2.65543122490587,36.2924648114215));
#56298=CARTESIAN_POINT('Ctrl Pts',(18.5371996944003,2.65119821146943,36.2436041082686));
#56299=CARTESIAN_POINT('Ctrl Pts',(18.5912189776084,2.64751053174626,36.2010380670825));
#56300=CARTESIAN_POINT('Ctrl Pts',(18.6470245249846,2.6438228520231,36.1608894951088));
#56301=CARTESIAN_POINT('Ctrl Pts',(18.704372763647,2.64013517229993,36.1233006031972));
#56302=CARTESIAN_POINT('Ctrl Pts',(18.7702736401,2.63589752993283,36.0801058865043));
#56303=CARTESIAN_POINT('Ctrl Pts',(18.8384606739486,2.63165988756574,36.040129282216));
#56304=CARTESIAN_POINT('Ctrl Pts',(18.9085865914612,2.62742224519864,36.0036204512156));
#56305=CARTESIAN_POINT('Ctrl Pts',(18.9786116651466,2.62319069672792,35.9671641213499));
#56306=CARTESIAN_POINT('Ctrl Pts',(19.0505696730441,2.6189591482572,35.934165876144));
#56307=CARTESIAN_POINT('Ctrl Pts',(19.124084803758,2.61472759978647,35.9048318948444));
#56308=CARTESIAN_POINT('Ctrl Pts',(19.1975150224579,2.61050093887155,35.8755317951065));
#56309=CARTESIAN_POINT('Ctrl Pts',(19.272498356674,2.60627427795662,35.8498877214283));
#56310=CARTESIAN_POINT('Ctrl Pts',(19.3486362280133,2.6020476170417,35.8280590506258));
#56311=CARTESIAN_POINT('Ctrl Pts',(19.4247260387507,2.59782362412713,35.806244158762));
#56312=CARTESIAN_POINT('Ctrl Pts',(19.5019684906233,2.59359963121257,35.7882400182171));
#56313=CARTESIAN_POINT('Ctrl Pts',(19.5799480923609,2.589375638298,35.7741567473734));
#56314=CARTESIAN_POINT('Ctrl Pts',(19.6579027505566,2.58515299652323,35.7600779813828));
#56315=CARTESIAN_POINT('Ctrl Pts',(19.7365936293992,2.58093035474847,35.7499176777952));
#56316=CARTESIAN_POINT('Ctrl Pts',(19.8155947041848,2.57670771297371,35.7437349198837));
#56317=CARTESIAN_POINT('Ctrl Pts',(19.8945951057447,2.57248510718315,35.7375522146601));
#56318=CARTESIAN_POINT('Ctrl Pts',(19.9739052305367,2.56826250139259,35.7353470228679));
#56319=CARTESIAN_POINT('Ctrl Pts',(20.053095078038,2.56403989560204,35.7371264626332));
#56320=CARTESIAN_POINT('Ctrl Pts',(20.1323636696737,2.55981309097225,35.7389076718229));
#56321=CARTESIAN_POINT('Ctrl Pts',(20.211511275372,2.55558628634247,35.744681416536));
#56322=CARTESIAN_POINT('Ctrl Pts',(20.290109656557,2.55135948171269,35.7544026713708));
#56323=CARTESIAN_POINT('Ctrl Pts',(20.3687461251371,2.54713062884761,35.764128636955));
#56324=CARTESIAN_POINT('Ctrl Pts',(20.4468323766782,2.54290177598254,35.7778058423894));
#56325=CARTESIAN_POINT('Ctrl Pts',(20.5239495837537,2.53867292311746,35.7953379261627));
#56326=CARTESIAN_POINT('Ctrl Pts',(20.6012053873477,2.53443647007719,35.8129015189319));
#56327=CARTESIAN_POINT('Ctrl Pts',(20.6774882142496,2.53020001703692,35.8343337058813));
#56328=CARTESIAN_POINT('Ctrl Pts',(20.7523938625888,2.52596356399665,35.8594880235895));
#56329=CARTESIAN_POINT('Ctrl Pts',(20.8204735442091,2.52211316845805,35.8823500904553));
#56330=CARTESIAN_POINT('Ctrl Pts',(20.8874155900921,2.51826277291945,35.908286097158));
#56331=CARTESIAN_POINT('Ctrl Pts',(20.9529331154744,2.51441237738085,35.9371525901413));
#56332=CARTESIAN_POINT('Ctrl Pts',(21.0250399543103,2.51017473487319,35.9689222814592));
#56333=CARTESIAN_POINT('Ctrl Pts',(21.0956916594874,2.50593709236553,36.0043614892623));
#56334=CARTESIAN_POINT('Ctrl Pts',(21.1644897651357,2.50169944985788,36.0433147961357));
#56335=CARTESIAN_POINT('Ctrl Pts',(21.2331889364188,2.49746790124579,36.0822120866312));
#56336=CARTESIAN_POINT('Ctrl Pts',(21.3000393971506,2.49323635263371,36.1246132115312));
#56337=CARTESIAN_POINT('Ctrl Pts',(21.3646636227348,2.48900480402162,36.1703151455006));
#56338=CARTESIAN_POINT('Ctrl Pts',(21.4292132055571,2.48477814296483,36.2159642924765));
#56339=CARTESIAN_POINT('Ctrl Pts',(21.491541282378,2.48055148190803,36.2649064027758));
#56340=CARTESIAN_POINT('Ctrl Pts',(21.5512971967595,2.47632482085123,36.3168938763422));
#56341=CARTESIAN_POINT('Ctrl Pts',(21.6110153913467,2.47210082779454,36.3688485337961));
#56342=CARTESIAN_POINT('Ctrl Pts',(21.6681642934807,2.46787683473784,36.423844432027));
#56343=CARTESIAN_POINT('Ctrl Pts',(21.7224253617482,2.46365284168114,36.4815929701998));
#56344=CARTESIAN_POINT('Ctrl Pts',(21.7766690733852,2.45943019976421,36.5393230361959));
#56345=CARTESIAN_POINT('Ctrl Pts',(21.8280264647536,2.45520755784727,36.5998036522649));
#56346=CARTESIAN_POINT('Ctrl Pts',(21.8762160724176,2.45098491593033,36.6627096011933));
#56347=CARTESIAN_POINT('Ctrl Pts',(21.9244052694213,2.44676230999774,36.7256150140523));
#56348=CARTESIAN_POINT('Ctrl Pts',(21.9694264524563,2.44253970406515,36.7909453456766));
#56349=CARTESIAN_POINT('Ctrl Pts',(22.0110395857854,2.43831709813256,36.8583437571919));
#56350=CARTESIAN_POINT('Ctrl Pts',(22.0526940980185,2.43409029336196,36.925809187751));
#56351=CARTESIAN_POINT('Ctrl Pts',(22.090933544425,2.42986348859136,36.9953464061484));
#56352=CARTESIAN_POINT('Ctrl Pts',(22.1255625898733,2.42563668382077,37.0665716679754));
#56353=CARTESIAN_POINT('Ctrl Pts',(22.1602084159447,2.42140783081532,37.1378314443048));
#56354=CARTESIAN_POINT('Ctrl Pts',(22.1912401720431,2.41717897780988,37.2107804616895));
#56355=CARTESIAN_POINT('Ctrl Pts',(22.2185107100584,2.41295012480443,37.28501492636));
#56356=CARTESIAN_POINT('Ctrl Pts',(22.2458302591889,2.40871367162619,37.3593828065828));
#56357=CARTESIAN_POINT('Ctrl Pts',(22.2693749440146,2.40447721844794,37.4350403014924));
#56358=CARTESIAN_POINT('Ctrl Pts',(22.2890476065036,2.40024076526969,37.5115686139742));
#56359=CARTESIAN_POINT('Ctrl Pts',(22.3069275413742,2.39639037100038,37.5811230651677));
#56360=CARTESIAN_POINT('Ctrl Pts',(22.3216095942983,2.39253997673108,37.6513964447735));
#56361=CARTESIAN_POINT('Ctrl Pts',(22.33305794227,2.38868958246177,37.7220700079234));
#56362=CARTESIAN_POINT('Ctrl Pts',(22.3456576913936,2.38445194031984,37.7998514631659));
#56363=CARTESIAN_POINT('Ctrl Pts',(22.3543871217923,2.38021429817791,37.8784097021737));
#56364=CARTESIAN_POINT('Ctrl Pts',(22.3591597089427,2.37597665603598,37.9573258656897));
#56365=CARTESIAN_POINT('Ctrl Pts',(22.3639254329255,2.3717451077898,38.0361285446649));
#56366=CARTESIAN_POINT('Ctrl Pts',(22.3647455855991,2.36751355954361,38.1152876619303));
#56367=CARTESIAN_POINT('Ctrl Pts',(22.3615849782599,2.36328201129742,38.1943760104973));
#56368=CARTESIAN_POINT('Ctrl Pts',(22.3584280215084,2.35905535060505,38.2733730098612));
#56369=CARTESIAN_POINT('Ctrl Pts',(22.3512994605252,2.35482868991268,38.3522989369354));
#56370=CARTESIAN_POINT('Ctrl Pts',(22.3402161241884,2.35060202922031,38.4307248599495));
#56371=CARTESIAN_POINT('Ctrl Pts',(22.3291397839965,2.346378036527,38.5091012780936));
#56372=CARTESIAN_POINT('Ctrl Pts',(22.3141136889076,2.34215404383368,38.5869778556978));
#56373=CARTESIAN_POINT('Ctrl Pts',(22.2952065433738,2.33793005114037,38.6639302830618));
#56374=CARTESIAN_POINT('Ctrl Pts',(22.2763054457119,2.33370740958526,38.7408580954768));
#56375=CARTESIAN_POINT('Ctrl Pts',(22.2535258746306,2.32948476803015,38.8168618897691));
#56376=CARTESIAN_POINT('Ctrl Pts',(22.2269874337358,2.32526212647504,38.8915285281548));
#56377=CARTESIAN_POINT('Ctrl Pts',(22.2004492189825,2.32103952090225,38.9661945302851));
#56378=CARTESIAN_POINT('Ctrl Pts',(22.1701523564412,2.31681691532946,39.0395229579402));
#56379=CARTESIAN_POINT('Ctrl Pts',(22.1362655266727,2.31259430975666,39.1111182128958));
#56380=CARTESIAN_POINT('Ctrl Pts',(22.102345000766,2.30836750534019,39.1827846602182));
#56381=CARTESIAN_POINT('Ctrl Pts',(22.0648275780222,2.30414070092371,39.2527140676081));
#56382=CARTESIAN_POINT('Ctrl Pts',(22.0239288413109,2.29991389650723,39.3205336890925));
#56383=CARTESIAN_POINT('Ctrl Pts',(21.9830102857687,2.29568504385335,39.38838617481));
#56384=CARTESIAN_POINT('Ctrl Pts',(21.9387074144306,2.29145619119947,39.4541264487122));
#56385=CARTESIAN_POINT('Ctrl Pts',(21.8912788588317,2.2872273385456,39.5174112737792));
#56386=CARTESIAN_POINT('Ctrl Pts',(21.8437650636547,2.28299088571053,39.5808098356387));
#56387=CARTESIAN_POINT('Ctrl Pts',(21.7931146601845,2.27875443287547,39.6417437697455));
#56388=CARTESIAN_POINT('Ctrl Pts',(21.7396260771504,2.27451798004041,39.6999036072834));
#56389=CARTESIAN_POINT('Ctrl Pts',(21.6910117494637,2.27066758254117,39.7527635119563));
#56390=CARTESIAN_POINT('Ctrl Pts',(21.6400536112878,2.26681718504193,39.8033321516061));
#56391=CARTESIAN_POINT('Ctrl Pts',(21.5869995482967,2.26296678754269,39.8514059708149));
#56392=CARTESIAN_POINT('Ctrl Pts',(21.5286096947538,2.25872914515703,39.9043147039938));
#56393=CARTESIAN_POINT('Ctrl Pts',(21.4674614702668,2.25449150277136,39.9543995829428));
#56394=CARTESIAN_POINT('Ctrl Pts',(21.4038591439485,2.2502538603857,40.0013600250485));
#56395=CARTESIAN_POINT('Ctrl Pts',(21.3403482803063,2.24602231189841,40.0482529361698));
#56396=CARTESIAN_POINT('Ctrl Pts',(21.274390697293,2.24179076341113,40.0920300571151));
#56397=CARTESIAN_POINT('Ctrl Pts',(21.206325610573,2.23755921492384,40.1324293252597));
#56398=CARTESIAN_POINT('Ctrl Pts',(21.1383391409639,2.2333325539954,40.1727819311007));
#56399=CARTESIAN_POINT('Ctrl Pts',(21.0682504061431,2.22910589306696,40.2097641993818));
#56400=CARTESIAN_POINT('Ctrl Pts',(20.9964283836556,2.22487923213852,40.2431567644821));
#56401=CARTESIAN_POINT('Ctrl Pts',(20.924651697503,2.2206552392123,40.2765282511379));
#56402=CARTESIAN_POINT('Ctrl Pts',(20.8511443193274,2.21643124628608,40.3063143351266));
#56403=CARTESIAN_POINT('Ctrl Pts',(20.776299587088,2.21220725335986,40.3323416835214));
#56404=CARTESIAN_POINT('Ctrl Pts',(20.7014787956642,2.2079846115753,40.3583607064678));
#56405=CARTESIAN_POINT('Ctrl Pts',(20.6253219421162,2.20376196979073,40.380623227526));
#56406=CARTESIAN_POINT('Ctrl Pts',(20.5482406988636,2.19953932800617,40.3990046926898));
#56407=CARTESIAN_POINT('Ctrl Pts',(20.4711601125105,2.19531672220768,40.4173860012036));
#56408=CARTESIAN_POINT('Ctrl Pts',(20.3931556084345,2.19109411640919,40.4318862122382));
#56409=CARTESIAN_POINT('Ctrl Pts',(20.3146508600194,2.18687151061071,40.4424314882594));
#56410=CARTESIAN_POINT('Ctrl Pts',(20.2360680487678,2.18264470597593,40.4529872501961));
#56411=CARTESIAN_POINT('Ctrl Pts',(20.1569844652424,2.17841790134116,40.4595801590354));
#56412=CARTESIAN_POINT('Ctrl Pts',(20.0778301434093,2.17419109670638,40.4621881613616));
#56413=CARTESIAN_POINT('Ctrl Pts',(19.998637464812,2.16996224383792,40.4647974274789));
#56414=CARTESIAN_POINT('Ctrl Pts',(19.9193744489222,2.16573339096945,40.4634179484446));
#56415=CARTESIAN_POINT('Ctrl Pts',(19.840469808524,2.16150453810098,40.4580798457448));
#56416=CARTESIAN_POINT('Ctrl Pts',(19.7614233592487,2.15726808506003,40.4527321493081));
#56417=CARTESIAN_POINT('Ctrl Pts',(19.6827370390208,2.15303163201909,40.4434116689938));
#56418=CARTESIAN_POINT('Ctrl Pts',(19.6048328966024,2.14879517897814,40.4302002920977));
#56419=CARTESIAN_POINT('Ctrl Pts',(19.534027967875,2.14494478352663,40.4181928356201));
#56420=CARTESIAN_POINT('Ctrl Pts',(19.4638692871082,2.14109438807512,40.4029720189242));
#56421=CARTESIAN_POINT('Ctrl Pts',(19.3946625428323,2.13724399262361,40.3846349826285));
#56422=CARTESIAN_POINT('Ctrl Pts',(19.3184954332277,2.13300634937881,40.3644537261921));
#56423=CARTESIAN_POINT('Ctrl Pts',(19.2431956849316,2.128768706134,40.3404214360633));
#56424=CARTESIAN_POINT('Ctrl Pts',(19.1691810715687,2.12453106288919,40.3126297360969));
#56425=CARTESIAN_POINT('Ctrl Pts',(19.0952728940357,2.12029951353659,40.2848780016524));
#56426=CARTESIAN_POINT('Ctrl Pts',(19.0226466165638,2.11606796418399,40.253377756956));
#56427=CARTESIAN_POINT('Ctrl Pts',(18.951706722241,2.11183641483139,40.2182709091864));
#56428=CARTESIAN_POINT('Ctrl Pts',(18.880848765411,2.1076097530325,40.1832046107736));
#56429=CARTESIAN_POINT('Ctrl Pts',(18.8116737389392,2.10338309123362,40.1445401944964));
#56430=CARTESIAN_POINT('Ctrl Pts',(18.7445665092171,2.09915642943474,40.1024677753014));
#56431=CARTESIAN_POINT('Ctrl Pts',(18.6775016396513,2.09493243563535,40.0604219135171));
#56432=CARTESIAN_POINT('Ctrl Pts',(18.6125023721764,2.09070844183596,40.0149725671351));
#56433=CARTESIAN_POINT('Ctrl Pts',(18.5499282180774,2.08648444803657,39.9663553434895));
#56434=CARTESIAN_POINT('Ctrl Pts',(18.4873740797401,2.08226180537735,39.917753671165));
#56435=CARTESIAN_POINT('Ctrl Pts',(18.4272438842452,2.07803916271813,39.8659864212264));
#56436=CARTESIAN_POINT('Ctrl Pts',(18.3698662039139,2.07381652005892,39.8113311332872));
#56437=CARTESIAN_POINT('Ctrl Pts',(18.3124890125612,2.06959391338551,39.7566763111261));
#56438=CARTESIAN_POINT('Ctrl Pts',(18.2578646281728,2.06537130671209,39.699133824258));
#56439=CARTESIAN_POINT('Ctrl Pts',(18.2062856112127,2.06114870003868,39.63901888629));
#56440=CARTESIAN_POINT('Ctrl Pts',(18.1546553056601,2.0569218945347,39.5788441718715));
#56441=CARTESIAN_POINT('Ctrl Pts',(18.1060767223792,2.05269508903072,39.5160922533979));
#56442=CARTESIAN_POINT('Ctrl Pts',(18.0608024441042,2.04846828352674,39.4511118680953));
#56443=CARTESIAN_POINT('Ctrl Pts',(18.0155062267494,2.04423942979081,39.386099994497));
#56444=CARTESIAN_POINT('Ctrl Pts',(17.9735177527947,2.04001057605487,39.3188579009626));
#56445=CARTESIAN_POINT('Ctrl Pts',(17.9350451179742,2.03578172231894,39.2497616170746));
#56446=CARTESIAN_POINT('Ctrl Pts',(17.8965033395575,2.03154526842365,39.180541152309));
#56447=CARTESIAN_POINT('Ctrl Pts',(17.8614902333218,2.02730881452837,39.1094602602954));
#56448=CARTESIAN_POINT('Ctrl Pts',(17.8301668428778,2.02307236063308,39.0369175583546));
#56449=CARTESIAN_POINT('Ctrl Pts',(17.8016979397624,2.01922197299023,38.9709856421728));
#56450=CARTESIAN_POINT('Ctrl Pts',(17.776276383819,2.01537158534738,38.9038467014695));
#56451=CARTESIAN_POINT('Ctrl Pts',(17.7539870835865,2.01152119770453,38.83581004356));
#56452=CARTESIAN_POINT('Ctrl Pts',(17.7247520329228,2.00647095940009,38.7465719284007));
#56453=CARTESIAN_POINT('Ctrl Pts',(17.7008157486621,2.00142072109565,38.6555178360481));
#56454=CARTESIAN_POINT('Ctrl Pts',(17.6823695053237,1.99637048279121,38.5632270836712));
#56455=CARTESIAN_POINT('Ctrl Pts',(17.6641279904338,1.99137629532779,38.4719606343029));
#56456=CARTESIAN_POINT('Ctrl Pts',(17.651255385937,1.98638210786438,38.3794848941208));
#56457=CARTESIAN_POINT('Ctrl Pts',(17.6438903546904,1.98138792040096,38.2863807398292));
#56458=CARTESIAN_POINT('Ctrl Pts',(17.6390429132866,1.97810089685982,38.2251023939168));
#56459=CARTESIAN_POINT('Ctrl Pts',(17.6365803430543,1.97481387331868,38.1635522471656));
#56460=CARTESIAN_POINT('Ctrl Pts',(17.6365307642293,1.97152684977754,38.1019006486528));
#56461=CARTESIAN_POINT('',(17.6365304902263,1.17777684969959,38.0984777417075));
#56462=CARTESIAN_POINT('Ctrl Pts',(17.6365307642285,1.97152684972829,38.1019006477291));
#56463=CARTESIAN_POINT('Ctrl Pts',(17.6364672651918,1.96731692886144,38.0229391350386));
#56464=CARTESIAN_POINT('Ctrl Pts',(17.6403651241089,1.96310700799459,37.9439206442699));
#56465=CARTESIAN_POINT('Ctrl Pts',(17.6482147911937,1.95889708712774,37.8652729829355));
#56466=CARTESIAN_POINT('Ctrl Pts',(17.6560624232589,1.95468825767937,37.7866457109418));
#56467=CARTESIAN_POINT('Ctrl Pts',(17.6678597823381,1.950479428231,37.7083895466702));
#56468=CARTESIAN_POINT('Ctrl Pts',(17.6835453668716,1.94627059878263,37.6309281786783));
#56469=CARTESIAN_POINT('Ctrl Pts',(17.6992318422657,1.94206153029438,37.5534624112789));
#56470=CARTESIAN_POINT('Ctrl Pts',(17.7188068863251,1.93785246180614,37.4767919918292));
#56471=CARTESIAN_POINT('Ctrl Pts',(17.7421579940123,1.93364339331789,37.4013298940864));
#56472=CARTESIAN_POINT('Ctrl Pts',(17.7655341420198,1.9294298112783,37.3257868753385));
#56473=CARTESIAN_POINT('Ctrl Pts',(17.7926942992056,1.92521622923872,37.2514552172083));
#56474=CARTESIAN_POINT('Ctrl Pts',(17.8234764060496,1.92100264719913,37.1787315885817));
#56475=CARTESIAN_POINT('Ctrl Pts',(17.8542754425718,1.91678674775519,37.1059679630946));
#56476=CARTESIAN_POINT('Ctrl Pts',(17.8887001887314,1.91257084831125,37.0348145525808));
#56477=CARTESIAN_POINT('Ctrl Pts',(17.9265419786131,1.90835494886731,36.965644555509));
#56478=CARTESIAN_POINT('Ctrl Pts',(17.9644524925575,1.90413139297429,36.8963489395585));
#56479=CARTESIAN_POINT('Ctrl Pts',(18.0057921972571,1.89990783708127,36.8290443336176));
#56480=CARTESIAN_POINT('Ctrl Pts',(18.0503085452814,1.89568428118824,36.7640757235916));
#56481=CARTESIAN_POINT('Ctrl Pts',(18.0850409851694,1.89238898838731,36.713386068162));
#56482=CARTESIAN_POINT('Ctrl Pts',(18.1217062669699,1.88909369558638,36.664117868854));
#56483=CARTESIAN_POINT('Ctrl Pts',(18.160168207798,1.88579840278545,36.6164200671002));
#56484=CARTESIAN_POINT('Ctrl Pts',(18.2096290557138,1.88156075974001,36.5550821921084));
#56485=CARTESIAN_POINT('Ctrl Pts',(18.2622535021514,1.87732311669457,36.4961053368348));
#56486=CARTESIAN_POINT('Ctrl Pts',(18.3177876717066,1.87308547364912,36.4398337060892));
#56487=CARTESIAN_POINT('Ctrl Pts',(18.3732419807513,1.86885392451558,36.3836429963548));
#56488=CARTESIAN_POINT('Ctrl Pts',(18.4315973767101,1.86462237538204,36.3301501164099));
#56489=CARTESIAN_POINT('Ctrl Pts',(18.4925594774106,1.8603908262485,36.279666648178));
#56490=CARTESIAN_POINT('Ctrl Pts',(18.5534511648287,1.85616416469693,36.2292414900547));
#56491=CARTESIAN_POINT('Ctrl Pts',(18.6169432144885,1.85193750314536,36.1818191334874));
#56492=CARTESIAN_POINT('Ctrl Pts',(18.682705210216,1.84771084159379,36.137673605715));
#56493=CARTESIAN_POINT('Ctrl Pts',(18.7484256946727,1.84348684805876,36.0935559441429));
#56494=CARTESIAN_POINT('Ctrl Pts',(18.816412892918,1.83926285452372,36.0527112663131));
#56495=CARTESIAN_POINT('Ctrl Pts',(18.8863051724119,1.83503886098868,36.015371910411));
#56496=CARTESIAN_POINT('Ctrl Pts',(18.956175095001,1.83081621861034,35.9780444984952));
#56497=CARTESIAN_POINT('Ctrl Pts',(19.0279484755394,1.826593576232,35.9442204026176));
#56498=CARTESIAN_POINT('Ctrl Pts',(19.1012379912428,1.82237093385366,35.9140866228245));
#56499=CARTESIAN_POINT('Ctrl Pts',(19.1745268820873,1.81814832747714,35.883953099949));
#56500=CARTESIAN_POINT('Ctrl Pts',(19.2493314482957,1.81392572110061,35.8575100075387));
#56501=CARTESIAN_POINT('Ctrl Pts',(19.3252446324073,1.80970311472409,35.8348961094897));
#56502=CARTESIAN_POINT('Ctrl Pts',(19.4012333018571,1.80547630953975,35.8122597249944));
#56503=CARTESIAN_POINT('Ctrl Pts',(19.478332340891,1.80124950435542,35.7934602747277));
#56504=CARTESIAN_POINT('Ctrl Pts',(19.556120363395,1.79702269917109,35.7785863554491));
#56505=CARTESIAN_POINT('Ctrl Pts',(19.6339460803034,1.79279384576777,35.7637052285887));
#56506=CARTESIAN_POINT('Ctrl Pts',(19.7124609809109,1.78856499236445,35.7527534870205));
#56507=CARTESIAN_POINT('Ctrl Pts',(19.7912368782203,1.78433613896113,35.7457679808726));
#56508=CARTESIAN_POINT('Ctrl Pts',(19.8701543524351,1.78009968541616,35.7387699202965));
#56509=CARTESIAN_POINT('Ctrl Pts',(19.9493332910468,1.77586323187119,35.735752355794));
#56510=CARTESIAN_POINT('Ctrl Pts',(20.0283440476992,1.77162677832622,35.7366999649092));
#56511=CARTESIAN_POINT('Ctrl Pts',(20.1001546402594,1.76777638817293,35.7375612194392));
#56512=CARTESIAN_POINT('Ctrl Pts',(20.1718260670583,1.76392599801965,35.7416972098081));
#56513=CARTESIAN_POINT('Ctrl Pts',(20.2430412607103,1.76007560786637,35.7490594676827));
#56514=CARTESIAN_POINT('Ctrl Pts',(20.3214190114522,1.75583795991208,35.7571621938428));
#56515=CARTESIAN_POINT('Ctrl Pts',(20.3995382347593,1.75160031195779,35.7692039567637));
#56516=CARTESIAN_POINT('Ctrl Pts',(20.4769719941166,1.74736266400351,35.7851591506697));
#56517=CARTESIAN_POINT('Ctrl Pts',(20.5542944013986,1.74313110991445,35.8010914005269));
#56518=CARTESIAN_POINT('Ctrl Pts',(20.6309328469414,1.7388995558254,35.820925811592));
#56519=CARTESIAN_POINT('Ctrl Pts',(20.706465711346,1.73466800173634,35.8445850404876));
#56520=CARTESIAN_POINT('Ctrl Pts',(20.7819113336741,1.73044133518291,35.868216942467));
#56521=CARTESIAN_POINT('Ctrl Pts',(20.8562534674485,1.72621466862947,35.8956647436907));
#56522=CARTESIAN_POINT('Ctrl Pts',(20.9290823821772,1.72198800207604,35.9268004306949));
#56523=CARTESIAN_POINT('Ctrl Pts',(21.0018653252485,1.71776400351329,35.9579164639786));
#56524=CARTESIAN_POINT('Ctrl Pts',(21.0731365153078,1.71354000495054,35.9927155786309));
#56525=CARTESIAN_POINT('Ctrl Pts',(21.1425042013522,1.70931600638779,36.0310208819825));
#56526=CARTESIAN_POINT('Ctrl Pts',(21.2118496986302,1.70509335896307,36.0693139325479));
#56527=CARTESIAN_POINT('Ctrl Pts',(21.2792924909367,1.70087071153834,36.111110718232));
#56528=CARTESIAN_POINT('Ctrl Pts',(21.3444648759035,1.69664806411361,36.1561881165191));
#56529=CARTESIAN_POINT('Ctrl Pts',(21.409636705396,1.69242545267916,36.2012651306044));
#56530=CARTESIAN_POINT('Ctrl Pts',(21.4725377813014,1.68820284124471,36.2496224338601));
#56531=CARTESIAN_POINT('Ctrl Pts',(21.5328301227423,1.68398022981027,36.3009940923627));
#56532=CARTESIAN_POINT('Ctrl Pts',(21.5931824163948,1.67975341958559,36.3524168327186));
#56533=CARTESIAN_POINT('Ctrl Pts',(21.6509204363752,1.67552660936091,36.4068596108128));
#56534=CARTESIAN_POINT('Ctrl Pts',(21.7057404858179,1.67129979913624,36.4640171651446));
#56535=CARTESIAN_POINT('Ctrl Pts',(21.7605870998265,1.66707094069418,36.5212024167445));
#56536=CARTESIAN_POINT('Ctrl Pts',(21.812512619037,1.66284208225211,36.581104710582));
#56537=CARTESIAN_POINT('Ctrl Pts',(21.8612530531965,1.65861322381005,36.6433849125913));
#56538=CARTESIAN_POINT('Ctrl Pts',(21.9100810833794,1.65437676528832,36.7057770442156));
#56539=CARTESIAN_POINT('Ctrl Pts',(21.9557123203718,1.65014030676659,36.7705552388603));
#56540=CARTESIAN_POINT('Ctrl Pts',(21.9979257454302,1.64590384824486,36.837350738864));
#56541=CARTESIAN_POINT('Ctrl Pts',(22.0362918130926,1.64205350314567,36.8980584561161));
#56542=CARTESIAN_POINT('Ctrl Pts',(22.071835123553,1.63820315804648,36.9604319462386));
#56543=CARTESIAN_POINT('Ctrl Pts',(22.1044237487931,1.63435281294729,37.0241788594681));
#56544=CARTESIAN_POINT('Ctrl Pts',(22.1402902674161,1.63011518484278,37.0943376904606));
#56545=CARTESIAN_POINT('Ctrl Pts',(22.1727117659432,1.62587755673826,37.1664237990782));
#56546=CARTESIAN_POINT('Ctrl Pts',(22.2014773272519,1.62163992863375,37.2400651079902));
#56547=CARTESIAN_POINT('Ctrl Pts',(22.2302015223787,1.61740839443066,37.3136005173599));
#56548=CARTESIAN_POINT('Ctrl Pts',(22.2552800518491,1.61317686022756,37.3886862526061));
#56549=CARTESIAN_POINT('Ctrl Pts',(22.2765482936958,1.60894532602447,37.4649265338793));
#56550=CARTESIAN_POINT('Ctrl Pts',(22.2977919703461,1.60471867931841,37.5410787562757));
#56551=CARTESIAN_POINT('Ctrl Pts',(22.3152339798406,1.60049203261236,37.6183824254067));
#56552=CARTESIAN_POINT('Ctrl Pts',(22.3287586771763,1.59626538590631,37.6964241528833));
#56553=CARTESIAN_POINT('Ctrl Pts',(22.3422748374071,1.59204140715842,37.7744166185981));
#56554=CARTESIAN_POINT('Ctrl Pts',(22.3518785136756,1.58781742841053,37.8531457572553));
#56555=CARTESIAN_POINT('Ctrl Pts',(22.357504850999,1.58359344966264,37.9321866560246));
#56556=CARTESIAN_POINT('Ctrl Pts',(22.3631293886866,1.57937082199321,38.0112022728352));
#56557=CARTESIAN_POINT('Ctrl Pts',(22.364779080483,1.57514819432379,38.0905289844784));
#56558=CARTESIAN_POINT('Ctrl Pts',(22.3624409426436,1.57092556665437,38.1697368870928));
#56559=CARTESIAN_POINT('Ctrl Pts',(22.3601028246846,1.56670297488862,38.2489441162272));
#56560=CARTESIAN_POINT('Ctrl Pts',(22.3537769597684,1.56248038312288,38.3280320698116));
#56561=CARTESIAN_POINT('Ctrl Pts',(22.343502455719,1.55825779135713,38.4065724725726));
#56562=CARTESIAN_POINT('Ctrl Pts',(22.3332177344175,1.55403100052894,38.4851909780898));
#56563=CARTESIAN_POINT('Ctrl Pts',(22.3189765914572,1.54980420970075,38.5632603792459));
#56564=CARTESIAN_POINT('Ctrl Pts',(22.3008697873043,1.54557741887256,38.6403597531));
#56565=CARTESIAN_POINT('Ctrl Pts',(22.2827542084542,1.54134857970887,38.7174964899065));
#56566=CARTESIAN_POINT('Ctrl Pts',(22.2607693666919,1.53711974054519,38.7936618119859));
#56567=CARTESIAN_POINT('Ctrl Pts',(22.2350560507775,1.5328909013815,38.8684496670459));
#56568=CARTESIAN_POINT('Ctrl Pts',(22.2092965202539,1.52865446171425,38.9433719385112));
#56569=CARTESIAN_POINT('Ctrl Pts',(22.1797953008886,1.524418022047,39.0169113601128));
#56570=CARTESIAN_POINT('Ctrl Pts',(22.1467414226089,1.52018158237975,39.0886818018732));
#56571=CARTESIAN_POINT('Ctrl Pts',(22.1166985853834,1.51633106092923,39.1539143195573));
#56572=CARTESIAN_POINT('Ctrl Pts',(22.0837215876223,1.51248053947872,39.2176855272462));
#56573=CARTESIAN_POINT('Ctrl Pts',(22.0479838852922,1.50863001802821,39.2797255810076));
#56574=CARTESIAN_POINT('Ctrl Pts',(22.0086531267125,1.50439236648092,39.3480031203474));
#56575=CARTESIAN_POINT('Ctrl Pts',(21.9658303594803,1.50015471493363,39.4144398044524));
#56576=CARTESIAN_POINT('Ctrl Pts',(21.9197129007478,1.49591706338634,39.4786561643871));
#56577=CARTESIAN_POINT('Ctrl Pts',(21.8736617617226,1.49168550583941,39.542780177295));
#56578=CARTESIAN_POINT('Ctrl Pts',(21.8243256115447,1.48745394829248,39.6046898293475));
#56579=CARTESIAN_POINT('Ctrl Pts',(21.7719468506317,1.48322239074554,39.6640315851787));
#56580=CARTESIAN_POINT('Ctrl Pts',(21.7196285909442,1.47899572095108,39.7233047970257));
#56581=CARTESIAN_POINT('Ctrl Pts',(21.6642750132269,1.47476905115662,39.7800156573782));
#56582=CARTESIAN_POINT('Ctrl Pts',(21.6061699489185,1.47054238136216,39.8338421312482));
#56583=CARTESIAN_POINT('Ctrl Pts',(21.5481015639615,1.46631837969153,39.8876346266658));
#56584=CARTESIAN_POINT('Ctrl Pts',(21.4872854829616,1.4620943780209,39.9385460319441));
#56585=CARTESIAN_POINT('Ctrl Pts',(21.4240428515956,1.45787037635027,39.9862906450808));
#56586=CARTESIAN_POINT('Ctrl Pts',(21.3608204517885,1.45364772595388,40.0340199845338));
#56587=CARTESIAN_POINT('Ctrl Pts',(21.2951734169776,1.44942507555749,40.0785842613587));
#56588=CARTESIAN_POINT('Ctrl Pts',(21.2274553150098,1.4452024251611,40.1197385698536));
#56589=CARTESIAN_POINT('Ctrl Pts',(21.1597377924494,1.44097981089442,40.1608925262253));
#56590=CARTESIAN_POINT('Ctrl Pts',(21.0899496393029,1.43675719662773,40.1986363300461));
#56591=CARTESIAN_POINT('Ctrl Pts',(21.0184714126016,1.43253458236105,40.2327696599992));
#56592=CARTESIAN_POINT('Ctrl Pts',(20.9469221149502,1.42830776954018,40.2669369287936));
#56593=CARTESIAN_POINT('Ctrl Pts',(20.8736798110474,1.4240809567193,40.2974863504011));
#56594=CARTESIAN_POINT('Ctrl Pts',(20.7991470067265,1.41985414389843,40.3242649353303));
#56595=CARTESIAN_POINT('Ctrl Pts',(20.7245780877089,1.41562528298525,40.3510564957606));
#56596=CARTESIAN_POINT('Ctrl Pts',(20.648717871736,1.41139642207206,40.3740734433361));
#56597=CARTESIAN_POINT('Ctrl Pts',(20.5719836225394,1.40716756115888,40.3932128502271));
#56598=CARTESIAN_POINT('Ctrl Pts',(20.4951114713913,1.40293110040366,40.4123866532527));
#56599=CARTESIAN_POINT('Ctrl Pts',(20.4173626095551,1.39869463964843,40.427668901285));
#56600=CARTESIAN_POINT('Ctrl Pts',(20.3391638481552,1.39445817889321,40.4390079788245));
#56601=CARTESIAN_POINT('Ctrl Pts',(20.2680926964329,1.39060786029852,40.4493135295234));
#56602=CARTESIAN_POINT('Ctrl Pts',(20.1966502644901,1.38675754170382,40.4563626067236));
#56603=CARTESIAN_POINT('Ctrl Pts',(20.1251572814483,1.38290722310913,40.4601538288426));
#56604=CARTESIAN_POINT('Ctrl Pts',(20.0464718075153,1.37866954647953,40.4643264636457));
#56605=CARTESIAN_POINT('Ctrl Pts',(19.9674297554087,1.37443186984992,40.4645676688016));
#56606=CARTESIAN_POINT('Ctrl Pts',(19.8884568612947,1.37019419322032,40.4608364130341));
#56607=CARTESIAN_POINT('Ctrl Pts',(19.8095975279049,1.36596261024642,40.4571105227039));
#56608=CARTESIAN_POINT('Ctrl Pts',(19.7308076193892,1.36173102727252,40.4494235374622));
#56609=CARTESIAN_POINT('Ctrl Pts',(19.6525156568587,1.35749944429862,40.4377863615334));
#56610=CARTESIAN_POINT('Ctrl Pts',(19.574314119327,1.35327274868318,40.4261626262131));
#56611=CARTESIAN_POINT('Ctrl Pts',(19.4966098462091,1.34904605306774,40.4105978353342));
#56612=CARTESIAN_POINT('Ctrl Pts',(19.4198274858161,1.3448193574523,40.3911547950074));
#56613=CARTESIAN_POINT('Ctrl Pts',(19.3430935905616,1.34059532973333,40.3717240271562));
#56614=CARTESIAN_POINT('Ctrl Pts',(19.2672809062322,1.33637130201436,40.3484199835529));
#56615=CARTESIAN_POINT('Ctrl Pts',(19.1928039135692,1.33214727429539,40.3213565492624));
#56616=CARTESIAN_POINT('Ctrl Pts',(19.1183507428936,1.32792459766125,40.2943017714008));
#56617=CARTESIAN_POINT('Ctrl Pts',(19.0452328557494,1.32370192102712,40.263490150698));
#56618=CARTESIAN_POINT('Ctrl Pts',(18.973848158353,1.31947924439298,40.229084976882));
#56619=CARTESIAN_POINT('Ctrl Pts',(18.9024640691693,1.31525660373695,40.1946800962053));
#56620=CARTESIAN_POINT('Ctrl Pts',(18.8328135620277,1.31103396308091,40.1566819281047));
#56621=CARTESIAN_POINT('Ctrl Pts',(18.7652718336524,1.30681132242487,40.1153006713957));
#56622=CARTESIAN_POINT('Ctrl Pts',(18.6976629480153,1.30258448316465,40.0738782689838));
#56623=CARTESIAN_POINT('Ctrl Pts',(18.632167430101,1.29835764390443,40.0290663041574));
#56624=CARTESIAN_POINT('Ctrl Pts',(18.5691327188234,1.2941308046442,39.9811191521428));
#56625=CARTESIAN_POINT('Ctrl Pts',(18.5060674633782,1.28990191722219,39.9331487668044));
#56626=CARTESIAN_POINT('Ctrl Pts',(18.4454657487965,1.28567302980018,39.882040470467));
#56627=CARTESIAN_POINT('Ctrl Pts',(18.3876410520472,1.28144414237817,39.8280882685374));
#56628=CARTESIAN_POINT('Ctrl Pts',(18.3297124397358,1.27720765531035,39.7740391102257));
#56629=CARTESIAN_POINT('Ctrl Pts',(18.2745711437923,1.27297116824253,39.7171361720341));
#56630=CARTESIAN_POINT('Ctrl Pts',(18.2224927938629,1.26873468117471,39.6577093994166));
#56631=CARTESIAN_POINT('Ctrl Pts',(18.1751644211586,1.26488459684649,39.6037028410892));
#56632=CARTESIAN_POINT('Ctrl Pts',(18.1303653946041,1.26103451251827,39.547612476359));
#56633=CARTESIAN_POINT('Ctrl Pts',(18.0882714251047,1.25718442819005,39.4897065506174));
#56634=CARTESIAN_POINT('Ctrl Pts',(18.0416356896263,1.25291893561627,39.4255528139269));
#56635=CARTESIAN_POINT('Ctrl Pts',(17.9981457106074,1.24865344304249,39.3589293252204));
#56636=CARTESIAN_POINT('Ctrl Pts',(17.9580708299778,1.24438795046871,39.290174653365));
#56637=CARTESIAN_POINT('Ctrl Pts',(17.9180549133786,1.24012873391197,39.2215211434468));
#56638=CARTESIAN_POINT('Ctrl Pts',(17.8814443465497,1.23586951735523,39.1507430715146));
#56639=CARTESIAN_POINT('Ctrl Pts',(17.8484665606069,1.23161030079849,39.0782097423729));
#56640=CARTESIAN_POINT('Ctrl Pts',(17.8155274888571,1.22735608433886,39.0057615635597));
#56641=CARTESIAN_POINT('Ctrl Pts',(17.786212915632,1.22310186787923,38.9315626377535));
#56642=CARTESIAN_POINT('Ctrl Pts',(17.7607047949425,1.2188476514196,38.8560075565141));
#56643=CARTESIAN_POINT('Ctrl Pts',(17.7352203500755,1.21459738358774,38.7805226030866));
#56644=CARTESIAN_POINT('Ctrl Pts',(17.7135354803532,1.21034711575588,38.7036844317353));
#56645=CARTESIAN_POINT('Ctrl Pts',(17.6957838047055,1.20609684792401,38.6259069939093));
#56646=CARTESIAN_POINT('Ctrl Pts',(17.6780415344963,1.20184883202787,38.5481707652017));
#56647=CARTESIAN_POINT('Ctrl Pts',(17.6642284180863,1.19760081613173,38.4694967075477));
#56648=CARTESIAN_POINT('Ctrl Pts',(17.6544277166018,1.19335280023559,38.3903120807924));
#56649=CARTESIAN_POINT('Ctrl Pts',(17.6446283443218,1.18910536046987,38.3111381933266));
#56650=CARTESIAN_POINT('Ctrl Pts',(17.6388403639534,1.18485792070415,38.231454330974));
#56651=CARTESIAN_POINT('Ctrl Pts',(17.6370954127973,1.18061048093843,38.1516948031864));
#56652=CARTESIAN_POINT('Ctrl Pts',(17.6367073713473,1.17966593720172,38.133957915421));
#56653=CARTESIAN_POINT('Ctrl Pts',(17.6365190645752,1.178721393465,38.1162172986552));
#56654=CARTESIAN_POINT('Ctrl Pts',(17.636530490226,1.17777684972829,38.0984777422465));
#56655=CARTESIAN_POINT('Ctrl Pts',(17.6365304902264,1.17777684969959,38.0984777417075));
#56656=CARTESIAN_POINT('Ctrl Pts',(17.6365882237607,1.1730040949641,38.0088402283102));
#56657=CARTESIAN_POINT('Ctrl Pts',(17.6417494431323,1.16823134022862,37.9193966228562));
#56658=CARTESIAN_POINT('Ctrl Pts',(17.6519239320934,1.16345858549314,37.8306875045147));
#56659=CARTESIAN_POINT('Ctrl Pts',(17.6621469747597,1.15866305468241,37.7415550571597));
#56660=CARTESIAN_POINT('Ctrl Pts',(17.6774311176323,1.15386752387167,37.6531643358699));
#56661=CARTESIAN_POINT('Ctrl Pts',(17.697635314948,1.14907199306094,37.5660456031409));
#56662=CARTESIAN_POINT('Ctrl Pts',(17.7179521886893,1.14424971814043,37.4784410195136));
#56663=CARTESIAN_POINT('Ctrl Pts',(17.7432440262356,1.13942744321992,37.3921228568976));
#56664=CARTESIAN_POINT('Ctrl Pts',(17.7733193362406,1.1346051682994,37.3076088954691));
#56665=CARTESIAN_POINT('Ctrl Pts',(17.7798544807557,1.13355732328992,37.2892446308483));
#56666=CARTESIAN_POINT('Ctrl Pts',(17.7866153068068,1.13250947828044,37.2709654671663));
#56667=CARTESIAN_POINT('Ctrl Pts',(17.7935995603932,1.13146163327096,37.2527765696094));
#56668=CARTESIAN_POINT('Ctrl Pts',(17.8218455723972,1.12722389442741,37.1792162653646));
#56669=CARTESIAN_POINT('Ctrl Pts',(17.8538273169042,1.12298615558387,37.1069320076802));
#56670=CARTESIAN_POINT('Ctrl Pts',(17.8894088186085,1.11874841674032,37.0363293244936));
#56671=CARTESIAN_POINT('Ctrl Pts',(17.9249391483456,1.11451677245216,36.9658281794099));
#56672=CARTESIAN_POINT('Ctrl Pts',(17.9640587449404,1.110285128164,36.8970042212857));
#56673=CARTESIAN_POINT('Ctrl Pts',(18.0065830683766,1.10605348387584,36.8302443630299));
#56674=CARTESIAN_POINT('Ctrl Pts',(18.0490582618386,1.10182672856787,36.7635616349869));
#56675=CARTESIAN_POINT('Ctrl Pts',(18.0949301144955,1.09759997325989,36.6989386610957));
#56676=CARTESIAN_POINT('Ctrl Pts',(18.1439682646889,1.09337321795192,36.6367376727265));
#56677=CARTESIAN_POINT('Ctrl Pts',(18.1929754506256,1.08914913155245,36.5745759600509));
#56678=CARTESIAN_POINT('Ctrl Pts',(18.2451446762482,1.08492504515298,36.5148335645099));
#56679=CARTESIAN_POINT('Ctrl Pts',(18.3002030740553,1.08070095875351,36.4578426228132));
#56680=CARTESIAN_POINT('Ctrl Pts',(18.3552438471663,1.07647822452269,36.4008699244376));
#56681=CARTESIAN_POINT('Ctrl Pts',(18.4131716304322,1.07225549029186,36.3466472677579));
#56682=CARTESIAN_POINT('Ctrl Pts',(18.4736751895664,1.06803275606103,36.2954715258675));
#56683=CARTESIAN_POINT('Ctrl Pts',(18.5341782166333,1.06381005896487,36.2442962340158));
#56684=CARTESIAN_POINT('Ctrl Pts',(18.5972566157142,1.05958736186871,36.196168105306));
#56685=CARTESIAN_POINT('Ctrl Pts',(18.6625655639975,1.05536466477255,36.1513441632));
#56686=CARTESIAN_POINT('Ctrl Pts',(18.7279394147492,1.05113777126116,36.1064756761341));
#56687=CARTESIAN_POINT('Ctrl Pts',(18.7955478551298,1.04691087774978,36.0649182005989));
#56688=CARTESIAN_POINT('Ctrl Pts',(18.8650170261336,1.04268398423839,36.0268854132168));
#56689=CARTESIAN_POINT('Ctrl Pts',(18.9345198404873,1.03845504367714,35.9888342068676));
#56690=CARTESIAN_POINT('Ctrl Pts',(19.0058847581297,1.03422610311589,35.954311293574));
#56691=CARTESIAN_POINT('Ctrl Pts',(19.0787155627366,1.02999716255464,35.9234831894616));
#56692=CARTESIAN_POINT('Ctrl Pts',(19.1516772057252,1.02576062482701,35.8925997035739));
#56693=CARTESIAN_POINT('Ctrl Pts',(19.2261095561485,1.02152408709938,35.8654244506196));
#56694=CARTESIAN_POINT('Ctrl Pts',(19.3015989934079,1.01728754937175,35.8420747410751));
#56695=CARTESIAN_POINT('Ctrl Pts',(19.370193189267,1.0134379790318,35.8208578051978));
#56696=CARTESIAN_POINT('Ctrl Pts',(19.4396597441982,1.00958840869185,35.8027988984575));
#56697=CARTESIAN_POINT('Ctrl Pts',(19.5096822305933,1.0057388383519,35.7879491947831));
#56698=CARTESIAN_POINT('Ctrl Pts',(19.5867672127342,1.00150099882088,35.7716017441074));
#56699=CARTESIAN_POINT('Ctrl Pts',(19.6648152223334,0.997263159289865,35.7590829273399));
#56700=CARTESIAN_POINT('Ctrl Pts',(19.7434120318108,0.99302531975885,35.7504994029623));
#56701=CARTESIAN_POINT('Ctrl Pts',(19.8218958550916,0.988793572299183,35.7419282177595));
#56702=CARTESIAN_POINT('Ctrl Pts',(19.9009264494113,0.984561824839515,35.7372811408079));
#56703=CARTESIAN_POINT('Ctrl Pts',(19.9800787707609,0.980330077379848,35.7366139575758));
#56704=CARTESIAN_POINT('Ctrl Pts',(20.0591397067108,0.976103215688868,35.7359475446409));
#56705=CARTESIAN_POINT('Ctrl Pts',(20.1383216240653,0.971876353997889,35.7392518979301));
#56706=CARTESIAN_POINT('Ctrl Pts',(20.2171952439491,0.967649492306909,35.7465309292651));
#56707=CARTESIAN_POINT('Ctrl Pts',(20.2960190972292,0.96342529762362,35.7538053677759));
#56708=CARTESIAN_POINT('Ctrl Pts',(20.3745345736319,0.959201102940331,35.7650494634725));
#56709=CARTESIAN_POINT('Ctrl Pts',(20.4523145051818,0.954976908257042,35.7802150898624));
#56710=CARTESIAN_POINT('Ctrl Pts',(20.5300695712347,0.950754064008214,35.7953758679472));
#56711=CARTESIAN_POINT('Ctrl Pts',(20.6070890996636,0.946531219759387,35.8144555975261));
#56712=CARTESIAN_POINT('Ctrl Pts',(20.6829546220782,0.942308375510559,35.8373547725987));
#56713=CARTESIAN_POINT('Ctrl Pts',(20.7588195055433,0.938085566827086,35.8602537548114));
#56714=CARTESIAN_POINT('Ctrl Pts',(20.833529954006,0.933862758143614,35.8869719817455));
#56715=CARTESIAN_POINT('Ctrl Pts',(20.9066826462485,0.929639949460142,35.9173600801113));
#56716=CARTESIAN_POINT('Ctrl Pts',(20.9799080625471,0.925412942711408,35.9477783885172));
#56717=CARTESIAN_POINT('Ctrl Pts',(21.0515721953663,0.921185935962673,35.9818736757559));
#56718=CARTESIAN_POINT('Ctrl Pts',(21.1212922818258,0.916958929213939,36.0194486164437));
#56719=CARTESIAN_POINT('Ctrl Pts',(21.1910461501188,0.912729874331789,36.0570417635117));
#56720=CARTESIAN_POINT('Ctrl Pts',(21.2588536941375,0.908500819449638,36.0981176796145));
#56721=CARTESIAN_POINT('Ctrl Pts',(21.3243595437161,0.904271764567488,36.1424346141526));
#56722=CARTESIAN_POINT('Ctrl Pts',(21.3899830765645,0.900035112058414,36.1868311654241));
#56723=CARTESIAN_POINT('Ctrl Pts',(21.4532962773062,0.89579845954934,36.2344800867139));
#56724=CARTESIAN_POINT('Ctrl Pts',(21.5139755799051,0.891561807040266,36.2850982438845));
#56725=CARTESIAN_POINT('Ctrl Pts',(21.5690968407095,0.887713219171115,36.3310799299511));
#56726=CARTESIAN_POINT('Ctrl Pts',(21.6220448664736,0.883864631301964,36.3795111358586));
#56727=CARTESIAN_POINT('Ctrl Pts',(21.6726046576235,0.880016043432813,36.430154468163));
#56728=CARTESIAN_POINT('Ctrl Pts',(21.7282653304164,0.875779178817131,36.4859071104193));
#56729=CARTESIAN_POINT('Ctrl Pts',(21.7812400674091,0.87154231420145,36.5445506652308));
#56730=CARTESIAN_POINT('Ctrl Pts',(21.8312139615278,0.867305449585769,36.605795908182));
#56731=CARTESIAN_POINT('Ctrl Pts',(21.8811159619345,0.863074680231024,36.6669530421728));
#56732=CARTESIAN_POINT('Ctrl Pts',(21.9280253986868,0.858843910876279,36.7307040710797));
#56733=CARTESIAN_POINT('Ctrl Pts',(21.971664141373,0.854613141521535,36.7967229939404));
#56734=CARTESIAN_POINT('Ctrl Pts',(22.0152524871653,0.850387258137864,36.8626656738011));
#56735=CARTESIAN_POINT('Ctrl Pts',(22.055577387786,0.846161374754194,36.9308706536058));
#56736=CARTESIAN_POINT('Ctrl Pts',(22.0924019147194,0.841935491370524,37.0009801329463));
#56737=CARTESIAN_POINT('Ctrl Pts',(22.1292032040468,0.83771227467184,37.0710453706742));
#56738=CARTESIAN_POINT('Ctrl Pts',(22.1625082864791,0.833489057973156,37.1430123084224));
#56739=CARTESIAN_POINT('Ctrl Pts',(22.1921250309563,0.829265841274472,37.2164965820355));
#56740=CARTESIAN_POINT('Ctrl Pts',(22.2217323167283,0.825043973345284,37.2899573869626));
#56741=CARTESIAN_POINT('Ctrl Pts',(22.2476534285012,0.820822105416095,37.3649341308112));
#56742=CARTESIAN_POINT('Ctrl Pts',(22.2697440688809,0.816600237486907,37.4410217737437));
#56743=CARTESIAN_POINT('Ctrl Pts',(22.2918345389071,0.812378402114952,37.517108829921));
#56744=CARTESIAN_POINT('Ctrl Pts',(22.3100944668947,0.808156566742998,37.5943063173825));
#56745=CARTESIAN_POINT('Ctrl Pts',(22.3244296318692,0.803934731371043,37.6721947553052));
#56746=CARTESIAN_POINT('Ctrl Pts',(22.3387790902978,0.799708686447955,37.7501608550346));
#56747=CARTESIAN_POINT('Ctrl Pts',(22.3491958837366,0.795482641524868,37.8288188190892));
#56748=CARTESIAN_POINT('Ctrl Pts',(22.3556372071988,0.79125659660178,37.9077403085395));
#56749=CARTESIAN_POINT('Ctrl Pts',(22.3620816596615,0.787028498793719,37.9867001356655));
#56750=CARTESIAN_POINT('Ctrl Pts',(22.3645467805294,0.782800400985658,38.0659232738646));
#56751=CARTESIAN_POINT('Ctrl Pts',(22.363041942897,0.778572303177597,38.1449801846302));
#56752=CARTESIAN_POINT('Ctrl Pts',(22.3615343943348,0.774336588549943,38.2241795145768));
#56753=CARTESIAN_POINT('Ctrl Pts',(22.3560426299536,0.77010087392229,38.3032115498097));
#56754=CARTESIAN_POINT('Ctrl Pts',(22.3466280503898,0.765865159294637,38.3816509080826));
#56755=CARTESIAN_POINT('Ctrl Pts',(22.3380545522257,0.762007855701003,38.4530826368805));
#56756=CARTESIAN_POINT('Ctrl Pts',(22.3262285401886,0.758150552107369,38.5240226863687));
#56757=CARTESIAN_POINT('Ctrl Pts',(22.3112327910835,0.754293248513735,38.5941593126921));
#56758=CARTESIAN_POINT('Ctrl Pts',(22.2947549221081,0.750054704459074,38.6712279626701));
#56759=CARTESIAN_POINT('Ctrl Pts',(22.2743871480269,0.745816160404412,38.7476159526973));
#56760=CARTESIAN_POINT('Ctrl Pts',(22.2502008691845,0.74157761634975,38.8229014381097));
#56761=CARTESIAN_POINT('Ctrl Pts',(22.2260493863507,0.73734517014983,38.898078612756));
#56762=CARTESIAN_POINT('Ctrl Pts',(22.1980904507105,0.733112723949911,38.9721559903171));
#56763=CARTESIAN_POINT('Ctrl Pts',(22.1664463281365,0.728880277749991,39.0447225773761));
#56764=CARTESIAN_POINT('Ctrl Pts',(22.1348388228573,0.724652729165109,39.1172051933244));
#56765=CARTESIAN_POINT('Ctrl Pts',(22.0995547914582,0.720425180580228,39.1881800656599));
#56766=CARTESIAN_POINT('Ctrl Pts',(22.0607655974215,0.716197631995346,39.2572534698086));
#56767=CARTESIAN_POINT('Ctrl Pts',(22.0220009430105,0.711972757930074,39.3262831753054));
#56768=CARTESIAN_POINT('Ctrl Pts',(21.9797357563619,0.707747883864801,39.393413392886));
#56769=CARTESIAN_POINT('Ctrl Pts',(21.9341880649202,0.703523009799529,39.4582735256274));
#56770=CARTESIAN_POINT('Ctrl Pts',(21.8886550226854,0.699299494552947,39.5231127978272));
#56771=CARTESIAN_POINT('Ctrl Pts',(21.8398418412436,0.695075979306365,39.58568305189));
#56772=CARTESIAN_POINT('Ctrl Pts',(21.7880099274264,0.690852464059783,39.6456425655127));
#56773=CARTESIAN_POINT('Ctrl Pts',(21.736178563767,0.686628993642725,39.7056014427091));
#56774=CARTESIAN_POINT('Ctrl Pts',(21.681328838936,0.682405523225666,39.7629492810137));
#56775=CARTESIAN_POINT('Ctrl Pts',(21.6237615331349,0.678182052808608,39.8173785035371));
#56776=CARTESIAN_POINT('Ctrl Pts',(21.5661372653819,0.673954403333392,39.871861582928));
#56777=CARTESIAN_POINT('Ctrl Pts',(21.5057903865848,0.669726753858176,39.9234199551932));
#56778=CARTESIAN_POINT('Ctrl Pts',(21.4430570967569,0.665499104382961,39.9717843509335));
#56779=CARTESIAN_POINT('Ctrl Pts',(21.3802935543493,0.661269416160799,40.0201720699802));
#56780=CARTESIAN_POINT('Ctrl Pts',(21.3151416937638,0.657039727938637,40.0653624766099));
#56781=CARTESIAN_POINT('Ctrl Pts',(21.2479671343398,0.652810039716476,40.1071294110017));
#56782=CARTESIAN_POINT('Ctrl Pts',(21.180672278697,0.648572776967528,40.1489711416305));
#56783=CARTESIAN_POINT('Ctrl Pts',(21.1113478974067,0.644335514218581,40.1873769224907));
#56784=CARTESIAN_POINT('Ctrl Pts',(21.040384453305,0.640098251469634,40.222166494463));
#56785=CARTESIAN_POINT('Ctrl Pts',(20.9760306248562,0.636255652177974,40.2537157262521));
#56786=CARTESIAN_POINT('Ctrl Pts',(20.910329365219,0.632413052886314,40.2822915244999));
#56787=CARTESIAN_POINT('Ctrl Pts',(20.8435835715002,0.628570453594655,40.3077946459748));
#56788=CARTESIAN_POINT('Ctrl Pts',(20.7699581473124,0.624331789447159,40.3359264282503));
#56789=CARTESIAN_POINT('Ctrl Pts',(20.6947864120994,0.620093125299663,40.360423862717));
#56790=CARTESIAN_POINT('Ctrl Pts',(20.6184612006793,0.615854461152167,40.3811173104762));
#56791=CARTESIAN_POINT('Ctrl Pts',(20.5422454777903,0.611621877369241,40.4017810734805));
#56792=CARTESIAN_POINT('Ctrl Pts',(20.4648800132238,0.607389293586315,40.41865156511));
#56793=CARTESIAN_POINT('Ctrl Pts',(20.3867762105732,0.60315670980339,40.4316077294079));
#56794=CARTESIAN_POINT('Ctrl Pts',(20.3087623158836,0.598928998292557,40.4445489794216));
#56795=CARTESIAN_POINT('Ctrl Pts',(20.2300122320118,0.594701286781725,40.4535847803177));
#56796=CARTESIAN_POINT('Ctrl Pts',(20.1509495880502,0.590473575270893,40.4586446664912));
#56797=CARTESIAN_POINT('Ctrl Pts',(20.0719366740902,0.586248522969131,40.463701370022));
#56798=CARTESIAN_POINT('Ctrl Pts',(19.992612056607,0.58202347066737,40.4647870929481));
#56799=CARTESIAN_POINT('Ctrl Pts',(19.913405348292,0.577798418365609,40.4618831061667));
#56800=CARTESIAN_POINT('Ctrl Pts',(19.83422383386,0.573574709958516,40.4589800430786));
#56801=CARTESIAN_POINT('Ctrl Pts',(19.7551606219727,0.569351001551423,40.4520898075416));
#56802=CARTESIAN_POINT('Ctrl Pts',(19.676644700725,0.565127293144331,40.4412457776429));
#56803=CARTESIAN_POINT('Ctrl Pts',(19.5981293423155,0.560903615014718,40.4304018254792));
#56804=CARTESIAN_POINT('Ctrl Pts',(19.5201617306439,0.556679936885105,40.4156042008339));
#56805=CARTESIAN_POINT('Ctrl Pts',(19.4431636280474,0.552456258755492,40.3969378954971));
#56806=CARTESIAN_POINT('Ctrl Pts',(19.3660889562055,0.548228380472418,40.3782530278209));
#56807=CARTESIAN_POINT('Ctrl Pts',(19.289986175618,0.544000502189343,40.3556919054373));
#56808=CARTESIAN_POINT('Ctrl Pts',(19.215264182522,0.539772623906269,40.3293900819882));
#56809=CARTESIAN_POINT('Ctrl Pts',(19.1405059468101,0.53554269496364,40.3030755012925));
#56810=CARTESIAN_POINT('Ctrl Pts',(19.0671302668755,0.531312766021011,40.2730167828784));
#56811=CARTESIAN_POINT('Ctrl Pts',(18.9955258770044,0.527082837078382,40.2393976201567));
#56812=CARTESIAN_POINT('Ctrl Pts',(18.923792977181,0.522845316590492,40.2057181203942));
#56813=CARTESIAN_POINT('Ctrl Pts',(18.8538381338368,0.518607796102602,40.1684656291719));
#56814=CARTESIAN_POINT('Ctrl Pts',(18.7860250899914,0.514370275614712,40.1278696602025));
#56815=CARTESIAN_POINT('Ctrl Pts',(18.7245596072136,0.510529403301667,40.0910736296744));
#56816=CARTESIAN_POINT('Ctrl Pts',(18.6648535817497,0.506688530988621,40.0515314697525));
#56817=CARTESIAN_POINT('Ctrl Pts',(18.607154751171,0.502847658675575,40.0094429956703));
#56818=CARTESIAN_POINT('Ctrl Pts',(18.5440944950677,0.498649889166365,39.9634436239674));
#56819=CARTESIAN_POINT('Ctrl Pts',(18.4831856799924,0.494452119657154,39.9142221837444));
#56820=CARTESIAN_POINT('Ctrl Pts',(18.424780789985,0.490254350147943,39.8620087631167));
#56821=CARTESIAN_POINT('Ctrl Pts',(18.3664603959426,0.486062653667637,39.8098708810844));
#56822=CARTESIAN_POINT('Ctrl Pts',(18.3106370903089,0.481870957187332,39.754749926423));
#56823=CARTESIAN_POINT('Ctrl Pts',(18.2576331101625,0.477679260707026,39.6969183016354));
#56824=CARTESIAN_POINT('Ctrl Pts',(18.2046896945328,0.473492353830652,39.6391527576288));
#56825=CARTESIAN_POINT('Ctrl Pts',(18.154559527168,0.469305446954278,39.5786830466592));
#56826=CARTESIAN_POINT('Ctrl Pts',(18.1075293268368,0.465118540077904,39.5158196184957));
#56827=CARTESIAN_POINT('Ctrl Pts',(18.0605277904194,0.46093418503284,39.4529945042639));
#56828=CARTESIAN_POINT('Ctrl Pts',(18.016622758633,0.456749829987776,39.3877789494164));
#56829=CARTESIAN_POINT('Ctrl Pts',(17.9760609471667,0.452565474942712,39.3205167558524));
#56830=CARTESIAN_POINT('Ctrl Pts',(17.935510634744,0.448382306138573,39.2532736307388));
#56831=CARTESIAN_POINT('Ctrl Pts',(17.8983019079526,0.444199137334434,39.1839854283694));
#56832=CARTESIAN_POINT('Ctrl Pts',(17.8646374777929,0.440015968530295,39.1130238593703));
#56833=CARTESIAN_POINT('Ctrl Pts',(17.8309716174094,0.435832622005396,39.0420592755888));
#56834=CARTESIAN_POINT('Ctrl Pts',(17.8008505554083,0.431649275480497,38.9694216174508));
#56835=CARTESIAN_POINT('Ctrl Pts',(17.7744297561447,0.427465928955598,38.8955045760811));
#56836=CARTESIAN_POINT('Ctrl Pts',(17.7479829229321,0.423278460336241,38.8215146999547));
#56837=CARTESIAN_POINT('Ctrl Pts',(17.725243790005,0.419090991716885,38.7462433761688));
#56838=CARTESIAN_POINT('Ctrl Pts',(17.7063183315099,0.414903523097528,38.6701007319173));
#56839=CARTESIAN_POINT('Ctrl Pts',(17.6873823111652,0.410713717551214,38.5939155942613));
#56840=CARTESIAN_POINT('Ctrl Pts',(17.6722642913954,0.4065239120049,38.5168586381407));
#56841=CARTESIAN_POINT('Ctrl Pts',(17.6610188679983,0.402334106458586,38.4393489428891));
#56842=CARTESIAN_POINT('Ctrl Pts',(17.6497553295379,0.398137551625042,38.3617143885742));
#56843=CARTESIAN_POINT('Ctrl Pts',(17.6423768800543,0.3939409967915,38.2836261155568));
#56844=CARTESIAN_POINT('Ctrl Pts',(17.6388860990133,0.389744441957957,38.2055063385164));
#56845=CARTESIAN_POINT('Ctrl Pts',(17.6373007618979,0.387838577896013,38.1700282662658));
#56846=CARTESIAN_POINT('Ctrl Pts',(17.6365165509045,0.38593271383407,38.1345436670864));
#56847=CARTESIAN_POINT('Ctrl Pts',(17.6365301745119,0.384026849772126,38.099091756019));
#56848=CARTESIAN_POINT('Origin',(20.,-1.3495818343519,38.1));
#56849=CARTESIAN_POINT('',(18.0708707491416,21.2722931656887,38.0982998874535));
#56850=CARTESIAN_POINT('Ctrl Pts',(19.3941040087494,21.1141809091495,36.2684889831927));
#56851=CARTESIAN_POINT('Ctrl Pts',(19.3627036109449,21.1163561899284,36.2788767859298));
#56852=CARTESIAN_POINT('Ctrl Pts',(19.3315975445805,21.1185314707073,36.2900633660934));
#56853=CARTESIAN_POINT('Ctrl Pts',(19.3008283950407,21.1207067514863,36.3020284697141));
#56854=CARTESIAN_POINT('Ctrl Pts',(19.2377524129147,21.1251660223333,36.3265566309862));
#56855=CARTESIAN_POINT('Ctrl Pts',(19.175844332916,21.1296252931803,36.3544564075852));
#56856=CARTESIAN_POINT('Ctrl Pts',(19.1154887940643,21.1340845640273,36.3855955892864));
#56857=CARTESIAN_POINT('Ctrl Pts',(19.0521316315247,21.1387656049598,36.4182833961378));
#56858=CARTESIAN_POINT('Ctrl Pts',(18.9904859997409,21.1434466458922,36.4545411133358));
#56859=CARTESIAN_POINT('Ctrl Pts',(18.9309759297778,21.1481276868246,36.4941575126478));
#56860=CARTESIAN_POINT('Ctrl Pts',(18.8744391227793,21.15257485195,36.5317945835379));
#56861=CARTESIAN_POINT('Ctrl Pts',(18.8198300706574,21.1570220170753,36.572462458363));
#56862=CARTESIAN_POINT('Ctrl Pts',(18.7674873179353,21.1614691822007,36.6159329376846));
#56863=CARTESIAN_POINT('Ctrl Pts',(18.7151762470697,21.1659136555599,36.6593771053313));
#56864=CARTESIAN_POINT('Ctrl Pts',(18.6651291328328,21.1703581289192,36.7056201980804));
#56865=CARTESIAN_POINT('Ctrl Pts',(18.6176531092621,21.1748026022785,36.7543924678543));
#56866=CARTESIAN_POINT('Ctrl Pts',(18.5701894778516,21.1792459155442,36.8031520071227));
#56867=CARTESIAN_POINT('Ctrl Pts',(18.5252959483506,21.18368922881,36.8544390596418));
#56868=CARTESIAN_POINT('Ctrl Pts',(18.4832429671676,21.1881325420758,36.907946871883));
#56869=CARTESIAN_POINT('Ctrl Pts',(18.4411864860854,21.1925762251405,36.9614591373626));
#56870=CARTESIAN_POINT('Ctrl Pts',(18.4019713250343,21.1970199082052,37.017192140241));
#56871=CARTESIAN_POINT('Ctrl Pts',(18.3658266378197,21.2014635912699,37.0748073453052));
#56872=CARTESIAN_POINT('Ctrl Pts',(18.3296431725879,21.2059120417633,37.1324843631441));
#56873=CARTESIAN_POINT('Ctrl Pts',(18.2965370163799,21.2103604922567,37.1920471940158));
#56874=CARTESIAN_POINT('Ctrl Pts',(18.2666925266657,21.2148089427501,37.2531306123235));
#56875=CARTESIAN_POINT('Ctrl Pts',(18.2368294566097,21.2192601627239,37.3142520594534));
#56876=CARTESIAN_POINT('Ctrl Pts',(18.2102322864395,21.2237113826978,37.3768955242203));
#56877=CARTESIAN_POINT('Ctrl Pts',(18.1870370415035,21.2281626026716,37.4406762039639));
#56878=CARTESIAN_POINT('Ctrl Pts',(18.1638027062202,21.2326213241715,37.5045643716398));
#56879=CARTESIAN_POINT('Ctrl Pts',(18.1439818790603,21.2370800456714,37.5695931074238));
#56880=CARTESIAN_POINT('Ctrl Pts',(18.1276603449738,21.2415387671712,37.6353638271547));
#56881=CARTESIAN_POINT('Ctrl Pts',(18.1216926387617,21.243169026916,37.6594118321176));
#56882=CARTESIAN_POINT('Ctrl Pts',(18.1161922483818,21.2447992866606,37.6835589537376));
#56883=CARTESIAN_POINT('Ctrl Pts',(18.1111616393731,21.2464295464053,37.7077855123479));
#56884=CARTESIAN_POINT('Ctrl Pts',(18.0918301223393,21.2526942737912,37.8008828152065));
#56885=CARTESIAN_POINT('Ctrl Pts',(18.0793762649212,21.258959001177,37.8954539813234));
#56886=CARTESIAN_POINT('Ctrl Pts',(18.0739715027794,21.2652237285629,37.9906529159316));
#56887=CARTESIAN_POINT('Ctrl Pts',(18.0719384999277,21.2675802075913,38.0264620228749));
#56888=CARTESIAN_POINT('Ctrl Pts',(18.0709024226888,21.2699366866197,38.06235971154));
#56889=CARTESIAN_POINT('Ctrl Pts',(18.0708707491422,21.2722931656481,38.098299886834));
#56890=CARTESIAN_POINT('',(21.5476173497497,21.75,36.9482955693174));
#56891=CARTESIAN_POINT('Ctrl Pts',(18.0708707491416,21.2722931656887,38.0982998874535));
#56892=CARTESIAN_POINT('Ctrl Pts',(18.0708117642268,21.2766815837971,38.1652304708287));
#56893=CARTESIAN_POINT('Ctrl Pts',(18.0742402209119,21.2810700019056,38.2322696432489));
#56894=CARTESIAN_POINT('Ctrl Pts',(18.0811633913888,21.285458420014,38.2990191607702));
#56895=CARTESIAN_POINT('Ctrl Pts',(18.0880808002805,21.289843186003,38.3657131281579));
#56896=CARTESIAN_POINT('Ctrl Pts',(18.0984871082126,21.294227951992,38.4321174151031));
#56897=CARTESIAN_POINT('Ctrl Pts',(18.1123375584943,21.2986127179809,38.4978354733163));
#56898=CARTESIAN_POINT('Ctrl Pts',(18.1261815683776,21.302995445073,38.5635229729216));
#56899=CARTESIAN_POINT('Ctrl Pts',(18.1434664408058,21.3073781721651,38.6285243800003));
#56900=CARTESIAN_POINT('Ctrl Pts',(18.1640960781561,21.3117608992572,38.6924519783564));
#56901=CARTESIAN_POINT('Ctrl Pts',(18.1847236974656,21.3161431976203,38.7563733231606));
#56902=CARTESIAN_POINT('Ctrl Pts',(18.2086952744819,21.3205254959835,38.8192205848984));
#56903=CARTESIAN_POINT('Ctrl Pts',(18.2358650602611,21.3249077943466,38.8806218491001));
#56904=CARTESIAN_POINT('Ctrl Pts',(18.2630601717377,21.3292941775695,38.9420803470929));
#56905=CARTESIAN_POINT('Ctrl Pts',(18.2934592370428,21.3336805607923,39.0020896913925));
#56906=CARTESIAN_POINT('Ctrl Pts',(18.3268691145082,21.3380669440151,39.0602997432642));
#56907=CARTESIAN_POINT('Ctrl Pts',(18.3602957555656,21.3424555281302,39.1185390023536));
#56908=CARTESIAN_POINT('Ctrl Pts',(18.3967359379642,21.3468441122452,39.1749767463128));
#56909=CARTESIAN_POINT('Ctrl Pts',(18.4359530809998,21.3512326963603,39.2292917214192));
#56910=CARTESIAN_POINT('Ctrl Pts',(18.4752380586776,21.3556288714932,39.2837006461767));
#56911=CARTESIAN_POINT('Ctrl Pts',(18.5173092640418,21.3600250466261,39.3359790791136));
#56912=CARTESIAN_POINT('Ctrl Pts',(18.5618904093106,21.364421221759,39.3858395553362));
#56913=CARTESIAN_POINT('Ctrl Pts',(18.5880238968701,21.3669982616141,39.4150677890933));
#56914=CARTESIAN_POINT('Ctrl Pts',(18.6150191785668,21.3695753014693,39.4434658355131));
#56915=CARTESIAN_POINT('Ctrl Pts',(18.6428152478348,21.3721523413244,39.4709821681518));
#56916=CARTESIAN_POINT('Ctrl Pts',(18.6908402055143,21.3766048496553,39.5185238078611));
#56917=CARTESIAN_POINT('Ctrl Pts',(18.7414626085893,21.3810573579862,39.5636343380257));
#56918=CARTESIAN_POINT('Ctrl Pts',(18.7944061999614,21.385509866317,39.6060166487156));
#56919=CARTESIAN_POINT('Ctrl Pts',(18.8472699163602,21.3899556572346,39.6483350180323));
#56920=CARTESIAN_POINT('Ctrl Pts',(18.902447488726,21.3944014481522,39.6879330292911));
#56921=CARTESIAN_POINT('Ctrl Pts',(18.9596262385859,21.3988472390698,39.7245507051062));
#56922=CARTESIAN_POINT('Ctrl Pts',(19.0167381012465,21.4032878293402,39.7611255458857));
#56923=CARTESIAN_POINT('Ctrl Pts',(19.0758460782621,21.4077284196106,39.7947267089443));
#56924=CARTESIAN_POINT('Ctrl Pts',(19.1366063571682,21.412169009881,39.8251359292582));
#56925=CARTESIAN_POINT('Ctrl Pts',(19.1973289329325,21.4166068446637,39.8555262799559));
#56926=CARTESIAN_POINT('Ctrl Pts',(19.2597013356713,21.4210446794463,39.8827283956558));
#56927=CARTESIAN_POINT('Ctrl Pts',(19.3233542501424,21.425482514229,39.9065694246554));
#56928=CARTESIAN_POINT('Ctrl Pts',(19.38698975622,21.4299191353112,39.9304039333877));
#56929=CARTESIAN_POINT('Ctrl Pts',(19.4519046159155,21.4343557563933,39.9508790067391));
#56930=CARTESIAN_POINT('Ctrl Pts',(19.5177103068475,21.4387923774755,39.9678702333885));
#56931=CARTESIAN_POINT('Ctrl Pts',(19.5835208368066,21.4432293248049,39.9848627094893));
#56932=CARTESIAN_POINT('Ctrl Pts',(19.6502218485231,21.4476662721344,39.998370709307));
#56933=CARTESIAN_POINT('Ctrl Pts',(19.7174122649928,21.4521032194638,40.008320394725));
#56934=CARTESIAN_POINT('Ctrl Pts',(19.7846756128002,21.4565449828448,40.0182808799551));
#56935=CARTESIAN_POINT('Ctrl Pts',(19.852428935245,21.4609867462257,40.024675271164));
#56936=CARTESIAN_POINT('Ctrl Pts',(19.920264669978,21.4654285096066,40.0274814743718));
#56937=CARTESIAN_POINT('Ctrl Pts',(19.9881423296492,21.469873018158,40.0302894119146));
#56938=CARTESIAN_POINT('Ctrl Pts',(20.0561020084809,21.4743175267094,40.0295047546418));
#56939=CARTESIAN_POINT('Ctrl Pts',(20.123737637891,21.4787620352608,40.0251575400131));
#56940=CARTESIAN_POINT('Ctrl Pts',(20.1914905344253,21.483214249732,40.0208027881535));
#56941=CARTESIAN_POINT('Ctrl Pts',(20.2589177697175,21.4876664642032,40.0128732109645));
#56942=CARTESIAN_POINT('Ctrl Pts',(20.3256208080778,21.4921186786744,40.0014504059393));
#56943=CARTESIAN_POINT('Ctrl Pts',(20.3543685404356,21.4940374978641,39.996527395688));
#56944=CARTESIAN_POINT('Ctrl Pts',(20.3829819219436,21.4959563170538,39.9909561758273));
#56945=CARTESIAN_POINT('Ctrl Pts',(20.4114299415252,21.4978751362435,39.984746126171));
#56946=CARTESIAN_POINT('Ctrl Pts',(20.4776508976573,21.5023417403606,39.9702904476417));
#56947=CARTESIAN_POINT('Ctrl Pts',(20.5432377940952,21.5068083444777,39.952312427416));
#56948=CARTESIAN_POINT('Ctrl Pts',(20.6077891663749,21.5112749485948,39.9308836353349));
#56949=CARTESIAN_POINT('Ctrl Pts',(20.6754263324151,21.5159550728685,39.9084304679298));
#56950=CARTESIAN_POINT('Ctrl Pts',(20.7419259401755,21.5206351971421,39.8821883482491));
#56951=CARTESIAN_POINT('Ctrl Pts',(20.8068377368834,21.5253153214158,39.8523000380188));
#56952=CARTESIAN_POINT('Ctrl Pts',(20.8686190326334,21.529769737355,39.8238531512054));
#56953=CARTESIAN_POINT('Ctrl Pts',(20.9289616178721,21.5342241532942,39.7921038646062));
#56954=CARTESIAN_POINT('Ctrl Pts',(20.9874947374449,21.5386785692334,39.757225603356));
#56955=CARTESIAN_POINT('Ctrl Pts',(21.045991836734,21.543130244001,39.722368805593));
#56956=CARTESIAN_POINT('Ctrl Pts',(21.102681258503,21.5475819187686,39.6843871042582));
#56957=CARTESIAN_POINT('Ctrl Pts',(21.157216832345,21.5520335935361,39.6434998412172));
#56958=CARTESIAN_POINT('Ctrl Pts',(21.2117374550972,21.5564840478638,39.602623787541));
#56959=CARTESIAN_POINT('Ctrl Pts',(21.2641050095886,21.5609345021915,39.5588440483339));
#56960=CARTESIAN_POINT('Ctrl Pts',(21.3140038091691,21.5653849565192,39.5124222266692));
#56961=CARTESIAN_POINT('Ctrl Pts',(21.3639059550048,21.5698357092981,39.4659972919183));
#56962=CARTESIAN_POINT('Ctrl Pts',(21.4113386595033,21.574286462077,39.4169302594691));
#56963=CARTESIAN_POINT('Ctrl Pts',(21.4560220645719,21.5787372148559,39.3655205665575));
#56964=CARTESIAN_POINT('Ctrl Pts',(21.5007518148429,21.5831925839132,39.3140575520017));
#56965=CARTESIAN_POINT('Ctrl Pts',(21.5427262529987,21.5876479529705,39.2602473999785));
#56966=CARTESIAN_POINT('Ctrl Pts',(21.5817056006401,21.5921033220278,39.2044229035128));
#56967=CARTESIAN_POINT('Ctrl Pts',(21.6207084830151,21.596561381123,39.1485647016434));
#56968=CARTESIAN_POINT('Ctrl Pts',(21.6567124160615,21.6010194402183,39.0906901516005));
#56969=CARTESIAN_POINT('Ctrl Pts',(21.6895222800999,21.6054774993135,39.0311589670654));
#56970=CARTESIAN_POINT('Ctrl Pts',(21.7223860199728,21.6099428788186,38.9715300286277));
#56971=CARTESIAN_POINT('Ctrl Pts',(21.7520450113432,21.6144082583238,38.9102394691559));
#56972=CARTESIAN_POINT('Ctrl Pts',(21.7783515883805,21.618873637829,38.8476684994063));
#56973=CARTESIAN_POINT('Ctrl Pts',(21.7876288876848,21.6204484022735,38.8256021692523));
#56974=CARTESIAN_POINT('Ctrl Pts',(21.7964896994039,21.6220231667181,38.8033767407199));
#56975=CARTESIAN_POINT('Ctrl Pts',(21.8049290351548,21.6235979311626,38.7810093501232));
#56976=CARTESIAN_POINT('Ctrl Pts',(21.8288495946408,21.6280614633273,38.7176109366569));
#56977=CARTESIAN_POINT('Ctrl Pts',(21.8494717851415,21.632524995492,38.652828802607));
#56978=CARTESIAN_POINT('Ctrl Pts',(21.866637600227,21.6369885276567,38.5870386291853));
#56979=CARTESIAN_POINT('Ctrl Pts',(21.8846378602152,21.6416690359244,38.5180503393572));
#56980=CARTESIAN_POINT('Ctrl Pts',(21.8988368583806,21.6463495441921,38.4479539776668));
#56981=CARTESIAN_POINT('Ctrl Pts',(21.9091096038987,21.6510300524598,38.3772058390467));
#56982=CARTESIAN_POINT('Ctrl Pts',(21.9188801237923,21.6554817347351,38.3099165156038));
#56983=CARTESIAN_POINT('Ctrl Pts',(21.9250992104239,21.6599334170103,38.2420382053687));
#56984=CARTESIAN_POINT('Ctrl Pts',(21.9277111001389,21.6643850992856,38.1739761535979));
#56985=CARTESIAN_POINT('Ctrl Pts',(21.9303214576001,21.6688341700006,38.1059540301361));
#56986=CARTESIAN_POINT('Ctrl Pts',(21.9293287975894,21.6732832407157,38.0377488693417));
#56987=CARTESIAN_POINT('Ctrl Pts',(21.9247292680504,21.6777323114308,37.96977019692));
#56988=CARTESIAN_POINT('Ctrl Pts',(21.9201308633023,21.6821802941488,37.9018081483282));
#56989=CARTESIAN_POINT('Ctrl Pts',(21.9119273736502,21.6866282768668,37.834072968505));
#56990=CARTESIAN_POINT('Ctrl Pts',(21.9001669892711,21.6910762595848,37.7669715180585));
#56991=CARTESIAN_POINT('Ctrl Pts',(21.888405457762,21.6955246761675,37.69986352241));
#56992=CARTESIAN_POINT('Ctrl Pts',(21.8730864303068,21.6999730927501,37.6333898626534));
#56993=CARTESIAN_POINT('Ctrl Pts',(21.8543093192622,21.7044215093328,37.5679478358305));
#56994=CARTESIAN_POINT('Ctrl Pts',(21.835511817859,21.7088747565206,37.5024347444871));
#56995=CARTESIAN_POINT('Ctrl Pts',(21.8132488761256,21.7133280037083,37.437955994717));
#56996=CARTESIAN_POINT('Ctrl Pts',(21.7876696778375,21.7177812508961,37.3748933320949));
#56997=CARTESIAN_POINT('Ctrl Pts',(21.7620743308935,21.7222373095073,37.3117908567617));
#56998=CARTESIAN_POINT('Ctrl Pts',(21.733158769686,21.7266933681184,37.2501066927458));
#56999=CARTESIAN_POINT('Ctrl Pts',(21.701119016288,21.7311494267296,37.1901996651334));
#57000=CARTESIAN_POINT('Ctrl Pts',(21.6690252080924,21.7356130032309,37.1301915673846));
#57001=CARTESIAN_POINT('Ctrl Pts',(21.6337969447907,21.7400765797321,37.0719670086048));
#57002=CARTESIAN_POINT('Ctrl Pts',(21.5956740511215,21.7445401562334,37.0158566148901));
#57003=CARTESIAN_POINT('Ctrl Pts',(21.582063951989,21.7461336795162,36.9958248715643));
#57004=CARTESIAN_POINT('Ctrl Pts',(21.5680852976313,21.7477272027989,36.9760622789677));
#57005=CARTESIAN_POINT('Ctrl Pts',(21.553750203327,21.7493207260817,36.9565828134224));
#57006=CARTESIAN_POINT('Ctrl Pts',(21.5517133215352,21.7495471507211,36.953814964963));
#57007=CARTESIAN_POINT('Ctrl Pts',(21.5496690309495,21.7497735753606,36.9510525417979));
#57008=CARTESIAN_POINT('Ctrl Pts',(21.5476173497497,21.75,36.9482955693174));
#57009=CARTESIAN_POINT('',(21.45785946511,21.75,39.3634034735148));
#57010=CARTESIAN_POINT('Origin',(20.,21.75,38.1));
#57011=CARTESIAN_POINT('',(18.0708701150598,21.4433318344123,38.100666281098));
#57012=CARTESIAN_POINT('Ctrl Pts',(18.0708701150598,21.4433318344123,38.100666281098));
#57013=CARTESIAN_POINT('Ctrl Pts',(18.0708957469507,21.4481676676054,38.1748800730484));
#57014=CARTESIAN_POINT('Ctrl Pts',(18.0752081170122,21.4530035007986,38.2489637478113));
#57015=CARTESIAN_POINT('Ctrl Pts',(18.0837371745069,21.4578393339917,38.3224395210687));
#57016=CARTESIAN_POINT('Ctrl Pts',(18.0922900823321,21.462688689924,38.3961207591715));
#57017=CARTESIAN_POINT('Ctrl Pts',(18.105083161469,21.4675380458563,38.469190363243));
#57018=CARTESIAN_POINT('Ctrl Pts',(18.1219954280233,21.4723874017887,38.541181804401));
#57019=CARTESIAN_POINT('Ctrl Pts',(18.1389805387895,21.4772576447801,38.6134833258064));
#57020=CARTESIAN_POINT('Ctrl Pts',(18.160120250225,21.4821278877716,38.684697057785));
#57021=CARTESIAN_POINT('Ctrl Pts',(18.1852433867281,21.486998130763,38.7543706835472));
#57022=CARTESIAN_POINT('Ctrl Pts',(18.2051143996883,21.490850223896,38.8094786721667));
#57023=CARTESIAN_POINT('Ctrl Pts',(18.2274764284197,21.4947023170289,38.8636235298763));
#57024=CARTESIAN_POINT('Ctrl Pts',(18.252224385491,21.4985544101619,38.9165922839629));
#57025=CARTESIAN_POINT('Ctrl Pts',(18.2805717918491,21.5029667682831,38.9772650413967));
#57026=CARTESIAN_POINT('Ctrl Pts',(18.3121450401223,21.5073791264044,39.0365939290971));
#57027=CARTESIAN_POINT('Ctrl Pts',(18.3467935985325,21.5117914845257,39.0942088065628));
#57028=CARTESIAN_POINT('Ctrl Pts',(18.3813893343138,21.5161971158922,39.1517358486485));
#57029=CARTESIAN_POINT('Ctrl Pts',(18.4190508245653,21.5206027472587,39.2075536347135));
#57030=CARTESIAN_POINT('Ctrl Pts',(18.4595803006785,21.5250083786252,39.2613137848326));
#57031=CARTESIAN_POINT('Ctrl Pts',(18.5000634584664,21.5294089751014,39.3150124962074));
#57032=CARTESIAN_POINT('Ctrl Pts',(18.5434077962888,21.5338095715776,39.366657837327));
#57033=CARTESIAN_POINT('Ctrl Pts',(18.5893716704543,21.5382101680538,39.415929433056));
#57034=CARTESIAN_POINT('Ctrl Pts',(18.6353079755125,21.5426081250545,39.4651714757082));
#57035=CARTESIAN_POINT('Ctrl Pts',(18.6838603595823,21.5470060820553,39.5120422270587));
#57036=CARTESIAN_POINT('Ctrl Pts',(18.7347473629116,21.5514040390561,39.5562548956968));
#57037=CARTESIAN_POINT('Ctrl Pts',(18.7856222591027,21.5558009496861,39.6004570451678));
#57038=CARTESIAN_POINT('Ctrl Pts',(18.8388302921501,21.5601978603161,39.6420020359081));
#57039=CARTESIAN_POINT('Ctrl Pts',(18.8940551187641,21.5645947709461,39.6806417926172));
#57040=CARTESIAN_POINT('Ctrl Pts',(18.9492867909995,21.5689922266133,39.7192863390769));
#57041=CARTESIAN_POINT('Ctrl Pts',(19.0065353380151,21.5733896822805,39.7550246503077));
#57042=CARTESIAN_POINT('Ctrl Pts',(19.0654551368492,21.5777871379478,39.7876517578157));
#57043=CARTESIAN_POINT('Ctrl Pts',(19.1244473456659,21.5821899979051,39.820318962682));
#57044=CARTESIAN_POINT('Ctrl Pts',(19.1851144618776,21.5865928578625,39.8498670911014));
#57045=CARTESIAN_POINT('Ctrl Pts',(19.2470869161592,21.5909957178198,39.8761375073686));
#57046=CARTESIAN_POINT('Ctrl Pts',(19.3091017949215,21.5954015918429,39.9024259075736));
#57047=CARTESIAN_POINT('Ctrl Pts',(19.3724233142563,21.5998074658659,39.9254319640702));
#57048=CARTESIAN_POINT('Ctrl Pts',(19.436665530953,21.6042133398889,39.9450465665895));
#57049=CARTESIAN_POINT('Ctrl Pts',(19.5010320913046,21.6086277416762,39.9646991340404));
#57050=CARTESIAN_POINT('Ctrl Pts',(19.5663224156939,21.6130421434635,39.980947030881));
#57051=CARTESIAN_POINT('Ctrl Pts',(19.6321400638034,21.6174565452508,39.9937321944355));
#57052=CARTESIAN_POINT('Ctrl Pts',(19.6660381856185,21.6197300985275,40.0003169485864));
#57053=CARTESIAN_POINT('Ctrl Pts',(19.7000760964438,21.6220036518042,40.0059840359317));
#57054=CARTESIAN_POINT('Ctrl Pts',(19.7341994520756,21.6242772050809,40.0107309139759));
#57055=CARTESIAN_POINT('Ctrl Pts',(19.802951938091,21.6288580101328,40.0202950280646));
#57056=CARTESIAN_POINT('Ctrl Pts',(19.8723324705866,21.6334388151846,40.0261595313805));
#57057=CARTESIAN_POINT('Ctrl Pts',(19.9419211784638,21.6380196202364,40.0282555347746));
#57058=CARTESIAN_POINT('Ctrl Pts',(20.01280182287,21.6426854693932,40.0303904511395));
#57059=CARTESIAN_POINT('Ctrl Pts',(20.0838979863156,21.64735131855,40.0286153721321));
#57060=CARTESIAN_POINT('Ctrl Pts',(20.1547573315076,21.6520171677069,40.0229125630784));
#57061=CARTESIAN_POINT('Ctrl Pts',(20.2240947373107,21.6565828022823,40.0173322407581));
#57062=CARTESIAN_POINT('Ctrl Pts',(20.2932049107954,21.6611484368578,40.0079912596888));
#57063=CARTESIAN_POINT('Ctrl Pts',(20.3616628893468,21.6657140714332,39.9949254632754));
#57064=CARTESIAN_POINT('Ctrl Pts',(20.4300562009068,21.6702753932045,39.9818720091157));
#57065=CARTESIAN_POINT('Ctrl Pts',(20.4977980913606,21.6748367149759,39.9651008177934));
#57066=CARTESIAN_POINT('Ctrl Pts',(20.5644705860265,21.6793980367472,39.9446993018947));
#57067=CARTESIAN_POINT('Ctrl Pts',(20.631098306068,21.6839562953143,39.9243114868515));
#57068=CARTESIAN_POINT('Ctrl Pts',(20.6966576187536,21.6885145538814,39.9002983283355));
#57069=CARTESIAN_POINT('Ctrl Pts',(20.7607439627118,21.6930728124485,39.8727975575619));
#57070=CARTESIAN_POINT('Ctrl Pts',(20.8274407664053,21.6978167447444,39.8441765847241));
#57071=CARTESIAN_POINT('Ctrl Pts',(20.8925415197652,21.7025606770404,39.8117779140257));
#57072=CARTESIAN_POINT('Ctrl Pts',(20.9556123210989,21.7073046093363,39.7758125338665));
#57073=CARTESIAN_POINT('Ctrl Pts',(21.0161992792482,21.7118617169266,39.7412635359712));
#57074=CARTESIAN_POINT('Ctrl Pts',(21.0749127748468,21.7164188245168,39.7034237799828));
#57075=CARTESIAN_POINT('Ctrl Pts',(21.1313942764615,21.720975932107,39.6625266551615));
#57076=CARTESIAN_POINT('Ctrl Pts',(21.1878812173633,21.7255334785562,39.6216255918612));
#57077=CARTESIAN_POINT('Ctrl Pts',(21.2421353687718,21.7300910250055,39.577666850821));
#57078=CARTESIAN_POINT('Ctrl Pts',(21.2938295118927,21.7346485714547,39.5309254875973));
#57079=CARTESIAN_POINT('Ctrl Pts',(21.3455582994798,21.7392091722879,39.4841527991696));
#57080=CARTESIAN_POINT('Ctrl Pts',(21.3947233205039,21.7437697731212,39.4345940833591));
#57081=CARTESIAN_POINT('Ctrl Pts',(21.441033354978,21.7483303739544,39.3825620557076));
#57082=CARTESIAN_POINT('Ctrl Pts',(21.4466846892762,21.7488869159696,39.3762124516571));
#57083=CARTESIAN_POINT('Ctrl Pts',(21.4522935554523,21.7494434579848,39.3698260568356));
#57084=CARTESIAN_POINT('Ctrl Pts',(21.45785946511,21.75,39.3634034735148));
#57085=CARTESIAN_POINT('Ctrl Pts',(18.0708700849959,21.444817201297,38.1005726573522));
#57086=CARTESIAN_POINT('Ctrl Pts',(18.0708621447113,21.4431312111911,38.0738239558221));
#57087=CARTESIAN_POINT('Ctrl Pts',(18.0714105371302,21.4414297588578,38.0470788578902));
#57088=CARTESIAN_POINT('Ctrl Pts',(18.0728453930802,21.4391969107969,38.0123541562582));
#57089=CARTESIAN_POINT('Ctrl Pts',(18.0732257813741,21.438680981368,38.0043559712711));
#57090=CARTESIAN_POINT('Ctrl Pts',(18.073992734373,21.4377584137641,37.9901006430405));
#57091=CARTESIAN_POINT('Ctrl Pts',(18.0743600285079,21.4373523687922,37.9838425439747));
#57092=CARTESIAN_POINT('Ctrl Pts',(18.0751569577228,21.4365370228772,37.9713089544374));
#57093=CARTESIAN_POINT('Ctrl Pts',(18.0755867960074,21.436127720581,37.9650335546474));
#57094=CARTESIAN_POINT('Ctrl Pts',(18.0765727849264,21.4352493641535,37.9516025025255));
#57095=CARTESIAN_POINT('Ctrl Pts',(18.0771381923196,21.4347800319043,37.9444476448115));
#57096=CARTESIAN_POINT('Ctrl Pts',(18.0787389410611,21.4335356335069,37.9255356745032));
#57097=CARTESIAN_POINT('Ctrl Pts',(18.0798422632143,21.4327584961842,37.9137847668753));
#57098=CARTESIAN_POINT('Ctrl Pts',(18.0850286803668,21.4294161828354,37.8635084173905));
#57099=CARTESIAN_POINT('Ctrl Pts',(18.0901637139054,21.4268191404273,37.8251028789182));
#57100=CARTESIAN_POINT('Ctrl Pts',(18.1216694805466,21.4136383917863,37.6335699464261));
#57101=CARTESIAN_POINT('Ctrl Pts',(18.1653144164803,21.4025341672775,37.4838857843554));
#57102=CARTESIAN_POINT('Ctrl Pts',(18.2558626995096,21.3862392303953,37.2722743844936));
#57103=CARTESIAN_POINT('Ctrl Pts',(18.2892901562238,21.3809912022391,37.2052269950852));
#57104=CARTESIAN_POINT('Ctrl Pts',(18.333534336177,21.374975598533,37.1280777750873));
#57105=CARTESIAN_POINT('Ctrl Pts',(18.3406693203647,21.3740304301354,37.115945965412));
#57106=CARTESIAN_POINT('Ctrl Pts',(18.3507486549677,21.3727302879657,37.0992291893859));
#57107=CARTESIAN_POINT('Ctrl Pts',(18.3535804122822,21.3723687334392,37.0945773240205));
#57108=CARTESIAN_POINT('Ctrl Pts',(18.3584105676622,21.3717583594154,37.0867177222553));
#57109=CARTESIAN_POINT('Ctrl Pts',(18.3603987412837,21.371508906987,37.083503786643));
#57110=CARTESIAN_POINT('Ctrl Pts',(18.36418960164,21.3710366822543,37.0774158192065));
#57111=CARTESIAN_POINT('Ctrl Pts',(18.3659904051399,21.37081380124,37.0745407320344));
#57112=CARTESIAN_POINT('Ctrl Pts',(18.3707638299532,21.3702267695268,37.0669641833853));
#57113=CARTESIAN_POINT('Ctrl Pts',(18.3737492241718,21.3698634419188,37.0622707905371));
#57114=CARTESIAN_POINT('Ctrl Pts',(18.3843722057136,21.3685837511249,37.0457286357568));
#57115=CARTESIAN_POINT('Ctrl Pts',(18.3921195428945,21.3676741976809,37.0339504034153));
#57116=CARTESIAN_POINT('Ctrl Pts',(18.4740450669705,21.3582870123036,36.9123246602368));
#57117=CARTESIAN_POINT('Ctrl Pts',(18.5592388113022,21.3504410898259,36.8102989275548));
#57118=CARTESIAN_POINT('Ctrl Pts',(18.7211152388735,21.3369263369857,36.6526888317364));
#57119=CARTESIAN_POINT('Ctrl Pts',(18.7926282984253,21.3313211867468,36.5925161895644));
#57120=CARTESIAN_POINT('Ctrl Pts',(18.8940316318945,21.3235546398041,36.5190531102441));
#57121=CARTESIAN_POINT('Ctrl Pts',(18.9203098247461,21.3215577163147,36.500991539715));
#57122=CARTESIAN_POINT('Ctrl Pts',(18.959926887435,21.3185618140299,36.4751838048304));
#57123=CARTESIAN_POINT('Ctrl Pts',(18.9729312209725,21.3175806979886,36.4669325030817));
#57124=CARTESIAN_POINT('Ctrl Pts',(18.9938730382735,21.316003560162,36.4539939155586));
#57125=CARTESIAN_POINT('Ctrl Pts',(19.0017479069026,21.3154111298052,36.4492061767031));
#57126=CARTESIAN_POINT('Ctrl Pts',(19.0167546023702,21.3142831780889,36.4402290958583));
#57127=CARTESIAN_POINT('Ctrl Pts',(19.023879674651,21.3137480614945,36.4360288244223));
#57128=CARTESIAN_POINT('Ctrl Pts',(19.0365197796093,21.3127993908049,36.4286865323672));
#57129=CARTESIAN_POINT('Ctrl Pts',(19.0420237565756,21.3123865175655,36.4255256473703));
#57130=CARTESIAN_POINT('Ctrl Pts',(19.0528328874467,21.3115760538106,36.4193887962615));
#57131=CARTESIAN_POINT('Ctrl Pts',(19.0581367202113,21.311178547083,36.4164106444847));
#57132=CARTESIAN_POINT('Ctrl Pts',(19.0708300795819,21.3102275794654,36.4093619577762));
#57133=CARTESIAN_POINT('Ctrl Pts',(19.0782323473301,21.3096733036281,36.4053147426393));
#57134=CARTESIAN_POINT('Ctrl Pts',(19.1049635197194,21.3076725702162,36.3909263326198));
#57135=CARTESIAN_POINT('Ctrl Pts',(19.1244412025445,21.306216346879,36.3808665476503));
#57136=CARTESIAN_POINT('Ctrl Pts',(19.2249999922806,21.2987033875505,36.3310824162271));
#57137=CARTESIAN_POINT('Ctrl Pts',(19.3085497672861,21.2924705746517,36.2967918114816));
#57138=CARTESIAN_POINT('Ctrl Pts',(19.3941043260691,21.2861174117667,36.2684888782178));
#57139=CARTESIAN_POINT('Origin',(20.,21.75,38.1));
#57140=CARTESIAN_POINT('',(17.883581703528,21.75,39.1520285334812));
#57141=CARTESIAN_POINT('Origin',(20.,21.75,38.1));
#57142=CARTESIAN_POINT('Ctrl Pts',(17.883581703528,21.75,39.1520285334812));
#57143=CARTESIAN_POINT('Ctrl Pts',(17.9277932180658,21.7500000000001,39.22297989717));
#57144=CARTESIAN_POINT('Ctrl Pts',(17.9760877855519,21.7500000000001,39.2913445416396));
#57145=CARTESIAN_POINT('Ctrl Pts',(18.0281130771647,21.7500000000001,39.3569276629741));
#57146=CARTESIAN_POINT('Ctrl Pts',(18.0729426874247,21.7500000000001,39.4134399030387));
#57147=CARTESIAN_POINT('Ctrl Pts',(18.1205434589414,21.7500000000001,39.4678864547816));
#57148=CARTESIAN_POINT('Ctrl Pts',(18.1707077965432,21.7500000000001,39.5201173219611));
#57149=CARTESIAN_POINT('Ctrl Pts',(18.1818183450819,21.7500000000001,39.5316855716931));
#57150=CARTESIAN_POINT('Ctrl Pts',(18.1930524042112,21.7500000000001,39.5431425628877));
#57151=CARTESIAN_POINT('Ctrl Pts',(18.2044015768659,21.7500000000001,39.554480823305));
#57152=CARTESIAN_POINT('Ctrl Pts',(18.2631474317285,21.75,39.6131701939873));
#57153=CARTESIAN_POINT('Ctrl Pts',(18.325021894181,21.7500000000001,39.6687306291731));
#57154=CARTESIAN_POINT('Ctrl Pts',(18.3896927432761,21.7500000000001,39.7209522333743));
#57155=CARTESIAN_POINT('Ctrl Pts',(18.4364046733552,21.75,39.7586720400291));
#57156=CARTESIAN_POINT('Ctrl Pts',(18.4845762623831,21.75,39.7946490527158));
#57157=CARTESIAN_POINT('Ctrl Pts',(18.5340885148965,21.7500000000001,39.8287884171533));
#57158=CARTESIAN_POINT('Ctrl Pts',(18.5462898292441,21.7500000000001,39.8372013875997));
#57159=CARTESIAN_POINT('Ctrl Pts',(18.5585725745402,21.75,39.8455026943682));
#57160=CARTESIAN_POINT('Ctrl Pts',(18.570934994616,21.75,39.8536907833519));
#57161=CARTESIAN_POINT('Ctrl Pts',(18.582644131702,21.75,39.8614461788));
#57162=CARTESIAN_POINT('Ctrl Pts',(18.5944162834139,21.7500000000001,39.8690943988968));
#57163=CARTESIAN_POINT('Ctrl Pts',(18.6062494302586,21.7500000000001,39.8766343834877));
#57164=CARTESIAN_POINT('Ctrl Pts',(18.674676426647,21.75,39.9202355071059));
#57165=CARTESIAN_POINT('Ctrl Pts',(18.7451450843928,21.75,39.9602236491718));
#57166=CARTESIAN_POINT('Ctrl Pts',(18.8173443875306,21.75,39.99641011754));
#57167=CARTESIAN_POINT('Ctrl Pts',(18.8887220445928,21.75,40.0321847748735));
#57168=CARTESIAN_POINT('Ctrl Pts',(18.9617921137688,21.75,40.0642440963409));
#57169=CARTESIAN_POINT('Ctrl Pts',(19.0362665833562,21.75,40.0923568791639));
#57170=CARTESIAN_POINT('Ctrl Pts',(19.1085593322196,21.7500000000001,40.1196461013596));
#57171=CARTESIAN_POINT('Ctrl Pts',(19.1821761823731,21.7500000000001,40.1432167252266));
#57172=CARTESIAN_POINT('Ctrl Pts',(19.256853078291,21.75,40.1628082746128));
#57173=CARTESIAN_POINT('Ctrl Pts',(19.2785430184841,21.75,40.1684986495173));
#57174=CARTESIAN_POINT('Ctrl Pts',(19.3003223413584,21.75,40.1738530151002));
#57175=CARTESIAN_POINT('Ctrl Pts',(19.322184426739,21.75,40.1788641632569));
#57176=CARTESIAN_POINT('Ctrl Pts',(19.3343537500359,21.75,40.1816535715383));
#57177=CARTESIAN_POINT('Ctrl Pts',(19.3465487155545,21.75,40.1843366275288));
#57178=CARTESIAN_POINT('Ctrl Pts',(19.3587681675008,21.75,40.1869120359227));
#57179=CARTESIAN_POINT('Ctrl Pts',(19.3718709904236,21.75,40.1896736262369));
#57180=CARTESIAN_POINT('Ctrl Pts',(19.3849932065373,21.75,40.1923095652966));
#57181=CARTESIAN_POINT('Ctrl Pts',(19.3981287272652,21.75,40.1948179331189));
#57182=CARTESIAN_POINT('Ctrl Pts',(19.4729976305839,21.75,40.2091149489636));
#57183=CARTESIAN_POINT('Ctrl Pts',(19.548347373974,21.75,40.2192819902038));
#57184=CARTESIAN_POINT('Ctrl Pts',(19.6239185624981,21.75,40.2251172383339));
#57185=CARTESIAN_POINT('Ctrl Pts',(19.6505037576844,21.75,40.2271700207968));
#57186=CARTESIAN_POINT('Ctrl Pts',(19.6771163593369,21.75,40.2286862521491));
#57187=CARTESIAN_POINT('Ctrl Pts',(19.703744980525,21.75,40.2296555953342));
#57188=CARTESIAN_POINT('Ctrl Pts',(19.7813518609821,21.75,40.2324806646516));
#57189=CARTESIAN_POINT('Ctrl Pts',(19.8590961441614,21.75,40.2306641911219));
#57190=CARTESIAN_POINT('Ctrl Pts',(19.9366408209257,21.75,40.2243619036731));
#57191=CARTESIAN_POINT('Ctrl Pts',(20.0110102784872,21.75,40.2183176757708));
#57192=CARTESIAN_POINT('Ctrl Pts',(20.0851968055271,21.75,40.2081466928086));
#57193=CARTESIAN_POINT('Ctrl Pts',(20.1588811181686,21.75,40.1939470315399));
#57194=CARTESIAN_POINT('Ctrl Pts',(20.1744047711941,21.75,40.1909554773445));
#57195=CARTESIAN_POINT('Ctrl Pts',(20.1899095582806,21.75,40.1877841069774));
#57196=CARTESIAN_POINT('Ctrl Pts',(20.2053667593194,21.75,40.184439537327));
#57197=CARTESIAN_POINT('Ctrl Pts',(20.2795029508407,21.75,40.1683982336304));
#57198=CARTESIAN_POINT('Ctrl Pts',(20.3526602952137,21.75,40.1483566584602));
#57199=CARTESIAN_POINT('Ctrl Pts',(20.4245337957823,21.75,40.1244889058307));
#57200=CARTESIAN_POINT('Ctrl Pts',(20.4961137461482,21.75,40.1007186353549));
#57201=CARTESIAN_POINT('Ctrl Pts',(20.566421180313,21.75,40.0731527585199));
#57202=CARTESIAN_POINT('Ctrl Pts',(20.6351295047781,21.75,40.0419190370673));
#57203=CARTESIAN_POINT('Ctrl Pts',(20.7032602977131,21.75,40.0109478523462));
#57204=CARTESIAN_POINT('Ctrl Pts',(20.7698195230793,21.75,39.9763696283126));
#57205=CARTESIAN_POINT('Ctrl Pts',(20.8344517025453,21.75,39.9382744436647));
#57206=CARTESIAN_POINT('Ctrl Pts',(20.8581546852447,21.75,39.9243035469674));
#57207=CARTESIAN_POINT('Ctrl Pts',(20.881598069502,21.75,39.9098593416072));
#57208=CARTESIAN_POINT('Ctrl Pts',(20.9047627456548,21.75,39.8949453334425));
#57209=CARTESIAN_POINT('Ctrl Pts',(20.9147055515707,21.75,39.8885439018995));
#57210=CARTESIAN_POINT('Ctrl Pts',(20.924595831536,21.75,39.8820565812407));
#57211=CARTESIAN_POINT('Ctrl Pts',(20.9344220826436,21.75,39.8754905971792));
#57212=CARTESIAN_POINT('Ctrl Pts',(20.9953083722281,21.75,39.8348058637445));
#57213=CARTESIAN_POINT('Ctrl Pts',(21.0538466168534,21.75,39.7910353867451));
#57214=CARTESIAN_POINT('Ctrl Pts',(21.109739867734,21.75,39.7443037617988));
#57215=CARTESIAN_POINT('Ctrl Pts',(21.164047120997,21.75,39.6988981689703));
#57216=CARTESIAN_POINT('Ctrl Pts',(21.2158578668268,21.75,39.6506964389093));
#57217=CARTESIAN_POINT('Ctrl Pts',(21.2648614302667,21.75,39.5997839374079));
#57218=CARTESIAN_POINT('Ctrl Pts',(21.3132198492097,21.75,39.5495417120633));
#57219=CARTESIAN_POINT('Ctrl Pts',(21.3588450296455,21.75,39.4966591220955));
#57220=CARTESIAN_POINT('Ctrl Pts',(21.4013929325376,21.75,39.4411979346476));
#57221=CARTESIAN_POINT('Ctrl Pts',(21.4208730776474,21.75,39.4158055673156));
#57222=CARTESIAN_POINT('Ctrl Pts',(21.4397074908361,21.75,39.3898724435325));
#57223=CARTESIAN_POINT('Ctrl Pts',(21.45785946511,21.75,39.3634034735148));
#57224=CARTESIAN_POINT('Ctrl Pts',(21.5504048836412,21.75,36.9462211449553));
#57225=CARTESIAN_POINT('Ctrl Pts',(21.5152004352802,21.75,36.885761931632));
#57226=CARTESIAN_POINT('Ctrl Pts',(21.4764419646285,21.75,36.8275241874393));
#57227=CARTESIAN_POINT('Ctrl Pts',(21.434486940511,21.75,36.7716059964527));
#57228=CARTESIAN_POINT('Ctrl Pts',(21.3986418022227,21.75,36.7238311391881));
#57229=CARTESIAN_POINT('Ctrl Pts',(21.3604621811875,21.75,36.6777494040042));
#57230=CARTESIAN_POINT('Ctrl Pts',(21.3201424774326,21.75,36.63343135754));
#57231=CARTESIAN_POINT('Ctrl Pts',(21.3089460542563,21.75,36.62112463015));
#57232=CARTESIAN_POINT('Ctrl Pts',(21.2975828442927,21.75,36.6089522848169));
#57233=CARTESIAN_POINT('Ctrl Pts',(21.286061915094,21.75,36.5969214204494));
#57234=CARTESIAN_POINT('Ctrl Pts',(21.2354736072089,21.75,36.54409399132));
#57235=CARTESIAN_POINT('Ctrl Pts',(21.1819369929417,21.75,36.494083574989));
#57236=CARTESIAN_POINT('Ctrl Pts',(21.1258151639906,21.75,36.4470065366406));
#57237=CARTESIAN_POINT('Ctrl Pts',(21.0820213593962,21.75,36.4102706950465));
#57238=CARTESIAN_POINT('Ctrl Pts',(21.0366521413219,21.75,36.3753212937733));
#57239=CARTESIAN_POINT('Ctrl Pts',(20.9898607439523,21.75,36.3422241650772));
#57240=CARTESIAN_POINT('Ctrl Pts',(20.9774656288495,21.75,36.3334566833857));
#57241=CARTESIAN_POINT('Ctrl Pts',(20.9649706346163,21.75,36.3248192401923));
#57242=CARTESIAN_POINT('Ctrl Pts',(20.9523784433775,21.75,36.316313194054));
#57243=CARTESIAN_POINT('Ctrl Pts',(20.9403661339154,21.75,36.3081988590208));
#57244=CARTESIAN_POINT('Ctrl Pts',(20.928272392671,21.75,36.3002088768254));
#57245=CARTESIAN_POINT('Ctrl Pts',(20.9161036367489,21.75,36.2923464263246));
#57246=CARTESIAN_POINT('Ctrl Pts',(20.8521530733458,21.75,36.251026825334));
#57247=CARTESIAN_POINT('Ctrl Pts',(20.7861025993975,21.75,36.2132056325107));
#57248=CARTESIAN_POINT('Ctrl Pts',(20.7183291552492,21.75,36.1790042619072));
#57249=CARTESIAN_POINT('Ctrl Pts',(20.6505632332243,21.75,36.1448066872879));
#57250=CARTESIAN_POINT('Ctrl Pts',(20.5810738836283,21.7499999999999,36.1142275037117));
#57251=CARTESIAN_POINT('Ctrl Pts',(20.5101966664877,21.75,36.0874199201387));
#57252=CARTESIAN_POINT('Ctrl Pts',(20.4392415021213,21.75,36.0605828549234));
#57253=CARTESIAN_POINT('Ctrl Pts',(20.3668945577923,21.75,36.0375250306173));
#57254=CARTESIAN_POINT('Ctrl Pts',(20.2934638749207,21.75,36.0184417253472));
#57255=CARTESIAN_POINT('Ctrl Pts',(20.2698818894381,21.7499999999999,36.0123131941905));
#57256=CARTESIAN_POINT('Ctrl Pts',(20.2461879660648,21.7499999999999,36.0065949361045));
#57257=CARTESIAN_POINT('Ctrl Pts',(20.2223919096731,21.7499999999999,36.0012945023363));
#57258=CARTESIAN_POINT('Ctrl Pts',(20.2103027038764,21.7499999999999,35.9986017017486));
#57259=CARTESIAN_POINT('Ctrl Pts',(20.1981910225857,21.7499999999999,35.9960176758035));
#57260=CARTESIAN_POINT('Ctrl Pts',(20.1860677365327,21.75,35.9935450303039));
#57261=CARTESIAN_POINT('Ctrl Pts',(20.1090016189117,21.75,35.9778267516066));
#57262=CARTESIAN_POINT('Ctrl Pts',(20.0313570587203,21.75,35.9665807998749));
#57263=CARTESIAN_POINT('Ctrl Pts',(19.9534981235114,21.75,35.9599575860445));
#57264=CARTESIAN_POINT('Ctrl Pts',(19.9266953868611,21.75,35.9576775618494));
#57265=CARTESIAN_POINT('Ctrl Pts',(19.8998669686043,21.75,35.9559457213365));
#57266=CARTESIAN_POINT('Ctrl Pts',(19.873026956781,21.75,35.9547694100208));
#57267=CARTESIAN_POINT('Ctrl Pts',(19.796957402718,21.75,35.9514355263469));
#57268=CARTESIAN_POINT('Ctrl Pts',(19.7207955629966,21.75,35.9525599283831));
#57269=CARTESIAN_POINT('Ctrl Pts',(19.6448113276275,21.75,35.9579222236047));
#57270=CARTESIAN_POINT('Ctrl Pts',(19.5688270922584,21.75,35.9632845188263));
#57271=CARTESIAN_POINT('Ctrl Pts',(19.4930196712211,21.75,35.9728849486848));
#57272=CARTESIAN_POINT('Ctrl Pts',(19.4176534273628,21.75,35.9865551032572));
#57273=CARTESIAN_POINT('Ctrl Pts',(19.4003670978281,21.75,35.9896905493751));
#57274=CARTESIAN_POINT('Ctrl Pts',(19.3830988100698,21.75,35.9930415012686));
#57275=CARTESIAN_POINT('Ctrl Pts',(19.3658826346092,21.75,35.9965995273322));
#57276=CARTESIAN_POINT('Ctrl Pts',(19.2892535472449,21.75,36.0124362786883));
#57277=CARTESIAN_POINT('Ctrl Pts',(19.2135567969655,21.75,36.0323869962119));
#57278=CARTESIAN_POINT('Ctrl Pts',(19.1390725001544,21.75,36.0561990525511));
#57279=CARTESIAN_POINT('Ctrl Pts',(19.0622735673651,21.75,36.0807510801953));
#57280=CARTESIAN_POINT('Ctrl Pts',(18.9867627690563,21.75,36.1094081944649));
#57281=CARTESIAN_POINT('Ctrl Pts',(18.912841317696,21.75,36.1419496464839));
#57282=CARTESIAN_POINT('Ctrl Pts',(18.8389198663356,21.75,36.1744910985028));
#57283=CARTESIAN_POINT('Ctrl Pts',(18.7665868250202,21.75,36.2109172193929));
#57284=CARTESIAN_POINT('Ctrl Pts',(18.6961512285367,21.75,36.2510593784398));
#57285=CARTESIAN_POINT('Ctrl Pts',(18.6664445302591,21.75,36.2679896106882));
#57286=CARTESIAN_POINT('Ctrl Pts',(18.6370755244225,21.75,36.2855814538998));
#57287=CARTESIAN_POINT('Ctrl Pts',(18.6080684406704,21.75,36.3038248169416));
#57288=CARTESIAN_POINT('Ctrl Pts',(18.5950040138221,21.75,36.3120413989311));
#57289=CARTESIAN_POINT('Ctrl Pts',(18.5820114468336,21.75,36.320391318453));
#57290=CARTESIAN_POINT('Ctrl Pts',(18.5691115639433,21.75,36.3288611784974));
#57291=CARTESIAN_POINT('Ctrl Pts',(18.4992480227799,21.75,36.37473247988));
#57292=CARTESIAN_POINT('Ctrl Pts',(18.4319799898637,21.75,36.4241928678248));
#57293=CARTESIAN_POINT('Ctrl Pts',(18.3676173103639,21.75,36.4770057143139));
#57294=CARTESIAN_POINT('Ctrl Pts',(18.3032905441657,21.75,36.5297890921157));
#57295=CARTESIAN_POINT('Ctrl Pts',(18.2418649238884,21.75,36.5859215783093));
#57296=CARTESIAN_POINT('Ctrl Pts',(18.1836636252436,21.75,36.6452170871453));
#57297=CARTESIAN_POINT('Ctrl Pts',(18.1266152525058,21.75,36.7033379945567));
#57298=CARTESIAN_POINT('Ctrl Pts',(18.072663886905,21.75,36.7644983503434));
#57299=CARTESIAN_POINT('Ctrl Pts',(18.0221403945991,21.75,36.8285642992791));
#57300=CARTESIAN_POINT('Ctrl Pts',(17.9954862842875,21.75,36.862362851046));
#57301=CARTESIAN_POINT('Ctrl Pts',(17.9697867357093,21.75,36.8969707358832));
#57302=CARTESIAN_POINT('Ctrl Pts',(17.9450946017473,21.75,36.932372385933));
#57303=CARTESIAN_POINT('Ctrl Pts',(19.1114077309894,-0.12774359558736,36.3915666551543));
#57304=CARTESIAN_POINT('Ctrl Pts',(18.5446637169267,-0.0858359972810003,
36.6863421879098));
#57305=CARTESIAN_POINT('Ctrl Pts',(17.7372336080694,-0.00202080066828049,
37.8791160387151));
#57306=CARTESIAN_POINT('Ctrl Pts',(18.5843637960128,0.123701994250799,39.8818024076985));
#57307=CARTESIAN_POINT('Ctrl Pts',(20.7234950721292,0.249424789169879,40.2555031365194));
#57308=CARTESIAN_POINT('Ctrl Pts',(22.202317510923,0.375147584088957,38.6673870046074));
#57309=CARTESIAN_POINT('Ctrl Pts',(21.6746022358962,0.500870379008037,36.5608878176203));
#57310=CARTESIAN_POINT('Ctrl Pts',(19.6205166436687,0.626593173927117,35.8576992053172));
#57311=CARTESIAN_POINT('Ctrl Pts',(17.9123977241599,0.752315968846196,37.1976370239046));
#57312=CARTESIAN_POINT('Ctrl Pts',(18.1067028033701,0.878038763765275,39.3601034488986));
#57313=CARTESIAN_POINT('Ctrl Pts',(20.0264596815545,1.00376155868435,40.3741087222362));
#57314=CARTESIAN_POINT('Ctrl Pts',(21.9220848862426,1.12948435360343,39.3157005884543));
#57315=CARTESIAN_POINT('Ctrl Pts',(22.0660679021208,1.25520714852251,37.1493647266486));
#57316=CARTESIAN_POINT('Ctrl Pts',(20.3271786047828,1.38092994344159,35.8493829925345));
#57317=CARTESIAN_POINT('Ctrl Pts',(18.2901244766361,1.50665273836067,36.6004471178591));
#57318=CARTESIAN_POINT('Ctrl Pts',(17.8113281044618,1.63237553327975,38.7181005585794));
#57319=CARTESIAN_POINT('Ctrl Pts',(19.3271324331515,1.75809832819883,40.2724593299136));
#57320=CARTESIAN_POINT('Ctrl Pts',(21.4561401039683,1.88382112311791,39.8469939456022));
#57321=CARTESIAN_POINT('Ctrl Pts',(22.2581253366117,2.00954391803699,37.8294419590792));
#57322=CARTESIAN_POINT('Ctrl Pts',(21.0022155117262,2.13526671295606,36.0584575842664));
#57323=CARTESIAN_POINT('Ctrl Pts',(18.8329577355021,2.26098950787515,36.1479897686354));
#57324=CARTESIAN_POINT('Ctrl Pts',(17.7272593230923,2.38671230279422,38.0164454289377));
#57325=CARTESIAN_POINT('Ctrl Pts',(18.6927752719204,2.51243509771331,39.9610467549065));
#57326=CARTESIAN_POINT('Ctrl Pts',(20.8496029381568,2.63815789263238,40.2096223341063));
#57327=CARTESIAN_POINT('Ctrl Pts',(22.2321628639168,2.76388068755146,38.5356380220699));
#57328=CARTESIAN_POINT('Ctrl Pts',(21.5804881745105,2.88960348247054,36.4646441783065));
#57329=CARTESIAN_POINT('Ctrl Pts',(19.4884688755281,3.01532627738962,35.8839974173462));
#57330=CARTESIAN_POINT('Ctrl Pts',(17.8626226927863,3.1410490723087,37.3228579390602));
#57331=CARTESIAN_POINT('Ctrl Pts',(18.1846303029432,3.26677186722778,39.4699505096519));
#57332=CARTESIAN_POINT('Ctrl Pts',(20.1610368520708,3.39249466214686,40.3685675367379));
#57333=CARTESIAN_POINT('Ctrl Pts',(21.9906858577964,3.51821745706594,39.1997733183766));
#57334=CARTESIAN_POINT('Ctrl Pts',(22.0061652337193,3.64394025198502,37.0287238492198));
#57335=CARTESIAN_POINT('Ctrl Pts',(20.1933681766596,3.7696630469041,35.8339593374025));
#57336=CARTESIAN_POINT('Ctrl Pts',(18.2043491044069,3.89538584182318,36.7043032573617));
#57337=CARTESIAN_POINT('Ctrl Pts',(17.851758656844,4.02110863674226,38.8465860083142));
#57338=CARTESIAN_POINT('Ctrl Pts',(19.4569227122844,4.14683143166134,40.3084833247801));
#57339=CARTESIAN_POINT('Ctrl Pts',(21.5570088158898,4.27255422658041,39.7577258770679));
#57340=CARTESIAN_POINT('Ctrl Pts',(22.2381477279983,4.3982770214995,37.6962348654038));
#57341=CARTESIAN_POINT('Ctrl Pts',(20.8795978468344,4.52399981641858,36.0027067052734));
#57342=CARTESIAN_POINT('Ctrl Pts',(18.7194449935648,4.64972261133765,36.2205026172528));
#57343=CARTESIAN_POINT('Ctrl Pts',(17.7262989750634,4.77544540625674,38.1511388840565));
#57344=CARTESIAN_POINT('Ctrl Pts',(18.8052424981953,4.90116820117581,40.0351708059346));
#57345=CARTESIAN_POINT('Ctrl Pts',(20.9730031072704,5.0268909960949,40.1556255713292));
#57346=CARTESIAN_POINT('Ctrl Pts',(22.2540378273918,5.15261379101397,38.40272926675));
#57347=CARTESIAN_POINT('Ctrl Pts',(21.4809026468269,5.27833658593306,36.373947020836));
#57348=CARTESIAN_POINT('Ctrl Pts',(19.3581780290348,5.40405938085213,35.9181668043027));
#57349=CARTESIAN_POINT('Ctrl Pts',(17.8203643467799,5.52978217577121,37.4507543180954));
#57350=CARTESIAN_POINT('Ctrl Pts',(18.2689157107976,5.65550497069029,39.5750182100357));
#57351=CARTESIAN_POINT('Ctrl Pts',(20.2950542826331,5.78122776560936,40.3550553222838));
#57352=CARTESIAN_POINT('Ctrl Pts',(22.0523013482622,5.90695056052845,39.0799952613055));
#57353=CARTESIAN_POINT('Ctrl Pts',(21.9392268045967,6.03267335544753,36.9118371590588));
#57354=CARTESIAN_POINT('Ctrl Pts',(20.0588787554923,6.15839615036661,35.8264862374703));
#57355=CARTESIAN_POINT('Ctrl Pts',(18.1248727926419,6.28411894528568,36.8130541998647));
#57356=CARTESIAN_POINT('Ctrl Pts',(17.8997245173177,6.40984174020477,38.9724531122665));
#57357=CARTESIAN_POINT('Ctrl Pts',(19.5886180682867,6.53556453512385,40.3367602559326));
#57358=CARTESIAN_POINT('Ctrl Pts',(21.6524158784223,6.66128733004292,39.6626430497711));
#57359=CARTESIAN_POINT('Ctrl Pts',(22.2103192800337,6.78701012496201,37.5644440117305));
#57360=CARTESIAN_POINT('Ctrl Pts',(20.7538947583175,6.91273291988108,35.9543126440133));
#57361=CARTESIAN_POINT('Ctrl Pts',(18.6104241267262,7.03845571480017,36.2996082568853));
#57362=CARTESIAN_POINT('Ctrl Pts',(17.7333142007588,7.16417850971926,38.2856529659826));
#57363=CARTESIAN_POINT('Ctrl Pts',(18.921900638238,7.28990130463832,40.1025067546524));
#57364=CARTESIAN_POINT('Ctrl Pts',(21.0929902227223,7.41562409955741,40.0944181881676));
#57365=CARTESIAN_POINT('Ctrl Pts',(22.2680061876885,7.5413468944765,38.2687586112371));
#57366=CARTESIAN_POINT('Ctrl Pts',(21.376122481006,7.66706968939556,36.2893044282569));
#57367=CARTESIAN_POINT('Ctrl Pts',(19.2301385343949,7.79279248431465,35.9599895187087));
#57368=CARTESIAN_POINT('Ctrl Pts',(17.7857516200634,7.91851527923373,37.5809280895596));
#57369=CARTESIAN_POINT('Ctrl Pts',(18.3592733315035,8.0442380741528,39.6749119135826));
#57370=CARTESIAN_POINT('Ctrl Pts',(20.4280367361936,8.16996086907188,40.3336329350923));
#57371=CARTESIAN_POINT('Ctrl Pts',(22.1067178764283,8.29568366399096,38.956779624756));
#57372=CARTESIAN_POINT('Ctrl Pts',(21.8654860505154,8.42140645891005,36.7991182484206));
#57373=CARTESIAN_POINT('Ctrl Pts',(19.9241828023082,8.54712925382911,35.8269880579295));
#57374=CARTESIAN_POINT('Ctrl Pts',(18.0519739603972,8.6728520487482,36.9263194279151));
#57375=CARTESIAN_POINT('Ctrl Pts',(17.9550576214233,8.79857484366728,39.0952598678542));
#57376=CARTESIAN_POINT('Ctrl Pts',(19.7217564497116,8.92429763858637,40.3571911888414));
#57377=CARTESIAN_POINT('Ctrl Pts',(21.7420266773424,9.05002043350544,39.5620788595995));
#57378=CARTESIAN_POINT('Ctrl Pts',(22.1747375821867,9.17574322842452,37.4345317551639));
#57379=CARTESIAN_POINT('Ctrl Pts',(20.6255471946341,9.30146602334358,35.9134451199328));
#57380=CARTESIAN_POINT('Ctrl Pts',(18.5062775461834,9.42718881826269,36.3850292226326));
#57381=CARTESIAN_POINT('Ctrl Pts',(17.7482803960562,9.55291161318175,38.4195158235133));
#57382=CARTESIAN_POINT('Ctrl Pts',(19.0423404825012,9.67863440810083,40.1628184081019));
#57383=CARTESIAN_POINT('Ctrl Pts',(21.2091434005197,9.80435720301992,40.0262148824157));
#57384=CARTESIAN_POINT('Ctrl Pts',(22.274018946789,9.93007999793899,38.1341959925202));
#57385=CARTESIAN_POINT('Ctrl Pts',(21.2665152200408,10.0558027928581,36.2110133050587));
#57386=CARTESIAN_POINT('Ctrl Pts',(19.1047995221564,10.1815255877772,36.0093188572313));
#57387=CARTESIAN_POINT('Ctrl Pts',(17.758905925534,10.3072483826963,37.7129226360877));
#57388=CARTESIAN_POINT('Ctrl Pts',(18.455386212983,10.4329711776153,39.7692812181347));
#57389=CARTESIAN_POINT('Ctrl Pts',(20.5595177434226,10.5586939725344,40.3043755195192));
#57390=CARTESIAN_POINT('Ctrl Pts',(22.1537445626494,10.6844167674535,38.8305586185368));
#57391=CARTESIAN_POINT('Ctrl Pts',(21.7852016356913,10.8101395623726,36.6909625071754));
#57392=CARTESIAN_POINT('Ctrl Pts',(19.7897527969826,10.9358623572916,35.8354630385256));
#57393=CARTESIAN_POINT('Ctrl Pts',(17.9859083186327,11.0615851522108,37.0437016352813));
#57394=CARTESIAN_POINT('Ctrl Pts',(18.0175638744037,11.1873079471298,39.2145754995472));
#57395=CARTESIAN_POINT('Ctrl Pts',(19.8558708402556,11.3130307420489,40.3697044568779));
#57396=CARTESIAN_POINT('Ctrl Pts',(21.8255268802713,11.438753536968,39.4563860607021));
#57397=CARTESIAN_POINT('Ctrl Pts',(22.1315274461966,11.564476331887,37.3069537955639));
#57398=CARTESIAN_POINT('Ctrl Pts',(20.4950053670916,11.6901991268062,35.8802474861349));
#57399=CARTESIAN_POINT('Ctrl Pts',(18.4073705722187,11.8159219217252,36.476465879008));
#57400=CARTESIAN_POINT('Ctrl Pts',(17.7711450632678,11.9416447166443,38.5522578990629));
#57401=CARTESIAN_POINT('Ctrl Pts',(19.1661395579888,12.0673675115634,40.2158942080144));
#57402=CARTESIAN_POINT('Ctrl Pts',(21.3210552042258,12.1930903064825,39.951254894294));
#57403=CARTESIAN_POINT('Ctrl Pts',(22.272055013431,12.3188131014015,37.9995134227731));
#57404=CARTESIAN_POINT('Ctrl Pts',(21.1524653389212,12.4445358963206,36.1393482770146));
#57405=CARTESIAN_POINT('Ctrl Pts',(18.9826006503776,12.5702586912397,36.0659817848288));
#57406=CARTESIAN_POINT('Ctrl Pts',(17.7399214312059,12.6959814861588,37.8462749536643));
#57407=CARTESIAN_POINT('Ctrl Pts',(18.5569172151707,12.8217042810779,39.8577950996602));
#57408=CARTESIAN_POINT('Ctrl Pts',(20.6890361016724,12.9474270759969,40.2673857032961));
#57409=CARTESIAN_POINT('Ctrl Pts',(22.1932164490149,13.073149870916,38.7017749945208));
#57410=CARTESIAN_POINT('Ctrl Pts',(21.6986551778685,13.1988726658351,36.5877493187435));
#57411=CARTESIAN_POINT('Ctrl Pts',(19.6560602865144,13.3245954607542,35.8518814511358));
#57412=CARTESIAN_POINT('Ctrl Pts',(17.926907609176,13.4503182556732,37.1647890743968));
#57413=CARTESIAN_POINT('Ctrl Pts',(18.0870240198812,13.5760410505923,39.3299814778073));
#57414=CARTESIAN_POINT('Ctrl Pts',(19.9904908000181,13.7017638455114,40.3742561666127));
#57415=CARTESIAN_POINT('Ctrl Pts',(21.9026235892807,13.8274866404305,39.3459353971103));
#57416=CARTESIAN_POINT('Ctrl Pts',(22.0808404424659,13.9532094353496,37.1821576446587));
#57417=CARTESIAN_POINT('Ctrl Pts',(20.3627271839287,14.0789322302686,35.8548361916556));
#57418=CARTESIAN_POINT('Ctrl Pts',(18.3140501458789,14.2046550251877,36.5735974889797));
#57419=CARTESIAN_POINT('Ctrl Pts',(17.8018279988321,14.3303778201068,38.6834135664704));
#57420=CARTESIAN_POINT('Ctrl Pts',(19.2928636083578,14.4561006150259,40.2615479776945));
#57421=CARTESIAN_POINT('Ctrl Pts',(21.4283330750883,14.581823409945,39.8698011647836));
#57422=CARTESIAN_POINT('Ctrl Pts',(22.262121276604,14.707546204864,37.8651833349275));
#57423=CARTESIAN_POINT('Ctrl Pts',(21.0343728962431,14.8332689997831,36.0745607272056));
#57424=CARTESIAN_POINT('Ctrl Pts',(18.863970562285,14.9589917947022,36.1297795420549));
#57425=CARTESIAN_POINT('Ctrl Pts',(17.7288647299603,15.0847145896213,37.9805172755509));
#57426=CARTESIAN_POINT('Ctrl Pts',(18.663510192582,15.2104373845404,39.9401430734941));
#57427=CARTESIAN_POINT('Ctrl Pts',(20.8161374927797,15.3361601794594,40.2227932374915));
#57428=CARTESIAN_POINT('Ctrl Pts',(22.2249950779723,15.4618829743785,38.5708804936067));
#57429=CARTESIAN_POINT('Ctrl Pts',(21.6061502604796,15.5876057692976,36.4898407292998));
#57430=CARTESIAN_POINT('Ctrl Pts',(19.5235742309539,15.7133285642167,35.8761857040551));
#57431=CARTESIAN_POINT('Ctrl Pts',(17.8751787918303,15.8390513591358,37.2891570006639));
#57432=CARTESIAN_POINT('Ctrl Pts',(18.1631944089545,15.9647741540548,39.4410729871876));
#57433=CARTESIAN_POINT('Ctrl Pts',(20.1251441156871,16.0904969489739,40.3708303517809));
#57434=CARTESIAN_POINT('Ctrl Pts',(21.9730463683049,16.216219743893,39.2311143022607));
#57435=CARTESIAN_POINT('Ctrl Pts',(22.0228543683874,16.3419425388121,37.0605810562838));
#57436=CARTESIAN_POINT('Ctrl Pts',(20.2291766440881,16.4676653337312,35.8373003729914));
#57437=CARTESIAN_POINT('Ctrl Pts',(18.2266436119918,16.5933881286502,36.6760833390361));
#57438=CARTESIAN_POINT('Ctrl Pts',(17.8402215746481,16.7191109235693,38.8125227642993));
#57439=CARTESIAN_POINT('Ctrl Pts',(19.4220681171815,16.8448337184884,40.2996195750816));
#57440=CARTESIAN_POINT('Ctrl Pts',(21.5306007090374,16.9705565134075,39.7821394132931));
#57441=CARTESIAN_POINT('Ctrl Pts',(22.2442525813841,17.0962793083265,37.7316769254967));
#57442=CARTESIAN_POINT('Ctrl Pts',(20.9126521309017,17.2220021032456,36.0168779142305));
#57443=CARTESIAN_POINT('Ctrl Pts',(18.7493253827009,17.3477248981647,36.2004883422566));
#57444=CARTESIAN_POINT('Ctrl Pts',(17.7257746059519,17.4734476930838,38.1151787130956));
#57445=CARTESIAN_POINT('Ctrl Pts',(18.7747912435853,17.5991704880029,40.0160362834403));
#57446=CARTESIAN_POINT('Ctrl Pts',(20.9403760766967,17.7248932829219,40.1707545413767));
#57447=CARTESIAN_POINT('Ctrl Pts',(22.2489689780076,17.850616077841,38.4383342611231));
#57448=CARTESIAN_POINT('Ctrl Pts',(21.5080113677371,17.9763388727601,36.3975801778086));
#57449=CARTESIAN_POINT('Ctrl Pts',(19.3927593584336,18.1020616676792,35.9082905440105));
#57450=CARTESIAN_POINT('Ctrl Pts',(17.8309033183622,18.2277844625983,37.416369162359));
#57451=CARTESIAN_POINT('Ctrl Pts',(18.2458078549532,18.3535072575174,39.5474603463113));
#57452=CARTESIAN_POINT('Ctrl Pts',(20.2593584567611,18.4792300524364,40.3594390293124));
#57453=CARTESIAN_POINT('Ctrl Pts',(22.0365481921237,18.6049528473555,39.1123255399277));
#57454=CARTESIAN_POINT('Ctrl Pts',(21.9577726239778,18.7306756422746,36.9426504909417));
#57455=CARTESIAN_POINT('Ctrl Pts',(20.0948222109758,18.8563984371937,35.8277015412522));
#57456=CARTESIAN_POINT('Ctrl Pts',(18.1454575682997,18.9821212321127,36.7835639346676));
#57457=CARTESIAN_POINT('Ctrl Pts',(17.8861911206918,19.1078440270318,38.9391326089534));
#57458=CARTESIAN_POINT('Ctrl Pts',(19.5532998573488,19.2335668219509,40.329975455778));
#57459=CARTESIAN_POINT('Ctrl Pts',(21.6274993957651,19.35928961687,39.6885771329276));
#57460=CARTESIAN_POINT('Ctrl Pts',(22.2185115696939,19.4850124117891,37.5994625065813));
#57461=CARTESIAN_POINT('Ctrl Pts',(20.787730080782,19.6107352067082,35.9665021656478));
#57462=CARTESIAN_POINT('Ctrl Pts',(18.6390671193433,19.7364580016272,36.2778601747661));
#57463=CARTESIAN_POINT('Ctrl Pts',(17.7306621680414,19.8621807965463,38.2497868722107));
#57464=CARTESIAN_POINT('Ctrl Pts',(18.8903694996679,19.9879035914654,40.0852085833905));
#57465=CARTESIAN_POINT('Ctrl Pts',(21.0613170676605,20.1136263863845,40.1114520212098));
#57466=CARTESIAN_POINT('Ctrl Pts',(22.2650520927181,20.2393491813036,38.3046014931365));
#57467=CARTESIAN_POINT('Ctrl Pts',(21.4045865489703,20.3650719762226,36.3112907934586));
#57468=CARTESIAN_POINT('Ctrl Pts',(19.2640671650938,20.4907947711417,35.948084320147));
#57469=CARTESIAN_POINT('Ctrl Pts',(17.7942507800659,20.6165175660608,37.5459774606941));
#57470=CARTESIAN_POINT('Ctrl Pts',(18.334546885942,20.7422403609799,39.648773999513));
#57471=CARTESIAN_POINT('Ctrl Pts',(20.3927166898407,20.867963155899,40.3401151319165));
#57472=CARTESIAN_POINT('Ctrl Pts',(22.0928023143269,20.993685950818,38.9899994071434));
#57473=CARTESIAN_POINT('Ctrl Pts',(21.8860250841065,21.1194087457371,36.8287532338137));
#57474=CARTESIAN_POINT('Ctrl Pts',(19.9597442617979,21.2451315406562,35.8261244740626));
#57475=CARTESIAN_POINT('Ctrl Pts',(18.071536445263,21.3708543355753,36.895563530529));
#57476=CARTESIAN_POINT('Ctrl Pts',(17.9380830578744,21.4965771304943,39.0629871265469));
#57477=CARTESIAN_POINT('Ctrl Pts',(19.6894213454275,21.622316577962,40.3523470934528));
#57478=CARTESIAN_POINT('Ctrl Pts',(21.0374380936755,21.7061484271234,39.8437203447635));
#57479=CARTESIAN_POINT('Ctrl Pts',(21.4557699665296,21.7480726779785,39.3605849726844));
#57480=CARTESIAN_POINT('Ctrl Pts',(19.0436064803604,-0.0429106862021636,
36.2612099984105));
#57481=CARTESIAN_POINT('Ctrl Pts',(18.4336188389561,-0.00100308789580381,
36.5784774551593));
#57482=CARTESIAN_POINT('Ctrl Pts',(17.5645803039565,0.0828121087169158,
37.8622621797055));
#57483=CARTESIAN_POINT('Ctrl Pts',(18.4763481082636,0.208534903635996,40.017757261042));
#57484=CARTESIAN_POINT('Ctrl Pts',(20.7786990981206,0.334257698555075,40.4199720538028));
#57485=CARTESIAN_POINT('Ctrl Pts',(22.3703584524549,0.459980493474155,38.7106796933293));
#57486=CARTESIAN_POINT('Ctrl Pts',(21.8023775158073,0.585703288393234,36.4434506819814));
#57487=CARTESIAN_POINT('Ctrl Pts',(19.5915613544439,0.711426083312313,35.6866074645181));
#57488=CARTESIAN_POINT('Ctrl Pts',(17.753109769432,0.837148878231393,37.1287850425919));
#57489=CARTESIAN_POINT('Ctrl Pts',(17.9622406892819,0.962871673150472,39.4562516967922));
#57490=CARTESIAN_POINT('Ctrl Pts',(20.0284786047021,1.08859446806955,40.5476274673468));
#57491=CARTESIAN_POINT('Ctrl Pts',(22.0687435548436,1.21431726298863,39.4084608151208));
#57492=CARTESIAN_POINT('Ctrl Pts',(22.2237127438928,1.34004005790771,37.0768294788493));
#57493=CARTESIAN_POINT('Ctrl Pts',(20.3521429437231,1.46576285282679,35.6776567091597));
#57494=CARTESIAN_POINT('Ctrl Pts',(18.1596577789763,1.59148564774587,36.4860284307524));
#57495=CARTESIAN_POINT('Ctrl Pts',(17.6443283488832,1.71720844266495,38.7652627862372));
#57496=CARTESIAN_POINT('Ctrl Pts',(19.2757913804202,1.84293123758403,40.4382220364387));
#57497=CARTESIAN_POINT('Ctrl Pts',(21.5672463149755,1.96865403250311,39.9802928482416));
#57498=CARTESIAN_POINT('Ctrl Pts',(22.4304245195311,2.09437682742219,37.8087978749678));
#57499=CARTESIAN_POINT('Ctrl Pts',(21.0786864281009,2.22009962234127,35.9026840829364));
#57500=CARTESIAN_POINT('Ctrl Pts',(18.7439102298808,2.34582241726035,35.9990477402805));
#57501=CARTESIAN_POINT('Ctrl Pts',(17.5538449623967,2.47154521217943,38.0100700590282));
#57502=CARTESIAN_POINT('Ctrl Pts',(18.5930315823703,2.59726800709851,40.1030481000252));
#57503=CARTESIAN_POINT('Ctrl Pts',(20.9144292299826,2.72299080201759,40.3705904604286));
#57504=CARTESIAN_POINT('Ctrl Pts',(22.4024810616538,2.84871359693667,38.5688780172262));
#57505=CARTESIAN_POINT('Ctrl Pts',(21.7010823756679,2.97443639185575,36.3398634731384));
#57506=CARTESIAN_POINT('Ctrl Pts',(19.4494380948377,3.10015918677483,35.714912279268));
#57507=CARTESIAN_POINT('Ctrl Pts',(17.6995368101505,3.22588198169391,37.2635605475731));
#57508=CARTESIAN_POINT('Ctrl Pts',(18.0461142026948,3.35160477661299,39.574480293551));
#57509=CARTESIAN_POINT('Ctrl Pts',(20.1733242648118,3.47732757153206,40.5416634790403));
#57510=CARTESIAN_POINT('Ctrl Pts',(22.1425789087208,3.60305036645114,39.283688077704));
#57511=CARTESIAN_POINT('Ctrl Pts',(22.1592393899528,3.72877316137022,36.9469834770324));
#57512=CARTESIAN_POINT('Ctrl Pts',(20.2081225298838,3.85449595628931,35.661056200319));
#57513=CARTESIAN_POINT('Ctrl Pts',(18.0673375855584,3.98021875120838,36.5978089877741));
#57514=CARTESIAN_POINT('Ctrl Pts',(17.6878438279644,4.10594154612746,38.9035519158862));
#57515=CARTESIAN_POINT('Ctrl Pts',(19.4154849003888,4.23166434104654,40.4769947294314));
#57516=CARTESIAN_POINT('Ctrl Pts',(21.6758114981089,4.35738713596562,39.8842134592636));
#57517=CARTESIAN_POINT('Ctrl Pts',(22.4089225820486,4.4831099308847,37.6654268311222));
#57518=CARTESIAN_POINT('Ctrl Pts',(20.9467128062435,4.60883272580378,35.842679307695));
#57519=CARTESIAN_POINT('Ctrl Pts',(18.6217362536136,4.73455552072286,36.0770934547515));
#57520=CARTESIAN_POINT('Ctrl Pts',(17.5528113380187,4.86027831564194,38.1550408764728));
#57521=CARTESIAN_POINT('Ctrl Pts',(18.7140802681763,4.98600111056102,40.1828279546616));
#57522=CARTESIAN_POINT('Ctrl Pts',(21.0472450625962,5.1117239054801,40.3124736437482));
#57523=CARTESIAN_POINT('Ctrl Pts',(22.4260251257194,5.23744670039918,38.4258280755102));
#57524=CARTESIAN_POINT('Ctrl Pts',(21.5938982861276,5.36316949531825,36.2422459530679));
#57525=CARTESIAN_POINT('Ctrl Pts',(19.3092058132839,5.48889229023733,35.7516888543014));
#57526=CARTESIAN_POINT('Ctrl Pts',(17.6540540733761,5.61461508515642,37.4012156593273));
#57527=CARTESIAN_POINT('Ctrl Pts',(18.1368307446719,5.74033788007549,39.6875648558131));
#57528=CARTESIAN_POINT('Ctrl Pts',(20.317567475763,5.86606067499458,40.527120257373));
#57529=CARTESIAN_POINT('Ctrl Pts',(22.2088957762494,5.99178346991365,39.1547707310503));
#57530=CARTESIAN_POINT('Ctrl Pts',(22.087193433601,6.11750626483274,36.821178113987));
#57531=CARTESIAN_POINT('Ctrl Pts',(20.0633713145625,6.24322905975181,35.6530128888971));
#57532=CARTESIAN_POINT('Ctrl Pts',(17.9817970826894,6.36895185467089,36.7148578304118));
#57533=CARTESIAN_POINT('Ctrl Pts',(17.7394695732254,6.49467464958997,39.0390229150768));
#57534=CARTESIAN_POINT('Ctrl Pts',(19.5572288581518,6.62039744450905,40.5074292432716));
#57535=CARTESIAN_POINT('Ctrl Pts',(21.7784982977988,6.74612023942813,39.7818756345639));
#57536=CARTESIAN_POINT('Ctrl Pts',(22.3789707715017,6.87184303434721,37.5235800890376));
#57537=CARTESIAN_POINT('Ctrl Pts',(20.8114183371727,6.99756582926629,35.7905926891272));
#57538=CARTESIAN_POINT('Ctrl Pts',(18.504396890909,7.12328862418536,36.1622350025119));
#57539=CARTESIAN_POINT('Ctrl Pts',(17.5603618385438,7.24901141910446,38.2998186342149));
#57540=CARTESIAN_POINT('Ctrl Pts',(18.8396396423022,7.37473421402352,40.2553017620966));
#57541=CARTESIAN_POINT('Ctrl Pts',(21.1763874191757,7.50045700894261,40.2465960228738));
#57542=CARTESIAN_POINT('Ctrl Pts',(22.4410592980093,7.62617980386168,38.2816352086321));
#57543=CARTESIAN_POINT('Ctrl Pts',(21.481123197853,7.75190259878077,36.1511449725044));
#57544=CARTESIAN_POINT('Ctrl Pts',(19.1713966659368,7.87762539369984,35.7967027199703));
#57545=CARTESIAN_POINT('Ctrl Pts',(17.6168003309307,8.00334818861892,37.5413219328085));
#57546=CARTESIAN_POINT('Ctrl Pts',(18.2340828206879,8.129070983538,39.795080635611));
#57547=CARTESIAN_POINT('Ctrl Pts',(20.4606967390331,8.25479377845708,40.504063302007));
#57548=CARTESIAN_POINT('Ctrl Pts',(22.2674643872022,8.38051657337616,39.0221535111804));
#57549=CARTESIAN_POINT('Ctrl Pts',(22.0078261221847,8.50623936829525,36.6998585398304));
#57550=CARTESIAN_POINT('Ctrl Pts',(19.9183978084455,8.63196216321431,35.6535529991953));
#57551=CARTESIAN_POINT('Ctrl Pts',(17.903335933319,8.75768495813341,36.8367654070199));
#57552=CARTESIAN_POINT('Ctrl Pts',(17.7990246965748,8.88340775305248,39.1712000556036));
#57553=CARTESIAN_POINT('Ctrl Pts',(19.7005259468737,9.00913054797156,40.5294190945403));
#57554=CARTESIAN_POINT('Ctrl Pts',(21.8749465681312,9.13485334289064,39.673638208759));
#57555=CARTESIAN_POINT('Ctrl Pts',(22.3406741236175,9.26057613780971,37.383755284529));
#57556=CARTESIAN_POINT('Ctrl Pts',(20.6732776145384,9.3862989327288,35.7466068965907));
#57557=CARTESIAN_POINT('Ctrl Pts',(18.3923037316531,9.51202172764788,36.2541737475709));
#57558=CARTESIAN_POINT('Ctrl Pts',(17.5764699825097,9.63774452256696,38.4438954779233));
#57559=CARTESIAN_POINT('Ctrl Pts',(18.9692692717474,9.76346731748603,40.3202153074079));
#57560=CARTESIAN_POINT('Ctrl Pts',(21.3014033014935,9.88919011240512,40.1731886774423));
#57561=CARTESIAN_POINT('Ctrl Pts',(22.4475308418653,10.0149129073242,38.1368052106512));
#57562=CARTESIAN_POINT('Ctrl Pts',(21.363152698054,10.1406357022433,36.0668800903044));
#57563=CARTESIAN_POINT('Ctrl Pts',(19.036494052845,10.2663584971624,35.8497959792033));
#57564=CARTESIAN_POINT('Ctrl Pts',(17.5879062597423,10.3920812920814,37.6833879098936));
#57565=CARTESIAN_POINT('Ctrl Pts',(18.3375292946295,10.5178040870005,39.8966504944474));
#57566=CARTESIAN_POINT('Ctrl Pts',(20.6022099928108,10.6435268819196,40.4725734909528));
#57567=CARTESIAN_POINT('Ctrl Pts',(22.3180792974602,10.7692496768387,38.8863016063186));
#57568=CARTESIAN_POINT('Ctrl Pts',(21.9214158564827,10.8949724717578,36.5834503134188));
#57569=CARTESIAN_POINT('Ctrl Pts',(19.7737105425055,11.0206952666768,35.6626746366478));
#57570=CARTESIAN_POINT('Ctrl Pts',(17.8322293596317,11.1464180615959,36.9631040961593));
#57571=CARTESIAN_POINT('Ctrl Pts',(17.8663002934623,11.272140856515,39.2996196929586));
#57572=CARTESIAN_POINT('Ctrl Pts',(19.8448735160344,11.3978636514341,40.5428871483115));
#57573=CARTESIAN_POINT('Ctrl Pts',(21.9648179925797,11.5235864463532,39.5598808517986));
#57574=CARTESIAN_POINT('Ctrl Pts',(22.2941669735052,11.6493092412722,37.246442888208));
#57575=CARTESIAN_POINT('Ctrl Pts',(20.532775201612,11.7750320361913,35.7108762212978));
#57576=CARTESIAN_POINT('Ctrl Pts',(18.2858499707485,11.9007548311104,36.3525871916946));
#57577=CARTESIAN_POINT('Ctrl Pts',(17.6010792665565,12.0264776260295,38.5867660218912));
#57578=CARTESIAN_POINT('Ctrl Pts',(19.1025144480368,12.1522004209485,40.377340890036));
#57579=CARTESIAN_POINT('Ctrl Pts',(21.4218541849508,12.2779232158676,40.09250910215));
#57580=CARTESIAN_POINT('Ctrl Pts',(22.4454170567221,12.4036460107867,37.9918461091523));
#57581=CARTESIAN_POINT('Ctrl Pts',(21.2404005978811,12.5293688057058,35.9897468867008));
#57582=CARTESIAN_POINT('Ctrl Pts',(18.9049711787976,12.6550916006249,35.910782394062));
#57583=CARTESIAN_POINT('Ctrl Pts',(17.567473213021,12.780814395544,37.8269152584955));
#57584=CARTESIAN_POINT('Ctrl Pts',(18.4468073020141,12.906537190463,39.9919181505383));
#57585=CARTESIAN_POINT('Ctrl Pts',(20.7416108438247,13.0322599853821,40.4327612826292));
#57586=CARTESIAN_POINT('Ctrl Pts',(22.3605629625162,13.1579827803012,38.7476915511336));
#57587=CARTESIAN_POINT('Ctrl Pts',(21.8282657421995,13.2837055752202,36.472361765836));
#57588=CARTESIAN_POINT('Ctrl Pts',(19.6298170436588,13.4094283701394,35.680345804821));
#57589=CARTESIAN_POINT('Ctrl Pts',(17.7687267857893,13.5351511650584,37.0934307331541));
#57590=CARTESIAN_POINT('Ctrl Pts',(17.9410603778394,13.6608739599775,39.423831363018));
#57591=CARTESIAN_POINT('Ctrl Pts',(19.9897652302897,13.7865967548966,40.5477861620047));
#57592=CARTESIAN_POINT('Ctrl Pts',(22.0477973245563,13.9123195498157,39.4410025961767));
#57593=CARTESIAN_POINT('Ctrl Pts',(22.2396124566716,14.0380423447347,37.1121245577836));
#57594=CARTESIAN_POINT('Ctrl Pts',(20.3904039458871,14.1637651396538,35.683525997564));
#57595=CARTESIAN_POINT('Ctrl Pts',(18.1854090214921,14.2894879345729,36.457130125016));
#57596=CARTESIAN_POINT('Ctrl Pts',(17.6341033674412,14.415210729492,38.7279291118112));
#57597=CARTESIAN_POINT('Ctrl Pts',(19.238907780257,14.5409335244111,40.4264781276555));
#57598=CARTESIAN_POINT('Ctrl Pts',(21.5373175578291,14.6666563193301,40.004840300866));
#57599=CARTESIAN_POINT('Ctrl Pts',(22.434725357212,14.7923791142492,37.8472663845829));
#57600=CARTESIAN_POINT('Ctrl Pts',(21.1132974811485,14.9181019091683,35.9200159257734));
#57601=CARTESIAN_POINT('Ctrl Pts',(18.7772893933007,15.0438247040874,35.9794480393827));
#57602=CARTESIAN_POINT('Ctrl Pts',(17.5555728648087,15.1695474990065,37.9714005203993));
#57603=CARTESIAN_POINT('Ctrl Pts',(18.5615335227911,15.2952702939255,40.0805494286584));
#57604=CARTESIAN_POINT('Ctrl Pts',(20.8784103085867,15.4209930888446,40.3847663283543));
#57605=CARTESIAN_POINT('Ctrl Pts',(22.3947663602474,15.5467158837637,38.6068095551986));
#57606=CARTESIAN_POINT('Ctrl Pts',(21.7287025267509,15.6724386786828,36.3669825680571));
#57607=CARTESIAN_POINT('Ctrl Pts',(19.4872220544836,15.7981614736018,35.7065045176552));
#57608=CARTESIAN_POINT('Ctrl Pts',(17.7130509630151,15.9238842685209,37.2272881646004));
#57609=CARTESIAN_POINT('Ctrl Pts',(18.0230427099378,16.04960706344,39.5433993621595));
#57610=CARTESIAN_POINT('Ctrl Pts',(20.1346928455696,16.1753298583591,40.5440989510993));
#57611=CARTESIAN_POINT('Ctrl Pts',(22.1235934932184,16.3010526532782,39.3174204372251));
#57612=CARTESIAN_POINT('Ctrl Pts',(22.1772019367829,16.4267754481972,36.9812714485266));
#57613=CARTESIAN_POINT('Ctrl Pts',(20.2466632502921,16.5524982431163,35.6646521631667));
#57614=CARTESIAN_POINT('Ctrl Pts',(18.0913332057336,16.6782210380354,36.5674358369459));
#57615=CARTESIAN_POINT('Ctrl Pts',(17.6754264448377,16.8039438329545,38.8668895826994));
#57616=CARTESIAN_POINT('Ctrl Pts',(19.377970834547,16.9296666278735,40.4674546590671));
#57617=CARTESIAN_POINT('Ctrl Pts',(21.647388403355,17.0553894227927,39.9104897939243));
#57618=CARTESIAN_POINT('Ctrl Pts',(22.4154932471558,17.1811122177117,37.7035731866305));
#57619=CARTESIAN_POINT('Ctrl Pts',(20.9822891939532,17.3068350126308,35.8579318063771));
#57620=CARTESIAN_POINT('Ctrl Pts',(18.653896572278,17.4325578075499,36.0555520531726));
#57621=CARTESIAN_POINT('Ctrl Pts',(17.552246958564,17.558280602469,38.1163368772691));
#57622=CARTESIAN_POINT('Ctrl Pts',(18.6813055259356,17.684003397388,40.1622334323443));
#57623=CARTESIAN_POINT('Ctrl Pts',(21.0121285286199,17.8097261923071,40.3287569824818));
#57624=CARTESIAN_POINT('Ctrl Pts',(22.4205695136552,17.9354489872262,38.4641497974886));
#57625=CARTESIAN_POINT('Ctrl Pts',(21.623075453101,18.0611717821453,36.2676823640807));
#57626=CARTESIAN_POINT('Ctrl Pts',(19.3464257627376,18.1868945770644,35.7410590168932));
#57627=CARTESIAN_POINT('Ctrl Pts',(17.6653971881842,18.3126173719835,37.364206851953));
#57628=CARTESIAN_POINT('Ctrl Pts',(18.1119597162451,18.4383401669025,39.6579042755893));
#57629=CARTESIAN_POINT('Ctrl Pts',(20.2791479916725,18.5640629618216,40.5318384494398));
#57630=CARTESIAN_POINT('Ctrl Pts',(22.1919406248596,18.6897857567407,39.1895678703468));
#57631=CARTESIAN_POINT('Ctrl Pts',(22.1071543336573,18.8155085516598,36.8543425606733));
#57632=CARTESIAN_POINT('Ctrl Pts',(20.1020573228665,18.9412313465789,35.6543209226286));
#57633=CARTESIAN_POINT('Ctrl Pts',(18.0039525151963,19.0669541414979,36.6831174028719));
#57634=CARTESIAN_POINT('Ctrl Pts',(17.7249035531474,19.192676936417,39.0031599950952));
#57635=CARTESIAN_POINT('Ctrl Pts',(19.5192158017205,19.3183997313361,40.5001267501863));
#57636=CARTESIAN_POINT('Ctrl Pts',(21.7516806409536,19.4441225262551,39.809788536728));
#57637=CARTESIAN_POINT('Ctrl Pts',(22.3877881481717,19.5698453211742,37.561270560484));
#57638=CARTESIAN_POINT('Ctrl Pts',(20.8478353579689,19.6955681160933,35.8037122940409));
#57639=CARTESIAN_POINT('Ctrl Pts',(18.5352253973877,19.8212909110124,36.1388275010866));
#57640=CARTESIAN_POINT('Ctrl Pts',(17.5575074507744,19.9470137059315,38.2612158904656));
#57641=CARTESIAN_POINT('Ctrl Pts',(18.8057026189372,20.0727365008505,40.2366837080424));
#57642=CARTESIAN_POINT('Ctrl Pts',(21.1422975431955,20.1984592957697,40.2649295692081));
#57643=CARTESIAN_POINT('Ctrl Pts',(22.4378798000725,20.3241820906887,38.3202129693996));
#57644=CARTESIAN_POINT('Ctrl Pts',(21.5117591273934,20.4499048856078,36.1748089384568));
#57645=CARTESIAN_POINT('Ctrl Pts',(19.2079141145602,20.5756276805269,35.7838891325111));
#57646=CARTESIAN_POINT('Ctrl Pts',(17.6259479927237,20.701350475446,37.5037045056489));
#57647=CARTESIAN_POINT('Ctrl Pts',(18.207469701124,20.827073270365,39.766948349854));
#57648=CARTESIAN_POINT('Ctrl Pts',(20.4226817071412,20.9527960652841,40.5110401025622));
#57649=CARTESIAN_POINT('Ctrl Pts',(22.2524870417086,21.0785188602032,39.0579080250413));
#57650=CARTESIAN_POINT('Ctrl Pts',(22.0299323224199,21.2042416551223,36.7317547299878));
#57651=CARTESIAN_POINT('Ctrl Pts',(19.9566726737475,21.3299644500414,35.6526235222652));
#57652=CARTESIAN_POINT('Ctrl Pts',(17.9243910723363,21.4556872449604,36.8036627771902));
#57653=CARTESIAN_POINT('Ctrl Pts',(17.780754942107,21.5814100398795,39.1364648438266));
#57654=CARTESIAN_POINT('Ctrl Pts',(19.6657236137085,21.7071494873473,40.5242053856216));
#57655=CARTESIAN_POINT('Ctrl Pts',(21.1165965588731,21.7909813365086,39.9767694655415));
#57656=CARTESIAN_POINT('Ctrl Pts',(21.5668479353584,21.8329055873637,39.4567699617426));
#57657=CARTESIAN_POINT('Ctrl Pts',(18.9758052297315,0.0419222231830331,
36.1308533416667));
#57658=CARTESIAN_POINT('Ctrl Pts',(18.3225739609854,0.083829821489393,36.4706127224088));
#57659=CARTESIAN_POINT('Ctrl Pts',(17.3919269998435,0.167645018102112,37.8454083206958));
#57660=CARTESIAN_POINT('Ctrl Pts',(18.3683324205143,0.293367813021192,40.1537121143855));
#57661=CARTESIAN_POINT('Ctrl Pts',(20.833903124112,0.419090607940272,40.5844409710861));
#57662=CARTESIAN_POINT('Ctrl Pts',(22.5383993939867,0.544813402859351,38.7539723820513));
#57663=CARTESIAN_POINT('Ctrl Pts',(21.9301527957185,0.67053619777843,36.3260135463425));
#57664=CARTESIAN_POINT('Ctrl Pts',(19.5626060652191,0.79625899269751,35.515515723719));
#57665=CARTESIAN_POINT('Ctrl Pts',(17.5938218147042,0.921981787616588,37.0599330612793));
#57666=CARTESIAN_POINT('Ctrl Pts',(17.8177785751937,1.04770458253567,39.5523999446856));
#57667=CARTESIAN_POINT('Ctrl Pts',(20.0304975278497,1.17342737745475,40.7211462124573));
#57668=CARTESIAN_POINT('Ctrl Pts',(22.2154022234444,1.29915017237383,39.5012210417873));
#57669=CARTESIAN_POINT('Ctrl Pts',(22.3813575856649,1.42487296729291,37.0042942310502));
#57670=CARTESIAN_POINT('Ctrl Pts',(20.3771072826633,1.55059576221199,35.5059304257848));
#57671=CARTESIAN_POINT('Ctrl Pts',(18.0291910813165,1.67631855713107,36.3716097436458));
#57672=CARTESIAN_POINT('Ctrl Pts',(17.4773285933046,1.80204135205015,38.8124250138951));
#57673=CARTESIAN_POINT('Ctrl Pts',(19.2244503276889,1.92776414696923,40.603984742964));
#57674=CARTESIAN_POINT('Ctrl Pts',(21.6783525259826,2.05348694188831,40.1135917508809));
#57675=CARTESIAN_POINT('Ctrl Pts',(22.6027237024506,2.17920973680738,37.7881537908565));
#57676=CARTESIAN_POINT('Ctrl Pts',(21.1551573444755,2.30493253172647,35.7469105816062));
#57677=CARTESIAN_POINT('Ctrl Pts',(18.6548627242596,2.43065532664554,35.8501057119256));
#57678=CARTESIAN_POINT('Ctrl Pts',(17.3804306017012,2.55637812156462,38.0036946891185));
#57679=CARTESIAN_POINT('Ctrl Pts',(18.4932878928202,2.6821009164837,40.2450494451438));
#57680=CARTESIAN_POINT('Ctrl Pts',(20.9792555218084,2.80782371140278,40.5315585867508));
#57681=CARTESIAN_POINT('Ctrl Pts',(22.5727992593908,2.93354650632186,38.6021180123824));
#57682=CARTESIAN_POINT('Ctrl Pts',(21.8216765768254,3.05926930124094,36.2150827679703));
#57683=CARTESIAN_POINT('Ctrl Pts',(19.4104073141475,3.18499209616002,35.54582714119));
#57684=CARTESIAN_POINT('Ctrl Pts',(17.5364509275148,3.3107148910791,37.2042631560859));
#57685=CARTESIAN_POINT('Ctrl Pts',(17.9075981024465,3.43643768599817,39.6790100774501));
#57686=CARTESIAN_POINT('Ctrl Pts',(20.1856116775528,3.56216048091726,40.7147594213426));
#57687=CARTESIAN_POINT('Ctrl Pts',(22.2944719596453,3.68788327583633,39.3676028370313));
#57688=CARTESIAN_POINT('Ctrl Pts',(22.3123135461862,3.81360607075542,36.865243104845));
#57689=CARTESIAN_POINT('Ctrl Pts',(20.2228768831082,3.9393288656745,35.4881530632354));
#57690=CARTESIAN_POINT('Ctrl Pts',(17.93032606671,4.06505166059357,36.4913147181865));
#57691=CARTESIAN_POINT('Ctrl Pts',(17.5239289990847,4.19077445551266,38.9605178234583));
#57692=CARTESIAN_POINT('Ctrl Pts',(19.374047088493,4.31649725043174,40.6455061340825));
#57693=CARTESIAN_POINT('Ctrl Pts',(21.7946141803279,4.44222004535081,40.0107010414595));
#57694=CARTESIAN_POINT('Ctrl Pts',(22.5796974360989,4.56794284026989,37.6346187968407));
#57695=CARTESIAN_POINT('Ctrl Pts',(21.0138277656526,4.69366563518897,35.6826519101167));
#57696=CARTESIAN_POINT('Ctrl Pts',(18.5240275136623,4.81938843010805,35.93368429225));
#57697=CARTESIAN_POINT('Ctrl Pts',(17.3793237009739,4.94511122502714,38.158942868889));
#57698=CARTESIAN_POINT('Ctrl Pts',(18.6229180381575,5.0708340199462,40.3304851033885));
#57699=CARTESIAN_POINT('Ctrl Pts',(21.121487017922,5.1965568148653,40.4693217161674));
#57700=CARTESIAN_POINT('Ctrl Pts',(22.5980124240472,5.32227960978436,38.4489268842704));
#57701=CARTESIAN_POINT('Ctrl Pts',(21.7068939254283,5.44800240470346,36.1105448853));
#57702=CARTESIAN_POINT('Ctrl Pts',(19.260233597533,5.57372519962252,35.5852109043001));
#57703=CARTESIAN_POINT('Ctrl Pts',(17.4877437999723,5.69944799454161,37.3516770005591));
#57704=CARTESIAN_POINT('Ctrl Pts',(18.004745778546,5.82517078946069,39.8001115015904));
#57705=CARTESIAN_POINT('Ctrl Pts',(20.3400806688929,5.95089358437976,40.6991851924624));
#57706=CARTESIAN_POINT('Ctrl Pts',(22.3654902042366,6.07661637929885,39.2295462007951));
#57707=CARTESIAN_POINT('Ctrl Pts',(22.2351600626052,6.20233917421792,36.7305190689153));
#57708=CARTESIAN_POINT('Ctrl Pts',(20.0678638736327,6.32806196913701,35.479539540324));
#57709=CARTESIAN_POINT('Ctrl Pts',(17.8387213727366,6.45378476405608,36.6166614609588));
#57710=CARTESIAN_POINT('Ctrl Pts',(17.5792146291333,6.57950755897517,39.1055927178871));
#57711=CARTESIAN_POINT('Ctrl Pts',(19.5258396480168,6.70523035389424,40.6780982306105));
#57712=CARTESIAN_POINT('Ctrl Pts',(21.9045807171753,6.83095314881333,39.9011082193567));
#57713=CARTESIAN_POINT('Ctrl Pts',(22.5476222629695,6.95667594373239,37.4827161663445));
#57714=CARTESIAN_POINT('Ctrl Pts',(20.8689419160278,7.08239873865149,35.6268727342411));
#57715=CARTESIAN_POINT('Ctrl Pts',(18.3983696550917,7.20812153357055,36.0248617481384));
#57716=CARTESIAN_POINT('Ctrl Pts',(17.3874094763289,7.33384432848965,38.3139843024473));
#57717=CARTESIAN_POINT('Ctrl Pts',(18.7573786463665,7.45956712340871,40.4080967695405));
#57718=CARTESIAN_POINT('Ctrl Pts',(21.2597846156292,7.58528991832781,40.3987738575802));
#57719=CARTESIAN_POINT('Ctrl Pts',(22.6141124083302,7.71101271324687,38.2945118060269));
#57720=CARTESIAN_POINT('Ctrl Pts',(21.5861239146998,7.83673550816597,36.0129855167519));
#57721=CARTESIAN_POINT('Ctrl Pts',(19.1126547974788,7.96245830308503,35.6334159212318));
#57722=CARTESIAN_POINT('Ctrl Pts',(17.447849041798,8.08818109800412,37.5017157760575));
#57723=CARTESIAN_POINT('Ctrl Pts',(18.1088923098723,8.21390389292319,39.9152493576393));
#57724=CARTESIAN_POINT('Ctrl Pts',(20.4933567418726,8.33962668784228,40.6744936689219));
#57725=CARTESIAN_POINT('Ctrl Pts',(22.4282108979761,8.46534948276135,39.0875273976046));
#57726=CARTESIAN_POINT('Ctrl Pts',(22.1501661938539,8.59107227768044,36.6005988312404));
#57727=CARTESIAN_POINT('Ctrl Pts',(19.9126128145828,8.71679507259951,35.4801179404609));
#57728=CARTESIAN_POINT('Ctrl Pts',(17.7546979062407,8.8425178675186,36.7472113861249));
#57729=CARTESIAN_POINT('Ctrl Pts',(17.6429917717263,8.96824066243768,39.2471402433529));
#57730=CARTESIAN_POINT('Ctrl Pts',(19.6792954440358,9.09396345735676,40.7016470002393));
#57731=CARTESIAN_POINT('Ctrl Pts',(22.00786645892,9.21968625227583,39.7851975579183));
#57732=CARTESIAN_POINT('Ctrl Pts',(22.5066106650485,9.34540904719491,37.3329788138943));
#57733=CARTESIAN_POINT('Ctrl Pts',(20.7210080344426,9.47113184211399,35.5797686732486));
#57734=CARTESIAN_POINT('Ctrl Pts',(18.2783299171228,9.59685463703307,36.1233182725093));
#57735=CARTESIAN_POINT('Ctrl Pts',(17.4046595689631,9.72257743195216,38.4682751323334));
#57736=CARTESIAN_POINT('Ctrl Pts',(18.8961980609935,9.84830022687122,40.477612206714));
#57737=CARTESIAN_POINT('Ctrl Pts',(21.3936632024671,9.97402302179031,40.3201624724688));
#57738=CARTESIAN_POINT('Ctrl Pts',(22.6210427369415,10.0997458167094,38.1394144287822));
#57739=CARTESIAN_POINT('Ctrl Pts',(21.4597901760673,10.2254686116285,35.92274687555));
#57740=CARTESIAN_POINT('Ctrl Pts',(18.9681885835334,10.3511914065475,35.6902731011753));
#57741=CARTESIAN_POINT('Ctrl Pts',(17.4169065939508,10.4769142014666,37.6538531836996));
#57742=CARTESIAN_POINT('Ctrl Pts',(18.219672376276,10.6026369963857,40.0240197707599));
#57743=CARTESIAN_POINT('Ctrl Pts',(20.6449022421991,10.7283597913048,40.6407714623863));
#57744=CARTESIAN_POINT('Ctrl Pts',(22.4824140322711,10.8540825862239,38.9420445941005));
#57745=CARTESIAN_POINT('Ctrl Pts',(22.0576300772742,10.9798053811429,36.4759381196621));
#57746=CARTESIAN_POINT('Ctrl Pts',(19.7576682880285,11.105528176062,35.48988623477));
#57747=CARTESIAN_POINT('Ctrl Pts',(17.6785504006306,11.2312509709811,36.8825065570371));
#57748=CARTESIAN_POINT('Ctrl Pts',(17.715036712521,11.3569737659002,39.38466388637));
#57749=CARTESIAN_POINT('Ctrl Pts',(19.8338761918132,11.4826965608193,40.716069839745));
#57750=CARTESIAN_POINT('Ctrl Pts',(22.104109104888,11.6084193557383,39.6633756428951));
#57751=CARTESIAN_POINT('Ctrl Pts',(22.4568065008138,11.7341421506574,37.1859319808521));
#57752=CARTESIAN_POINT('Ctrl Pts',(20.5705450361326,11.8598649455765,35.5415049564609));
#57753=CARTESIAN_POINT('Ctrl Pts',(18.1643293692783,11.9855877404956,36.2287085043811));
#57754=CARTESIAN_POINT('Ctrl Pts',(17.4310134698452,12.1113105354147,38.6212741447195));
#57755=CARTESIAN_POINT('Ctrl Pts',(19.0388893380848,12.2370333303337,40.5387875720576));
#57756=CARTESIAN_POINT('Ctrl Pts',(21.5226531656758,12.3627561252528,40.233763310006));
#57757=CARTESIAN_POINT('Ctrl Pts',(22.6187791000131,12.4884789201719,37.9841787955316));
#57758=CARTESIAN_POINT('Ctrl Pts',(21.3283358568412,12.614201715091,35.840145496387));
#57759=CARTESIAN_POINT('Ctrl Pts',(18.8273417072175,12.7399245100101,35.7555830032952));
#57760=CARTESIAN_POINT('Ctrl Pts',(17.3950249948361,12.8656473049291,37.8075555633267));
#57761=CARTESIAN_POINT('Ctrl Pts',(18.3366973888574,12.9913700998482,40.1260412014163));
#57762=CARTESIAN_POINT('Ctrl Pts',(20.7941855859771,13.1170928947673,40.5981368619626));
#57763=CARTESIAN_POINT('Ctrl Pts',(22.5279094760174,13.2428156896864,38.7936081077463));
#57764=CARTESIAN_POINT('Ctrl Pts',(21.9578763065307,13.3685384846054,36.3569742129286));
#57765=CARTESIAN_POINT('Ctrl Pts',(19.6035738008031,13.4942612795245,35.5088101585062));
#57766=CARTESIAN_POINT('Ctrl Pts',(17.6105459624027,13.6199840744436,37.0220723919115));
#57767=CARTESIAN_POINT('Ctrl Pts',(17.7950967357975,13.7457068693627,39.5176812482286));
#57768=CARTESIAN_POINT('Ctrl Pts',(19.9890396605614,13.8714296642818,40.7213161573968));
#57769=CARTESIAN_POINT('Ctrl Pts',(22.1929710598319,13.9971524592008,39.5360697952432));
#57770=CARTESIAN_POINT('Ctrl Pts',(22.3983844708772,14.1228752541199,37.0420914709082));
#57771=CARTESIAN_POINT('Ctrl Pts',(20.4180807078455,14.248598049039,35.5122158034726));
#57772=CARTESIAN_POINT('Ctrl Pts',(18.0567678971051,14.3743208439581,36.3406627610522));
#57773=CARTESIAN_POINT('Ctrl Pts',(17.4663787360504,14.5000436388772,38.7724446571519));
#57774=CARTESIAN_POINT('Ctrl Pts',(19.1849519521561,14.6257664337962,40.5914082776165));
#57775=CARTESIAN_POINT('Ctrl Pts',(21.6463020405699,14.7514892287153,40.1398794369485));
#57776=CARTESIAN_POINT('Ctrl Pts',(22.60732943782,14.8772120236344,37.8293494342383));
#57777=CARTESIAN_POINT('Ctrl Pts',(21.192222066054,15.0029348185535,35.7654711243414));
#57778=CARTESIAN_POINT('Ctrl Pts',(18.6906082243163,15.1286576134725,35.8291165367105));
#57779=CARTESIAN_POINT('Ctrl Pts',(17.3822809996572,15.2543804083917,37.9622837652478));
#57780=CARTESIAN_POINT('Ctrl Pts',(18.4595568530001,15.3801032033107,40.2209557838228));
#57781=CARTESIAN_POINT('Ctrl Pts',(20.9406831243936,15.5058259982298,40.5467394192171));
#57782=CARTESIAN_POINT('Ctrl Pts',(22.5645376425225,15.6315487931489,38.6427386167903));
#57783=CARTESIAN_POINT('Ctrl Pts',(21.8512547930222,15.7572715880679,36.2441244068143));
#57784=CARTESIAN_POINT('Ctrl Pts',(19.4508698780133,15.8829943829871,35.5368233312554));
#57785=CARTESIAN_POINT('Ctrl Pts',(17.5509231341999,16.0087171779061,37.165419328537));
#57786=CARTESIAN_POINT('Ctrl Pts',(17.8828910109209,16.1344399728252,39.6457257371314));
#57787=CARTESIAN_POINT('Ctrl Pts',(20.144241575452,16.2601627677443,40.717367550418));
#57788=CARTESIAN_POINT('Ctrl Pts',(22.2741406181319,16.3858855626634,39.4037265721894));
#57789=CARTESIAN_POINT('Ctrl Pts',(22.3315495051783,16.5116083575824,36.9019618407693));
#57790=CARTESIAN_POINT('Ctrl Pts',(20.2641498564961,16.6373311525015,35.4920039533422));
#57791=CARTESIAN_POINT('Ctrl Pts',(17.9560227994754,16.7630539474206,36.4587883348557));
#57792=CARTESIAN_POINT('Ctrl Pts',(17.5106313150273,16.8887767423397,38.9212564010996));
#57793=CARTESIAN_POINT('Ctrl Pts',(19.3338735519126,17.0144995372588,40.6352897430527));
#57794=CARTESIAN_POINT('Ctrl Pts',(21.7641760976727,17.1402223321778,40.0388401745554));
#57795=CARTESIAN_POINT('Ctrl Pts',(22.5867339129275,17.2659451270969,37.6754694477643));
#57796=CARTESIAN_POINT('Ctrl Pts',(21.0519262570048,17.391667922016,35.6989856985238));
#57797=CARTESIAN_POINT('Ctrl Pts',(18.5584677618551,17.5173907169351,35.9106157640885));
#57798=CARTESIAN_POINT('Ctrl Pts',(17.3787193111763,17.6431135118542,38.1174950414426));
#57799=CARTESIAN_POINT('Ctrl Pts',(18.587819808286,17.7688363067732,40.3084305812485));
#57800=CARTESIAN_POINT('Ctrl Pts',(21.0838809805431,17.8945591016923,40.4867594235869));
#57801=CARTESIAN_POINT('Ctrl Pts',(22.5921700493026,18.0202818966114,38.489965333854));
#57802=CARTESIAN_POINT('Ctrl Pts',(21.7381395384649,18.1460046915305,36.1377845503528));
#57803=CARTESIAN_POINT('Ctrl Pts',(19.3000921670417,18.2717274864495,35.5738274897759));
#57804=CARTESIAN_POINT('Ctrl Pts',(17.4998910580062,18.3974502813686,37.312044541547));
#57805=CARTESIAN_POINT('Ctrl Pts',(17.978111577537,18.5231730762877,39.7683482048675));
#57806=CARTESIAN_POINT('Ctrl Pts',(20.2989375265839,18.6488958712068,40.7042378695672));
#57807=CARTESIAN_POINT('Ctrl Pts',(22.3473330575957,18.7746186661259,39.2668102007657));
#57808=CARTESIAN_POINT('Ctrl Pts',(22.2565360433367,18.9003414610449,36.7660346304049));
#57809=CARTESIAN_POINT('Ctrl Pts',(20.1092924347572,19.026064255964,35.480940304005));
#57810=CARTESIAN_POINT('Ctrl Pts',(17.8624474620928,19.1517870508831,36.5826708710764));
#57811=CARTESIAN_POINT('Ctrl Pts',(17.5636159856029,19.2775098458022,39.0671873812369));
#57812=CARTESIAN_POINT('Ctrl Pts',(19.4851317460922,19.4032326407212,40.6702780445947));
#57813=CARTESIAN_POINT('Ctrl Pts',(21.8758618861422,19.5289554356404,39.9309999405283));
#57814=CARTESIAN_POINT('Ctrl Pts',(22.5570647266494,19.6546782305594,37.5230786143868));
#57815=CARTESIAN_POINT('Ctrl Pts',(20.9079406351558,19.7804010254785,35.640922422434));
#57816=CARTESIAN_POINT('Ctrl Pts',(18.431383675432,19.9061238203976,35.999794827407));
#57817=CARTESIAN_POINT('Ctrl Pts',(17.3843527335073,20.0318466153166,38.2726449087205));
#57818=CARTESIAN_POINT('Ctrl Pts',(18.7210357382066,20.1575694102357,40.3881588326942));
#57819=CARTESIAN_POINT('Ctrl Pts',(21.2232780187304,20.2832922051548,40.4184071172065));
#57820=CARTESIAN_POINT('Ctrl Pts',(22.6107075074267,20.4090150000739,38.3358244456626));
#57821=CARTESIAN_POINT('Ctrl Pts',(21.6189317058165,20.534737794993,36.0383270834549));
#57822=CARTESIAN_POINT('Ctrl Pts',(19.1517610640266,20.660460589912,35.6196939448752));
#57823=CARTESIAN_POINT('Ctrl Pts',(17.4576452053814,20.7861833848311,37.4614315506035));
#57824=CARTESIAN_POINT('Ctrl Pts',(18.080392516306,20.9119061797502,39.8851227001952));
#57825=CARTESIAN_POINT('Ctrl Pts',(20.4526467244417,21.0376289746693,40.6819650732079));
#57826=CARTESIAN_POINT('Ctrl Pts',(22.4121717690902,21.1633517695884,39.1258166429392));
#57827=CARTESIAN_POINT('Ctrl Pts',(22.1738395607332,21.2890745645074,36.6347562261618));
#57828=CARTESIAN_POINT('Ctrl Pts',(19.9536010856973,21.4147973594266,35.4791225704681));
#57829=CARTESIAN_POINT('Ctrl Pts',(17.7772456994095,21.5405201543456,36.7117620238512));
#57830=CARTESIAN_POINT('Ctrl Pts',(17.6234268263395,21.6662429492647,39.2099425611065));
#57831=CARTESIAN_POINT('Ctrl Pts',(19.6420258819895,21.7919823967325,40.6960636777901));
#57832=CARTESIAN_POINT('Ctrl Pts',(21.1957550240706,21.8758142458938,40.1098185863196));
#57833=CARTESIAN_POINT('Ctrl Pts',(21.6779259041872,21.9177384967489,39.5529549508008));
#57834=CARTESIAN_POINT('Ctrl Pts',(18.9080039791026,0.12675513256823,36.0004966849229));
#57835=CARTESIAN_POINT('Ctrl Pts',(18.2115290830147,0.16866273087459,36.3627479896582));
#57836=CARTESIAN_POINT('Ctrl Pts',(17.2192736957306,0.252477927487309,37.8285544616862));
#57837=CARTESIAN_POINT('Ctrl Pts',(18.260316732765,0.378200722406389,40.2896669677291));
#57838=CARTESIAN_POINT('Ctrl Pts',(20.8891071501034,0.503923517325469,40.7489098883695));
#57839=CARTESIAN_POINT('Ctrl Pts',(22.7064403355186,0.629646312244547,38.7972650707732));
#57840=CARTESIAN_POINT('Ctrl Pts',(22.0579280756295,0.755369107163628,36.2085764107035));
#57841=CARTESIAN_POINT('Ctrl Pts',(19.5336507759943,0.881091902082706,35.3444239829199));
#57842=CARTESIAN_POINT('Ctrl Pts',(17.4345338599763,1.00681469700178,36.9910810799666));
#57843=CARTESIAN_POINT('Ctrl Pts',(17.6733164611056,1.13253749192086,39.6485481925792));
#57844=CARTESIAN_POINT('Ctrl Pts',(20.0325164509972,1.25826028683994,40.8946649575679));
#57845=CARTESIAN_POINT('Ctrl Pts',(22.3620608920454,1.38398308175902,39.5939812684537));
#57846=CARTESIAN_POINT('Ctrl Pts',(22.5390024274368,1.5097058766781,36.9317589832509));
#57847=CARTESIAN_POINT('Ctrl Pts',(20.4020716216036,1.63542867159718,35.33420414241));
#57848=CARTESIAN_POINT('Ctrl Pts',(17.8987243836568,1.76115146651626,36.2571910565391));
#57849=CARTESIAN_POINT('Ctrl Pts',(17.3103288377261,1.88687426143534,38.8595872415529));
#57850=CARTESIAN_POINT('Ctrl Pts',(19.1731092749576,2.01259705635442,40.7697474494891));
#57851=CARTESIAN_POINT('Ctrl Pts',(21.7894587369895,2.1383198512735,40.2468906535202));
#57852=CARTESIAN_POINT('Ctrl Pts',(22.77502288537,2.26404264619258,37.7675097067451));
#57853=CARTESIAN_POINT('Ctrl Pts',(21.2316282608502,2.38976544111166,35.5911370802761));
#57854=CARTESIAN_POINT('Ctrl Pts',(18.5658152186384,2.51548823603074,35.7011636835708));
#57855=CARTESIAN_POINT('Ctrl Pts',(17.2070162410056,2.64121103094982,37.9973193192089));
#57856=CARTESIAN_POINT('Ctrl Pts',(18.3935442032701,2.76693382586889,40.3870507902624));
#57857=CARTESIAN_POINT('Ctrl Pts',(21.0440818136342,2.89265662078798,40.692526713073));
#57858=CARTESIAN_POINT('Ctrl Pts',(22.7431174571279,3.01837941570705,38.6353580075387));
#57859=CARTESIAN_POINT('Ctrl Pts',(21.9422707779827,3.14410221062614,36.0903020628022));
#57860=CARTESIAN_POINT('Ctrl Pts',(19.3713765334573,3.26982500554521,35.3767420031119));
#57861=CARTESIAN_POINT('Ctrl Pts',(17.373365044879,3.3955478004643,37.1449657645987));
#57862=CARTESIAN_POINT('Ctrl Pts',(17.7690820021981,3.52127059538337,39.7835398613493));
#57863=CARTESIAN_POINT('Ctrl Pts',(20.1978990902937,3.64699339030245,40.8878553636448));
#57864=CARTESIAN_POINT('Ctrl Pts',(22.4463650105696,3.77271618522153,39.4515175963588));
#57865=CARTESIAN_POINT('Ctrl Pts',(22.4653877024197,3.89843898014061,36.7835027326575));
#57866=CARTESIAN_POINT('Ctrl Pts',(20.2376312363324,4.02416177505969,35.3152499261521));
#57867=CARTESIAN_POINT('Ctrl Pts',(17.7933145478616,4.14988456997877,36.3848204485987));
#57868=CARTESIAN_POINT('Ctrl Pts',(17.3600141702051,4.27560736489784,39.0174837310305));
#57869=CARTESIAN_POINT('Ctrl Pts',(19.3326092765973,4.40133015981694,40.8140175387337));
#57870=CARTESIAN_POINT('Ctrl Pts',(21.913416862547,4.527052954736,40.1371886236553));
#57871=CARTESIAN_POINT('Ctrl Pts',(22.7504722901491,4.65277574965509,37.6038107625591));
#57872=CARTESIAN_POINT('Ctrl Pts',(21.0809427250616,4.77849854457416,35.5226245125383));
#57873=CARTESIAN_POINT('Ctrl Pts',(18.4263187737112,4.90422133949325,35.7902751297487));
#57874=CARTESIAN_POINT('Ctrl Pts',(17.2058360639291,5.02994413441233,38.1628448613054));
#57875=CARTESIAN_POINT('Ctrl Pts',(18.5317558081385,5.1556669293314,40.4781422521153));
#57876=CARTESIAN_POINT('Ctrl Pts',(21.1957289732478,5.28138972425049,40.6261697885866));
#57877=CARTESIAN_POINT('Ctrl Pts',(22.7699997223748,5.40711251916956,38.4720256930304));
#57878=CARTESIAN_POINT('Ctrl Pts',(21.8198895647289,5.53283531408866,35.978843817532));
#57879=CARTESIAN_POINT('Ctrl Pts',(19.2112613817822,5.65855810900771,35.4187329542988));
#57880=CARTESIAN_POINT('Ctrl Pts',(17.3214335265685,5.78428090392682,37.302138341791));
#57881=CARTESIAN_POINT('Ctrl Pts',(17.8726608124202,5.91000369884587,39.9126581473677));
#57882=CARTESIAN_POINT('Ctrl Pts',(20.3625938620227,6.03572649376497,40.8712501275516));
#57883=CARTESIAN_POINT('Ctrl Pts',(22.5220846322238,6.16144928868404,39.30432167054));
#57884=CARTESIAN_POINT('Ctrl Pts',(22.3831266916095,6.28717208360312,36.6398600238435));
#57885=CARTESIAN_POINT('Ctrl Pts',(20.0723564327029,6.4128948785222,35.3060661917509));
#57886=CARTESIAN_POINT('Ctrl Pts',(17.695645662784,6.53861767344128,36.5184650915059));
#57887=CARTESIAN_POINT('Ctrl Pts',(17.418959685041,6.66434046836036,39.1721625206974));
#57888=CARTESIAN_POINT('Ctrl Pts',(19.4944504378819,6.79006326327943,40.8487672179494));
#57889=CARTESIAN_POINT('Ctrl Pts',(22.0306631365517,6.91578605819852,40.0203408041494));
#57890=CARTESIAN_POINT('Ctrl Pts',(22.7162737544373,7.04150885311759,37.4418522436515));
#57891=CARTESIAN_POINT('Ctrl Pts',(20.9264654948829,7.16723164803668,35.463152779355));
#57892=CARTESIAN_POINT('Ctrl Pts',(18.2923424192746,7.29295444295576,35.887488493765));
#57893=CARTESIAN_POINT('Ctrl Pts',(17.2144571141139,7.41867723787484,38.3281499706796));
#57894=CARTESIAN_POINT('Ctrl Pts',(18.6751176504306,7.54440003279391,40.5608917769847));
#57895=CARTESIAN_POINT('Ctrl Pts',(21.3431818120828,7.670122827713,40.5509516922863));
#57896=CARTESIAN_POINT('Ctrl Pts',(22.7871655186511,7.79584562263208,38.3073884034218));
#57897=CARTESIAN_POINT('Ctrl Pts',(21.6911246315466,7.92156841755115,35.8748260609994));
#57898=CARTESIAN_POINT('Ctrl Pts',(19.0539129290207,8.04729121247024,35.4701291224934));
#57899=CARTESIAN_POINT('Ctrl Pts',(17.2788977526653,8.1730140073893,37.4621096193065));
#57900=CARTESIAN_POINT('Ctrl Pts',(17.9837017990567,8.2987368023084,40.0354180796676));
#57901=CARTESIAN_POINT('Ctrl Pts',(20.5260167447122,8.42445959722746,40.8449240358367));
#57902=CARTESIAN_POINT('Ctrl Pts',(22.58895740875,8.55018239214656,39.1529012840289));
#57903=CARTESIAN_POINT('Ctrl Pts',(22.2925062655231,8.67590518706562,36.5013391226503));
#57904=CARTESIAN_POINT('Ctrl Pts',(19.90682782072,8.80162798198472,35.3066828817265));
#57905=CARTESIAN_POINT('Ctrl Pts',(17.6060598791625,8.92735077690378,36.6576573652298));
#57906=CARTESIAN_POINT('Ctrl Pts',(17.4869588468777,9.05307357182287,39.3230804311022));
#57907=CARTESIAN_POINT('Ctrl Pts',(19.6580649411979,9.17879636674194,40.8738749059382));
#57908=CARTESIAN_POINT('Ctrl Pts',(22.1407863497089,9.30451916166103,39.8967569070777));
#57909=CARTESIAN_POINT('Ctrl Pts',(22.6725472064794,9.4302419565801,37.2822023432595));
#57910=CARTESIAN_POINT('Ctrl Pts',(20.7687384543469,9.55596475149919,35.4129304499065));
#57911=CARTESIAN_POINT('Ctrl Pts',(18.1643561025926,9.68168754641826,35.9924627974476));
#57912=CARTESIAN_POINT('Ctrl Pts',(17.2328491554166,9.80741034133735,38.4926547867434));
#57913=CARTESIAN_POINT('Ctrl Pts',(18.8231268502398,9.93313313625642,40.6350091060201));
#57914=CARTESIAN_POINT('Ctrl Pts',(21.4859231034409,10.0588559311755,40.4671362674954));
#57915=CARTESIAN_POINT('Ctrl Pts',(22.7945546320177,10.1845787260945,38.1420236469132));
#57916=CARTESIAN_POINT('Ctrl Pts',(21.5564276540805,10.3103015210136,35.7786136607956));
#57917=CARTESIAN_POINT('Ctrl Pts',(18.8998831142219,10.4360243159327,35.5307502231475));
#57918=CARTESIAN_POINT('Ctrl Pts',(17.2459069281592,10.5617471108518,37.6243184575056));
#57919=CARTESIAN_POINT('Ctrl Pts',(18.1018154579225,10.6874699057709,40.1513890470726));
#57920=CARTESIAN_POINT('Ctrl Pts',(20.6875944915874,10.81319270069,40.8089694338198));
#57921=CARTESIAN_POINT('Ctrl Pts',(22.6467487670819,10.938915495609,38.9977875818823));
#57922=CARTESIAN_POINT('Ctrl Pts',(22.1938442980656,11.0646382905281,36.3684259259055));
#57923=CARTESIAN_POINT('Ctrl Pts',(19.7416260335514,11.1903610854472,35.3170978328922));
#57924=CARTESIAN_POINT('Ctrl Pts',(17.5248714416295,11.3160838803663,36.8019090179151));
#57925=CARTESIAN_POINT('Ctrl Pts',(17.5637731315797,11.4418066752854,39.4697080797815));
#57926=CARTESIAN_POINT('Ctrl Pts',(19.8228788675921,11.5675294702044,40.8892525311785));
#57927=CARTESIAN_POINT('Ctrl Pts',(22.2434002171962,11.6932522651235,39.7668704339915));
#57928=CARTESIAN_POINT('Ctrl Pts',(22.6194460281224,11.8189750600426,37.1254210734962));
#57929=CARTESIAN_POINT('Ctrl Pts',(20.6083148706532,11.9446978549617,35.3721336916239));
#57930=CARTESIAN_POINT('Ctrl Pts',(18.0428087678081,12.0704206498807,36.1048298170676));
#57931=CARTESIAN_POINT('Ctrl Pts',(17.2609476731339,12.1961434447998,38.6557822675478));
#57932=CARTESIAN_POINT('Ctrl Pts',(18.9752642281328,12.3218662397189,40.7002342540793));
#57933=CARTESIAN_POINT('Ctrl Pts',(21.6234521464007,12.447589034638,40.3750175178618));
#57934=CARTESIAN_POINT('Ctrl Pts',(22.7921411433041,12.5733118295571,37.976511481911));
#57935=CARTESIAN_POINT('Ctrl Pts',(21.4162711158012,12.6990346244761,35.6905441060732));
#57936=CARTESIAN_POINT('Ctrl Pts',(18.7497122356375,12.8247574193952,35.6003836125284));
#57937=CARTESIAN_POINT('Ctrl Pts',(17.2225767766511,12.9504802143143,37.7881958681579));
#57938=CARTESIAN_POINT('Ctrl Pts',(18.2265874757008,13.0762030092334,40.2601642522943));
#57939=CARTESIAN_POINT('Ctrl Pts',(20.8467603281295,13.2019258041525,40.7635124412958));
#57940=CARTESIAN_POINT('Ctrl Pts',(22.6952559895186,13.3276485990715,38.839524664359));
#57941=CARTESIAN_POINT('Ctrl Pts',(22.0874868708618,13.4533713939906,36.2415866600212));
#57942=CARTESIAN_POINT('Ctrl Pts',(19.5773305579474,13.5790941889097,35.3372745121915));
#57943=CARTESIAN_POINT('Ctrl Pts',(17.4523651390159,13.7048169838288,36.9507140506687));
#57944=CARTESIAN_POINT('Ctrl Pts',(17.6491330937556,13.8305397787478,39.6115311334393));
#57945=CARTESIAN_POINT('Ctrl Pts',(19.988314090833,13.956262573667,40.8948461527887));
#57946=CARTESIAN_POINT('Ctrl Pts',(22.3381447951075,14.081985368586,39.6311369943095));
#57947=CARTESIAN_POINT('Ctrl Pts',(22.5571564850828,14.2077081635051,36.972058384033));
#57948=CARTESIAN_POINT('Ctrl Pts',(20.4457574698038,14.3334309584241,35.3409056093809));
#57949=CARTESIAN_POINT('Ctrl Pts',(17.9281267727182,14.4591537533433,36.2241953970884));
#57950=CARTESIAN_POINT('Ctrl Pts',(17.2986541046595,14.5848765482623,38.8169602024926));
#57951=CARTESIAN_POINT('Ctrl Pts',(19.1309961240551,14.7105993431814,40.7563384275775));
#57952=CARTESIAN_POINT('Ctrl Pts',(21.7552865233107,14.8363221381005,40.274918573031));
#57953=CARTESIAN_POINT('Ctrl Pts',(22.779933518428,14.9620449330196,37.8114324838938));
#57954=CARTESIAN_POINT('Ctrl Pts',(21.2711466509595,15.0877677279387,35.6109263229093));
#57955=CARTESIAN_POINT('Ctrl Pts',(18.6039270553319,15.2134905228577,35.6787850340383));
#57956=CARTESIAN_POINT('Ctrl Pts',(17.2089891345057,15.3392133177768,37.9531670100962));
#57957=CARTESIAN_POINT('Ctrl Pts',(18.3575801832093,15.4649361126959,40.3613621389871));
#57958=CARTESIAN_POINT('Ctrl Pts',(21.0029559402006,15.590658907615,40.70871251008));
#57959=CARTESIAN_POINT('Ctrl Pts',(22.7343089247975,15.7163817025341,38.6786676783821));
#57960=CARTESIAN_POINT('Ctrl Pts',(21.9738070592936,15.8421044974531,36.1212662455716));
#57961=CARTESIAN_POINT('Ctrl Pts',(19.414517701543,15.9678272923722,35.3671421448555));
#57962=CARTESIAN_POINT('Ctrl Pts',(17.3887953053845,16.0935500872913,37.1035504924735));
#57963=CARTESIAN_POINT('Ctrl Pts',(17.7427393119042,16.2192728822104,39.7480521121034));
#57964=CARTESIAN_POINT('Ctrl Pts',(20.1537903053346,16.3449956771294,40.8906361497366));
#57965=CARTESIAN_POINT('Ctrl Pts',(22.4246877430453,16.4707184720485,39.4900327071537));
#57966=CARTESIAN_POINT('Ctrl Pts',(22.4858970735737,16.5964412669676,36.8226522330121));
#57967=CARTESIAN_POINT('Ctrl Pts',(20.2816364627001,16.7221640618867,35.3193557435175));
#57968=CARTESIAN_POINT('Ctrl Pts',(17.8207123932173,16.8478868568058,36.3501408327656));
#57969=CARTESIAN_POINT('Ctrl Pts',(17.3458361852168,16.9736096517248,38.9756232194996));
#57970=CARTESIAN_POINT('Ctrl Pts',(19.289776269278,17.0993324466439,40.8031248270383));
#57971=CARTESIAN_POINT('Ctrl Pts',(21.8809637919903,17.225055241563,40.1671905551865));
#57972=CARTESIAN_POINT('Ctrl Pts',(22.7579745786992,17.3507780364821,37.6473657088982));
#57973=CARTESIAN_POINT('Ctrl Pts',(21.1215633200564,17.4765008314011,35.5400395906704));
#57974=CARTESIAN_POINT('Ctrl Pts',(18.4630389514322,17.6022236263203,35.7656794750045));
#57975=CARTESIAN_POINT('Ctrl Pts',(17.2051916637884,17.7279464212393,38.1186532056162));
#57976=CARTESIAN_POINT('Ctrl Pts',(18.4943340906363,17.8536692161584,40.4546277301526));
#57977=CARTESIAN_POINT('Ctrl Pts',(21.1556334324663,17.9793920110775,40.6447618646919));
#57978=CARTESIAN_POINT('Ctrl Pts',(22.7637705849502,18.1051148059966,38.5157808702195));
#57979=CARTESIAN_POINT('Ctrl Pts',(21.8532036238288,18.2308376009156,36.0078867366249));
#57980=CARTESIAN_POINT('Ctrl Pts',(19.2537585713457,18.3565603958347,35.4065959626586));
#57981=CARTESIAN_POINT('Ctrl Pts',(17.3343849278281,18.4822831907538,37.259882231141));
#57982=CARTESIAN_POINT('Ctrl Pts',(17.8442634388288,18.6080059856729,39.8787921341454));
#57983=CARTESIAN_POINT('Ctrl Pts',(20.3187270614952,18.733728780592,40.8766372896946));
#57984=CARTESIAN_POINT('Ctrl Pts',(22.5027254903318,18.859451575511,39.3440525311847));
#57985=CARTESIAN_POINT('Ctrl Pts',(22.405917753016,18.9851743704301,36.6777267001364));
#57986=CARTESIAN_POINT('Ctrl Pts',(20.1165275466479,19.1108971653492,35.3075596853814));
#57987=CARTESIAN_POINT('Ctrl Pts',(17.7209424089894,19.2366199602683,36.4822243392808));
#57988=CARTESIAN_POINT('Ctrl Pts',(17.4023284180584,19.3623427551874,39.1312147673787));
#57989=CARTESIAN_POINT('Ctrl Pts',(19.4510476904639,19.4880655501064,40.8404293390032));
#57990=CARTESIAN_POINT('Ctrl Pts',(22.0000431313306,19.6137883450255,40.0522113443288));
#57991=CARTESIAN_POINT('Ctrl Pts',(22.7263413051272,19.7395111399446,37.4848866682896));
#57992=CARTESIAN_POINT('Ctrl Pts',(20.9680459123426,19.8652339348637,35.4781325508272));
#57993=CARTESIAN_POINT('Ctrl Pts',(18.3275419534764,19.9909567297828,35.8607621537274));
#57994=CARTESIAN_POINT('Ctrl Pts',(17.2111980162402,20.1166795247018,38.2840739269754));
#57995=CARTESIAN_POINT('Ctrl Pts',(18.636368857476,20.2424023196209,40.5396339573463));
#57996=CARTESIAN_POINT('Ctrl Pts',(21.3042584942653,20.36812511454,40.5718846652048));
#57997=CARTESIAN_POINT('Ctrl Pts',(22.7835352147811,20.4938479094591,38.3514359219257));
#57998=CARTESIAN_POINT('Ctrl Pts',(21.7261042842396,20.6195707043781,35.901845228453));
#57999=CARTESIAN_POINT('Ctrl Pts',(19.095608013493,20.7452934992973,35.4554987572394));
#58000=CARTESIAN_POINT('Ctrl Pts',(17.2893424180392,20.8710162942162,37.4191585955583));
#58001=CARTESIAN_POINT('Ctrl Pts',(17.953315331488,20.9967390891354,40.0032970505363));
#58002=CARTESIAN_POINT('Ctrl Pts',(20.4826117417423,21.1224618840544,40.8528900438537));
#58003=CARTESIAN_POINT('Ctrl Pts',(22.5718564964719,21.2481846789736,39.1937252608371));
#58004=CARTESIAN_POINT('Ctrl Pts',(22.3177467990465,21.3739074738926,36.5377577223358));
#58005=CARTESIAN_POINT('Ctrl Pts',(19.9505294976469,21.4996302688117,35.3056216186709));
#58006=CARTESIAN_POINT('Ctrl Pts',(17.6301003264828,21.6253530637308,36.6198612705124));
#58007=CARTESIAN_POINT('Ctrl Pts',(17.466098710572,21.7510758586498,39.2834202783864));
#58008=CARTESIAN_POINT('Ctrl Pts',(19.6183281502704,21.8768153061177,40.8679219699589));
#58009=CARTESIAN_POINT('Ctrl Pts',(21.2749134892681,21.960647155279,40.2428677070976));
#58010=CARTESIAN_POINT('Ctrl Pts',(21.789003873016,22.002571406134,39.6491399398589));
#58011=CARTESIAN_POINT('Ctrl Pts',(17.8632119920882,21.75,39.1124570460077));
#58012=CARTESIAN_POINT('Ctrl Pts',(17.8700018959015,21.75,39.1256475418322));
#58013=CARTESIAN_POINT('Ctrl Pts',(17.8767917997148,21.75,39.1388380376567));
#58014=CARTESIAN_POINT('Ctrl Pts',(17.883581703528,21.75,39.1520285334812));
#58015=CARTESIAN_POINT('Ctrl Pts',(18.7894999003326,0.125000000000002,39.6065358483297));
#58016=CARTESIAN_POINT('Ctrl Pts',(18.7303882588618,0.125000000000002,39.5691127845715));
#58017=CARTESIAN_POINT('Ctrl Pts',(18.6736284073276,0.124999999999993,39.5282205607498));
#58018=CARTESIAN_POINT('Ctrl Pts',(18.6193051004316,0.125,39.4842200364387));
#58019=CARTESIAN_POINT('Ctrl Pts',(18.5728930747577,0.125000000000007,39.44662745269));
#58020=CARTESIAN_POINT('Ctrl Pts',(18.5282595960142,0.124999999999996,39.4067648264074));
#58021=CARTESIAN_POINT('Ctrl Pts',(18.4854679692591,0.125000000000011,39.3648290378955));
#58022=CARTESIAN_POINT('Ctrl Pts',(18.4735851139617,0.125000000000015,39.3531838412892));
#58023=CARTESIAN_POINT('Ctrl Pts',(18.4618427346802,0.125000000000011,39.34137695956));
#58024=CARTESIAN_POINT('Ctrl Pts',(18.4502475884037,0.125000000000005,39.3294177166378));
#58025=CARTESIAN_POINT('Ctrl Pts',(18.3993536433843,0.12499999999998,39.2769256620104));
#58026=CARTESIAN_POINT('Ctrl Pts',(18.3513818001719,0.125000000000007,39.2215941156987));
#58027=CARTESIAN_POINT('Ctrl Pts',(18.3064347445308,0.124999999999996,39.1637898014797));
#58028=CARTESIAN_POINT('Ctrl Pts',(18.2713288207951,0.124999999999988,39.1186417085152));
#58029=CARTESIAN_POINT('Ctrl Pts',(18.2380684235828,0.125000000000006,39.0719839207988));
#58030=CARTESIAN_POINT('Ctrl Pts',(18.2067137449448,0.125,39.0239722527309));
#58031=CARTESIAN_POINT('Ctrl Pts',(18.1984121807502,0.124999999999998,39.0112605311675));
#58032=CARTESIAN_POINT('Ctrl Pts',(18.190244268825,0.125000000000026,38.9984538246221));
#58033=CARTESIAN_POINT('Ctrl Pts',(18.1822112672552,0.125000000000005,38.9855548636928));
#58034=CARTESIAN_POINT('Ctrl Pts',(18.1745479872583,0.124999999999984,38.9732495817366));
#58035=CARTESIAN_POINT('Ctrl Pts',(18.1670119998787,0.124999999999989,38.960867533343));
#58036=CARTESIAN_POINT('Ctrl Pts',(18.1596062445286,0.124999999999994,38.9484152505001));
#58037=CARTESIAN_POINT('Ctrl Pts',(18.1209741842544,0.125000000000019,38.883458022156));
#58038=CARTESIAN_POINT('Ctrl Pts',(18.0858635979701,0.124999999999999,38.8165609525249));
#58039=CARTESIAN_POINT('Ctrl Pts',(18.0543793695552,0.125000000000003,38.7480970247487));
#58040=CARTESIAN_POINT('Ctrl Pts',(18.0223692110303,0.125000000000007,38.6784894373409));
#58041=CARTESIAN_POINT('Ctrl Pts',(17.9941068720973,0.125000000000014,38.607261439698));
#58042=CARTESIAN_POINT('Ctrl Pts',(17.9697368784911,0.125000000000005,38.5347637724566));
#58043=CARTESIAN_POINT('Ctrl Pts',(17.9523900077114,0.124999999999998,38.4831590126941));
#58044=CARTESIAN_POINT('Ctrl Pts',(17.9370159956698,0.125000000000009,38.4309100395559));
#58045=CARTESIAN_POINT('Ctrl Pts',(17.9236803055237,0.125000000000006,38.3781343478896));
#58046=CARTESIAN_POINT('Ctrl Pts',(17.9125026607243,0.125000000000004,38.3338990717977));
#58047=CARTESIAN_POINT('Ctrl Pts',(17.9027571739107,0.124999999999998,38.2892935789823));
#58048=CARTESIAN_POINT('Ctrl Pts',(17.8944894387071,0.124999999999992,38.2443844913444));
#58049=CARTESIAN_POINT('Ctrl Pts',(17.8922469722116,0.12499999999999,38.2322037523763));
#58050=CARTESIAN_POINT('Ctrl Pts',(17.8901140385265,0.125000000000003,38.2200045883144));
#58051=CARTESIAN_POINT('Ctrl Pts',(17.8880928384044,0.125000000000004,38.2077979591711));
#58052=CARTESIAN_POINT('Ctrl Pts',(17.8752443028934,0.125000000000006,38.1302018288823));
#58053=CARTESIAN_POINT('Ctrl Pts',(17.8668864697125,0.125000000000001,38.0521935532589));
#58054=CARTESIAN_POINT('Ctrl Pts',(17.8631561393029,0.125000000000009,37.9741425264019));
#58055=CARTESIAN_POINT('Ctrl Pts',(17.8618719786648,0.125000000000011,37.9472735776917));
#58056=CARTESIAN_POINT('Ctrl Pts',(17.861136579869,0.124999999999983,37.920399299391));
#58057=CARTESIAN_POINT('Ctrl Pts',(17.8609567607682,0.124999999999984,37.893534042365));
#58058=CARTESIAN_POINT('Ctrl Pts',(17.8604471216823,0.124999999999988,37.8173931598032));
#58059=CARTESIAN_POINT('Ctrl Pts',(17.864396119628,0.124999999999993,37.7413254308285));
#58060=CARTESIAN_POINT('Ctrl Pts',(17.8725735026586,0.125,37.6655923866698));
#58061=CARTESIAN_POINT('Ctrl Pts',(17.8807508856893,0.125000000000007,37.5898593425112));
#58062=CARTESIAN_POINT('Ctrl Pts',(17.8931569243958,0.124999999999979,37.5144602026434));
#58063=CARTESIAN_POINT('Ctrl Pts',(17.9096135186795,0.124999999999975,37.4396529031886));
#58064=CARTESIAN_POINT('Ctrl Pts',(17.913388066869,0.124999999999975,37.4224948113105));
#58065=CARTESIAN_POINT('Ctrl Pts',(17.9173773022217,0.124999999999984,37.4053627429111));
#58066=CARTESIAN_POINT('Ctrl Pts',(17.9215715350817,0.124999999999988,37.3882904321903));
#58067=CARTESIAN_POINT('Ctrl Pts',(17.9402979407093,0.125000000000007,37.3120660006368));
#58068=CARTESIAN_POINT('Ctrl Pts',(17.9631261749276,0.124999999999991,37.2369326093909));
#58069=CARTESIAN_POINT('Ctrl Pts',(17.9897910243411,0.124999999999986,37.1631633241872));
#58070=CARTESIAN_POINT('Ctrl Pts',(18.0169444069738,0.12499999999998,37.0880424938904));
#58071=CARTESIAN_POINT('Ctrl Pts',(18.0480764496311,0.124999999999978,37.0143353847301));
#58072=CARTESIAN_POINT('Ctrl Pts',(18.0829617098189,0.124999999999994,36.9423267037387));
#58073=CARTESIAN_POINT('Ctrl Pts',(18.1182336230504,0.125000000000011,36.8695199098616));
#58074=CARTESIAN_POINT('Ctrl Pts',(18.1573426808453,0.125000000000015,36.7984484679073));
#58075=CARTESIAN_POINT('Ctrl Pts',(18.2001077312806,0.125,36.7294163768159));
#58076=CARTESIAN_POINT('Ctrl Pts',(18.2183117477341,0.124999999999993,36.7000311356142));
#58077=CARTESIAN_POINT('Ctrl Pts',(18.237178840091,0.124999999999991,36.6710156254998));
#58078=CARTESIAN_POINT('Ctrl Pts',(18.2566976515838,0.124999999999997,36.6423944743196));
#58079=CARTESIAN_POINT('Ctrl Pts',(18.2653932320242,0.125,36.6296438249024));
#58080=CARTESIAN_POINT('Ctrl Pts',(18.2742193927629,0.125000000000004,36.6169699325046));
#58081=CARTESIAN_POINT('Ctrl Pts',(18.283161973467,0.124999999999999,36.6043931101447));
#58082=CARTESIAN_POINT('Ctrl Pts',(18.3314585616185,0.124999999999973,36.5364689135547));
#58083=CARTESIAN_POINT('Ctrl Pts',(18.383226098352,0.12499999999998,36.4712564282192));
#58084=CARTESIAN_POINT('Ctrl Pts',(18.4382186185833,0.124999999999998,36.4090539912327));
#58085=CARTESIAN_POINT('Ctrl Pts',(18.4931810653168,0.125000000000015,36.3468855705967));
#58086=CARTESIAN_POINT('Ctrl Pts',(18.5513653889031,0.124999999999998,36.2877229691864));
#58087=CARTESIAN_POINT('Ctrl Pts',(18.6125750949098,0.125000000000011,36.23187952165));
#58088=CARTESIAN_POINT('Ctrl Pts',(18.6730802615304,0.125000000000024,36.1766788464909));
#58089=CARTESIAN_POINT('Ctrl Pts',(18.736542045183,0.125000000000005,36.1247204853757));
#58090=CARTESIAN_POINT('Ctrl Pts',(18.802811802905,0.125000000000003,36.0763355898799));
#58091=CARTESIAN_POINT('Ctrl Pts',(18.8375759192312,0.125000000000002,36.0509536027825));
#58092=CARTESIAN_POINT('Ctrl Pts',(18.8731134037565,0.124999999999986,36.0265555500945));
#58093=CARTESIAN_POINT('Ctrl Pts',(18.9094067387628,0.124999999999998,36.0031936714508));
#58094=CARTESIAN_POINT('Origin',(20.,0.125,38.1));
#58095=CARTESIAN_POINT('',(21.1298171225045,0.125,36.0240655813356));
#58096=CARTESIAN_POINT('',(20.,0.125,40.46347));
#58097=CARTESIAN_POINT('Origin',(20.,0.125,38.1));
#58098=CARTESIAN_POINT('Ctrl Pts',(21.1298171225045,0.125000000000001,36.0240655813356));
#58099=CARTESIAN_POINT('Ctrl Pts',(21.1990795490775,0.124999999999983,36.0708787850807));
#58100=CARTESIAN_POINT('Ctrl Pts',(21.2656055745096,0.124999999999974,36.1216762809117));
#58101=CARTESIAN_POINT('Ctrl Pts',(21.3292135975137,0.124999999999986,36.1760987535025));
#58102=CARTESIAN_POINT('Ctrl Pts',(21.3840237393438,0.124999999999996,36.2229938352951));
#58103=CARTESIAN_POINT('Ctrl Pts',(21.4366668305791,0.125000000000016,36.2725815275598));
#58104=CARTESIAN_POINT('Ctrl Pts',(21.4870006796613,0.124999999999999,36.3246488141442));
#58105=CARTESIAN_POINT('Ctrl Pts',(21.4981487712734,0.124999999999995,36.3361808326848));
#58106=CARTESIAN_POINT('Ctrl Pts',(21.5091811000541,0.124999999999995,36.3478321489414));
#58107=CARTESIAN_POINT('Ctrl Pts',(21.5200905103336,0.124999999999994,36.3595940943587));
#58108=CARTESIAN_POINT('Ctrl Pts',(21.5765602420148,0.124999999999991,36.4204767529757));
#58109=CARTESIAN_POINT('Ctrl Pts',(21.6297871336939,0.124999999999987,36.4843697963929));
#58110=CARTESIAN_POINT('Ctrl Pts',(21.679573757162,0.124999999999998,36.5509334434494));
#58111=CARTESIAN_POINT('Ctrl Pts',(21.7155347807542,0.125000000000005,36.5990125601968));
#58112=CARTESIAN_POINT('Ctrl Pts',(21.7497000611184,0.125000000000016,36.6484856808021));
#58113=CARTESIAN_POINT('Ctrl Pts',(21.7819792229568,0.124999999999998,36.6992303718909));
#58114=CARTESIAN_POINT('Ctrl Pts',(21.7899338814766,0.124999999999994,36.71173555066));
#58115=CARTESIAN_POINT('Ctrl Pts',(21.7977739294712,0.124999999999996,36.724317963909));
#58116=CARTESIAN_POINT('Ctrl Pts',(21.805497878986,0.124999999999994,36.736975798943));
#58117=CARTESIAN_POINT('Ctrl Pts',(21.8128135352517,0.124999999999993,36.748964532168));
#58118=CARTESIAN_POINT('Ctrl Pts',(21.8200197531888,0.12500000000002,36.7610122599784));
#58119=CARTESIAN_POINT('Ctrl Pts',(21.8271155484798,0.125000000000018,36.7731169252624));
#58120=CARTESIAN_POINT('Ctrl Pts',(21.8680753538153,0.125000000000005,36.8429899575797));
#58121=CARTESIAN_POINT('Ctrl Pts',(21.9053620001245,0.125000000000023,36.9147624502371));
#58122=CARTESIAN_POINT('Ctrl Pts',(21.9387994467918,0.125000000000017,36.988118275587));
#58123=CARTESIAN_POINT('Ctrl Pts',(21.9716838232338,0.125000000000011,37.0602607629909));
#58124=CARTESIAN_POINT('Ctrl Pts',(22.0008454994912,0.125000000000007,37.1339355659331));
#58125=CARTESIAN_POINT('Ctrl Pts',(22.0260689714308,0.125000000000008,37.2088524461688));
#58126=CARTESIAN_POINT('Ctrl Pts',(22.0443784407949,0.125000000000009,37.2632338702174));
#58127=CARTESIAN_POINT('Ctrl Pts',(22.0606118324242,0.124999999999994,37.3182700210257));
#58128=CARTESIAN_POINT('Ctrl Pts',(22.0746694285563,0.12500000000001,37.3738493642667));
#58129=CARTESIAN_POINT('Ctrl Pts',(22.0852126256554,0.125000000000022,37.4155338716975));
#58130=CARTESIAN_POINT('Ctrl Pts',(22.0945316433851,0.125000000000003,37.457523925268));
#58131=CARTESIAN_POINT('Ctrl Pts',(22.1025786506068,0.125000000000016,37.4997713275294));
#58132=CARTESIAN_POINT('Ctrl Pts',(22.104914689879,0.12500000000002,37.5120357120529));
#58133=CARTESIAN_POINT('Ctrl Pts',(22.1071434994731,0.124999999999998,37.5243217754371));
#58134=CARTESIAN_POINT('Ctrl Pts',(22.1092638278586,0.125000000000007,37.5366283146355));
#58135=CARTESIAN_POINT('Ctrl Pts',(22.1115374551523,0.125000000000018,37.5498246117773));
#58136=CARTESIAN_POINT('Ctrl Pts',(22.1136847973057,0.12500000000001,37.5630356275134));
#58137=CARTESIAN_POINT('Ctrl Pts',(22.115704161457,0.125000000000008,37.5762552059159));
#58138=CARTESIAN_POINT('Ctrl Pts',(22.1272139470258,0.124999999999996,37.6516029398159));
#58139=CARTESIAN_POINT('Ctrl Pts',(22.1345787609411,0.125000000000017,37.7272779645949));
#58140=CARTESIAN_POINT('Ctrl Pts',(22.1376065452356,0.125000000000015,37.8030135753196));
#58141=CARTESIAN_POINT('Ctrl Pts',(22.1386716922244,0.125000000000014,37.8296566746506));
#58142=CARTESIAN_POINT('Ctrl Pts',(22.1391996378238,0.125000000000004,37.8563072559143));
#58143=CARTESIAN_POINT('Ctrl Pts',(22.139180474393,0.125000000000001,37.8829535563851));
#58144=CARTESIAN_POINT('Ctrl Pts',(22.1391246242936,0.124999999999991,37.9606118082407));
#58145=CARTESIAN_POINT('Ctrl Pts',(22.1344253216884,0.124999999999991,38.038235169254));
#58146=CARTESIAN_POINT('Ctrl Pts',(22.1252506920211,0.125000000000001,38.1154926420498));
#58147=CARTESIAN_POINT('Ctrl Pts',(22.1164517360991,0.12500000000001,38.1895866515542));
#58148=CARTESIAN_POINT('Ctrl Pts',(22.1035356471174,0.125000000000017,38.2633447580134));
#58149=CARTESIAN_POINT('Ctrl Pts',(22.0866122802599,0.125000000000001,38.3364515381243));
#58150=CARTESIAN_POINT('Ctrl Pts',(22.0830468966271,0.124999999999997,38.3518535393601));
#58151=CARTESIAN_POINT('Ctrl Pts',(22.0793025198156,0.125000000000007,38.3672300166854));
#58152=CARTESIAN_POINT('Ctrl Pts',(22.0753868276315,0.125000000000004,38.3825525151837));
#58153=CARTESIAN_POINT('Ctrl Pts',(22.0566063195045,0.124999999999987,38.456042537903));
#58154=CARTESIAN_POINT('Ctrl Pts',(22.0338646030691,0.124999999999995,38.5284059841618));
#58155=CARTESIAN_POINT('Ctrl Pts',(22.0073469685367,0.125000000000004,38.5993445283026));
#58156=CARTESIAN_POINT('Ctrl Pts',(21.9809376237444,0.125000000000013,38.6699933815777));
#58157=CARTESIAN_POINT('Ctrl Pts',(21.950782486382,0.125000000000022,38.739229785024));
#58158=CARTESIAN_POINT('Ctrl Pts',(21.9170213476871,0.125000000000023,38.8067321116329));
#58159=CARTESIAN_POINT('Ctrl Pts',(21.8835439844181,0.125000000000023,38.8736670550841));
#58160=CARTESIAN_POINT('Ctrl Pts',(21.8465203603964,0.125000000000007,38.9388977000179));
#58161=CARTESIAN_POINT('Ctrl Pts',(21.8060536812907,0.125000000000008,39.0020721563215));
#58162=CARTESIAN_POINT('Ctrl Pts',(21.7912130945568,0.125000000000008,39.0252405017074));
#58163=CARTESIAN_POINT('Ctrl Pts',(21.7759091563608,0.125000000000006,39.0481318698271));
#58164=CARTESIAN_POINT('Ctrl Pts',(21.7601460791288,0.125000000000019,39.0707272944136));
#58165=CARTESIAN_POINT('Ctrl Pts',(21.7533802017367,0.125000000000025,39.0804257733415));
#58166=CARTESIAN_POINT('Ctrl Pts',(21.7465304429989,0.125000000000001,39.0900685762855));
#58167=CARTESIAN_POINT('Ctrl Pts',(21.7396044503488,0.125000000000002,39.0996444763858));
#58168=CARTESIAN_POINT('Ctrl Pts',(21.6966889753724,0.12500000000001,39.15897955251));
#58169=CARTESIAN_POINT('Ctrl Pts',(21.6507769855365,0.125000000000004,39.2158537293796));
#58170=CARTESIAN_POINT('Ctrl Pts',(21.6020040083035,0.12500000000001,39.2699748866719));
#58171=CARTESIAN_POINT('Ctrl Pts',(21.5546149694859,0.125000000000016,39.3225603503708));
#58172=CARTESIAN_POINT('Ctrl Pts',(21.5045243298926,0.125000000000015,39.3725472978381));
#58173=CARTESIAN_POINT('Ctrl Pts',(21.4518289233424,0.125000000000007,39.4196284362144));
#58174=CARTESIAN_POINT('Ctrl Pts',(21.3998272581665,0.125,39.466089745733));
#58175=CARTESIAN_POINT('Ctrl Pts',(21.3452884405721,0.124999999999977,39.5097217501793));
#58176=CARTESIAN_POINT('Ctrl Pts',(21.2882869596872,0.124999999999972,39.5501829399227));
#58177=CARTESIAN_POINT('Ctrl Pts',(21.2621895577287,0.12499999999997,39.5687075802664));
#58178=CARTESIAN_POINT('Ctrl Pts',(21.2355757334482,0.124999999999981,39.5865668821878));
#58179=CARTESIAN_POINT('Ctrl Pts',(21.2084517554459,0.124999999999999,39.6037243469665));
#58180=CARTESIAN_POINT('Origin',(20.,0.125,38.1));
#58181=CARTESIAN_POINT('Ctrl Pts',(21.4817071279173,-0.127571370348389,
39.9452406715398));
#58182=CARTESIAN_POINT('Ctrl Pts',(22.0940973315942,-0.0856471207638085,
39.4535296222823));
#58183=CARTESIAN_POINT('Ctrl Pts',(22.7801769572279,-0.00181527287286855,
37.8212744373185));
#58184=CARTESIAN_POINT('Ctrl Pts',(21.2766046668293,0.123924173324431,35.6117430346468));
#58185=CARTESIAN_POINT('Ctrl Pts',(18.6087965704713,0.249646968243511,35.6768240224488));
#58186=CARTESIAN_POINT('Ctrl Pts',(17.2093803185729,0.37536976316259,37.9469002644723));
#58187=CARTESIAN_POINT('Ctrl Pts',(18.352852044017,0.501092558081669,40.3581971702879));
#58188=CARTESIAN_POINT('Ctrl Pts',(20.9975643581775,0.626815353000749,40.7106596417877));
#58189=CARTESIAN_POINT('Ctrl Pts',(22.7330915324132,0.752538147919828,38.6844033171128));
#58190=CARTESIAN_POINT('Ctrl Pts',(21.9779124571561,0.878260942838908,36.1253306736311));
#58191=CARTESIAN_POINT('Ctrl Pts',(19.4201843152843,1.00398373775798,35.3659513962466));
#58192=CARTESIAN_POINT('Ctrl Pts',(17.390869413503,1.12970653267706,37.0981277714779));
#58193=CARTESIAN_POINT('Ctrl Pts',(17.7393253384899,1.25542932759614,39.7433712754338));
#58194=CARTESIAN_POINT('Ctrl Pts',(20.148002280105,1.38115212251522,40.8909464790416));
#58195=CARTESIAN_POINT('Ctrl Pts',(22.4217990278434,1.5068749174343,39.4950599053239));
#58196=CARTESIAN_POINT('Ctrl Pts',(22.488540977682,1.63259771235338,36.8278104747239));
#58197=CARTESIAN_POINT('Ctrl Pts',(20.2874031381624,1.75832050727246,35.31994644143));
#58198=CARTESIAN_POINT('Ctrl Pts',(17.8243466987466,1.88404330219154,36.3456244965799));
#58199=CARTESIAN_POINT('Ctrl Pts',(17.3440259713813,2.00976609711062,38.9701163209587));
#58200=CARTESIAN_POINT('Ctrl Pts',(19.2841712887778,2.13548889202969,40.8016456505112));
#58201=CARTESIAN_POINT('Ctrl Pts',(21.87667199869,2.26121168694878,40.171087277866));
#58202=CARTESIAN_POINT('Ctrl Pts',(22.7589072219985,2.38693448186786,37.6530870516505));
#58203=CARTESIAN_POINT('Ctrl Pts',(21.1268704479201,2.51265727678694,35.5423715711052));
#58204=CARTESIAN_POINT('Ctrl Pts',(18.467884028376,2.63838007170603,35.7624968697667));
#58205=CARTESIAN_POINT('Ctrl Pts',(17.2051592290664,2.7641028666251,38.1128564263638));
#58206=CARTESIAN_POINT('Ctrl Pts',(18.489453703936,2.88982566154418,40.4514995436837));
#58207=CARTESIAN_POINT('Ctrl Pts',(21.1503527309155,3.01554845646325,40.6471530808971));
#58208=CARTESIAN_POINT('Ctrl Pts',(22.7629020249366,3.14127125138234,38.5215123030072));
#58209=CARTESIAN_POINT('Ctrl Pts',(21.8575387491212,3.26699404630141,36.0117351662413));
#58210=CARTESIAN_POINT('Ctrl Pts',(19.2593466568257,3.3927168412205,35.4050542034166));
#58211=CARTESIAN_POINT('Ctrl Pts',(17.3361333895618,3.51843963613957,37.2543553330546));
#58212=CARTESIAN_POINT('Ctrl Pts',(17.8405788528435,3.64416243105865,39.8743169192987));
#58213=CARTESIAN_POINT('Ctrl Pts',(20.3129672980339,3.76988522597773,40.8772921508858));
#58214=CARTESIAN_POINT('Ctrl Pts',(22.5001395877116,3.89560802089681,39.3492406745362));
#58215=CARTESIAN_POINT('Ctrl Pts',(22.408862320693,4.02133081581589,36.6827200202844));
#58216=CARTESIAN_POINT('Ctrl Pts',(20.1223191118479,4.14705361073498,35.3078076255658));
#58217=CARTESIAN_POINT('Ctrl Pts',(17.7243029566375,4.27277640565405,36.477500943669));
#58218=CARTESIAN_POINT('Ctrl Pts',(17.4001953724141,4.39849920057313,39.1258246045731));
#58219=CARTESIAN_POINT('Ctrl Pts',(19.4453649798832,4.52422199549221,40.8392846174551));
#58220=CARTESIAN_POINT('Ctrl Pts',(21.9959895315176,4.6499447904113,40.0563552875276));
#58221=CARTESIAN_POINT('Ctrl Pts',(22.727611062039,4.77566758533037,37.490542769993));
#58222=CARTESIAN_POINT('Ctrl Pts',(20.9734816986179,4.90139038024944,35.4801462629716));
#58223=CARTESIAN_POINT('Ctrl Pts',(18.3321902920983,5.02711317516853,35.8572982812701));
#58224=CARTESIAN_POINT('Ctrl Pts',(17.2108221363827,5.1528359700876,38.2782892763806));
#58225=CARTESIAN_POINT('Ctrl Pts',(18.6313124825418,5.27855876500669,40.5368000944927));
#58226=CARTESIAN_POINT('Ctrl Pts',(21.2991273711915,5.40428155992577,40.5745844690344));
#58227=CARTESIAN_POINT('Ctrl Pts',(22.7830098916132,5.53000435484485,38.3572084060612));
#58228=CARTESIAN_POINT('Ctrl Pts',(21.7306549615396,5.65572714976392,35.9054308794062));
#58229=CARTESIAN_POINT('Ctrl Pts',(19.1011040823716,5.78144994468301,35.4536276999946));
#58230=CARTESIAN_POINT('Ctrl Pts',(17.2907430656818,5.90717273960207,37.4135401797522));
#58231=CARTESIAN_POINT('Ctrl Pts',(17.9494062952009,6.03289553452117,39.9990433588531));
#58232=CARTESIAN_POINT('Ctrl Pts',(20.4768349091098,6.15861832944025,40.8538933694716));
#58233=CARTESIAN_POINT('Ctrl Pts',(22.5697100714367,6.28434112435933,39.1990406588125));
#58234=CARTESIAN_POINT('Ctrl Pts',(22.3207340819822,6.4100639192784,36.5426003911355));
#58235=CARTESIAN_POINT('Ctrl Pts',(19.9568059649405,6.53578671419749,35.3054634559017));
#58236=CARTESIAN_POINT('Ctrl Pts',(17.6322418220212,6.66150950911657,36.6150685431375));
#58237=CARTESIAN_POINT('Ctrl Pts',(17.4654842261801,6.78723230403565,39.2779346387738));
#58238=CARTESIAN_POINT('Ctrl Pts',(19.60850420023,6.91295509895471,40.8673148103763));
#58239=CARTESIAN_POINT('Ctrl Pts',(22.1083056259307,7.03867789387381,39.9347609132075));
#58240=CARTESIAN_POINT('Ctrl Pts',(22.6867471234151,7.16440068879287,37.3301363005141));
#58241=CARTESIAN_POINT('Ctrl Pts',(20.8166782167678,7.29012348371197,35.4271107559007));
#58242=CARTESIAN_POINT('Ctrl Pts',(18.2023468176975,7.41584627863103,35.9599665289712));
#58243=CARTESIAN_POINT('Ctrl Pts',(17.2262687851341,7.54156907355013,38.4430967336541));
#58244=CARTESIAN_POINT('Ctrl Pts',(18.7779722764348,7.66729186846919,40.6135529562361));
#58245=CARTESIAN_POINT('Ctrl Pts',(21.4433449959297,7.79301466338828,40.4933356312248));
#58246=CARTESIAN_POINT('Ctrl Pts',(22.7933556523239,7.91873745830735,38.1920022858178));
#58247=CARTESIAN_POINT('Ctrl Pts',(21.5977004670959,8.04446025322644,35.8068245949324));
#58248=CARTESIAN_POINT('Ctrl Pts',(18.9460146110701,8.17018304814552,35.5114840118539));
#58249=CARTESIAN_POINT('Ctrl Pts',(17.2548561407841,8.2959058430646,37.5751329566698));
#58250=CARTESIAN_POINT('Ctrl Pts',(18.0654267098815,8.42162863798366,40.1171084269631));
#58251=CARTESIAN_POINT('Ctrl Pts',(20.6390299020081,8.54735143290277,40.8208346155739));
#58252=CARTESIAN_POINT('Ctrl Pts',(22.6302666518364,8.67307422782184,39.0449854820062));
#58253=CARTESIAN_POINT('Ctrl Pts',(22.2244652857459,8.79879702274091,36.4079437321775));
#58254=CARTESIAN_POINT('Ctrl Pts',(19.7914443319572,8.92451981766,35.3129218248688));
#58255=CARTESIAN_POINT('Ctrl Pts',(17.5484861937545,9.05024261257907,36.7578449125555));
#58256=CARTESIAN_POINT('Ctrl Pts',(17.5396635304358,9.17596540749815,39.4259127714512));
#58257=CARTESIAN_POINT('Ctrl Pts',(19.7730166903984,9.30168820241722,40.8856379517316));
#58258=CARTESIAN_POINT('Ctrl Pts',(22.2132263089687,9.42741099733632,39.8067306542786));
#58259=CARTESIAN_POINT('Ctrl Pts',(22.6364587446177,9.55313379225539,37.1724303212727));
#58260=CARTESIAN_POINT('Ctrl Pts',(20.657010031006,9.67885658717447,35.3834510790116));
#58261=CARTESIAN_POINT('Ctrl Pts',(18.0788090632215,9.80457938209355,36.0701414814314));
#58262=CARTESIAN_POINT('Ctrl Pts',(17.2514449926014,9.93030217701264,38.606700692983));
#58263=CARTESIAN_POINT('Ctrl Pts',(18.9289186394175,10.0560249719317,40.6814888998364));
#58264=CARTESIAN_POINT('Ctrl Pts',(21.5824997256729,10.1817477668508,40.4036915677257));
#58265=CARTESIAN_POINT('Ctrl Pts',(22.7939030166767,10.3074705617699,38.0264734444553));
#58266=CARTESIAN_POINT('Ctrl Pts',(21.4591416370836,10.433193356689,35.7162621990046));
#58267=CARTESIAN_POINT('Ctrl Pts',(18.7946222581744,10.558916151608,35.5784201935143));
#58268=CARTESIAN_POINT('Ctrl Pts',(17.2285984972737,10.6846389465271,37.7385668365352));
#58269=CARTESIAN_POINT('Ctrl Pts',(18.1882331261458,10.8103617414462,40.228097980773));
#58270=CARTESIAN_POINT('Ctrl Pts',(20.7989833370656,10.9360845363653,40.7782318510646));
#58271=CARTESIAN_POINT('Ctrl Pts',(22.6815969114991,11.0618073312843,38.8876155313373));
#58272=CARTESIAN_POINT('Ctrl Pts',(22.1203936189598,11.1875301262034,36.2792223854518));
#58273=CARTESIAN_POINT('Ctrl Pts',(19.6268142603477,11.3132529211225,35.3301565703662));
#58274=CARTESIAN_POINT('Ctrl Pts',(17.4733298657346,11.4389757160416,36.9053292279559));
#58275=CARTESIAN_POINT('Ctrl Pts',(17.6224730826451,11.5646985109607,39.5692399321481));
#58276=CARTESIAN_POINT('Ctrl Pts',(19.9383253815204,11.6904213058798,40.8941897685019));
#58277=CARTESIAN_POINT('Ctrl Pts',(22.3103835449902,11.8161441007988,39.6727136090224));
#58278=CARTESIAN_POINT('Ctrl Pts',(22.5769223247629,11.9418668957179,37.0179780255909));
#58279=CARTESIAN_POINT('Ctrl Pts',(20.4950372175861,12.067589690637,35.3493203795843));
#58280=CARTESIAN_POINT('Ctrl Pts',(17.9620103683644,12.1933124855561,36.1874366723398));
#58281=CARTESIAN_POINT('Ctrl Pts',(17.286262446915,12.3190352804751,38.7685272723994));
#58282=CARTESIAN_POINT('Ctrl Pts',(19.0836220892193,12.4447580753942,40.7403696229124));
#58283=CARTESIAN_POINT('Ctrl Pts',(21.7161034402651,12.5704808703133,40.3059667275995));
#58284=CARTESIAN_POINT('Ctrl Pts',(22.7846500646538,12.6962036652324,37.8612025159488));
#58285=CARTESIAN_POINT('Ctrl Pts',(21.3154645013911,12.8219264601515,35.6340613619667));
#58286=CARTESIAN_POINT('Ctrl Pts',(18.6474580703767,12.9476492550705,35.6542014495105));
#58287=CARTESIAN_POINT('Ctrl Pts',(17.212062240429,13.0733720499896,37.9032685339766));
#58288=CARTESIAN_POINT('Ctrl Pts',(18.3173947696519,13.1990948449087,40.331622696553));
#58289=CARTESIAN_POINT('Ctrl Pts',(20.956134137445,13.3248176398278,40.7262345158379));
#58290=CARTESIAN_POINT('Ctrl Pts',(22.7235207966499,13.4505404347469,38.7274828214233));
#58291=CARTESIAN_POINT('Ctrl Pts',(22.0088841391277,13.5762632296659,36.1568878734034));
#58292=CARTESIAN_POINT('Ctrl Pts',(19.4634932314263,13.701986024585,35.3571072371964));
#58293=CARTESIAN_POINT('Ctrl Pts',(17.4070364676536,13.8277088195041,37.0570041510691));
#58294=CARTESIAN_POINT('Ctrl Pts',(17.7136224075105,13.9534316144232,39.707413364859));
#58295=CARTESIAN_POINT('Ctrl Pts',(20.1038504118531,14.0791544093423,40.8929402630424));
#58296=CARTESIAN_POINT('Ctrl Pts',(22.3994365305938,14.2048772042613,39.5331798758766));
#58297=CARTESIAN_POINT('Ctrl Pts',(22.5083467027926,14.3305999991804,36.8673211936783));
#58298=CARTESIAN_POINT('Ctrl Pts',(20.3313279368224,14.4563227940995,35.3248383796171));
#58299=CARTESIAN_POINT('Ctrl Pts',(17.8523604338763,14.5820455890186,36.3114406593615));
#58300=CARTESIAN_POINT('Ctrl Pts',(17.3305990171115,14.7077683839377,38.9280088245419));
#58301=CARTESIAN_POINT('Ctrl Pts',(19.2415399646442,14.8334911788567,40.7899885865433));
#58302=CARTESIAN_POINT('Ctrl Pts',(21.8436874911296,14.9592139737758,40.2005039052613));
#58303=CARTESIAN_POINT('Ctrl Pts',(22.7656292533077,15.0849367686949,37.6967692295793));
#58304=CARTESIAN_POINT('Ctrl Pts',(21.1671730436487,15.210659563614,35.5605104238951));
#58305=CARTESIAN_POINT('Ctrl Pts',(18.5050382630183,15.3363823585331,35.7385619580589));
#58306=CARTESIAN_POINT('Ctrl Pts',(17.2053053753228,15.4621051534521,38.0686603164341));
#58307=CARTESIAN_POINT('Ctrl Pts',(18.452458573503,15.5878279483712,40.4273194353679));
#58308=CARTESIAN_POINT('Ctrl Pts',(21.1099310572534,15.7135507432903,40.6650250036032));
#58309=CARTESIAN_POINT('Ctrl Pts',(22.7558912487344,15.8392735382094,38.5651490579532));
#58310=CARTESIAN_POINT('Ctrl Pts',(21.8903279937497,15.9649963331285,36.0413693150515));
#58311=CARTESIAN_POINT('Ctrl Pts',(19.3020541347117,16.0907191280475,35.3936792891285));
#58312=CARTESIAN_POINT('Ctrl Pts',(17.3498385402515,16.2164419229666,37.2123376440172));
#58313=CARTESIAN_POINT('Ctrl Pts',(17.8127917758874,16.3421647178857,39.8399483915737));
#58314=CARTESIAN_POINT('Ctrl Pts',(20.2690111607896,16.4678875128048,40.8818938183072));
#58315=CARTESIAN_POINT('Ctrl Pts',(22.4800728900715,16.5936103077239,39.3886189044468));
#58316=CARTESIAN_POINT('Ctrl Pts',(22.4309724249204,16.7193331026429,36.7209882922026));
#58317=CARTESIAN_POINT('Ctrl Pts',(20.1664564401246,16.845055897562,35.3100909558722));
#58318=CARTESIAN_POINT('Ctrl Pts',(17.7502438844354,16.9707786924811,36.4417184673749));
#58319=CARTESIAN_POINT('Ctrl Pts',(17.3842991815377,17.0965014874002,39.0845859278207));
#58320=CARTESIAN_POINT('Ctrl Pts',(19.4021183290917,17.2222242823192,40.8301717397549));
#58321=CARTESIAN_POINT('Ctrl Pts',(21.9648043451713,17.3479470772383,40.0876730380422));
#58322=CARTESIAN_POINT('Ctrl Pts',(22.7369073029115,17.4736698721574,37.5337503763873));
#58323=CARTESIAN_POINT('Ctrl Pts',(21.0147874333784,17.5993926670765,35.4958673831745));
#58324=CARTESIAN_POINT('Ctrl Pts',(18.3678624093392,17.7251154619956,35.8312058034916));
#58325=CARTESIAN_POINT('Ctrl Pts',(17.2083516033483,17.8508382569146,38.2341620307038));
#58326=CARTESIAN_POINT('Ctrl Pts',(18.5929507675084,17.9765610518337,40.5148525168716));
#58327=CARTESIAN_POINT('Ctrl Pts',(21.2598346151463,18.1022838467528,40.5948180221049));
#58328=CARTESIAN_POINT('Ctrl Pts',(22.7785947203223,18.2280066416719,38.4011836673442));
#58329=CARTESIAN_POINT('Ctrl Pts',(21.7651410481622,18.353729436591,35.9330719207845));
#58330=CARTESIAN_POINT('Ctrl Pts',(19.143063258592,18.47945223151,35.4397444404324));
#58331=CARTESIAN_POINT('Ctrl Pts',(17.301936719196,18.6051750264291,37.3707848357136));
#58332=CARTESIAN_POINT('Ctrl Pts',(17.9196333271384,18.7308978213482,39.9663801121273));
#58333=CARTESIAN_POINT('Ctrl Pts',(20.4332282839357,18.8566206162673,40.8610891830162));
#58334=CARTESIAN_POINT('Ctrl Pts',(22.5520097742367,18.9823434111863,39.2395377775908));
#58335=CARTESIAN_POINT('Ctrl Pts',(22.3450708948629,19.1080662061055,36.5794926225918));
#58336=CARTESIAN_POINT('Ctrl Pts',(20.0010010672759,19.2337890010245,35.3051298347038));
#58337=CARTESIAN_POINT('Ctrl Pts',(17.6560188969823,19.3595117959436,36.5778131218862));
#58338=CARTESIAN_POINT('Ctrl Pts',(17.4471746169796,19.4852345908627,39.237709333944));
#58339=CARTESIAN_POINT('Ctrl Pts',(19.5647938291461,19.6109573857818,40.8607781586984));
#58340=CARTESIAN_POINT('Ctrl Pts',(22.0790293183196,19.7366801807008,39.9678698530205));
#58341=CARTESIAN_POINT('Ctrl Pts',(22.6985846456872,19.8624029756199,37.372717893521));
#58342=CARTESIAN_POINT('Ctrl Pts',(20.8588428161005,19.988125770539,35.4403587830203));
#58343=CARTESIAN_POINT('Ctrl Pts',(18.2364104968719,20.1138485654581,35.9318084182521));
#58344=CARTESIAN_POINT('Ctrl Pts',(17.2211925474339,20.2395713603771,38.3991923551073));
#58345=CARTESIAN_POINT('Ctrl Pts',(18.7383740669321,20.3652941552962,40.5939164138209));
#58346=CARTESIAN_POINT('Ctrl Pts',(21.4053276546846,20.4910169502153,40.5158569002854));
#58347=CARTESIAN_POINT('Ctrl Pts',(22.7915347766057,20.6167397451344,38.2361674958629));
#58348=CARTESIAN_POINT('Ctrl Pts',(21.6337949755707,20.7424625400534,35.8323645322771));
#58349=CARTESIAN_POINT('Ctrl Pts',(18.9870152307706,20.8681853349726,35.4951624966401));
#58350=CARTESIAN_POINT('Ctrl Pts',(17.2636212567748,20.9939081298916,37.5317484821045));
#58351=CARTESIAN_POINT('Ctrl Pts',(18.0335354157021,21.1196309248107,40.086345359573));
#58352=CARTESIAN_POINT('Ctrl Pts',(20.5963850122518,21.2453537197298,40.8304436732054));
#58353=CARTESIAN_POINT('Ctrl Pts',(22.6141023677897,21.3710765146489,39.0867611723361));
#58354=CARTESIAN_POINT('Ctrl Pts',(22.2526978385088,21.4967993095679,36.4427448448181));
#58355=CARTESIAN_POINT('Ctrl Pts',(19.8316106131819,21.6225368858548,35.3109838910756));
#58356=CARTESIAN_POINT('Ctrl Pts',(18.3297609408629,21.7063668638354,36.2486441106533));
#58357=CARTESIAN_POINT('Ctrl Pts',(17.9420413053583,21.7482892435095,36.9315928900642));
#58358=CARTESIAN_POINT('Ctrl Pts',(21.3897090577788,-0.0427385219042173,
39.8306710798006));
#58359=CARTESIAN_POINT('Ctrl Pts',(21.9640764188518,-0.00081427231963721,
39.3694899961113));
#58360=CARTESIAN_POINT('Ctrl Pts',(22.6075578816433,0.0830175755713031,
37.8385802957988));
#58361=CARTESIAN_POINT('Ctrl Pts',(21.1973412527138,0.208757021768603,35.7662370196645));
#58362=CARTESIAN_POINT('Ctrl Pts',(18.6951753347191,0.334479816687684,35.8272771783663));
#58363=CARTESIAN_POINT('Ctrl Pts',(17.3826477749713,0.460202611606761,37.9564061107638));
#58364=CARTESIAN_POINT('Ctrl Pts',(18.4551222095092,0.585925406525842,40.2179874232035));
#58365=CARTESIAN_POINT('Ctrl Pts',(20.9356263448805,0.71164820144492,40.5485657675615));
#58366=CARTESIAN_POINT('Ctrl Pts',(22.5633959550915,0.837370996364001,38.648118159038));
#58367=CARTESIAN_POINT('Ctrl Pts',(21.855105375019,0.963093791283079,36.2479363922409));
#58368=CARTESIAN_POINT('Ctrl Pts',(19.456184630748,1.08881658620216,35.5357063974009));
#58369=CARTESIAN_POINT('Ctrl Pts',(17.5528683498476,1.21453938112124,37.1603332571726));
#58370=CARTESIAN_POINT('Ctrl Pts',(17.8796889111226,1.34026217604032,39.6413356011684));
#58371=CARTESIAN_POINT('Ctrl Pts',(20.1388129309487,1.46598497095939,40.7176587320276));
#58372=CARTESIAN_POINT('Ctrl Pts',(22.2714313656875,1.59170776587848,39.4084416954231));
#58373=CARTESIAN_POINT('Ctrl Pts',(22.3340293585545,1.71743056079755,36.906799756054));
#58374=CARTESIAN_POINT('Ctrl Pts',(20.2695584956116,1.84315335571663,35.4925578552857));
#58375=CARTESIAN_POINT('Ctrl Pts',(17.9594313596992,1.96887615063571,36.4545523390475));
#58376=CARTESIAN_POINT('Ctrl Pts',(17.5089333814672,2.09459894555479,38.9160914594892));
#58377=CARTESIAN_POINT('Ctrl Pts',(19.3286165497482,2.22032174047387,40.633902524112));
#58378=CARTESIAN_POINT('Ctrl Pts',(21.7601508597217,2.34604453539295,40.0424950418823));
#58379=CARTESIAN_POINT('Ctrl Pts',(22.5876087681188,2.47176733031203,37.6808355371598));
#58380=CARTESIAN_POINT('Ctrl Pts',(21.0569039177257,2.59749012523111,35.701172777603));
#58381=CARTESIAN_POINT('Ctrl Pts',(18.5630119453321,2.72321292015019,35.9076306636672));
#58382=CARTESIAN_POINT('Ctrl Pts',(17.3786887697062,2.84893571506927,38.1120581806159));
#58383=CARTESIAN_POINT('Ctrl Pts',(18.5832423761198,2.97465850998835,40.3054967231031));
#58384=CARTESIAN_POINT('Ctrl Pts',(21.0789282036058,3.10038130490743,40.4890022808));
#58385=CARTESIAN_POINT('Ctrl Pts',(22.5913555367767,3.22610409982651,38.4953409242742));
#58386=CARTESIAN_POINT('Ctrl Pts',(21.7422055790859,3.35182689474558,36.1413939436233));
#58387=CARTESIAN_POINT('Ctrl Pts',(19.3053332603386,3.47754968966468,35.5723813409743));
#58388=CARTESIAN_POINT('Ctrl Pts',(17.501530844058,3.60327248458374,37.306860768114));
#58389=CARTESIAN_POINT('Ctrl Pts',(17.9746556716773,3.72899527950283,39.7641509294657));
#58390=CARTESIAN_POINT('Ctrl Pts',(20.293535396214,3.8547180744219,40.7048521907358));
#58391=CARTESIAN_POINT('Ctrl Pts',(22.3449078196972,3.98044086934098,39.2716762699177));
#58392=CARTESIAN_POINT('Ctrl Pts',(22.259297888858,4.10616366426007,36.7707178577268));
#58393=CARTESIAN_POINT('Ctrl Pts',(20.1147244111011,4.23188645917914,35.4811727292785));
#58394=CARTESIAN_POINT('Ctrl Pts',(17.865599257549,4.35760925409822,36.5782406777038));
#58395=CARTESIAN_POINT('Ctrl Pts',(17.5616152670535,4.48333204901731,39.0621319340425));
#58396=CARTESIAN_POINT('Ctrl Pts',(19.479801847008,4.60905484393638,40.6692045161871));
#58397=CARTESIAN_POINT('Ctrl Pts',(21.8720600575641,4.73477763885547,39.9348866736791));
#58398=CARTESIAN_POINT('Ctrl Pts',(22.55825576296,4.86050043377454,37.5283835064896));
#58399=CARTESIAN_POINT('Ctrl Pts',(20.9130389593609,4.98622322869362,35.6428109915879));
#58400=CARTESIAN_POINT('Ctrl Pts',(18.4357433300734,5.1119460236127,35.9965459275369));
#58401=CARTESIAN_POINT('Ctrl Pts',(17.3840000714084,5.23766881853178,38.2672194306302));
#58402=CARTESIAN_POINT('Ctrl Pts',(18.7162932509112,5.36339161345086,40.3855010275026));
#58403=CARTESIAN_POINT('Ctrl Pts',(21.2184655394692,5.48911440836994,40.4209393989282));
#58404=CARTESIAN_POINT('Ctrl Pts',(22.6102149212844,5.61483720328902,38.3412385314921));
#58405=CARTESIAN_POINT('Ctrl Pts',(21.6231999095005,5.7405599982081,36.0416900092141));
#58406=CARTESIAN_POINT('Ctrl Pts',(19.1569158471387,5.86628279312718,35.6179389460439));
#58407=CARTESIAN_POINT('Ctrl Pts',(17.4589587709116,5.99200558804625,37.4561619485894));
#58408=CARTESIAN_POINT('Ctrl Pts',(18.0767261007989,6.11772838296534,39.8811331991244));
#58409=CARTESIAN_POINT('Ctrl Pts',(20.4472285917842,6.24345117788442,40.6829062218869));
#58410=CARTESIAN_POINT('Ctrl Pts',(22.4101587249301,6.3691739728035,39.1308020590856));
#58411=CARTESIAN_POINT('Ctrl Pts',(22.1766414655508,6.49489676772258,36.6392981499235));
#58412=CARTESIAN_POINT('Ctrl Pts',(19.9594878497692,6.62061956264165,35.4789741073284));
#58413=CARTESIAN_POINT('Ctrl Pts',(17.7792541288559,6.74634235756073,36.7072668094111));
#58414=CARTESIAN_POINT('Ctrl Pts',(17.6228503854794,6.87206515247981,39.2047975717553));
#58415=CARTESIAN_POINT('Ctrl Pts',(19.6328118770762,6.99778794739889,40.6954943357201));
#58416=CARTESIAN_POINT('Ctrl Pts',(21.977402530985,7.12351074231797,39.8208420017032));
#58417=CARTESIAN_POINT('Ctrl Pts',(22.519929035247,7.24923353723705,37.3779365528634));
#58418=CARTESIAN_POINT('Ctrl Pts',(20.7659712865986,7.37495633215614,35.5930684188678));
#58419=CARTESIAN_POINT('Ctrl Pts',(18.3139617383752,7.5006791270752,36.0928395817203));
#58420=CARTESIAN_POINT('Ctrl Pts',(17.3984876494714,7.6264019219943,38.4217941180613));
#58421=CARTESIAN_POINT('Ctrl Pts',(18.8538470495971,7.75212471691336,40.4574883623582));
#58422=CARTESIAN_POINT('Ctrl Pts',(21.3537288014283,7.87784751183246,40.3447352397454));
#58423=CARTESIAN_POINT('Ctrl Pts',(22.6199183215705,8.00357030675152,38.186289933772));
#58424=CARTESIAN_POINT('Ctrl Pts',(21.4985004586309,8.12929310167061,35.9492061140465));
#58425=CARTESIAN_POINT('Ctrl Pts',(19.0114557633118,8.25501589658968,35.6722030034448));
#58426=CARTESIAN_POINT('Ctrl Pts',(17.4253000379226,8.38073869150878,37.6077215527263));
#58427=CARTESIAN_POINT('Ctrl Pts',(18.1855428960556,8.50646148642784,39.9918676968322));
#58428=CARTESIAN_POINT('Ctrl Pts',(20.599353020769,8.63218428134693,40.6519000609089));
#58429=CARTESIAN_POINT('Ctrl Pts',(22.4669553932489,8.75790707626599,38.9863120511942));
#58430=CARTESIAN_POINT('Ctrl Pts',(22.0863499257514,8.8836298711851,36.5130022206416));
#58431=CARTESIAN_POINT('Ctrl Pts',(19.8043933949771,9.00935266610415,35.4859693918313));
#58432=CARTESIAN_POINT('Ctrl Pts',(17.7006988239315,9.13507546102325,36.8411783024981));
#58433=CARTESIAN_POINT('Ctrl Pts',(17.6924239530769,9.26079825594232,39.3435878545717));
#58434=CARTESIAN_POINT('Ctrl Pts',(19.7871099116859,9.3865210508614,40.7126798071462));
#58435=CARTESIAN_POINT('Ctrl Pts',(22.0758087685058,9.51224384578049,39.7007610443055));
#58436=CARTESIAN_POINT('Ctrl Pts',(22.4727630236925,9.63796664069955,37.2300224180872));
#58437=CARTESIAN_POINT('Ctrl Pts',(20.6162167772143,9.76368943561865,35.5521195381551));
#58438=CARTESIAN_POINT('Ctrl Pts',(18.1980943492413,9.88941223053771,36.1961738550658));
#58439=CARTESIAN_POINT('Ctrl Pts',(17.4221006853397,10.0151350254568,38.5752400318213));
#58440=CARTESIAN_POINT('Ctrl Pts',(18.9954212675538,10.1408578203759,40.5212062148211));
#58441=CARTESIAN_POINT('Ctrl Pts',(21.484243519697,10.266580615295,40.2606571080598));
#58442=CARTESIAN_POINT('Ctrl Pts',(22.6204317004865,10.3923034102141,38.0310386524419));
#58443=CARTESIAN_POINT('Ctrl Pts',(21.3685446411314,10.5180262051331,35.8642666684951));
#58444=CARTESIAN_POINT('Ctrl Pts',(18.8694632466171,10.6437490000522,35.7349831684274));
#58445=CARTESIAN_POINT('Ctrl Pts',(17.4006727115538,10.7694717949713,37.7610079471273));
#58446=CARTESIAN_POINT('Ctrl Pts',(18.3007243552118,10.8951945898904,40.0959659935483));
#58447=CARTESIAN_POINT('Ctrl Pts',(20.7493750685367,11.0209173848094,40.6119424696889));
#58448=CARTESIAN_POINT('Ctrl Pts',(22.5150985960771,11.1466401797285,38.8387130812318));
#58449=CARTESIAN_POINT('Ctrl Pts',(21.9887399897083,11.2723629746476,36.3922730845633));
#58450=CARTESIAN_POINT('Ctrl Pts',(19.6499850794686,11.3980857695667,35.5021340450715));
#58451=CARTESIAN_POINT('Ctrl Pts',(17.6302088952332,11.5238085644857,36.9795054287771));
#58452=CARTESIAN_POINT('Ctrl Pts',(17.7700919230879,11.6495313594049,39.4780159407255));
#58453=CARTESIAN_POINT('Ctrl Pts',(19.9421547117366,11.7752541543239,40.7207006481087));
#58454=CARTESIAN_POINT('Ctrl Pts',(22.1669335855388,11.900976949243,39.5750650155964));
#58455=CARTESIAN_POINT('Ctrl Pts',(22.4169231749254,12.0266997441621,37.0851599481297));
#58456=CARTESIAN_POINT('Ctrl Pts',(20.4643007327528,12.1524225390811,35.5201079879311));
#58457=CARTESIAN_POINT('Ctrl Pts',(18.0885475966331,12.2781453340003,36.3061862766624));
#58458=CARTESIAN_POINT('Ctrl Pts',(17.4547563503607,12.4038681289193,38.7270189218375));
#58459=CARTESIAN_POINT('Ctrl Pts',(19.1405192976627,12.5295909238384,40.5764310785245));
#58460=CARTESIAN_POINT('Ctrl Pts',(21.6095518811291,12.6553137187575,40.1689999290297));
#58461=CARTESIAN_POINT('Ctrl Pts',(22.6117532572266,12.7810365136766,37.8760292703545));
#58462=CARTESIAN_POINT('Ctrl Pts',(21.2337883096637,12.9067593085956,35.787169618993));
#58463=CARTESIAN_POINT('Ctrl Pts',(18.7314363714608,13.0324821035147,35.8060592237987));
#58464=CARTESIAN_POINT('Ctrl Pts',(17.3851631783365,13.1582048984338,37.9154834412742));
#58465=CARTESIAN_POINT('Ctrl Pts',(18.4218664503776,13.2839276933529,40.1930629383581));
#58466=CARTESIAN_POINT('Ctrl Pts',(20.8967684950848,13.409650488272,40.5631736095118));
#58467=CARTESIAN_POINT('Ctrl Pts',(22.5544194590421,13.535373283191,38.6885228896471));
#58468=CARTESIAN_POINT('Ctrl Pts',(21.8841540487817,13.6610960781101,36.2775342294486));
#58469=CARTESIAN_POINT('Ctrl Pts',(19.4968045291821,13.7868188730292,35.5274113654686));
#58470=CARTESIAN_POINT('Ctrl Pts',(17.5680316038858,13.9125416679483,37.1217629711195));
#58471=CARTESIAN_POINT('Ctrl Pts',(17.855581855605,14.0382644628674,39.6076102899493));
#58472=CARTESIAN_POINT('Ctrl Pts',(20.097402418661,14.1639872577864,40.7195287234941));
#58473=CARTESIAN_POINT('Ctrl Pts',(22.2504573389066,14.2897100527055,39.4441948259583));
#58474=CARTESIAN_POINT('Ctrl Pts',(22.3526053612365,14.4154328476246,36.9438572844788));
#58475=CARTESIAN_POINT('Ctrl Pts',(20.3107560368861,14.5411556425437,35.4971460567465));
#58476=CARTESIAN_POINT('Ctrl Pts',(17.9857057432925,14.6668784374627,36.4224909503174));
#58477=CARTESIAN_POINT('Ctrl Pts',(17.4963400965896,14.7926012323818,38.876598385542));
#58478=CARTESIAN_POINT('Ctrl Pts',(19.2886321721494,14.9183240273009,40.6229692383917));
#58479=CARTESIAN_POINT('Ctrl Pts',(21.7292143351823,15.04404682222,40.070085213226));
#58480=CARTESIAN_POINT('Ctrl Pts',(22.5939134336097,15.1697696171391,37.72180552184));
#58481=CARTESIAN_POINT('Ctrl Pts',(21.0947041558975,15.2954924120581,35.7181854028005));
#58482=CARTESIAN_POINT('Ctrl Pts',(18.597859301766,15.4212152069772,35.8851818524476));
#58483=CARTESIAN_POINT('Ctrl Pts',(17.3788258418525,15.5469380018963,38.0706061735827));
#58484=CARTESIAN_POINT('Ctrl Pts',(18.5485442452357,15.6726607968154,40.2828179393466));
#58485=CARTESIAN_POINT('Ctrl Pts',(21.0410162809591,15.7983835917345,40.5057645494));
#58486=CARTESIAN_POINT('Ctrl Pts',(22.5847800543438,15.9241063866536,38.5362683062499));
#58487=CARTESIAN_POINT('Ctrl Pts',(21.7729589644207,16.0498291815726,36.1691881306424));
#58488=CARTESIAN_POINT('Ctrl Pts',(19.3453890633611,16.1755519764917,35.5617126864745));
#58489=CARTESIAN_POINT('Ctrl Pts',(17.5143850523512,16.3012747714108,37.2674519254743));
#58490=CARTESIAN_POINT('Ctrl Pts',(17.9485938732237,16.4269975663299,39.7319163175226));
#58491=CARTESIAN_POINT('Ctrl Pts',(20.2523084621442,16.5527203612489,40.7091681441222));
#58492=CARTESIAN_POINT('Ctrl Pts',(22.3260870480718,16.678443156168,39.3086095354431));
#58493=CARTESIAN_POINT('Ctrl Pts',(22.2800351935076,16.8041659510871,36.8066100817083));
#58494=CARTESIAN_POINT('Ctrl Pts',(20.1561212861896,16.9298887460062,35.4833142893404));
#58495=CARTESIAN_POINT('Ctrl Pts',(17.8899295328436,17.0556115409253,36.5446799081842));
#58496=CARTESIAN_POINT('Ctrl Pts',(17.5467060585947,17.1813343358443,39.0234537354066));
#58497=CARTESIAN_POINT('Ctrl Pts',(19.439240347916,17.3070571307634,40.6606574501416));
#58498=CARTESIAN_POINT('Ctrl Pts',(21.8428111357511,17.4327799256825,39.9642599288516));
#58499=CARTESIAN_POINT('Ctrl Pts',(22.5669748072978,17.5585027206016,37.5689083854212));
#58500=CARTESIAN_POINT('Ctrl Pts',(20.9517800524239,17.6842255155207,35.6575559993785));
#58501=CARTESIAN_POINT('Ctrl Pts',(18.4692005926496,17.8099483104397,35.9720735118851));
#58502=CARTESIAN_POINT('Ctrl Pts',(17.3816829318936,17.9356711053588,38.2258320121205));
#58503=CARTESIAN_POINT('Ctrl Pts',(18.6803133856264,18.0613939002779,40.3649161583056));
#58504=CARTESIAN_POINT('Ctrl Pts',(21.181612440802,18.187116695197,40.439916666057));
#58505=CARTESIAN_POINT('Ctrl Pts',(22.6060738846253,18.3128394901161,38.3824834022036));
#58506=CARTESIAN_POINT('Ctrl Pts',(21.6555447811986,18.4385622850351,36.0676148393279));
#58507=CARTESIAN_POINT('Ctrl Pts',(19.1962698099778,18.5642850799542,35.604917687523));
#58508=CARTESIAN_POINT('Ctrl Pts',(17.4694574189812,18.6900078748733,37.416061251387));
#58509=CARTESIAN_POINT('Ctrl Pts',(18.0488017137092,18.8157306697924,39.8504979885785));
#58510=CARTESIAN_POINT('Ctrl Pts',(20.4063294688456,18.9414534647115,40.6896552528342));
#58511=CARTESIAN_POINT('Ctrl Pts',(22.393557425739,19.0671762596305,39.1687847425188));
#58512=CARTESIAN_POINT('Ctrl Pts',(22.1994672242047,19.1928990545496,36.6738997707503));
#58513=CARTESIAN_POINT('Ctrl Pts',(20.0009389117691,19.3186218494687,35.4786612004172));
#58514=CARTESIAN_POINT('Ctrl Pts',(17.8015549032927,19.4443446443878,36.6723245489679));
#58515=CARTESIAN_POINT('Ctrl Pts',(17.6056776060072,19.5700674393069,39.1670698255491));
#58516=CARTESIAN_POINT('Ctrl Pts',(19.5918154497326,19.6957902342259,40.6893635397801));
#58517=CARTESIAN_POINT('Ctrl Pts',(21.9499439670764,19.821513029145,39.8518952325912));
#58518=CARTESIAN_POINT('Ctrl Pts',(22.5310315747525,19.9472358240641,37.4178742871035));
#58519=CARTESIAN_POINT('Ctrl Pts',(20.8055179179848,20.0729586189832,35.6054938860462));
#58520=CARTESIAN_POINT('Ctrl Pts',(18.3459104295828,20.1986814139022,36.066429786708));
#58521=CARTESIAN_POINT('Ctrl Pts',(17.3937265915144,20.3244042088213,38.3806157290309));
#58522=CARTESIAN_POINT('Ctrl Pts',(18.8167074628455,20.4501270037404,40.4390710379465));
#58523=CARTESIAN_POINT('Ctrl Pts',(21.318071928025,20.5758497986595,40.3658581803161));
#58524=CARTESIAN_POINT('Ctrl Pts',(22.6182105026428,20.7015725935786,38.2277129594711));
#58525=CARTESIAN_POINT('Ctrl Pts',(21.5323538864901,20.8272953884976,35.9731602960804));
#58526=CARTESIAN_POINT('Ctrl Pts',(19.0499106856773,20.9530181834167,35.6568948787136));
#58527=CARTESIAN_POINT('Ctrl Pts',(17.4335209345191,21.0787409783358,37.5670307872341));
#58528=CARTESIAN_POINT('Ctrl Pts',(18.1556317081086,21.2044637732549,39.9630146849301));
#58529=CARTESIAN_POINT('Ctrl Pts',(20.5593559198267,21.3301865681739,40.6609124994508));
#58530=CARTESIAN_POINT('Ctrl Pts',(22.4517947373209,21.455909363093,39.0254939206425));
#58531=CARTESIAN_POINT('Ctrl Pts',(22.1128295407574,21.5816321580121,36.5456425586315));
#58532=CARTESIAN_POINT('Ctrl Pts',(19.8420657823089,21.707369734299,35.4841517828753));
#58533=CARTESIAN_POINT('Ctrl Pts',(18.433464815411,21.7911997122795,36.3635933916213));
#58534=CARTESIAN_POINT('Ctrl Pts',(18.0698183975814,21.8331220919537,37.004138400054));
#58535=CARTESIAN_POINT('Ctrl Pts',(21.2977109876404,0.0420943265399541,
39.7161014880613));
#58536=CARTESIAN_POINT('Ctrl Pts',(21.8340555061094,0.0840185761245343,
39.2854503699403));
#58537=CARTESIAN_POINT('Ctrl Pts',(22.4349388060586,0.167850424015474,37.8558861542791));
#58538=CARTESIAN_POINT('Ctrl Pts',(21.1180778385984,0.293589870212774,35.9207310046821));
#58539=CARTESIAN_POINT('Ctrl Pts',(18.7815540989668,0.419312665131854,35.9777303342837));
#58540=CARTESIAN_POINT('Ctrl Pts',(17.5559152313698,0.545035460050933,37.9659119570555));
#58541=CARTESIAN_POINT('Ctrl Pts',(18.5573923750011,0.670758254970012,40.0777776761189));
#58542=CARTESIAN_POINT('Ctrl Pts',(20.8736883315835,0.796481049889092,40.3864718933352));
#58543=CARTESIAN_POINT('Ctrl Pts',(22.3937003777697,0.922203844808171,38.6118330009634));
#58544=CARTESIAN_POINT('Ctrl Pts',(21.7322982928821,1.04792663972725,36.3705421108507));
#58545=CARTESIAN_POINT('Ctrl Pts',(19.4921849462116,1.17364943464633,35.7054613985552));
#58546=CARTESIAN_POINT('Ctrl Pts',(17.7148672861923,1.29937222956541,37.2225387428673));
#58547=CARTESIAN_POINT('Ctrl Pts',(18.0200524837552,1.42509502448449,39.539299926903));
#58548=CARTESIAN_POINT('Ctrl Pts',(20.1296235817924,1.55081781940357,40.5443709850134));
#58549=CARTESIAN_POINT('Ctrl Pts',(22.1210637035315,1.67654061432265,39.3218234855224));
#58550=CARTESIAN_POINT('Ctrl Pts',(22.1795177394272,1.80226340924173,36.9857890373839));
#58551=CARTESIAN_POINT('Ctrl Pts',(20.2517138530609,1.92798620416081,35.6651692691415));
#58552=CARTESIAN_POINT('Ctrl Pts',(18.0945160206517,2.05370899907988,36.563480181515));
#58553=CARTESIAN_POINT('Ctrl Pts',(17.6738407915532,2.17943179399897,38.8620665980196));
#58554=CARTESIAN_POINT('Ctrl Pts',(19.3730618107187,2.30515458891804,40.4661593977127));
#58555=CARTESIAN_POINT('Ctrl Pts',(21.6436297207534,2.43087738383713,39.9139028058985));
#58556=CARTESIAN_POINT('Ctrl Pts',(22.416310314239,2.55660017875621,37.7085840226691));
#58557=CARTESIAN_POINT('Ctrl Pts',(20.9869373875313,2.68232297367528,35.8599739841007));
#58558=CARTESIAN_POINT('Ctrl Pts',(18.658139862288,2.80804576859437,36.0527644575676));
#58559=CARTESIAN_POINT('Ctrl Pts',(17.5522183103459,2.93376856351344,38.1112599348682));
#58560=CARTESIAN_POINT('Ctrl Pts',(18.6770310483036,3.05949135843252,40.1594939025224));
#58561=CARTESIAN_POINT('Ctrl Pts',(21.0075036762963,3.1852141533516,40.3308514807028));
#58562=CARTESIAN_POINT('Ctrl Pts',(22.4198090486167,3.31093694827068,38.4691695455411));
#58563=CARTESIAN_POINT('Ctrl Pts',(21.6268724090507,3.43665974318976,36.2710527210051));
#58564=CARTESIAN_POINT('Ctrl Pts',(19.3513198638514,3.56238253810884,35.7397084785321));
#58565=CARTESIAN_POINT('Ctrl Pts',(17.6669282985544,3.68810533302792,37.3593662031733));
#58566=CARTESIAN_POINT('Ctrl Pts',(18.1087324905111,3.813828127947,39.6539849396328));
#58567=CARTESIAN_POINT('Ctrl Pts',(20.2741034943941,3.93955092286608,40.5324122305857));
#58568=CARTESIAN_POINT('Ctrl Pts',(22.1896760516827,4.06527371778516,39.1941118652993));
#58569=CARTESIAN_POINT('Ctrl Pts',(22.1097334570229,4.19099651270424,36.8587156951692));
#58570=CARTESIAN_POINT('Ctrl Pts',(20.1071297103542,4.31671930762331,35.6545378329912));
#58571=CARTESIAN_POINT('Ctrl Pts',(18.0068955584607,4.4424421025424,36.6789804117387));
#58572=CARTESIAN_POINT('Ctrl Pts',(17.723035161693,4.56816489746147,38.9984392635119));
#58573=CARTESIAN_POINT('Ctrl Pts',(19.5142387141328,4.69388769238056,40.499124414919));
#58574=CARTESIAN_POINT('Ctrl Pts',(21.7481305836104,4.81961048729963,39.8134180598305));
#58575=CARTESIAN_POINT('Ctrl Pts',(22.3889004638811,4.94533328221871,37.5662242429861));
#58576=CARTESIAN_POINT('Ctrl Pts',(20.8525962201039,5.07105607713779,35.8054757202043));
#58577=CARTESIAN_POINT('Ctrl Pts',(18.5392963680484,5.19677887205687,36.1357935738037));
#58578=CARTESIAN_POINT('Ctrl Pts',(17.5571780064341,5.32250166697596,38.2561495848798));
#58579=CARTESIAN_POINT('Ctrl Pts',(18.8012740192805,5.44822446189503,40.2342019605124));
#58580=CARTESIAN_POINT('Ctrl Pts',(21.137803707747,5.57394725681411,40.267294328822));
#58581=CARTESIAN_POINT('Ctrl Pts',(22.4374199509555,5.6996700517332,38.325268656923));
#58582=CARTESIAN_POINT('Ctrl Pts',(21.5157448574613,5.82539284665227,36.1779491390219));
#58583=CARTESIAN_POINT('Ctrl Pts',(19.212727611906,5.95111564157135,35.7822501920932));
#58584=CARTESIAN_POINT('Ctrl Pts',(17.6271744761412,6.07683843649043,37.4987837174265));
#58585=CARTESIAN_POINT('Ctrl Pts',(18.2040459063968,6.2025612314095,39.7632230393958));
#58586=CARTESIAN_POINT('Ctrl Pts',(20.4176222744586,6.32828402632859,40.5119190743023));
#58587=CARTESIAN_POINT('Ctrl Pts',(22.2506073784236,6.45400682124767,39.0625634593587));
#58588=CARTESIAN_POINT('Ctrl Pts',(22.0325488491192,6.57972961616675,36.7359959087116));
#58589=CARTESIAN_POINT('Ctrl Pts',(19.9621697345979,6.70545241108583,35.652484758755));
#58590=CARTESIAN_POINT('Ctrl Pts',(17.9262664356906,6.8311752060049,36.7994650756846));
#58591=CARTESIAN_POINT('Ctrl Pts',(17.7802165447788,6.95689800092399,39.1316605047367));
#58592=CARTESIAN_POINT('Ctrl Pts',(19.6571195539224,7.08262079584305,40.5236738610639));
#58593=CARTESIAN_POINT('Ctrl Pts',(21.8464994360391,7.20834359076215,39.7069230901989));
#58594=CARTESIAN_POINT('Ctrl Pts',(22.3531109470789,7.33406638568122,37.4257368052129));
#58595=CARTESIAN_POINT('Ctrl Pts',(20.7152643564292,7.45978918060031,35.759026081835));
#58596=CARTESIAN_POINT('Ctrl Pts',(18.4255766590528,7.58551197551937,36.2257126344692));
#58597=CARTESIAN_POINT('Ctrl Pts',(17.5707065138088,7.71123477043847,38.4004915024686));
#58598=CARTESIAN_POINT('Ctrl Pts',(18.9297218227593,7.83695756535754,40.3014237684802));
#58599=CARTESIAN_POINT('Ctrl Pts',(21.2641126069269,7.96268036027662,40.1961348482662));
#58600=CARTESIAN_POINT('Ctrl Pts',(22.4464809908173,8.0884031551957,38.180577581726));
#58601=CARTESIAN_POINT('Ctrl Pts',(21.3993004501658,8.21412595011479,36.0915876331608));
#58602=CARTESIAN_POINT('Ctrl Pts',(19.0768969155535,8.33984874503385,35.8329219950357));
#58603=CARTESIAN_POINT('Ctrl Pts',(17.5957439350612,8.46557153995296,37.6403101487827));
#58604=CARTESIAN_POINT('Ctrl Pts',(18.3056590822296,8.59129433487201,39.8666269667012));
#58605=CARTESIAN_POINT('Ctrl Pts',(20.5596761395299,8.7170171297911,40.4829655062439));
#58606=CARTESIAN_POINT('Ctrl Pts',(22.3036441346612,8.84273992471017,38.9276386203823));
#58607=CARTESIAN_POINT('Ctrl Pts',(21.9482345657571,8.96846271962927,36.6180607091055));
#58608=CARTESIAN_POINT('Ctrl Pts',(19.817342457997,9.09418551454833,35.6590169587937));
#58609=CARTESIAN_POINT('Ctrl Pts',(17.8529114541085,9.21990830946742,36.9245116924406));
#58610=CARTESIAN_POINT('Ctrl Pts',(17.8451843757182,9.34563110438649,39.2612629376924));
#58611=CARTESIAN_POINT('Ctrl Pts',(19.8012031329734,9.47135389930557,40.5397216625606));
#58612=CARTESIAN_POINT('Ctrl Pts',(21.9383912280429,9.59707669422467,39.5947914343325));
#58613=CARTESIAN_POINT('Ctrl Pts',(22.3090673027673,9.72279948914372,37.2876145149019));
#58614=CARTESIAN_POINT('Ctrl Pts',(20.5754235234226,9.84852228406283,35.7207879972984));
#58615=CARTESIAN_POINT('Ctrl Pts',(18.3173796352609,9.97424507898189,36.3222062287001));
#58616=CARTESIAN_POINT('Ctrl Pts',(17.592756378078,10.099967873901,38.5437793706595));
#58617=CARTESIAN_POINT('Ctrl Pts',(19.0619238956901,10.2256906688201,40.3609235298059));
#58618=CARTESIAN_POINT('Ctrl Pts',(21.3859873137211,10.3514134637392,40.1176226483937));
#58619=CARTESIAN_POINT('Ctrl Pts',(22.4469603842963,10.4771362586582,38.0356038604284));
#58620=CARTESIAN_POINT('Ctrl Pts',(21.2779476451792,10.6028590535773,36.0122711379855));
#58621=CARTESIAN_POINT('Ctrl Pts',(18.9443042350597,10.7285818484964,35.8915461433405));
#58622=CARTESIAN_POINT('Ctrl Pts',(17.572746925834,10.8543046434155,37.7834490577195));
#58623=CARTESIAN_POINT('Ctrl Pts',(18.4132155842779,10.9800274383345,39.9638340063237));
#58624=CARTESIAN_POINT('Ctrl Pts',(20.6997668000079,11.1057502332536,40.4456530883133));
#58625=CARTESIAN_POINT('Ctrl Pts',(22.348600280655,11.2314730281727,38.7898106311262));
#58626=CARTESIAN_POINT('Ctrl Pts',(21.8570863604567,11.3571958230918,36.505323783675));
#58627=CARTESIAN_POINT('Ctrl Pts',(19.6731558985896,11.4829186180109,35.6741115197767));
#58628=CARTESIAN_POINT('Ctrl Pts',(17.7870879247318,11.6086414129299,37.0536816295986));
#58629=CARTESIAN_POINT('Ctrl Pts',(17.9177107635305,11.734364207849,39.3867919493028));
#58630=CARTESIAN_POINT('Ctrl Pts',(19.9459840419529,11.8600870027681,40.5472115277155));
#58631=CARTESIAN_POINT('Ctrl Pts',(22.0234836260872,11.9858097976872,39.4774164221702));
#58632=CARTESIAN_POINT('Ctrl Pts',(22.256924025088,12.1115325926063,37.1523418706686));
#58633=CARTESIAN_POINT('Ctrl Pts',(20.4335642479196,12.2372553875253,35.6908955962779));
#58634=CARTESIAN_POINT('Ctrl Pts',(18.2150848249019,12.3629781824444,36.4249358809851));
#58635=CARTESIAN_POINT('Ctrl Pts',(17.6232502538064,12.4887009773635,38.6855105712756));
#58636=CARTESIAN_POINT('Ctrl Pts',(19.1974165061062,12.6144237722826,40.4124925341364));
#58637=CARTESIAN_POINT('Ctrl Pts',(21.5030003219933,12.7401465672016,40.03203313046));
#58638=CARTESIAN_POINT('Ctrl Pts',(22.4388564497993,12.8658693621208,37.8908560247601));
#58639=CARTESIAN_POINT('Ctrl Pts',(21.1521121179363,12.9915921570398,35.9402778760194));
#58640=CARTESIAN_POINT('Ctrl Pts',(18.815414672545,13.1173149519589,35.9579169980868));
#58641=CARTESIAN_POINT('Ctrl Pts',(17.5582641162439,13.243037746878,37.9276983485718));
#58642=CARTESIAN_POINT('Ctrl Pts',(18.5263381311034,13.3687605417971,40.054503180163));
#58643=CARTESIAN_POINT('Ctrl Pts',(20.8374028527246,13.4944833367161,40.4001127031856));
#58644=CARTESIAN_POINT('Ctrl Pts',(22.3853181214344,13.6202061316352,38.649562957871));
#58645=CARTESIAN_POINT('Ctrl Pts',(21.7594239584356,13.7459289265543,36.3981805854939));
#58646=CARTESIAN_POINT('Ctrl Pts',(19.530115826938,13.8716517214733,35.6977154937408));
#58647=CARTESIAN_POINT('Ctrl Pts',(17.729026740118,13.9973745163925,37.1865217911697));
#58648=CARTESIAN_POINT('Ctrl Pts',(17.9975413036994,14.1230973113115,39.5078072150396));
#58649=CARTESIAN_POINT('Ctrl Pts',(20.0909544254689,14.2488201062306,40.5461171839458));
#58650=CARTESIAN_POINT('Ctrl Pts',(22.1014781472193,14.3745429011497,39.3552097760401));
#58651=CARTESIAN_POINT('Ctrl Pts',(22.1968640196805,14.5002656960688,37.0203933752795));
#58652=CARTESIAN_POINT('Ctrl Pts',(20.2901841369496,14.6259884909878,35.6694537338759));
#58653=CARTESIAN_POINT('Ctrl Pts',(18.1190510527088,14.7517112859069,36.5335412412735));
#58654=CARTESIAN_POINT('Ctrl Pts',(17.6620811760677,14.877434080826,38.8251879465421));
#58655=CARTESIAN_POINT('Ctrl Pts',(19.3357243796546,15.0031568757451,40.45594989024));
#58656=CARTESIAN_POINT('Ctrl Pts',(21.614741179235,15.1288796706642,39.9396665211908));
#58657=CARTESIAN_POINT('Ctrl Pts',(22.4221976139118,15.2546024655832,37.7468418141005));
#58658=CARTESIAN_POINT('Ctrl Pts',(21.0222352681462,15.3803252605023,35.8758603817059));
#58659=CARTESIAN_POINT('Ctrl Pts',(18.6906803405137,15.5060480554214,36.0318017468361));
#58660=CARTESIAN_POINT('Ctrl Pts',(17.5523463083822,15.6317708503405,38.0725520307311));
#58661=CARTESIAN_POINT('Ctrl Pts',(18.6446299169683,15.7574936452595,40.1383164433252));
#58662=CARTESIAN_POINT('Ctrl Pts',(20.9721015046648,15.8832164401786,40.3465040951967));
#58663=CARTESIAN_POINT('Ctrl Pts',(22.4136688599532,16.0089392350977,38.5073875545465));
#58664=CARTESIAN_POINT('Ctrl Pts',(21.6555899350916,16.1346620300168,36.2970069462334));
#58665=CARTESIAN_POINT('Ctrl Pts',(19.3887239920105,16.2603848249359,35.7297460838206));
#58666=CARTESIAN_POINT('Ctrl Pts',(17.678931564451,16.3861076198549,37.3225662069312));
#58667=CARTESIAN_POINT('Ctrl Pts',(18.08439597056,16.511830414774,39.6238842434713));
#58668=CARTESIAN_POINT('Ctrl Pts',(20.2356057634987,16.6375532096931,40.5364424699371));
#58669=CARTESIAN_POINT('Ctrl Pts',(22.1721012060722,16.7632760046122,39.2286001664393));
#58670=CARTESIAN_POINT('Ctrl Pts',(22.1290979620948,16.8889987995313,36.8922318712142));
#58671=CARTESIAN_POINT('Ctrl Pts',(20.1457861322546,17.0147215944504,35.6565376228087));
#58672=CARTESIAN_POINT('Ctrl Pts',(18.0296151812518,17.1404443893694,36.6476413489935));
#58673=CARTESIAN_POINT('Ctrl Pts',(17.7091129356516,17.2661671842885,38.9623215429927));
#58674=CARTESIAN_POINT('Ctrl Pts',(19.4763623667403,17.3918899792076,40.4911431605282));
#58675=CARTESIAN_POINT('Ctrl Pts',(21.720817926331,17.5176127741267,39.840846819661));
#58676=CARTESIAN_POINT('Ctrl Pts',(22.397042311684,17.6433355690457,37.6040663944551));
#58677=CARTESIAN_POINT('Ctrl Pts',(20.8887726714696,17.7690583639648,35.8192446155825));
#58678=CARTESIAN_POINT('Ctrl Pts',(18.57053877596,17.8947811588839,36.1129412202786));
#58679=CARTESIAN_POINT('Ctrl Pts',(17.555014260439,18.020503953803,38.2175019935372));
#58680=CARTESIAN_POINT('Ctrl Pts',(18.7676760037445,18.1462267487221,40.2149797997396));
#58681=CARTESIAN_POINT('Ctrl Pts',(21.1033902664578,18.2719495436411,40.2850153100092));
#58682=CARTESIAN_POINT('Ctrl Pts',(22.4335530489282,18.3976723385602,38.3637831370628));
#58683=CARTESIAN_POINT('Ctrl Pts',(21.5459485142351,18.5233951334793,36.2021577578715));
#58684=CARTESIAN_POINT('Ctrl Pts',(19.2494763613636,18.6491179283984,35.7700909346134));
#58685=CARTESIAN_POINT('Ctrl Pts',(17.6369781187664,18.7748407233175,37.4613376670606));
#58686=CARTESIAN_POINT('Ctrl Pts',(18.1779701002801,18.9005635182365,39.7346158650296));
#58687=CARTESIAN_POINT('Ctrl Pts',(20.3794306537555,19.0262863131556,40.5182213226522));
#58688=CARTESIAN_POINT('Ctrl Pts',(22.2351050772414,19.1520091080747,39.0980317074466));
#58689=CARTESIAN_POINT('Ctrl Pts',(22.0538635535465,19.2777319029938,36.7683069189088));
#58690=CARTESIAN_POINT('Ctrl Pts',(20.0008767562623,19.4034546979128,35.6521925661306));
#58691=CARTESIAN_POINT('Ctrl Pts',(17.947090909603,19.529177492832,36.7668359760495));
#58692=CARTESIAN_POINT('Ctrl Pts',(17.7641805950347,19.654900287751,39.0964303171541));
#58693=CARTESIAN_POINT('Ctrl Pts',(19.6188370703191,19.7806230826701,40.5179489208616));
#58694=CARTESIAN_POINT('Ctrl Pts',(21.8208586158333,19.9063458775892,39.7359206121618));
#58695=CARTESIAN_POINT('Ctrl Pts',(22.3634785038178,20.0320686725083,37.4630306806861));
#58696=CARTESIAN_POINT('Ctrl Pts',(20.7521930198691,20.1577914674273,35.770628989072));
#58697=CARTESIAN_POINT('Ctrl Pts',(18.4554103622938,20.2835142623465,36.2010511551641));
#58698=CARTESIAN_POINT('Ctrl Pts',(17.5662606355948,20.4092370572655,38.3620391029544));
#58699=CARTESIAN_POINT('Ctrl Pts',(18.8950408587589,20.5349598521846,40.2842256620722));
#58700=CARTESIAN_POINT('Ctrl Pts',(21.2308162013654,20.6606826471036,40.215859460347));
#58701=CARTESIAN_POINT('Ctrl Pts',(22.4448862286797,20.7864054420227,38.2192584230794));
#58702=CARTESIAN_POINT('Ctrl Pts',(21.4309127974096,20.9121282369418,36.1139560598838));
#58703=CARTESIAN_POINT('Ctrl Pts',(19.1128061405839,21.0378510318609,35.8186272607871));
#58704=CARTESIAN_POINT('Ctrl Pts',(17.6034206122633,21.16357382678,37.6023130923634));
#58705=CARTESIAN_POINT('Ctrl Pts',(18.277728000515,21.2892966216991,39.8396840102872));
#58706=CARTESIAN_POINT('Ctrl Pts',(20.5223268274015,21.4150194166181,40.4913813256959));
#58707=CARTESIAN_POINT('Ctrl Pts',(22.2894871068521,21.5407422115372,38.9642266689488));
#58708=CARTESIAN_POINT('Ctrl Pts',(21.972961243006,21.6664650064563,36.6485402724449));
#58709=CARTESIAN_POINT('Ctrl Pts',(19.8525209514359,21.7922025827432,35.6573196746751));
#58710=CARTESIAN_POINT('Ctrl Pts',(18.537168689959,21.8760325607237,36.4785426725894));
#58711=CARTESIAN_POINT('Ctrl Pts',(18.1975954898047,21.9179549403979,37.0766839100436));
#58712=CARTESIAN_POINT('Ctrl Pts',(21.2057129175019,0.126927174984125,39.6015318963221));
#58713=CARTESIAN_POINT('Ctrl Pts',(21.7040345933669,0.168851424568706,39.2014107437692));
#58714=CARTESIAN_POINT('Ctrl Pts',(22.2623197304739,0.252683272459645,37.8731920127594));
#58715=CARTESIAN_POINT('Ctrl Pts',(21.0388144244828,0.378422718656945,36.0752249896998));
#58716=CARTESIAN_POINT('Ctrl Pts',(18.8679328632146,0.504145513576025,36.1281834902012));
#58717=CARTESIAN_POINT('Ctrl Pts',(17.7291826877682,0.629868308495104,37.9754178033472));
#58718=CARTESIAN_POINT('Ctrl Pts',(18.6596625404933,0.755591103414184,39.9375679290345));
#58719=CARTESIAN_POINT('Ctrl Pts',(20.8117503182865,0.881313898333262,40.2243780191089));
#58720=CARTESIAN_POINT('Ctrl Pts',(22.2240048004479,1.00703669325235,38.5755478428887));
#58721=CARTESIAN_POINT('Ctrl Pts',(21.6094912107451,1.13275948817143,36.4931478294605));
#58722=CARTESIAN_POINT('Ctrl Pts',(19.5281852616754,1.2584822830905,35.8752163997095));
#58723=CARTESIAN_POINT('Ctrl Pts',(17.876866222537,1.38420507800959,37.2847442285619));
#58724=CARTESIAN_POINT('Ctrl Pts',(18.160416056388,1.50992787292866,39.4372642526377));
#58725=CARTESIAN_POINT('Ctrl Pts',(20.1204342326361,1.63565066784774,40.3710832379994));
#58726=CARTESIAN_POINT('Ctrl Pts',(21.9706960413755,1.76137346276682,39.2352052756217));
#58727=CARTESIAN_POINT('Ctrl Pts',(22.0250061202997,1.8870962576859,37.064778318714));
#58728=CARTESIAN_POINT('Ctrl Pts',(20.23386921051,2.01281905260498,35.8377806829972));
#58729=CARTESIAN_POINT('Ctrl Pts',(18.2296006816042,2.13854184752406,36.6724080239824));
#58730=CARTESIAN_POINT('Ctrl Pts',(17.8387482016392,2.26426464244315,38.8080417365501));
#58731=CARTESIAN_POINT('Ctrl Pts',(19.4175070716892,2.38998743736221,40.2984162713134));
#58732=CARTESIAN_POINT('Ctrl Pts',(21.5271085817852,2.5157102322813,39.7853105699147));
#58733=CARTESIAN_POINT('Ctrl Pts',(22.2450118603592,2.64143302720037,37.7363325081784));
#58734=CARTESIAN_POINT('Ctrl Pts',(20.9169708573369,2.76715582211946,36.0187751905983));
#58735=CARTESIAN_POINT('Ctrl Pts',(18.7532677792441,2.89287861703854,36.1978982514681));
#58736=CARTESIAN_POINT('Ctrl Pts',(17.7257478509857,3.01860141195762,38.1104616891203));
#58737=CARTESIAN_POINT('Ctrl Pts',(18.7708197204874,3.1443242068767,40.0134910819418));
#58738=CARTESIAN_POINT('Ctrl Pts',(20.9360791489867,3.27004700179578,40.1727006806057));
#58739=CARTESIAN_POINT('Ctrl Pts',(22.2482625604568,3.39576979671486,38.442998166808));
#58740=CARTESIAN_POINT('Ctrl Pts',(21.5115392390155,3.52149259163393,36.400711498387));
#58741=CARTESIAN_POINT('Ctrl Pts',(19.3973064673642,3.64721538655302,35.90703561609));
#58742=CARTESIAN_POINT('Ctrl Pts',(17.8323257530507,3.77293818147209,37.4118716382326));
#58743=CARTESIAN_POINT('Ctrl Pts',(18.2428093093449,3.89866097639118,39.5438189498));
#58744=CARTESIAN_POINT('Ctrl Pts',(20.2546715925742,4.02438377131025,40.3599722704356));
#58745=CARTESIAN_POINT('Ctrl Pts',(22.0344442836683,4.15010656622933,39.1165474606809));
#58746=CARTESIAN_POINT('Ctrl Pts',(21.9601690251878,4.27582936114841,36.9467135326116));
#58747=CARTESIAN_POINT('Ctrl Pts',(20.0995350096073,4.40155215606749,35.8279029367039));
#58748=CARTESIAN_POINT('Ctrl Pts',(18.1481918593724,4.52727495098657,36.7797201457734));
#58749=CARTESIAN_POINT('Ctrl Pts',(17.8844550563323,4.65299774590565,38.9347465929813));
#58750=CARTESIAN_POINT('Ctrl Pts',(19.5486755812576,4.77872054082473,40.329044313651));
#58751=CARTESIAN_POINT('Ctrl Pts',(21.6242011096567,4.90444333574381,39.6919494459819));
#58752=CARTESIAN_POINT('Ctrl Pts',(22.2195451648021,5.03016613066288,37.6040649794827));
#58753=CARTESIAN_POINT('Ctrl Pts',(20.7921534808469,5.15588892558196,35.9681404488207));
#58754=CARTESIAN_POINT('Ctrl Pts',(18.6428494060235,5.28161172050103,36.2750412200706));
#58755=CARTESIAN_POINT('Ctrl Pts',(17.7303559414599,5.40733451542013,38.2450797391293));
#58756=CARTESIAN_POINT('Ctrl Pts',(18.8862547876498,5.53305731033921,40.0829028935224));
#58757=CARTESIAN_POINT('Ctrl Pts',(21.0571418760249,5.65878010525829,40.1136492587158));
#58758=CARTESIAN_POINT('Ctrl Pts',(22.2646249806265,5.78450290017737,38.3092987823539));
#58759=CARTESIAN_POINT('Ctrl Pts',(21.4082898054222,5.91022569509645,36.3142082688297));
#58760=CARTESIAN_POINT('Ctrl Pts',(19.2685393766731,6.03594849001553,35.9465614381426));
#58761=CARTESIAN_POINT('Ctrl Pts',(17.7953901813709,6.1616712849346,37.5414054862636));
#58762=CARTESIAN_POINT('Ctrl Pts',(18.3313657119948,6.28739407985369,39.6453128796672));
#58763=CARTESIAN_POINT('Ctrl Pts',(20.3880159571329,6.41311687477276,40.3409319267177));
#58764=CARTESIAN_POINT('Ctrl Pts',(22.0910560319171,6.53883966969183,38.9943248596318));
#58765=CARTESIAN_POINT('Ctrl Pts',(21.8884562326876,6.66456246461093,36.8326936674997));
#58766=CARTESIAN_POINT('Ctrl Pts',(19.9648516194267,6.79028525952999,35.8259954101816));
#58767=CARTESIAN_POINT('Ctrl Pts',(18.0732787425253,6.91600805444907,36.8916633419583));
#58768=CARTESIAN_POINT('Ctrl Pts',(17.9375827040782,7.04173084936815,39.058523437718));
#58769=CARTESIAN_POINT('Ctrl Pts',(19.6814272307687,7.16745364428724,40.3518533864079));
#58770=CARTESIAN_POINT('Ctrl Pts',(21.7155963410933,7.29317643920632,39.5930041786945));
#58771=CARTESIAN_POINT('Ctrl Pts',(22.1862928589108,7.41889923412539,37.4735370575624));
#58772=CARTESIAN_POINT('Ctrl Pts',(20.6645574262598,7.54462202904449,35.9249837448021));
#58773=CARTESIAN_POINT('Ctrl Pts',(18.5371915797305,7.67034482396355,36.3585856872182));
#58774=CARTESIAN_POINT('Ctrl Pts',(17.742925378146,7.79606761888264,38.3791888868759));
#58775=CARTESIAN_POINT('Ctrl Pts',(19.0055965959216,7.92179041380171,40.1453591746023));
#58776=CARTESIAN_POINT('Ctrl Pts',(21.1744964124255,8.0475132087208,40.0475344567868));
#58777=CARTESIAN_POINT('Ctrl Pts',(22.273043660064,8.17323600363987,38.1748652296802));
#58778=CARTESIAN_POINT('Ctrl Pts',(21.3001004417008,8.29895879855895,36.2339691522749));
#58779=CARTESIAN_POINT('Ctrl Pts',(19.1423380677952,8.42468159347804,35.9936409866267));
#58780=CARTESIAN_POINT('Ctrl Pts',(17.7661878321998,8.55040438839711,37.6728987448391));
#58781=CARTESIAN_POINT('Ctrl Pts',(18.4257752684035,8.6761271833162,39.7413862365702));
#58782=CARTESIAN_POINT('Ctrl Pts',(20.5199992582908,8.80184997823527,40.3140309515788));
#58783=CARTESIAN_POINT('Ctrl Pts',(22.1403328760735,8.92757277315435,38.8689651895704));
#58784=CARTESIAN_POINT('Ctrl Pts',(21.8101192057626,9.05329556807344,36.7231191975695));
#58785=CARTESIAN_POINT('Ctrl Pts',(19.8302915210169,9.1790183629925,35.8320645257562));
#58786=CARTESIAN_POINT('Ctrl Pts',(18.0051240842855,9.30474115791159,37.0078450823832));
#58787=CARTESIAN_POINT('Ctrl Pts',(17.9979447983593,9.43046395283067,39.1789380208129));
#58788=CARTESIAN_POINT('Ctrl Pts',(19.8152963542609,9.55618674774975,40.3667635179752));
#58789=CARTESIAN_POINT('Ctrl Pts',(21.80097368758,9.68190954266882,39.4888218243594));
#58790=CARTESIAN_POINT('Ctrl Pts',(22.1453715818421,9.8076323375879,37.3452066117164));
#58791=CARTESIAN_POINT('Ctrl Pts',(20.5346302696308,9.93335513250699,35.8894564564418));
#58792=CARTESIAN_POINT('Ctrl Pts',(18.4366649212808,10.0590779274261,36.4482386023345));
#58793=CARTESIAN_POINT('Ctrl Pts',(17.7634120708163,10.1848007223452,38.5123187094979));
#58794=CARTESIAN_POINT('Ctrl Pts',(19.1284265238265,10.3105235172642,40.2006408447907));
#58795=CARTESIAN_POINT('Ctrl Pts',(21.2877311077452,10.4362463121833,39.9745881887277));
#58796=CARTESIAN_POINT('Ctrl Pts',(22.2734890681061,10.5619691071024,38.0401690684149));
#58797=CARTESIAN_POINT('Ctrl Pts',(21.187350649227,10.6876919020215,36.1602756074759));
#58798=CARTESIAN_POINT('Ctrl Pts',(19.0191452235023,10.8134146969406,36.0481091182536));
#58799=CARTESIAN_POINT('Ctrl Pts',(17.744821140114,10.9391374918596,37.8058901683115));
#58800=CARTESIAN_POINT('Ctrl Pts',(18.5257068133439,11.0648602867787,39.8317020190991));
#58801=CARTESIAN_POINT('Ctrl Pts',(20.650158531479,11.1905830816978,40.2793637069377));
#58802=CARTESIAN_POINT('Ctrl Pts',(22.1821019652329,11.3163058766169,38.7409081810206));
#58803=CARTESIAN_POINT('Ctrl Pts',(21.7254327312052,11.442028671536,36.6183744827865));
#58804=CARTESIAN_POINT('Ctrl Pts',(19.6963267177105,11.567751466455,35.8460889944819));
#58805=CARTESIAN_POINT('Ctrl Pts',(17.9439669542304,11.6934742613741,37.1278578304199));
#58806=CARTESIAN_POINT('Ctrl Pts',(18.0653296039732,11.8191970562932,39.2955679578802));
#58807=CARTESIAN_POINT('Ctrl Pts',(19.9498133721693,11.9449198512123,40.3737224073222));
#58808=CARTESIAN_POINT('Ctrl Pts',(21.8800336666357,12.0706426461313,39.3797678287443));
#58809=CARTESIAN_POINT('Ctrl Pts',(22.0969248752505,12.1963654410504,37.2195237932074));
#58810=CARTESIAN_POINT('Ctrl Pts',(20.4028277630863,12.3220882359695,35.8616832046247));
#58811=CARTESIAN_POINT('Ctrl Pts',(18.3416220531705,12.4478110308886,36.5436854853077));
#58812=CARTESIAN_POINT('Ctrl Pts',(17.791744157252,12.5735338258077,38.6440022207137));
#58813=CARTESIAN_POINT('Ctrl Pts',(19.2543137145497,12.6992566207267,40.2485539897483));
#58814=CARTESIAN_POINT('Ctrl Pts',(21.3964487628574,12.8249794156458,39.8950663318903));
#58815=CARTESIAN_POINT('Ctrl Pts',(22.2659596423722,12.9507022105649,37.9056827791656));
#58816=CARTESIAN_POINT('Ctrl Pts',(21.070435926209,13.076425005484,36.0933861330457));
#58817=CARTESIAN_POINT('Ctrl Pts',(18.899392973629,13.2021478004031,36.1097747723749));
#58818=CARTESIAN_POINT('Ctrl Pts',(17.7313650541513,13.3278705953222,37.9399132558693));
#58819=CARTESIAN_POINT('Ctrl Pts',(18.6308098118291,13.4535933902412,39.915943421968));
#58820=CARTESIAN_POINT('Ctrl Pts',(20.7780372103644,13.5793161851603,40.2370517968595));
#58821=CARTESIAN_POINT('Ctrl Pts',(22.2162167838267,13.7050389800794,38.6106030260947));
#58822=CARTESIAN_POINT('Ctrl Pts',(21.6346938680896,13.8307617749985,36.5188269415392));
#58823=CARTESIAN_POINT('Ctrl Pts',(19.5634271246938,13.9564845699175,35.868019622013));
#58824=CARTESIAN_POINT('Ctrl Pts',(17.8900218763501,14.0822073648366,37.2512806112199));
#58825=CARTESIAN_POINT('Ctrl Pts',(18.1395007517939,14.2079301597557,39.4080041401299));
#58826=CARTESIAN_POINT('Ctrl Pts',(20.0845064322766,14.3336529546748,40.3727056443974));
#58827=CARTESIAN_POINT('Ctrl Pts',(21.9524989555321,14.4593757495939,39.266224726122));
#58828=CARTESIAN_POINT('Ctrl Pts',(22.0411226781244,14.5850985445129,37.09692946608));
#58829=CARTESIAN_POINT('Ctrl Pts',(20.2696122370133,14.710821339432,35.8417614110053));
#58830=CARTESIAN_POINT('Ctrl Pts',(18.252396362125,14.8365441343511,36.6445915322294));
#58831=CARTESIAN_POINT('Ctrl Pts',(17.8278222555458,14.9622669292702,38.7737775075423));
#58832=CARTESIAN_POINT('Ctrl Pts',(19.3828165871599,15.0879897241893,40.2889305420883));
#58833=CARTESIAN_POINT('Ctrl Pts',(21.5002680232876,15.2137125191083,39.8092478291555));
#58834=CARTESIAN_POINT('Ctrl Pts',(22.2504817942136,15.3394353140274,37.771878106361));
#58835=CARTESIAN_POINT('Ctrl Pts',(20.949766380395,15.4651581089465,36.0335353606114));
#58836=CARTESIAN_POINT('Ctrl Pts',(18.7835013792615,15.5908809038656,36.1784216412247));
#58837=CARTESIAN_POINT('Ctrl Pts',(17.7258667749119,15.7166036987847,38.0744978878796));
#58838=CARTESIAN_POINT('Ctrl Pts',(18.740715588701,15.8423264937037,39.9938149473038));
#58839=CARTESIAN_POINT('Ctrl Pts',(20.9031867283705,15.9680492886228,40.1872436409934));
#58840=CARTESIAN_POINT('Ctrl Pts',(22.2425576655626,16.0937720835419,38.4785068028433));
#58841=CARTESIAN_POINT('Ctrl Pts',(21.5382209057625,16.219494878461,36.4248257618243));
#58842=CARTESIAN_POINT('Ctrl Pts',(19.43205892066,16.34521767338,35.8977794811667));
#58843=CARTESIAN_POINT('Ctrl Pts',(17.8434780765507,16.4709404682991,37.3776804883882));
#58844=CARTESIAN_POINT('Ctrl Pts',(18.2201980678962,16.5966632632182,39.5158521694202));
#58845=CARTESIAN_POINT('Ctrl Pts',(20.2189030648533,16.7223860581373,40.363716795752));
#58846=CARTESIAN_POINT('Ctrl Pts',(22.0181153640725,16.8481088530564,39.1485907974356));
#58847=CARTESIAN_POINT('Ctrl Pts',(21.9781607306821,16.9738316479754,36.9778536607199));
#58848=CARTESIAN_POINT('Ctrl Pts',(20.1354509783197,17.0995544428945,35.829760956277));
#58849=CARTESIAN_POINT('Ctrl Pts',(18.1693008296599,17.2252772378136,36.7506027898027));
#58850=CARTESIAN_POINT('Ctrl Pts',(17.8715198127086,17.3510000327327,38.9011893505787));
#58851=CARTESIAN_POINT('Ctrl Pts',(19.5134843855647,17.4767228276518,40.3216288709148));
#58852=CARTESIAN_POINT('Ctrl Pts',(21.5988247169108,17.6024456225708,39.7174337104706));
#58853=CARTESIAN_POINT('Ctrl Pts',(22.2271098160703,17.7281684174899,37.6392244034891));
#58854=CARTESIAN_POINT('Ctrl Pts',(20.8257652905152,17.853891212409,35.9809332317864));
#58855=CARTESIAN_POINT('Ctrl Pts',(18.6718769592704,17.9796140073281,36.2538089286721));
#58856=CARTESIAN_POINT('Ctrl Pts',(17.7283455889843,18.1053368022472,38.2091719749538));
#58857=CARTESIAN_POINT('Ctrl Pts',(18.8550386218625,18.2310595971662,40.0650434411737));
#58858=CARTESIAN_POINT('Ctrl Pts',(21.0251680921135,18.3567823920853,40.1301139539612));
#58859=CARTESIAN_POINT('Ctrl Pts',(22.2610322132312,18.4825051870044,38.3450828719222));
#58860=CARTESIAN_POINT('Ctrl Pts',(21.4363522472715,18.6082279819235,36.3367006764149));
#58861=CARTESIAN_POINT('Ctrl Pts',(19.3026829127495,18.7339507768426,35.9352641817039));
#58862=CARTESIAN_POINT('Ctrl Pts',(17.8044988185514,18.8596735717616,37.5066140827342));
#58863=CARTESIAN_POINT('Ctrl Pts',(18.3071384868509,18.9853963666807,39.6187337414808));
#58864=CARTESIAN_POINT('Ctrl Pts',(20.3525318386655,19.1111191615998,40.3467873924701));
#58865=CARTESIAN_POINT('Ctrl Pts',(22.0766527287437,19.2368419565189,39.0272786723744));
#58866=CARTESIAN_POINT('Ctrl Pts',(21.9082598828883,19.362564751438,36.8627140670674));
#58867=CARTESIAN_POINT('Ctrl Pts',(20.0008146007556,19.488287546357,35.825723931844));
#58868=CARTESIAN_POINT('Ctrl Pts',(18.0926269159133,19.6140103412761,36.8613474031311));
#58869=CARTESIAN_POINT('Ctrl Pts',(17.9226835840622,19.7397331361952,39.0257908087591));
#58870=CARTESIAN_POINT('Ctrl Pts',(19.6458586909056,19.8654559311143,40.3465343019432));
#58871=CARTESIAN_POINT('Ctrl Pts',(21.6917732645902,19.9911787260334,39.6199459917325));
#58872=CARTESIAN_POINT('Ctrl Pts',(22.195925432883,20.1169015209524,37.5081870742687));
#58873=CARTESIAN_POINT('Ctrl Pts',(20.6988681217534,20.2426243158715,35.9357640920978));
#58874=CARTESIAN_POINT('Ctrl Pts',(18.5649102950046,20.3683471107906,36.33567252362));
#58875=CARTESIAN_POINT('Ctrl Pts',(17.7387946796753,20.4940699057097,38.3434624768781));
#58876=CARTESIAN_POINT('Ctrl Pts',(18.9733742546723,20.6197927006287,40.1293802861978));
#58877=CARTESIAN_POINT('Ctrl Pts',(21.1435604747057,20.7455154955478,40.0658607403778));
#58878=CARTESIAN_POINT('Ctrl Pts',(22.2715619547167,20.8712382904669,38.2108038866874));
#58879=CARTESIAN_POINT('Ctrl Pts',(21.329471708329,20.996961085386,36.2547518236871));
#58880=CARTESIAN_POINT('Ctrl Pts',(19.1757015954905,21.1226838803051,35.9803596428606));
#58881=CARTESIAN_POINT('Ctrl Pts',(17.7733202900077,21.2484066752241,37.6375953974928));
#58882=CARTESIAN_POINT('Ctrl Pts',(18.3998242929215,21.3741294701433,39.7163533356445));
#58883=CARTESIAN_POINT('Ctrl Pts',(20.4852977349763,21.4998522650623,40.3218501519411));
#58884=CARTESIAN_POINT('Ctrl Pts',(22.1271794763833,21.6255750599814,38.9029594172551));
#58885=CARTESIAN_POINT('Ctrl Pts',(21.8330929452547,21.7512978549005,36.7514379862583));
#58886=CARTESIAN_POINT('Ctrl Pts',(19.8629761205629,21.8770354311873,35.8304875664748));
#58887=CARTESIAN_POINT('Ctrl Pts',(18.6408725645071,21.9608654091679,36.5934919535574));
#58888=CARTESIAN_POINT('Ctrl Pts',(18.3253725820279,22.002787788842,37.1492294200333));
#58889=CARTESIAN_POINT('Ctrl Pts',(21.0904144288932,0.125,36.00310066666));
#58890=CARTESIAN_POINT('Ctrl Pts',(21.103548660097,0.125,36.0100889715519));
#58891=CARTESIAN_POINT('Ctrl Pts',(21.1166828913007,0.125,36.0170772764437));
#58892=CARTESIAN_POINT('Ctrl Pts',(21.1298171225045,0.125,36.0240655813356));
#58893=CARTESIAN_POINT('Origin',(20.,0.125,38.1));
#58894=CARTESIAN_POINT('',(20.,-0.075,40.66347));
#58895=CARTESIAN_POINT('Origin',(20.,-0.075,38.1));
#58896=CARTESIAN_POINT('Origin',(20.,0.125,40.66347));
#58897=CARTESIAN_POINT('Origin',(20.,-0.075,38.1));
#58898=CARTESIAN_POINT('',(16.0376,-0.075,38.1));
#58899=CARTESIAN_POINT('Origin',(20.,-0.075,38.1));
#58900=CARTESIAN_POINT('Origin',(20.,21.95,38.1));
#58901=CARTESIAN_POINT('',(18.03653,22.15,38.1));
#58902=CARTESIAN_POINT('',(17.83653,21.95,38.1));
#58903=CARTESIAN_POINT('Origin',(20.,22.15,38.1));
#58904=CARTESIAN_POINT('Origin',(20.,22.15,38.1));
#58905=CARTESIAN_POINT('Origin',(24.2323742019726,-4.901,38.6431964418851));
#58906=CARTESIAN_POINT('',(23.9131875668744,-0.674999999999999,38.7225566853387));
#58907=CARTESIAN_POINT('',(23.9131875668744,-4.501,38.7225566853387));
#58908=CARTESIAN_POINT('',(23.9131875668744,-0.0750000000000001,38.7225566853387));
#58909=CARTESIAN_POINT('',(23.7544810775837,-0.674999999999999,38.7620163125374));
#58910=CARTESIAN_POINT('',(23.7544810775837,-0.674999999999999,38.7620163125374));
#58911=CARTESIAN_POINT('',(23.7544810775837,-4.651,38.7620163125374));
#58912=CARTESIAN_POINT('',(23.7544810775837,-4.901,38.7620163125374));
#58913=CARTESIAN_POINT('Ctrl Pts',(23.9131875668744,-4.50099999999998,38.7225566853387));
#58914=CARTESIAN_POINT('Ctrl Pts',(23.8323033520823,-4.57771996783978,38.7426671482203));
#58915=CARTESIAN_POINT('Ctrl Pts',(23.7544810775837,-4.651,38.7620163125374));
#58916=CARTESIAN_POINT('Origin',(23.7544810775837,-4.901,38.7620163125374));
#58917=CARTESIAN_POINT('',(23.8901204070909,-4.501,38.8533770492488));
#58918=CARTESIAN_POINT('Ctrl Pts',(23.7544810775837,-4.651,38.7620163125374));
#58919=CARTESIAN_POINT('Ctrl Pts',(23.82099229071,-4.57771996783967,38.8068153649425));
#58920=CARTESIAN_POINT('Ctrl Pts',(23.8901204070909,-4.50099999999998,38.8533770492489));
#58921=CARTESIAN_POINT('',(23.8901204070909,-0.674999999999999,38.8533770492488));
#58922=CARTESIAN_POINT('',(24.1629149309058,-0.674999999999999,39.03711954309));
#58923=CARTESIAN_POINT('',(23.8901204070909,-0.0750000000000001,38.8533770492488));
#58924=CARTESIAN_POINT('Origin',(23.9760628220115,-0.674999999999999,38.8010871525125));
#58925=CARTESIAN_POINT('Origin',(20.,-0.674999999999999,38.1));
#58926=CARTESIAN_POINT('Origin',(20.,-4.701,38.1));
#58927=CARTESIAN_POINT('',(16.1876,-4.651,38.1));
#58928=CARTESIAN_POINT('',(16.0381567112477,-4.501,38.0335807605545));
#58929=CARTESIAN_POINT('Ctrl Pts',(16.1876,-4.651,38.1));
#58930=CARTESIAN_POINT('Ctrl Pts',(16.1143199678399,-4.57771996783992,38.0674310968177));
#58931=CARTESIAN_POINT('Ctrl Pts',(16.0381567112477,-4.50099999999999,38.0335807605545));
#58932=CARTESIAN_POINT('',(16.0868124331256,-4.501,37.4774433146613));
#58933=CARTESIAN_POINT('Origin',(20.,-4.501,38.1));
#58934=CARTESIAN_POINT('',(16.2455189224163,-4.65100000000001,37.4379836874626));
#58935=CARTESIAN_POINT('Ctrl Pts',(16.0868124331256,-4.50099999999999,37.4774433146613));
#58936=CARTESIAN_POINT('Ctrl Pts',(16.1676966479178,-4.57771996783991,37.4573328517796));
#58937=CARTESIAN_POINT('Ctrl Pts',(16.2455189224163,-4.65100000000001,37.4379836874626));
#58938=CARTESIAN_POINT('',(16.1098795929091,-4.501,37.3466229507511));
#58939=CARTESIAN_POINT('Ctrl Pts',(16.2455189224163,-4.65100000000001,37.4379836874626));
#58940=CARTESIAN_POINT('Ctrl Pts',(16.1790077092902,-4.57771996783988,37.3931846350576));
#58941=CARTESIAN_POINT('Ctrl Pts',(16.1098795929091,-4.50099999999999,37.3466229507511));
#58942=CARTESIAN_POINT('',(16.2543683790546,-4.501,36.8073834597322));
#58943=CARTESIAN_POINT('Origin',(20.,-4.501,38.1));
#58944=CARTESIAN_POINT('',(16.4175158525158,-4.651,36.7960824055852));
#58945=CARTESIAN_POINT('Ctrl Pts',(16.2543683790546,-4.50099999999999,36.8073834597322));
#58946=CARTESIAN_POINT('Ctrl Pts',(16.3375159261096,-4.57771996783986,36.8016239164704));
#58947=CARTESIAN_POINT('Ctrl Pts',(16.4175158525158,-4.651,36.7960824055852));
#58948=CARTESIAN_POINT('',(16.299801814644,-4.501,36.682556121362));
#58949=CARTESIAN_POINT('Ctrl Pts',(16.4175158525158,-4.651,36.7960824055852));
#58950=CARTESIAN_POINT('Ctrl Pts',(16.3597943679782,-4.57771996783973,36.7404144004953));
#58951=CARTESIAN_POINT('Ctrl Pts',(16.299801814644,-4.50099999999999,36.682556121362));
#58952=CARTESIAN_POINT('',(16.5357334464049,-4.501,36.1765991042837));
#58953=CARTESIAN_POINT('Origin',(20.,-4.501,38.1));
#58954=CARTESIAN_POINT('',(16.6983647506122,-4.651,36.1938));
#58955=CARTESIAN_POINT('Ctrl Pts',(16.5357334464049,-4.50099999999999,36.1765991042837));
#58956=CARTESIAN_POINT('Ctrl Pts',(16.61861792958,-4.57771996783963,36.1853654814492));
#58957=CARTESIAN_POINT('Ctrl Pts',(16.6983647506122,-4.651,36.1938));
#58958=CARTESIAN_POINT('',(16.6021526858504,-4.501,36.0615576069641));
#58959=CARTESIAN_POINT('Ctrl Pts',(16.6983647506122,-4.651,36.1938));
#58960=CARTESIAN_POINT('Ctrl Pts',(16.6511868327625,-4.57771996783981,36.1289544863906));
#58961=CARTESIAN_POINT('Ctrl Pts',(16.6021526858504,-4.50099999999999,36.061557606964));
#58962=CARTESIAN_POINT('',(16.9223584999828,-4.501,35.6042563117636));
#58963=CARTESIAN_POINT('Origin',(20.,-4.501,38.1));
#58964=CARTESIAN_POINT('',(17.0795321650532,-4.651,35.649436516831));
#58965=CARTESIAN_POINT('Ctrl Pts',(16.9223584999827,-4.50099999999999,35.6042563117636));
#58966=CARTESIAN_POINT('Ctrl Pts',(17.0024615161987,-4.57771996783983,35.6272822474223));
#58967=CARTESIAN_POINT('Ctrl Pts',(17.0795321650532,-4.651,35.649436516831));
#58968=CARTESIAN_POINT('',(17.0077454283034,-4.501,35.5024961331769));
#58969=CARTESIAN_POINT('Ctrl Pts',(17.0795321650532,-4.651,35.649436516831));
#58970=CARTESIAN_POINT('Ctrl Pts',(17.0443312910519,-4.57771996783965,35.5773837928196));
#58971=CARTESIAN_POINT('Ctrl Pts',(17.0077454283034,-4.50099999999999,35.5024961331769));
#58972=CARTESIAN_POINT('',(17.4024961331769,-4.501,35.1077454283034));
#58973=CARTESIAN_POINT('Origin',(20.,-4.501,38.1));
#58974=CARTESIAN_POINT('',(17.549436516831,-4.651,35.1795321650532));
#58975=CARTESIAN_POINT('Ctrl Pts',(17.4024961331769,-4.50099999999999,35.1077454283034));
#58976=CARTESIAN_POINT('Ctrl Pts',(17.4773837928199,-4.57771996783995,35.1443312910521));
#58977=CARTESIAN_POINT('Ctrl Pts',(17.549436516831,-4.651,35.1795321650532));
#58978=CARTESIAN_POINT('',(17.5042563117636,-4.501,35.0223584999828));
#58979=CARTESIAN_POINT('Ctrl Pts',(17.549436516831,-4.651,35.1795321650532));
#58980=CARTESIAN_POINT('Ctrl Pts',(17.5272822474223,-4.57771996783968,35.1024615161985));
#58981=CARTESIAN_POINT('Ctrl Pts',(17.5042563117636,-4.501,35.0223584999827));
#58982=CARTESIAN_POINT('',(17.961557606964,-4.501,34.7021526858504));
#58983=CARTESIAN_POINT('Origin',(20.,-4.501,38.1));
#58984=CARTESIAN_POINT('',(18.0938,-4.651,34.7983647506122));
#58985=CARTESIAN_POINT('Ctrl Pts',(17.961557606964,-4.501,34.7021526858504));
#58986=CARTESIAN_POINT('Ctrl Pts',(18.0289544863906,-4.57771996783974,34.7511868327624));
#58987=CARTESIAN_POINT('Ctrl Pts',(18.0938,-4.651,34.7983647506122));
#58988=CARTESIAN_POINT('',(18.0765991042837,-4.501,34.6357334464049));
#58989=CARTESIAN_POINT('Ctrl Pts',(18.0938,-4.651,34.7983647506122));
#58990=CARTESIAN_POINT('Ctrl Pts',(18.0853654814492,-4.57771996783983,34.7186179295802));
#58991=CARTESIAN_POINT('Ctrl Pts',(18.0765991042837,-4.50099999999999,34.6357334464049));
#58992=CARTESIAN_POINT('',(18.582556121362,-4.501,34.399801814644));
#58993=CARTESIAN_POINT('Origin',(20.,-4.501,38.1));
#58994=CARTESIAN_POINT('',(18.6960824055852,-4.65100000000001,34.5175158525158));
#58995=CARTESIAN_POINT('Ctrl Pts',(18.582556121362,-4.50099999999999,34.399801814644));
#58996=CARTESIAN_POINT('Ctrl Pts',(18.6404144004955,-4.57771996784003,34.4597943679785));
#58997=CARTESIAN_POINT('Ctrl Pts',(18.6960824055852,-4.65100000000001,34.5175158525158));
#58998=CARTESIAN_POINT('',(18.7073834597322,-4.501,34.3543683790546));
#58999=CARTESIAN_POINT('Ctrl Pts',(18.6960824055852,-4.65100000000001,34.5175158525158));
#59000=CARTESIAN_POINT('Ctrl Pts',(18.7016239164704,-4.57771996783996,34.4375159261097));
#59001=CARTESIAN_POINT('Ctrl Pts',(18.7073834597322,-4.501,34.3543683790546));
#59002=CARTESIAN_POINT('',(19.2466229507512,-4.501,34.2098795929091));
#59003=CARTESIAN_POINT('Origin',(20.,-4.501,38.1));
#59004=CARTESIAN_POINT('',(19.3379836874626,-4.651,34.3455189224163));
#59005=CARTESIAN_POINT('Ctrl Pts',(19.2466229507511,-4.501,34.2098795929091));
#59006=CARTESIAN_POINT('Ctrl Pts',(19.2931846350574,-4.57771996783949,34.2790077092898));
#59007=CARTESIAN_POINT('Ctrl Pts',(19.3379836874626,-4.651,34.3455189224163));
#59008=CARTESIAN_POINT('',(19.3774433146613,-4.501,34.1868124331256));
#59009=CARTESIAN_POINT('Ctrl Pts',(19.3379836874626,-4.651,34.3455189224163));
#59010=CARTESIAN_POINT('Ctrl Pts',(19.3573328517797,-4.57771996783973,34.2676966479176));
#59011=CARTESIAN_POINT('Ctrl Pts',(19.3774433146613,-4.501,34.1868124331256));
#59012=CARTESIAN_POINT('',(19.9335807605545,-4.501,34.1381567112477));
#59013=CARTESIAN_POINT('Origin',(20.,-4.501,38.1));
#59014=CARTESIAN_POINT('',(20.,-4.65100000000001,34.2876));
#59015=CARTESIAN_POINT('Ctrl Pts',(19.9335807605545,-4.501,34.1381567112477));
#59016=CARTESIAN_POINT('Ctrl Pts',(19.9674310968175,-4.57771996783948,34.2143199678395));
#59017=CARTESIAN_POINT('Ctrl Pts',(20.,-4.65100000000001,34.2876));
#59018=CARTESIAN_POINT('',(20.0664192394455,-4.501,34.1381567112477));
#59019=CARTESIAN_POINT('Ctrl Pts',(20.,-4.65100000000001,34.2876));
#59020=CARTESIAN_POINT('Ctrl Pts',(20.0325689031823,-4.57771996783993,34.2143199678399));
#59021=CARTESIAN_POINT('Ctrl Pts',(20.0664192394455,-4.501,34.1381567112477));
#59022=CARTESIAN_POINT('',(20.6225566853387,-4.501,34.1868124331256));
#59023=CARTESIAN_POINT('Origin',(20.,-4.501,38.1));
#59024=CARTESIAN_POINT('',(20.6620163125374,-4.651,34.3455189224163));
#59025=CARTESIAN_POINT('Ctrl Pts',(20.6225566853387,-4.501,34.1868124331256));
#59026=CARTESIAN_POINT('Ctrl Pts',(20.6426671482203,-4.57771996783972,34.2676966479176));
#59027=CARTESIAN_POINT('Ctrl Pts',(20.6620163125374,-4.651,34.3455189224163));
#59028=CARTESIAN_POINT('',(20.7533770492488,-4.501,34.2098795929091));
#59029=CARTESIAN_POINT('Ctrl Pts',(20.6620163125374,-4.651,34.3455189224163));
#59030=CARTESIAN_POINT('Ctrl Pts',(20.7068153649425,-4.57771996783977,34.2790077092901));
#59031=CARTESIAN_POINT('Ctrl Pts',(20.7533770492489,-4.501,34.2098795929091));
#59032=CARTESIAN_POINT('',(21.2926165402678,-4.501,34.3543683790546));
#59033=CARTESIAN_POINT('Origin',(20.,-4.501,38.1));
#59034=CARTESIAN_POINT('',(21.3039175944148,-4.65100000000001,34.5175158525158));
#59035=CARTESIAN_POINT('Ctrl Pts',(21.2926165402678,-4.501,34.3543683790546));
#59036=CARTESIAN_POINT('Ctrl Pts',(21.2983760835296,-4.57771996783983,34.4375159261096));
#59037=CARTESIAN_POINT('Ctrl Pts',(21.3039175944148,-4.65100000000001,34.5175158525158));
#59038=CARTESIAN_POINT('',(21.417443878638,-4.501,34.399801814644));
#59039=CARTESIAN_POINT('Ctrl Pts',(21.3039175944148,-4.65100000000001,34.5175158525158));
#59040=CARTESIAN_POINT('Ctrl Pts',(21.3595855995048,-4.57771996783964,34.4597943679781));
#59041=CARTESIAN_POINT('Ctrl Pts',(21.417443878638,-4.501,34.399801814644));
#59042=CARTESIAN_POINT('',(21.9234008957163,-4.501,34.6357334464049));
#59043=CARTESIAN_POINT('Origin',(20.,-4.501,38.1));
#59044=CARTESIAN_POINT('',(21.9062,-4.651,34.7983647506122));
#59045=CARTESIAN_POINT('Ctrl Pts',(21.9234008957163,-4.501,34.6357334464049));
#59046=CARTESIAN_POINT('Ctrl Pts',(21.9146345185508,-4.57771996784004,34.7186179295804));
#59047=CARTESIAN_POINT('Ctrl Pts',(21.9062,-4.651,34.7983647506122));
#59048=CARTESIAN_POINT('',(22.038442393036,-4.501,34.7021526858504));
#59049=CARTESIAN_POINT('Ctrl Pts',(21.9062,-4.651,34.7983647506122));
#59050=CARTESIAN_POINT('Ctrl Pts',(21.9710455136096,-4.57771996783961,34.7511868327624));
#59051=CARTESIAN_POINT('Ctrl Pts',(22.038442393036,-4.501,34.7021526858504));
#59052=CARTESIAN_POINT('',(22.4957436882363,-4.501,35.0223584999827));
#59053=CARTESIAN_POINT('Origin',(20.,-4.501,38.1));
#59054=CARTESIAN_POINT('',(22.450563483169,-4.651,35.1795321650532));
#59055=CARTESIAN_POINT('Ctrl Pts',(22.4957436882364,-4.501,35.0223584999827));
#59056=CARTESIAN_POINT('Ctrl Pts',(22.4727177525778,-4.57771996783958,35.1024615161984));
#59057=CARTESIAN_POINT('Ctrl Pts',(22.450563483169,-4.651,35.1795321650532));
#59058=CARTESIAN_POINT('',(22.5975038668231,-4.501,35.1077454283034));
#59059=CARTESIAN_POINT('Ctrl Pts',(22.450563483169,-4.651,35.1795321650532));
#59060=CARTESIAN_POINT('Ctrl Pts',(22.5226162071807,-4.57771996783934,35.1443312910517));
#59061=CARTESIAN_POINT('Ctrl Pts',(22.5975038668231,-4.501,35.1077454283034));
#59062=CARTESIAN_POINT('',(22.9922545716966,-4.501,35.5024961331769));
#59063=CARTESIAN_POINT('Origin',(20.,-4.501,38.1));
#59064=CARTESIAN_POINT('',(22.9204678349468,-4.651,35.649436516831));
#59065=CARTESIAN_POINT('Ctrl Pts',(22.9922545716966,-4.501,35.5024961331769));
#59066=CARTESIAN_POINT('Ctrl Pts',(22.9556687089481,-4.57771996783959,35.5773837928195));
#59067=CARTESIAN_POINT('Ctrl Pts',(22.9204678349468,-4.651,35.649436516831));
#59068=CARTESIAN_POINT('',(23.0776415000172,-4.501,35.6042563117636));
#59069=CARTESIAN_POINT('Ctrl Pts',(22.9204678349468,-4.651,35.649436516831));
#59070=CARTESIAN_POINT('Ctrl Pts',(22.9975384838016,-4.57771996783957,35.6272822474222));
#59071=CARTESIAN_POINT('Ctrl Pts',(23.0776415000173,-4.501,35.6042563117636));
#59072=CARTESIAN_POINT('',(23.3978473141496,-4.501,36.061557606964));
#59073=CARTESIAN_POINT('Origin',(20.,-4.501,38.1));
#59074=CARTESIAN_POINT('',(23.3016352493878,-4.651,36.1938));
#59075=CARTESIAN_POINT('Ctrl Pts',(23.3978473141496,-4.501,36.061557606964));
#59076=CARTESIAN_POINT('Ctrl Pts',(23.3488131672376,-4.5777199678397,36.1289544863905));
#59077=CARTESIAN_POINT('Ctrl Pts',(23.3016352493878,-4.651,36.1938));
#59078=CARTESIAN_POINT('',(23.4642665535951,-4.501,36.1765991042837));
#59079=CARTESIAN_POINT('Ctrl Pts',(23.3016352493878,-4.651,36.1938));
#59080=CARTESIAN_POINT('Ctrl Pts',(23.3813820704202,-4.57771996783943,36.1853654814491));
#59081=CARTESIAN_POINT('Ctrl Pts',(23.4642665535951,-4.501,36.1765991042837));
#59082=CARTESIAN_POINT('',(23.700198185356,-4.501,36.682556121362));
#59083=CARTESIAN_POINT('Origin',(20.,-4.501,38.1));
#59084=CARTESIAN_POINT('',(23.5824841474842,-4.651,36.7960824055852));
#59085=CARTESIAN_POINT('Ctrl Pts',(23.700198185356,-4.501,36.682556121362));
#59086=CARTESIAN_POINT('Ctrl Pts',(23.6402056320216,-4.57771996784001,36.7404144004955));
#59087=CARTESIAN_POINT('Ctrl Pts',(23.5824841474842,-4.651,36.7960824055852));
#59088=CARTESIAN_POINT('',(23.7456316209454,-4.501,36.8073834597322));
#59089=CARTESIAN_POINT('Ctrl Pts',(23.5824841474842,-4.651,36.7960824055852));
#59090=CARTESIAN_POINT('Ctrl Pts',(23.6624840738904,-4.57771996783986,36.8016239164704));
#59091=CARTESIAN_POINT('Ctrl Pts',(23.7456316209454,-4.501,36.8073834597322));
#59092=CARTESIAN_POINT('',(23.8901204070909,-4.501,37.3466229507511));
#59093=CARTESIAN_POINT('Origin',(20.,-4.501,38.1));
#59094=CARTESIAN_POINT('',(23.7544810775837,-4.651,37.4379836874626));
#59095=CARTESIAN_POINT('Ctrl Pts',(23.8901204070909,-4.501,37.3466229507511));
#59096=CARTESIAN_POINT('Ctrl Pts',(23.8209922907099,-4.57771996783982,37.3931846350576));
#59097=CARTESIAN_POINT('Ctrl Pts',(23.7544810775837,-4.651,37.4379836874626));
#59098=CARTESIAN_POINT('',(23.9131875668744,-4.501,37.4774433146613));
#59099=CARTESIAN_POINT('Ctrl Pts',(23.7544810775837,-4.651,37.4379836874626));
#59100=CARTESIAN_POINT('Ctrl Pts',(23.8323033520825,-4.57771996783966,37.4573328517797));
#59101=CARTESIAN_POINT('Ctrl Pts',(23.9131875668744,-4.501,37.4774433146613));
#59102=CARTESIAN_POINT('',(23.9618432887523,-4.501,38.0335807605545));
#59103=CARTESIAN_POINT('Origin',(20.,-4.501,38.1));
#59104=CARTESIAN_POINT('',(23.8124,-4.651,38.1));
#59105=CARTESIAN_POINT('Ctrl Pts',(23.9618432887523,-4.501,38.0335807605545));
#59106=CARTESIAN_POINT('Ctrl Pts',(23.8856800321604,-4.57771996783957,38.0674310968176));
#59107=CARTESIAN_POINT('Ctrl Pts',(23.8124,-4.651,38.1));
#59108=CARTESIAN_POINT('',(23.9618432887523,-4.501,38.1664192394455));
#59109=CARTESIAN_POINT('Ctrl Pts',(23.8124,-4.651,38.1));
#59110=CARTESIAN_POINT('Ctrl Pts',(23.8856800321601,-4.57771996783995,38.1325689031822));
#59111=CARTESIAN_POINT('Ctrl Pts',(23.9618432887523,-4.501,38.1664192394455));
#59112=CARTESIAN_POINT('Origin',(20.,-4.501,38.1));
#59113=CARTESIAN_POINT('',(23.7456316209454,-4.501,39.3926165402678));
#59114=CARTESIAN_POINT('Origin',(20.,-4.501,38.1));
#59115=CARTESIAN_POINT('',(23.5824841474842,-4.65100000000001,39.4039175944148));
#59116=CARTESIAN_POINT('Ctrl Pts',(23.7456316209454,-4.50099999999998,39.3926165402678));
#59117=CARTESIAN_POINT('Ctrl Pts',(23.6624840738902,-4.57771996784001,39.3983760835296));
#59118=CARTESIAN_POINT('Ctrl Pts',(23.5824841474842,-4.65100000000001,39.4039175944148));
#59119=CARTESIAN_POINT('',(23.700198185356,-4.501,39.517443878638));
#59120=CARTESIAN_POINT('Ctrl Pts',(23.5824841474842,-4.65100000000001,39.4039175944148));
#59121=CARTESIAN_POINT('Ctrl Pts',(23.6402056320216,-4.57771996783998,39.4595855995045));
#59122=CARTESIAN_POINT('Ctrl Pts',(23.700198185356,-4.50099999999998,39.517443878638));
#59123=CARTESIAN_POINT('',(23.4642665535951,-4.501,40.0234008957163));
#59124=CARTESIAN_POINT('Origin',(20.,-4.501,38.1));
#59125=CARTESIAN_POINT('',(23.3016352493878,-4.651,40.0062));
#59126=CARTESIAN_POINT('Ctrl Pts',(23.4642665535951,-4.50099999999998,40.0234008957163));
#59127=CARTESIAN_POINT('Ctrl Pts',(23.3813820704201,-4.57771996783958,40.0146345185508));
#59128=CARTESIAN_POINT('Ctrl Pts',(23.3016352493878,-4.651,40.0062));
#59129=CARTESIAN_POINT('',(23.3978473141496,-4.501,40.1384423930359));
#59130=CARTESIAN_POINT('Ctrl Pts',(23.3016352493878,-4.651,40.0062));
#59131=CARTESIAN_POINT('Ctrl Pts',(23.3488131672377,-4.57771996783948,40.0710455136097));
#59132=CARTESIAN_POINT('Ctrl Pts',(23.3978473141496,-4.50099999999999,40.138442393036));
#59133=CARTESIAN_POINT('',(23.0776415000172,-4.501,40.5957436882364));
#59134=CARTESIAN_POINT('Origin',(20.,-4.501,38.1));
#59135=CARTESIAN_POINT('',(22.9204678349468,-4.651,40.550563483169));
#59136=CARTESIAN_POINT('Ctrl Pts',(23.0776415000173,-4.50099999999999,40.5957436882364));
#59137=CARTESIAN_POINT('Ctrl Pts',(22.9975384838016,-4.5777199678396,40.5727177525777));
#59138=CARTESIAN_POINT('Ctrl Pts',(22.9204678349468,-4.651,40.550563483169));
#59139=CARTESIAN_POINT('',(22.9922545716966,-4.501,40.6975038668231));
#59140=CARTESIAN_POINT('Ctrl Pts',(22.9204678349468,-4.651,40.550563483169));
#59141=CARTESIAN_POINT('Ctrl Pts',(22.955668708948,-4.57771996783992,40.6226162071801));
#59142=CARTESIAN_POINT('Ctrl Pts',(22.9922545716966,-4.50099999999998,40.6975038668231));
#59143=CARTESIAN_POINT('',(22.5975038668231,-4.501,41.0922545716966));
#59144=CARTESIAN_POINT('Origin',(20.,-4.501,38.1));
#59145=CARTESIAN_POINT('',(22.450563483169,-4.65100000000001,41.0204678349468));
#59146=CARTESIAN_POINT('Ctrl Pts',(22.5975038668231,-4.50099999999999,41.0922545716966));
#59147=CARTESIAN_POINT('Ctrl Pts',(22.5226162071807,-4.57771996783933,41.0556687089482));
#59148=CARTESIAN_POINT('Ctrl Pts',(22.450563483169,-4.65100000000001,41.0204678349468));
#59149=CARTESIAN_POINT('',(22.4957436882364,-4.501,41.1776415000172));
#59150=CARTESIAN_POINT('Ctrl Pts',(22.450563483169,-4.65100000000001,41.0204678349468));
#59151=CARTESIAN_POINT('Ctrl Pts',(22.4727177525775,-4.57771996784042,41.0975384838007));
#59152=CARTESIAN_POINT('Ctrl Pts',(22.4957436882364,-4.50099999999999,41.1776415000173));
#59153=CARTESIAN_POINT('',(22.038442393036,-4.501,41.4978473141496));
#59154=CARTESIAN_POINT('Origin',(20.,-4.501,38.1));
#59155=CARTESIAN_POINT('',(21.9062,-4.651,41.4016352493878));
#59156=CARTESIAN_POINT('Ctrl Pts',(22.038442393036,-4.50099999999999,41.4978473141496));
#59157=CARTESIAN_POINT('Ctrl Pts',(21.9710455136096,-4.57771996783954,41.4488131672377));
#59158=CARTESIAN_POINT('Ctrl Pts',(21.9062,-4.651,41.4016352493878));
#59159=CARTESIAN_POINT('',(21.9234008957163,-4.501,41.5642665535951));
#59160=CARTESIAN_POINT('Ctrl Pts',(21.9062,-4.651,41.4016352493878));
#59161=CARTESIAN_POINT('Ctrl Pts',(21.9146345185508,-4.57771996784014,41.4813820704194));
#59162=CARTESIAN_POINT('Ctrl Pts',(21.9234008957163,-4.50099999999999,41.5642665535951));
#59163=CARTESIAN_POINT('',(21.417443878638,-4.501,41.800198185356));
#59164=CARTESIAN_POINT('Origin',(20.,-4.501,38.1));
#59165=CARTESIAN_POINT('',(21.3039175944148,-4.65100000000001,41.6824841474842));
#59166=CARTESIAN_POINT('Ctrl Pts',(21.417443878638,-4.50099999999999,41.800198185356));
#59167=CARTESIAN_POINT('Ctrl Pts',(21.3595855995046,-4.57771996783985,41.7402056320217));
#59168=CARTESIAN_POINT('Ctrl Pts',(21.3039175944148,-4.65100000000001,41.6824841474842));
#59169=CARTESIAN_POINT('',(21.2926165402678,-4.501,41.8456316209454));
#59170=CARTESIAN_POINT('Ctrl Pts',(21.3039175944148,-4.65100000000001,41.6824841474842));
#59171=CARTESIAN_POINT('Ctrl Pts',(21.2983760835296,-4.57771996783928,41.762484073891));
#59172=CARTESIAN_POINT('Ctrl Pts',(21.2926165402678,-4.50099999999999,41.8456316209454));
#59173=CARTESIAN_POINT('',(20.7533770492488,-4.501,41.9901204070909));
#59174=CARTESIAN_POINT('Origin',(20.,-4.501,38.1));
#59175=CARTESIAN_POINT('',(20.6620163125374,-4.651,41.8544810775837));
#59176=CARTESIAN_POINT('Ctrl Pts',(20.7533770492489,-4.50099999999999,41.9901204070909));
#59177=CARTESIAN_POINT('Ctrl Pts',(20.7068153649426,-4.57771996783958,41.9209922907101));
#59178=CARTESIAN_POINT('Ctrl Pts',(20.6620163125374,-4.651,41.8544810775837));
#59179=CARTESIAN_POINT('',(20.6225566853387,-4.501,42.0131875668744));
#59180=CARTESIAN_POINT('Ctrl Pts',(20.6620163125374,-4.651,41.8544810775837));
#59181=CARTESIAN_POINT('Ctrl Pts',(20.6426671482204,-4.57771996783993,41.9323033520822));
#59182=CARTESIAN_POINT('Ctrl Pts',(20.6225566853387,-4.50099999999999,42.0131875668744));
#59183=CARTESIAN_POINT('',(20.0664192394455,-4.501,42.0618432887523));
#59184=CARTESIAN_POINT('Origin',(20.,-4.501,38.1));
#59185=CARTESIAN_POINT('',(20.,-4.651,41.9124));
#59186=CARTESIAN_POINT('Ctrl Pts',(20.0664192394455,-4.50099999999999,42.0618432887523));
#59187=CARTESIAN_POINT('Ctrl Pts',(20.0325689031823,-4.5777199678398,41.9856800321602));
#59188=CARTESIAN_POINT('Ctrl Pts',(20.,-4.651,41.9124));
#59189=CARTESIAN_POINT('',(19.9335807605545,-4.501,42.0618432887523));
#59190=CARTESIAN_POINT('Ctrl Pts',(20.,-4.651,41.9124));
#59191=CARTESIAN_POINT('Ctrl Pts',(19.9674310968177,-4.57771996783988,41.9856800321601));
#59192=CARTESIAN_POINT('Ctrl Pts',(19.9335807605545,-4.50099999999999,42.0618432887523));
#59193=CARTESIAN_POINT('',(19.3774433146613,-4.501,42.0131875668744));
#59194=CARTESIAN_POINT('Origin',(20.,-4.501,38.1));
#59195=CARTESIAN_POINT('',(19.3379836874626,-4.651,41.8544810775837));
#59196=CARTESIAN_POINT('Ctrl Pts',(19.3774433146613,-4.50099999999999,42.0131875668744));
#59197=CARTESIAN_POINT('Ctrl Pts',(19.3573328517796,-4.57771996784008,41.932303352082));
#59198=CARTESIAN_POINT('Ctrl Pts',(19.3379836874626,-4.651,41.8544810775837));
#59199=CARTESIAN_POINT('',(19.2466229507511,-4.501,41.9901204070909));
#59200=CARTESIAN_POINT('Ctrl Pts',(19.3379836874626,-4.651,41.8544810775837));
#59201=CARTESIAN_POINT('Ctrl Pts',(19.2931846350574,-4.57771996783954,41.9209922907101));
#59202=CARTESIAN_POINT('Ctrl Pts',(19.2466229507511,-4.50099999999999,41.9901204070909));
#59203=CARTESIAN_POINT('',(18.7073834597322,-4.501,41.8456316209454));
#59204=CARTESIAN_POINT('Origin',(20.,-4.501,38.1));
#59205=CARTESIAN_POINT('',(18.6960824055852,-4.65100000000001,41.6824841474842));
#59206=CARTESIAN_POINT('Ctrl Pts',(18.7073834597322,-4.50099999999999,41.8456316209454));
#59207=CARTESIAN_POINT('Ctrl Pts',(18.7016239164704,-4.57771996784026,41.76248407389));
#59208=CARTESIAN_POINT('Ctrl Pts',(18.6960824055852,-4.65100000000001,41.6824841474842));
#59209=CARTESIAN_POINT('',(18.582556121362,-4.501,41.800198185356));
#59210=CARTESIAN_POINT('Ctrl Pts',(18.6960824055852,-4.65100000000001,41.6824841474842));
#59211=CARTESIAN_POINT('Ctrl Pts',(18.6404144004953,-4.57771996783977,41.7402056320217));
#59212=CARTESIAN_POINT('Ctrl Pts',(18.582556121362,-4.50099999999999,41.800198185356));
#59213=CARTESIAN_POINT('',(18.0765991042837,-4.501,41.5642665535951));
#59214=CARTESIAN_POINT('Origin',(20.,-4.501,38.1));
#59215=CARTESIAN_POINT('',(18.0938,-4.651,41.4016352493878));
#59216=CARTESIAN_POINT('Ctrl Pts',(18.0765991042837,-4.50099999999999,41.5642665535951));
#59217=CARTESIAN_POINT('Ctrl Pts',(18.0853654814492,-4.57771996783993,41.4813820704197));
#59218=CARTESIAN_POINT('Ctrl Pts',(18.0938,-4.651,41.4016352493878));
#59219=CARTESIAN_POINT('',(17.961557606964,-4.501,41.4978473141496));
#59220=CARTESIAN_POINT('Ctrl Pts',(18.0938,-4.651,41.4016352493878));
#59221=CARTESIAN_POINT('Ctrl Pts',(18.0289544863912,-4.57771996784051,41.448813167237));
#59222=CARTESIAN_POINT('Ctrl Pts',(17.961557606964,-4.50099999999999,41.4978473141496));
#59223=CARTESIAN_POINT('',(17.5042563117637,-4.501,41.1776415000173));
#59224=CARTESIAN_POINT('Origin',(20.,-4.501,38.1));
#59225=CARTESIAN_POINT('',(17.549436516831,-4.65100000000001,41.0204678349468));
#59226=CARTESIAN_POINT('Ctrl Pts',(17.5042563117636,-4.50099999999999,41.1776415000173));
#59227=CARTESIAN_POINT('Ctrl Pts',(17.5272822474223,-4.57771996783969,41.0975384838015));
#59228=CARTESIAN_POINT('Ctrl Pts',(17.549436516831,-4.65100000000001,41.0204678349468));
#59229=CARTESIAN_POINT('',(17.4024961331769,-4.501,41.0922545716966));
#59230=CARTESIAN_POINT('Ctrl Pts',(17.549436516831,-4.65100000000001,41.0204678349468));
#59231=CARTESIAN_POINT('Ctrl Pts',(17.4773837928199,-4.57771996783993,41.055668708948));
#59232=CARTESIAN_POINT('Ctrl Pts',(17.4024961331769,-4.50099999999999,41.0922545716966));
#59233=CARTESIAN_POINT('',(17.0077454283034,-4.501,40.6975038668231));
#59234=CARTESIAN_POINT('Origin',(20.,-4.501,38.1));
#59235=CARTESIAN_POINT('',(17.0795321650532,-4.651,40.550563483169));
#59236=CARTESIAN_POINT('Ctrl Pts',(17.0077454283034,-4.50099999999999,40.6975038668231));
#59237=CARTESIAN_POINT('Ctrl Pts',(17.044331291052,-4.57771996783985,40.6226162071802));
#59238=CARTESIAN_POINT('Ctrl Pts',(17.0795321650532,-4.651,40.550563483169));
#59239=CARTESIAN_POINT('',(16.9223584999828,-4.501,40.5957436882364));
#59240=CARTESIAN_POINT('Ctrl Pts',(17.0795321650532,-4.651,40.550563483169));
#59241=CARTESIAN_POINT('Ctrl Pts',(17.0024615161981,-4.57771996783934,40.5727177525778));
#59242=CARTESIAN_POINT('Ctrl Pts',(16.9223584999827,-4.50099999999999,40.5957436882364));
#59243=CARTESIAN_POINT('',(16.6021526858504,-4.501,40.1384423930359));
#59244=CARTESIAN_POINT('Origin',(20.,-4.501,38.1));
#59245=CARTESIAN_POINT('',(16.6983647506122,-4.65100000000001,40.0062));
#59246=CARTESIAN_POINT('Ctrl Pts',(16.6021526858504,-4.50099999999999,40.1384423930359));
#59247=CARTESIAN_POINT('Ctrl Pts',(16.6511868327624,-4.57771996783963,40.0710455136095));
#59248=CARTESIAN_POINT('Ctrl Pts',(16.6983647506122,-4.65100000000001,40.0062));
#59249=CARTESIAN_POINT('',(16.5357334464049,-4.501,40.0234008957163));
#59250=CARTESIAN_POINT('Ctrl Pts',(16.6983647506122,-4.65100000000001,40.0062));
#59251=CARTESIAN_POINT('Ctrl Pts',(16.6186179295803,-4.57771996783988,40.0146345185508));
#59252=CARTESIAN_POINT('Ctrl Pts',(16.5357334464049,-4.50099999999999,40.0234008957163));
#59253=CARTESIAN_POINT('',(16.299801814644,-4.501,39.517443878638));
#59254=CARTESIAN_POINT('Origin',(20.,-4.501,38.1));
#59255=CARTESIAN_POINT('',(16.4175158525158,-4.651,39.4039175944148));
#59256=CARTESIAN_POINT('Ctrl Pts',(16.299801814644,-4.50099999999999,39.517443878638));
#59257=CARTESIAN_POINT('Ctrl Pts',(16.3597943679784,-4.57771996783994,39.4595855995045));
#59258=CARTESIAN_POINT('Ctrl Pts',(16.4175158525158,-4.651,39.4039175944148));
#59259=CARTESIAN_POINT('',(16.2543683790546,-4.501,39.3926165402678));
#59260=CARTESIAN_POINT('Ctrl Pts',(16.4175158525158,-4.651,39.4039175944148));
#59261=CARTESIAN_POINT('Ctrl Pts',(16.3375159261095,-4.57771996783976,39.3983760835296));
#59262=CARTESIAN_POINT('Ctrl Pts',(16.2543683790546,-4.50099999999999,39.3926165402678));
#59263=CARTESIAN_POINT('',(16.1098795929091,-4.501,38.8533770492488));
#59264=CARTESIAN_POINT('Origin',(20.,-4.501,38.1));
#59265=CARTESIAN_POINT('',(16.2455189224163,-4.651,38.7620163125374));
#59266=CARTESIAN_POINT('Ctrl Pts',(16.1098795929091,-4.50099999999999,38.8533770492489));
#59267=CARTESIAN_POINT('Ctrl Pts',(16.1790077092901,-4.57771996783979,38.8068153649424));
#59268=CARTESIAN_POINT('Ctrl Pts',(16.2455189224163,-4.651,38.7620163125374));
#59269=CARTESIAN_POINT('',(16.0868124331256,-4.501,38.7225566853387));
#59270=CARTESIAN_POINT('Ctrl Pts',(16.2455189224163,-4.651,38.7620163125374));
#59271=CARTESIAN_POINT('Ctrl Pts',(16.1676966479176,-4.5777199678397,38.7426671482203));
#59272=CARTESIAN_POINT('Ctrl Pts',(16.0868124331256,-4.50099999999999,38.7225566853387));
#59273=CARTESIAN_POINT('',(16.0381567112477,-4.501,38.1664192394455));
#59274=CARTESIAN_POINT('Origin',(20.,-4.501,38.1));
#59275=CARTESIAN_POINT('Ctrl Pts',(16.0381567112477,-4.50099999999999,38.1664192394455));
#59276=CARTESIAN_POINT('Ctrl Pts',(16.1143199678397,-4.57771996783974,38.1325689031823));
#59277=CARTESIAN_POINT('Ctrl Pts',(16.1876,-4.651,38.1));
#59278=CARTESIAN_POINT('',(16.4376,-4.901,38.1));
#59279=CARTESIAN_POINT('',(16.2376,-4.701,38.1));
#59280=CARTESIAN_POINT('Origin',(20.,-4.901,38.1));
#59281=CARTESIAN_POINT('Origin',(23.793914987161,-0.674999999999999,39.4808721266631));
#59282=CARTESIAN_POINT('',(23.700198185356,-0.674999999999999,39.517443878638));
#59283=CARTESIAN_POINT('',(23.7456316209454,-0.674999999999999,39.3926165402678));
#59284=CARTESIAN_POINT('Origin',(20.,-0.674999999999999,38.1));
#59285=CARTESIAN_POINT('',(23.5824841474842,-0.674999999999999,39.4039175944148));
#59286=CARTESIAN_POINT('',(23.9369417981727,-0.674999999999999,39.7457651830685));
#59287=CARTESIAN_POINT('',(23.5824841474842,-0.674999999999999,39.4039175944148));
#59288=CARTESIAN_POINT('Origin',(24.073749855503,-4.901,39.3698881347541));
#59289=CARTESIAN_POINT('',(23.7456316209454,-0.0750000000000001,39.3926165402678));
#59290=CARTESIAN_POINT('',(23.5824841474842,-4.901,39.4039175944148));
#59291=CARTESIAN_POINT('Origin',(23.5824841474842,-4.901,39.4039175944148));
#59292=CARTESIAN_POINT('',(23.700198185356,-0.0750000000000001,39.517443878638));
#59293=CARTESIAN_POINT('Origin',(20.,-0.075,38.1));
#59294=CARTESIAN_POINT('',(16.0381567112477,-0.674999999999999,38.0335807605545));
#59295=CARTESIAN_POINT('',(16.0376,-0.674999999999999,38.1));
#59296=CARTESIAN_POINT('Origin',(20.,-0.674999999999999,38.1));
#59297=CARTESIAN_POINT('',(16.0376,-0.075,38.1));
#59298=CARTESIAN_POINT('',(16.0381567112477,-0.674999999999999,38.1664192394455));
#59299=CARTESIAN_POINT('Origin',(20.,-0.674999999999999,38.1));
#59300=CARTESIAN_POINT('',(16.0381567112477,-0.0750000000000001,38.1664192394455));
#59301=CARTESIAN_POINT('',(16.0868124331256,-0.674999999999999,38.7225566853387));
#59302=CARTESIAN_POINT('',(16.0868124331256,-0.0750000000000001,38.7225566853387));
#59303=CARTESIAN_POINT('',(16.1098795929091,-0.674999999999999,38.8533770492488));
#59304=CARTESIAN_POINT('Origin',(20.,-0.674999999999999,38.1));
#59305=CARTESIAN_POINT('',(16.1098795929091,-0.0750000000000001,38.8533770492488));
#59306=CARTESIAN_POINT('',(16.2543683790546,-0.674999999999999,39.3926165402678));
#59307=CARTESIAN_POINT('',(16.2543683790546,-0.0750000000000001,39.3926165402678));
#59308=CARTESIAN_POINT('',(16.299801814644,-0.674999999999999,39.517443878638));
#59309=CARTESIAN_POINT('Origin',(20.,-0.674999999999999,38.1));
#59310=CARTESIAN_POINT('',(16.299801814644,-0.0750000000000001,39.517443878638));
#59311=CARTESIAN_POINT('',(16.5357334464049,-0.674999999999999,40.0234008957163));
#59312=CARTESIAN_POINT('',(16.5357334464049,-0.0750000000000001,40.0234008957163));
#59313=CARTESIAN_POINT('',(16.6021526858504,-0.674999999999999,40.1384423930359));
#59314=CARTESIAN_POINT('Origin',(20.,-0.674999999999999,38.1));
#59315=CARTESIAN_POINT('',(16.6021526858504,-0.0750000000000001,40.1384423930359));
#59316=CARTESIAN_POINT('',(16.9223584999828,-0.674999999999999,40.5957436882364));
#59317=CARTESIAN_POINT('',(16.9223584999828,-0.0750000000000001,40.5957436882364));
#59318=CARTESIAN_POINT('',(17.0077454283034,-0.674999999999999,40.6975038668231));
#59319=CARTESIAN_POINT('Origin',(20.,-0.674999999999999,38.1));
#59320=CARTESIAN_POINT('',(17.0077454283034,-0.0750000000000001,40.6975038668231));
#59321=CARTESIAN_POINT('',(17.4024961331769,-0.674999999999999,41.0922545716966));
#59322=CARTESIAN_POINT('',(17.4024961331769,-0.0750000000000001,41.0922545716966));
#59323=CARTESIAN_POINT('',(17.5042563117636,-0.674999999999999,41.1776415000172));
#59324=CARTESIAN_POINT('Origin',(20.,-0.674999999999999,38.1));
#59325=CARTESIAN_POINT('',(17.5042563117637,-0.0750000000000001,41.1776415000173));
#59326=CARTESIAN_POINT('',(17.9615576069641,-0.674999999999999,41.4978473141496));
#59327=CARTESIAN_POINT('',(17.961557606964,-0.0750000000000001,41.4978473141496));
#59328=CARTESIAN_POINT('',(18.0765991042837,-0.674999999999999,41.5642665535951));
#59329=CARTESIAN_POINT('Origin',(20.,-0.674999999999999,38.1));
#59330=CARTESIAN_POINT('',(18.0765991042837,-0.0750000000000001,41.5642665535951));
#59331=CARTESIAN_POINT('',(18.582556121362,-0.674999999999999,41.800198185356));
#59332=CARTESIAN_POINT('',(18.582556121362,-0.0750000000000001,41.800198185356));
#59333=CARTESIAN_POINT('',(18.7073834597322,-0.674999999999999,41.8456316209454));
#59334=CARTESIAN_POINT('Origin',(20.,-0.674999999999999,38.1));
#59335=CARTESIAN_POINT('',(18.7073834597322,-0.0750000000000001,41.8456316209454));
#59336=CARTESIAN_POINT('',(19.2466229507512,-0.674999999999999,41.9901204070909));
#59337=CARTESIAN_POINT('',(19.2466229507511,-0.0750000000000001,41.9901204070909));
#59338=CARTESIAN_POINT('',(19.3774433146613,-0.674999999999999,42.0131875668744));
#59339=CARTESIAN_POINT('Origin',(20.,-0.674999999999999,38.1));
#59340=CARTESIAN_POINT('',(19.3774433146613,-0.0750000000000001,42.0131875668744));
#59341=CARTESIAN_POINT('',(19.9335807605545,-0.674999999999999,42.0618432887523));
#59342=CARTESIAN_POINT('',(19.9335807605545,-0.0750000000000001,42.0618432887523));
#59343=CARTESIAN_POINT('',(20.0664192394455,-0.674999999999999,42.0618432887523));
#59344=CARTESIAN_POINT('Origin',(20.,-0.674999999999999,38.1));
#59345=CARTESIAN_POINT('',(20.0664192394455,-0.0750000000000001,42.0618432887523));
#59346=CARTESIAN_POINT('',(20.6225566853387,-0.674999999999999,42.0131875668744));
#59347=CARTESIAN_POINT('',(20.6225566853387,-0.0750000000000001,42.0131875668744));
#59348=CARTESIAN_POINT('',(20.7533770492489,-0.674999999999999,41.9901204070909));
#59349=CARTESIAN_POINT('Origin',(20.,-0.674999999999999,38.1));
#59350=CARTESIAN_POINT('',(20.7533770492488,-0.0750000000000001,41.9901204070909));
#59351=CARTESIAN_POINT('',(21.2926165402678,-0.674999999999999,41.8456316209454));
#59352=CARTESIAN_POINT('',(21.2926165402678,-0.0750000000000001,41.8456316209454));
#59353=CARTESIAN_POINT('',(21.417443878638,-0.674999999999999,41.800198185356));
#59354=CARTESIAN_POINT('Origin',(20.,-0.674999999999999,38.1));
#59355=CARTESIAN_POINT('',(21.417443878638,-0.0750000000000001,41.800198185356));
#59356=CARTESIAN_POINT('',(21.9234008957163,-0.674999999999999,41.5642665535951));
#59357=CARTESIAN_POINT('',(21.9234008957163,-0.0750000000000001,41.5642665535951));
#59358=CARTESIAN_POINT('',(22.038442393036,-0.674999999999999,41.4978473141496));
#59359=CARTESIAN_POINT('Origin',(20.,-0.674999999999999,38.1));
#59360=CARTESIAN_POINT('',(22.038442393036,-0.0750000000000001,41.4978473141496));
#59361=CARTESIAN_POINT('',(22.4957436882364,-0.674999999999999,41.1776415000172));
#59362=CARTESIAN_POINT('',(22.4957436882364,-0.0750000000000001,41.1776415000172));
#59363=CARTESIAN_POINT('',(22.5975038668231,-0.674999999999999,41.0922545716966));
#59364=CARTESIAN_POINT('Origin',(20.,-0.674999999999999,38.1));
#59365=CARTESIAN_POINT('',(22.5975038668231,-0.0750000000000001,41.0922545716966));
#59366=CARTESIAN_POINT('',(22.9922545716966,-0.674999999999999,40.6975038668231));
#59367=CARTESIAN_POINT('',(22.9922545716966,-0.0750000000000001,40.6975038668231));
#59368=CARTESIAN_POINT('',(23.0776415000173,-0.674999999999999,40.5957436882363));
#59369=CARTESIAN_POINT('Origin',(20.,-0.674999999999999,38.1));
#59370=CARTESIAN_POINT('',(23.0776415000172,-0.0750000000000001,40.5957436882364));
#59371=CARTESIAN_POINT('',(23.3978473141496,-0.674999999999999,40.1384423930359));
#59372=CARTESIAN_POINT('',(23.3978473141496,-0.0750000000000001,40.1384423930359));
#59373=CARTESIAN_POINT('',(23.4642665535951,-0.674999999999999,40.0234008957163));
#59374=CARTESIAN_POINT('Origin',(20.,-0.674999999999999,38.1));
#59375=CARTESIAN_POINT('',(23.4642665535951,-0.0750000000000001,40.0234008957163));
#59376=CARTESIAN_POINT('',(23.9618432887523,-0.674999999999999,38.1664192394455));
#59377=CARTESIAN_POINT('',(23.9618432887523,-0.0750000000000001,38.1664192394455));
#59378=CARTESIAN_POINT('',(23.9618432887523,-0.674999999999999,38.0335807605545));
#59379=CARTESIAN_POINT('Origin',(20.,-0.674999999999999,38.1));
#59380=CARTESIAN_POINT('',(23.9618432887523,-0.0750000000000001,38.0335807605545));
#59381=CARTESIAN_POINT('',(23.9131875668744,-0.674999999999999,37.4774433146613));
#59382=CARTESIAN_POINT('',(23.9131875668744,-0.0750000000000001,37.4774433146613));
#59383=CARTESIAN_POINT('',(23.8901204070909,-0.674999999999999,37.3466229507511));
#59384=CARTESIAN_POINT('Origin',(20.,-0.674999999999999,38.1));
#59385=CARTESIAN_POINT('',(23.8901204070909,-0.0750000000000001,37.3466229507511));
#59386=CARTESIAN_POINT('',(23.7456316209454,-0.674999999999999,36.8073834597322));
#59387=CARTESIAN_POINT('',(23.7456316209454,-0.0750000000000001,36.8073834597322));
#59388=CARTESIAN_POINT('',(23.700198185356,-0.674999999999999,36.682556121362));
#59389=CARTESIAN_POINT('Origin',(20.,-0.674999999999999,38.1));
#59390=CARTESIAN_POINT('',(23.700198185356,-0.0750000000000001,36.682556121362));
#59391=CARTESIAN_POINT('',(23.4642665535951,-0.674999999999999,36.1765991042837));
#59392=CARTESIAN_POINT('',(23.4642665535951,-0.0750000000000001,36.1765991042837));
#59393=CARTESIAN_POINT('',(23.3978473141496,-0.674999999999999,36.061557606964));
#59394=CARTESIAN_POINT('Origin',(20.,-0.674999999999999,38.1));
#59395=CARTESIAN_POINT('',(23.3978473141496,-0.0750000000000001,36.061557606964));
#59396=CARTESIAN_POINT('',(23.0776415000172,-0.674999999999999,35.6042563117636));
#59397=CARTESIAN_POINT('',(23.0776415000172,-0.0750000000000001,35.6042563117636));
#59398=CARTESIAN_POINT('',(22.9922545716966,-0.674999999999999,35.5024961331769));
#59399=CARTESIAN_POINT('Origin',(20.,-0.674999999999999,38.1));
#59400=CARTESIAN_POINT('',(22.9922545716966,-0.0750000000000001,35.5024961331769));
#59401=CARTESIAN_POINT('',(22.5975038668231,-0.674999999999999,35.1077454283034));
#59402=CARTESIAN_POINT('',(22.5975038668231,-0.0750000000000001,35.1077454283034));
#59403=CARTESIAN_POINT('',(22.4957436882364,-0.674999999999999,35.0223584999828));
#59404=CARTESIAN_POINT('Origin',(20.,-0.674999999999999,38.1));
#59405=CARTESIAN_POINT('',(22.4957436882363,-0.0750000000000001,35.0223584999827));
#59406=CARTESIAN_POINT('',(22.038442393036,-0.674999999999999,34.7021526858504));
#59407=CARTESIAN_POINT('',(22.038442393036,-0.0750000000000001,34.7021526858504));
#59408=CARTESIAN_POINT('',(21.9234008957163,-0.674999999999999,34.6357334464049));
#59409=CARTESIAN_POINT('Origin',(20.,-0.674999999999999,38.1));
#59410=CARTESIAN_POINT('',(21.9234008957163,-0.0750000000000001,34.6357334464049));
#59411=CARTESIAN_POINT('',(21.417443878638,-0.674999999999999,34.399801814644));
#59412=CARTESIAN_POINT('',(21.417443878638,-0.0750000000000001,34.399801814644));
#59413=CARTESIAN_POINT('',(21.2926165402678,-0.674999999999999,34.3543683790546));
#59414=CARTESIAN_POINT('Origin',(20.,-0.674999999999999,38.1));
#59415=CARTESIAN_POINT('',(21.2926165402678,-0.0750000000000001,34.3543683790546));
#59416=CARTESIAN_POINT('',(20.7533770492489,-0.674999999999999,34.2098795929091));
#59417=CARTESIAN_POINT('',(20.7533770492488,-0.0750000000000001,34.2098795929091));
#59418=CARTESIAN_POINT('',(20.6225566853387,-0.674999999999999,34.1868124331256));
#59419=CARTESIAN_POINT('Origin',(20.,-0.674999999999999,38.1));
#59420=CARTESIAN_POINT('',(20.6225566853387,-0.0750000000000001,34.1868124331256));
#59421=CARTESIAN_POINT('',(20.0664192394455,-0.674999999999999,34.1381567112477));
#59422=CARTESIAN_POINT('',(20.0664192394455,-0.0750000000000001,34.1381567112477));
#59423=CARTESIAN_POINT('',(19.9335807605545,-0.674999999999999,34.1381567112477));
#59424=CARTESIAN_POINT('Origin',(20.,-0.674999999999999,38.1));
#59425=CARTESIAN_POINT('',(19.9335807605545,-0.0750000000000001,34.1381567112477));
#59426=CARTESIAN_POINT('',(19.3774433146613,-0.674999999999999,34.1868124331256));
#59427=CARTESIAN_POINT('',(19.3774433146613,-0.0750000000000001,34.1868124331256));
#59428=CARTESIAN_POINT('',(19.2466229507511,-0.674999999999999,34.2098795929091));
#59429=CARTESIAN_POINT('Origin',(20.,-0.674999999999999,38.1));
#59430=CARTESIAN_POINT('',(19.2466229507512,-0.0750000000000001,34.2098795929091));
#59431=CARTESIAN_POINT('',(18.7073834597322,-0.674999999999999,34.3543683790546));
#59432=CARTESIAN_POINT('',(18.7073834597322,-0.0750000000000001,34.3543683790546));
#59433=CARTESIAN_POINT('',(18.582556121362,-0.674999999999999,34.399801814644));
#59434=CARTESIAN_POINT('Origin',(20.,-0.674999999999999,38.1));
#59435=CARTESIAN_POINT('',(18.582556121362,-0.0750000000000001,34.399801814644));
#59436=CARTESIAN_POINT('',(18.0765991042837,-0.674999999999999,34.6357334464049));
#59437=CARTESIAN_POINT('',(18.0765991042837,-0.0750000000000001,34.6357334464049));
#59438=CARTESIAN_POINT('',(17.961557606964,-0.674999999999999,34.7021526858504));
#59439=CARTESIAN_POINT('Origin',(20.,-0.674999999999999,38.1));
#59440=CARTESIAN_POINT('',(17.961557606964,-0.0750000000000001,34.7021526858504));
#59441=CARTESIAN_POINT('',(17.5042563117636,-0.674999999999999,35.0223584999828));
#59442=CARTESIAN_POINT('',(17.5042563117636,-0.0750000000000001,35.0223584999828));
#59443=CARTESIAN_POINT('',(17.4024961331769,-0.674999999999999,35.1077454283034));
#59444=CARTESIAN_POINT('Origin',(20.,-0.674999999999999,38.1));
#59445=CARTESIAN_POINT('',(17.4024961331769,-0.0750000000000001,35.1077454283034));
#59446=CARTESIAN_POINT('',(17.0077454283034,-0.674999999999999,35.5024961331769));
#59447=CARTESIAN_POINT('',(17.0077454283034,-0.0750000000000001,35.5024961331769));
#59448=CARTESIAN_POINT('',(16.9223584999828,-0.674999999999999,35.6042563117636));
#59449=CARTESIAN_POINT('Origin',(20.,-0.674999999999999,38.1));
#59450=CARTESIAN_POINT('',(16.9223584999828,-0.0750000000000001,35.6042563117636));
#59451=CARTESIAN_POINT('',(16.6021526858504,-0.674999999999999,36.0615576069641));
#59452=CARTESIAN_POINT('',(16.6021526858504,-0.0750000000000001,36.0615576069641));
#59453=CARTESIAN_POINT('',(16.5357334464049,-0.674999999999999,36.1765991042837));
#59454=CARTESIAN_POINT('Origin',(20.,-0.674999999999999,38.1));
#59455=CARTESIAN_POINT('',(16.5357334464049,-0.0750000000000001,36.1765991042837));
#59456=CARTESIAN_POINT('',(16.299801814644,-0.674999999999999,36.682556121362));
#59457=CARTESIAN_POINT('',(16.299801814644,-0.0750000000000001,36.682556121362));
#59458=CARTESIAN_POINT('',(16.2543683790546,-0.674999999999999,36.8073834597322));
#59459=CARTESIAN_POINT('Origin',(20.,-0.674999999999999,38.1));
#59460=CARTESIAN_POINT('',(16.2543683790546,-0.0750000000000001,36.8073834597322));
#59461=CARTESIAN_POINT('',(16.1098795929091,-0.674999999999999,37.3466229507511));
#59462=CARTESIAN_POINT('',(16.1098795929091,-0.0750000000000001,37.3466229507511));
#59463=CARTESIAN_POINT('',(16.0868124331256,-0.674999999999999,37.4774433146613));
#59464=CARTESIAN_POINT('Origin',(20.,-0.674999999999999,38.1));
#59465=CARTESIAN_POINT('',(16.0868124331256,-0.0750000000000001,37.4774433146613));
#59466=CARTESIAN_POINT('',(16.0381567112477,-0.0750000000000001,38.0335807605545));
#59467=CARTESIAN_POINT('Origin',(23.7913466810908,-4.901,40.0579949192431));
#59468=CARTESIAN_POINT('',(23.3016352493878,-0.674999999999999,40.0062));
#59469=CARTESIAN_POINT('',(23.3016352493878,-0.674999999999999,40.0062));
#59470=CARTESIAN_POINT('',(23.3016352493878,-4.901,40.0062));
#59471=CARTESIAN_POINT('Origin',(23.3016352493878,-4.901,40.0062));
#59472=CARTESIAN_POINT('',(23.5913466810908,-0.674999999999999,40.4044050807569));
#59473=CARTESIAN_POINT('Origin',(23.4964909652393,-0.674999999999999,40.1187));
#59474=CARTESIAN_POINT('Origin',(23.0928278346486,-0.674999999999999,40.6951906953484));
#59475=CARTESIAN_POINT('',(22.9204678349468,-0.674999999999999,40.550563483169));
#59476=CARTESIAN_POINT('',(23.136630312413,-0.674999999999999,40.9930267961517));
#59477=CARTESIAN_POINT('',(22.9204678349468,-0.674999999999999,40.550563483169));
#59478=CARTESIAN_POINT('Origin',(23.3937453562876,-4.901,40.6866090189041));
#59479=CARTESIAN_POINT('',(22.9204678349468,-4.901,40.550563483169));
#59480=CARTESIAN_POINT('Origin',(22.9204678349468,-4.901,40.550563483169));
#59481=CARTESIAN_POINT('Origin',(22.8930267961517,-4.901,41.236630312413));
#59482=CARTESIAN_POINT('',(22.450563483169,-0.674999999999999,41.0204678349468));
#59483=CARTESIAN_POINT('',(22.450563483169,-0.674999999999999,41.0204678349468));
#59484=CARTESIAN_POINT('',(22.450563483169,-4.901,41.0204678349468));
#59485=CARTESIAN_POINT('Origin',(22.450563483169,-4.901,41.0204678349468));
#59486=CARTESIAN_POINT('',(22.5866090189041,-0.674999999999999,41.4937453562876));
#59487=CARTESIAN_POINT('Origin',(22.5951906953484,-0.674999999999999,41.1928278346486));
#59488=CARTESIAN_POINT('Origin',(22.0187,-0.674999999999999,41.5964909652393));
#59489=CARTESIAN_POINT('',(21.9062,-0.674999999999999,41.4016352493878));
#59490=CARTESIAN_POINT('',(21.9579949192431,-0.674999999999999,41.8913466810908));
#59491=CARTESIAN_POINT('',(21.9062,-0.674999999999999,41.4016352493878));
#59492=CARTESIAN_POINT('Origin',(22.3044050807569,-4.901,41.6913466810908));
#59493=CARTESIAN_POINT('',(21.9062,-4.901,41.4016352493878));
#59494=CARTESIAN_POINT('Origin',(21.9062,-4.901,41.4016352493878));
#59495=CARTESIAN_POINT('Origin',(21.6457651830685,-4.901,42.0369417981727));
#59496=CARTESIAN_POINT('',(21.3039175944148,-0.674999999999999,41.6824841474842));
#59497=CARTESIAN_POINT('',(21.3039175944148,-0.674999999999999,41.6824841474842));
#59498=CARTESIAN_POINT('',(21.3039175944148,-4.901,41.6824841474842));
#59499=CARTESIAN_POINT('Origin',(21.3039175944148,-4.901,41.6824841474842));
#59500=CARTESIAN_POINT('',(21.2698881347541,-0.674999999999999,42.173749855503));
#59501=CARTESIAN_POINT('Origin',(21.3808721266631,-0.674999999999999,41.893914987161));
#59502=CARTESIAN_POINT('Origin',(20.7010871525125,-0.674999999999999,42.0760628220115));
#59503=CARTESIAN_POINT('',(20.6620163125374,-0.674999999999999,41.8544810775837));
#59504=CARTESIAN_POINT('',(20.5431964418851,-0.674999999999999,42.3323742019726));
#59505=CARTESIAN_POINT('',(20.6620163125374,-0.674999999999999,41.8544810775837));
#59506=CARTESIAN_POINT('Origin',(20.93711954309,-4.901,42.2629149309058));
#59507=CARTESIAN_POINT('',(20.6620163125374,-4.901,41.8544810775837));
#59508=CARTESIAN_POINT('Origin',(20.6620163125374,-4.901,41.8544810775837));
#59509=CARTESIAN_POINT('Origin',(20.2,-4.901,42.3624));
#59510=CARTESIAN_POINT('',(20.,-0.674999999999999,41.9124));
#59511=CARTESIAN_POINT('',(20.,-0.674999999999999,41.9124));
#59512=CARTESIAN_POINT('',(20.,-4.901,41.9124));
#59513=CARTESIAN_POINT('Origin',(20.,-4.901,41.9124));
#59514=CARTESIAN_POINT('',(19.8,-0.674999999999999,42.3624));
#59515=CARTESIAN_POINT('Origin',(20.,-0.674999999999999,42.1374));
#59516=CARTESIAN_POINT('Origin',(19.2989128474875,-0.674999999999999,42.0760628220115));
#59517=CARTESIAN_POINT('',(19.3379836874626,-0.674999999999999,41.8544810775837));
#59518=CARTESIAN_POINT('',(19.06288045691,-0.674999999999999,42.2629149309059));
#59519=CARTESIAN_POINT('',(19.3379836874626,-0.674999999999999,41.8544810775837));
#59520=CARTESIAN_POINT('Origin',(19.4568035581149,-4.901,42.3323742019726));
#59521=CARTESIAN_POINT('',(19.3379836874626,-4.901,41.8544810775837));
#59522=CARTESIAN_POINT('Origin',(19.3379836874626,-4.901,41.8544810775837));
#59523=CARTESIAN_POINT('Origin',(18.7301118652459,-4.901,42.173749855503));
#59524=CARTESIAN_POINT('',(18.6960824055852,-0.674999999999999,41.6824841474842));
#59525=CARTESIAN_POINT('',(18.6960824055852,-0.674999999999999,41.6824841474842));
#59526=CARTESIAN_POINT('',(18.6960824055852,-4.901,41.6824841474842));
#59527=CARTESIAN_POINT('Origin',(18.6960824055852,-4.901,41.6824841474842));
#59528=CARTESIAN_POINT('',(18.3542348169315,-0.674999999999999,42.0369417981727));
#59529=CARTESIAN_POINT('Origin',(18.6191278733369,-0.674999999999999,41.893914987161));
#59530=CARTESIAN_POINT('Origin',(17.9813,-0.674999999999999,41.5964909652393));
#59531=CARTESIAN_POINT('',(18.0938,-0.674999999999999,41.4016352493878));
#59532=CARTESIAN_POINT('',(17.6955949192431,-0.674999999999999,41.6913466810908));
#59533=CARTESIAN_POINT('',(18.0938,-0.674999999999999,41.4016352493878));
#59534=CARTESIAN_POINT('Origin',(18.0420050807569,-4.901,41.8913466810908));
#59535=CARTESIAN_POINT('',(18.0938,-4.901,41.4016352493878));
#59536=CARTESIAN_POINT('Origin',(18.0938,-4.901,41.4016352493878));
#59537=CARTESIAN_POINT('Origin',(17.4133909810959,-4.901,41.4937453562876));
#59538=CARTESIAN_POINT('',(17.549436516831,-0.674999999999999,41.0204678349468));
#59539=CARTESIAN_POINT('',(17.549436516831,-0.674999999999999,41.0204678349468));
#59540=CARTESIAN_POINT('',(17.549436516831,-4.901,41.0204678349468));
#59541=CARTESIAN_POINT('Origin',(17.549436516831,-4.901,41.0204678349468));
#59542=CARTESIAN_POINT('',(17.1069732038483,-0.674999999999999,41.236630312413));
#59543=CARTESIAN_POINT('Origin',(17.4048093046516,-0.674999999999999,41.1928278346486));
#59544=CARTESIAN_POINT('Origin',(16.9071721653514,-0.674999999999999,40.6951906953484));
#59545=CARTESIAN_POINT('',(17.0795321650532,-0.674999999999999,40.550563483169));
#59546=CARTESIAN_POINT('',(16.6062546437124,-0.674999999999999,40.6866090189041));
#59547=CARTESIAN_POINT('',(17.0795321650532,-0.674999999999999,40.550563483169));
#59548=CARTESIAN_POINT('Origin',(16.863369687587,-4.901,40.9930267961517));
#59549=CARTESIAN_POINT('',(17.0795321650532,-4.901,40.550563483169));
#59550=CARTESIAN_POINT('Origin',(17.0795321650532,-4.901,40.550563483169));
#59551=CARTESIAN_POINT('Origin',(16.4086533189092,-4.901,40.4044050807569));
#59552=CARTESIAN_POINT('',(16.6983647506122,-0.674999999999999,40.0062));
#59553=CARTESIAN_POINT('',(16.6983647506122,-0.674999999999999,40.0062));
#59554=CARTESIAN_POINT('',(16.6983647506122,-4.901,40.0062));
#59555=CARTESIAN_POINT('Origin',(16.6983647506122,-4.901,40.0062));
#59556=CARTESIAN_POINT('',(16.2086533189092,-0.674999999999999,40.0579949192431));
#59557=CARTESIAN_POINT('Origin',(16.5035090347607,-0.674999999999999,40.1187));
#59558=CARTESIAN_POINT('Origin',(16.206085012839,-0.674999999999999,39.480872126663));
#59559=CARTESIAN_POINT('',(16.4175158525158,-0.674999999999999,39.4039175944148));
#59560=CARTESIAN_POINT('',(15.926250144497,-0.674999999999999,39.3698881347541));
#59561=CARTESIAN_POINT('',(16.4175158525158,-0.674999999999999,39.4039175944148));
#59562=CARTESIAN_POINT('Origin',(16.0630582018273,-4.901,39.7457651830685));
#59563=CARTESIAN_POINT('',(16.4175158525158,-4.901,39.4039175944148));
#59564=CARTESIAN_POINT('Origin',(16.4175158525158,-4.901,39.4039175944148));
#59565=CARTESIAN_POINT('Origin',(15.8370850690942,-4.901,39.03711954309));
#59566=CARTESIAN_POINT('',(16.2455189224163,-0.674999999999999,38.7620163125374));
#59567=CARTESIAN_POINT('',(16.2455189224163,-0.674999999999999,38.7620163125374));
#59568=CARTESIAN_POINT('',(16.2455189224163,-4.901,38.7620163125374));
#59569=CARTESIAN_POINT('Origin',(16.2455189224163,-4.901,38.7620163125374));
#59570=CARTESIAN_POINT('',(15.7676257980274,-0.674999999999999,38.6431964418851));
#59571=CARTESIAN_POINT('Origin',(16.0239371779885,-0.674999999999999,38.8010871525125));
#59572=CARTESIAN_POINT('Origin',(15.9626,-0.674999999999999,38.1));
#59573=CARTESIAN_POINT('',(16.1876,-0.674999999999999,38.1));
#59574=CARTESIAN_POINT('',(15.7376,-0.674999999999999,37.9));
#59575=CARTESIAN_POINT('',(16.1876,-0.674999999999999,38.1));
#59576=CARTESIAN_POINT('Origin',(15.7376,-4.901,38.3));
#59577=CARTESIAN_POINT('',(16.1876,-4.901,38.1));
#59578=CARTESIAN_POINT('Origin',(16.1876,-4.901,38.1));
#59579=CARTESIAN_POINT('Origin',(15.7676257980274,-4.901,37.5568035581149));
#59580=CARTESIAN_POINT('',(16.2455189224163,-0.674999999999999,37.4379836874626));
#59581=CARTESIAN_POINT('',(16.2455189224163,-0.674999999999999,37.4379836874626));
#59582=CARTESIAN_POINT('',(16.2455189224163,-4.901,37.4379836874626));
#59583=CARTESIAN_POINT('Origin',(16.2455189224163,-4.901,37.4379836874626));
#59584=CARTESIAN_POINT('',(15.8370850690942,-0.674999999999999,37.16288045691));
#59585=CARTESIAN_POINT('Origin',(16.0239371779885,-0.674999999999999,37.3989128474875));
#59586=CARTESIAN_POINT('Origin',(16.206085012839,-0.674999999999999,36.7191278733369));
#59587=CARTESIAN_POINT('',(16.4175158525158,-0.674999999999999,36.7960824055852));
#59588=CARTESIAN_POINT('',(16.0630582018273,-0.674999999999999,36.4542348169315));
#59589=CARTESIAN_POINT('',(16.4175158525158,-0.674999999999999,36.7960824055852));
#59590=CARTESIAN_POINT('Origin',(15.926250144497,-4.901,36.8301118652458));
#59591=CARTESIAN_POINT('',(16.4175158525158,-4.901,36.7960824055852));
#59592=CARTESIAN_POINT('Origin',(16.4175158525158,-4.901,36.7960824055852));
#59593=CARTESIAN_POINT('Origin',(16.2086533189092,-4.901,36.1420050807569));
#59594=CARTESIAN_POINT('',(16.6983647506122,-0.674999999999999,36.1938));
#59595=CARTESIAN_POINT('',(16.6983647506122,-0.674999999999999,36.1938));
#59596=CARTESIAN_POINT('',(16.6983647506122,-4.901,36.1938));
#59597=CARTESIAN_POINT('Origin',(16.6983647506122,-4.901,36.1938));
#59598=CARTESIAN_POINT('',(16.4086533189092,-0.674999999999999,35.7955949192431));
#59599=CARTESIAN_POINT('Origin',(16.5035090347607,-0.674999999999999,36.0813));
#59600=CARTESIAN_POINT('Origin',(16.9071721653514,-0.674999999999999,35.5048093046516));
#59601=CARTESIAN_POINT('',(17.0795321650532,-0.674999999999999,35.649436516831));
#59602=CARTESIAN_POINT('',(16.863369687587,-0.674999999999999,35.2069732038483));
#59603=CARTESIAN_POINT('',(17.0795321650532,-0.674999999999999,35.649436516831));
#59604=CARTESIAN_POINT('Origin',(16.6062546437124,-4.901,35.5133909810959));
#59605=CARTESIAN_POINT('',(17.0795321650532,-4.901,35.649436516831));
#59606=CARTESIAN_POINT('Origin',(17.0795321650532,-4.901,35.649436516831));
#59607=CARTESIAN_POINT('Origin',(17.1069732038483,-4.901,34.963369687587));
#59608=CARTESIAN_POINT('',(17.549436516831,-0.674999999999999,35.1795321650532));
#59609=CARTESIAN_POINT('',(17.549436516831,-0.674999999999999,35.1795321650532));
#59610=CARTESIAN_POINT('',(17.549436516831,-4.901,35.1795321650532));
#59611=CARTESIAN_POINT('Origin',(17.549436516831,-4.901,35.1795321650532));
#59612=CARTESIAN_POINT('',(17.4133909810959,-0.674999999999999,34.7062546437124));
#59613=CARTESIAN_POINT('Origin',(17.4048093046516,-0.674999999999999,35.0071721653514));
#59614=CARTESIAN_POINT('Origin',(17.9813,-0.674999999999999,34.6035090347607));
#59615=CARTESIAN_POINT('',(18.0938,-0.674999999999999,34.7983647506122));
#59616=CARTESIAN_POINT('',(18.0420050807569,-0.674999999999999,34.3086533189092));
#59617=CARTESIAN_POINT('',(18.0938,-0.674999999999999,34.7983647506122));
#59618=CARTESIAN_POINT('Origin',(17.6955949192431,-4.901,34.5086533189092));
#59619=CARTESIAN_POINT('',(18.0938,-4.901,34.7983647506122));
#59620=CARTESIAN_POINT('Origin',(18.0938,-4.901,34.7983647506122));
#59621=CARTESIAN_POINT('Origin',(18.3542348169315,-4.901,34.1630582018273));
#59622=CARTESIAN_POINT('',(18.6960824055852,-0.674999999999999,34.5175158525158));
#59623=CARTESIAN_POINT('',(18.6960824055852,-0.674999999999999,34.5175158525158));
#59624=CARTESIAN_POINT('',(18.6960824055852,-4.901,34.5175158525158));
#59625=CARTESIAN_POINT('Origin',(18.6960824055852,-4.901,34.5175158525158));
#59626=CARTESIAN_POINT('',(18.7301118652459,-0.674999999999999,34.026250144497));
#59627=CARTESIAN_POINT('Origin',(18.6191278733369,-0.674999999999999,34.306085012839));
#59628=CARTESIAN_POINT('Origin',(19.2989128474875,-0.674999999999999,34.1239371779885));
#59629=CARTESIAN_POINT('',(19.3379836874626,-0.674999999999999,34.3455189224163));
#59630=CARTESIAN_POINT('',(19.4568035581149,-0.674999999999999,33.8676257980274));
#59631=CARTESIAN_POINT('',(19.3379836874626,-0.674999999999999,34.3455189224163));
#59632=CARTESIAN_POINT('Origin',(19.06288045691,-4.901,33.9370850690941));
#59633=CARTESIAN_POINT('',(19.3379836874626,-4.901,34.3455189224163));
#59634=CARTESIAN_POINT('Origin',(19.3379836874626,-4.901,34.3455189224163));
#59635=CARTESIAN_POINT('Origin',(19.8,-4.901,33.8376));
#59636=CARTESIAN_POINT('',(20.,-0.674999999999999,34.2876));
#59637=CARTESIAN_POINT('',(20.,-0.674999999999999,34.2876));
#59638=CARTESIAN_POINT('',(20.,-4.901,34.2876));
#59639=CARTESIAN_POINT('Origin',(20.,-4.901,34.2876));
#59640=CARTESIAN_POINT('',(20.2,-0.674999999999999,33.8376));
#59641=CARTESIAN_POINT('Origin',(20.,-0.674999999999999,34.0626));
#59642=CARTESIAN_POINT('Origin',(20.7010871525125,-0.674999999999999,34.1239371779885));
#59643=CARTESIAN_POINT('',(20.6620163125374,-0.674999999999999,34.3455189224163));
#59644=CARTESIAN_POINT('',(20.93711954309,-0.674999999999999,33.9370850690941));
#59645=CARTESIAN_POINT('',(20.6620163125374,-0.674999999999999,34.3455189224163));
#59646=CARTESIAN_POINT('Origin',(20.5431964418851,-4.901,33.8676257980274));
#59647=CARTESIAN_POINT('',(20.6620163125374,-4.901,34.3455189224163));
#59648=CARTESIAN_POINT('Origin',(20.6620163125374,-4.901,34.3455189224163));
#59649=CARTESIAN_POINT('Origin',(21.2698881347541,-4.901,34.026250144497));
#59650=CARTESIAN_POINT('',(21.3039175944148,-0.674999999999999,34.5175158525158));
#59651=CARTESIAN_POINT('',(21.3039175944148,-0.674999999999999,34.5175158525158));
#59652=CARTESIAN_POINT('',(21.3039175944148,-4.901,34.5175158525158));
#59653=CARTESIAN_POINT('Origin',(21.3039175944148,-4.901,34.5175158525158));
#59654=CARTESIAN_POINT('',(21.6457651830685,-0.674999999999999,34.1630582018273));
#59655=CARTESIAN_POINT('Origin',(21.3808721266631,-0.674999999999999,34.306085012839));
#59656=CARTESIAN_POINT('Origin',(22.0187,-0.674999999999999,34.6035090347607));
#59657=CARTESIAN_POINT('',(21.9062,-0.674999999999999,34.7983647506122));
#59658=CARTESIAN_POINT('',(22.3044050807569,-0.674999999999999,34.5086533189092));
#59659=CARTESIAN_POINT('',(21.9062,-0.674999999999999,34.7983647506122));
#59660=CARTESIAN_POINT('Origin',(21.9579949192431,-4.901,34.3086533189092));
#59661=CARTESIAN_POINT('',(21.9062,-4.901,34.7983647506122));
#59662=CARTESIAN_POINT('Origin',(21.9062,-4.901,34.7983647506122));
#59663=CARTESIAN_POINT('Origin',(22.5866090189041,-4.901,34.7062546437124));
#59664=CARTESIAN_POINT('',(22.450563483169,-0.674999999999999,35.1795321650532));
#59665=CARTESIAN_POINT('',(22.450563483169,-0.674999999999999,35.1795321650532));
#59666=CARTESIAN_POINT('',(22.450563483169,-4.901,35.1795321650532));
#59667=CARTESIAN_POINT('Origin',(22.450563483169,-4.901,35.1795321650532));
#59668=CARTESIAN_POINT('',(22.8930267961517,-0.674999999999999,34.963369687587));
#59669=CARTESIAN_POINT('Origin',(22.5951906953484,-0.674999999999999,35.0071721653514));
#59670=CARTESIAN_POINT('Origin',(23.0928278346486,-0.674999999999999,35.5048093046516));
#59671=CARTESIAN_POINT('',(22.9204678349468,-0.674999999999999,35.649436516831));
#59672=CARTESIAN_POINT('',(23.3937453562876,-0.674999999999999,35.5133909810959));
#59673=CARTESIAN_POINT('',(22.9204678349468,-0.674999999999999,35.649436516831));
#59674=CARTESIAN_POINT('Origin',(23.136630312413,-4.901,35.2069732038483));
#59675=CARTESIAN_POINT('',(22.9204678349468,-4.901,35.649436516831));
#59676=CARTESIAN_POINT('Origin',(22.9204678349468,-4.901,35.649436516831));
#59677=CARTESIAN_POINT('Origin',(23.5913466810908,-4.901,35.7955949192431));
#59678=CARTESIAN_POINT('',(23.3016352493878,-0.674999999999999,36.1938));
#59679=CARTESIAN_POINT('',(23.3016352493878,-0.674999999999999,36.1938));
#59680=CARTESIAN_POINT('',(23.3016352493878,-4.901,36.1938));
#59681=CARTESIAN_POINT('Origin',(23.3016352493878,-4.901,36.1938));
#59682=CARTESIAN_POINT('',(23.7913466810908,-0.674999999999999,36.1420050807569));
#59683=CARTESIAN_POINT('Origin',(23.4964909652393,-0.674999999999999,36.0813));
#59684=CARTESIAN_POINT('Origin',(23.793914987161,-0.674999999999999,36.7191278733369));
#59685=CARTESIAN_POINT('',(23.5824841474842,-0.674999999999999,36.7960824055852));
#59686=CARTESIAN_POINT('',(24.073749855503,-0.674999999999999,36.8301118652458));
#59687=CARTESIAN_POINT('',(23.5824841474842,-0.674999999999999,36.7960824055852));
#59688=CARTESIAN_POINT('Origin',(23.9369417981727,-4.901,36.4542348169315));
#59689=CARTESIAN_POINT('',(23.5824841474842,-4.901,36.7960824055852));
#59690=CARTESIAN_POINT('Origin',(23.5824841474842,-4.901,36.7960824055852));
#59691=CARTESIAN_POINT('Origin',(24.1629149309058,-4.901,37.16288045691));
#59692=CARTESIAN_POINT('',(23.7544810775837,-0.674999999999999,37.4379836874626));
#59693=CARTESIAN_POINT('',(23.7544810775837,-0.674999999999999,37.4379836874626));
#59694=CARTESIAN_POINT('',(23.7544810775837,-4.901,37.4379836874626));
#59695=CARTESIAN_POINT('Origin',(23.7544810775837,-4.901,37.4379836874626));
#59696=CARTESIAN_POINT('',(24.2323742019726,-0.674999999999999,37.5568035581149));
#59697=CARTESIAN_POINT('Origin',(23.9760628220115,-0.674999999999999,37.3989128474875));
#59698=CARTESIAN_POINT('Origin',(24.0374,-0.674999999999999,38.1));
#59699=CARTESIAN_POINT('',(23.8124,-0.674999999999999,38.1));
#59700=CARTESIAN_POINT('',(24.2624,-0.674999999999999,38.3));
#59701=CARTESIAN_POINT('',(23.8124,-0.674999999999999,38.1));
#59702=CARTESIAN_POINT('Origin',(24.2624,-4.901,37.9));
#59703=CARTESIAN_POINT('',(23.8124,-4.901,38.1));
#59704=CARTESIAN_POINT('Origin',(23.8124,-4.901,38.1));
#59705=CARTESIAN_POINT('Origin',(20.,-4.901,38.1));
#59706=CARTESIAN_POINT('',(22.2913588808463,-4.901,38.1));
#59707=CARTESIAN_POINT('',(21.1456794404232,-4.901,36.115625));
#59708=CARTESIAN_POINT('',(22.0049390207405,-4.901,37.60390625));
#59709=CARTESIAN_POINT('',(18.8543205595768,-4.901,36.115625));
#59710=CARTESIAN_POINT('',(20.5728397202116,-4.901,36.115625));
#59711=CARTESIAN_POINT('',(17.7086411191537,-4.901,38.1));
#59712=CARTESIAN_POINT('',(18.567900699471,-4.901,36.61171875));
#59713=CARTESIAN_POINT('',(18.8543205595768,-4.901,40.084375));
#59714=CARTESIAN_POINT('',(17.9950609792595,-4.901,38.59609375));
#59715=CARTESIAN_POINT('',(21.1456794404232,-4.901,40.084375));
#59716=CARTESIAN_POINT('',(19.4271602797884,-4.901,40.084375));
#59717=CARTESIAN_POINT('',(21.432099300529,-4.901,39.58828125));
#59718=CARTESIAN_POINT('Origin',(20.,-2.501,38.1));
#59719=CARTESIAN_POINT('',(22.2913588808463,-2.501,38.1));
#59720=CARTESIAN_POINT('',(21.1456794404232,-2.501,36.115625));
#59721=CARTESIAN_POINT('',(21.1456794404232,-2.501,36.115625));
#59722=CARTESIAN_POINT('Origin',(20.,-2.501,38.1));
#59723=CARTESIAN_POINT('Origin',(20.,-2.501,38.1));
#59724=CARTESIAN_POINT('',(18.8543205595768,-2.501,36.115625));
#59725=CARTESIAN_POINT('',(18.8543205595768,-2.501,36.115625));
#59726=CARTESIAN_POINT('Origin',(20.,-2.501,38.1));
#59727=CARTESIAN_POINT('Origin',(20.,-2.501,38.1));
#59728=CARTESIAN_POINT('',(17.7086411191537,-2.501,38.1));
#59729=CARTESIAN_POINT('',(17.7086411191537,-2.501,38.1));
#59730=CARTESIAN_POINT('Origin',(20.,-2.501,38.1));
#59731=CARTESIAN_POINT('Origin',(20.,-2.501,38.1));
#59732=CARTESIAN_POINT('',(18.8543205595768,-2.501,40.084375));
#59733=CARTESIAN_POINT('',(18.8543205595768,-2.501,40.084375));
#59734=CARTESIAN_POINT('Origin',(20.,-2.501,38.1));
#59735=CARTESIAN_POINT('Origin',(20.,-2.501,38.1));
#59736=CARTESIAN_POINT('',(21.1456794404232,-2.501,40.084375));
#59737=CARTESIAN_POINT('',(21.1456794404232,-2.501,40.084375));
#59738=CARTESIAN_POINT('Origin',(20.,-2.501,38.1));
#59739=CARTESIAN_POINT('Origin',(20.,-2.501,38.1));
#59740=CARTESIAN_POINT('',(22.2913588808463,-2.501,38.1));
#59741=CARTESIAN_POINT('Origin',(20.,-2.501,38.1));
#59742=CARTESIAN_POINT('Origin',(20.,-1.81260634222019,38.1));
#59743=CARTESIAN_POINT('',(20.,-1.12421268444038,38.1));
#59744=CARTESIAN_POINT('',(18.8543205595768,-1.81260634222019,38.1));
#59745=CARTESIAN_POINT('Origin',(22.2913588808463,-4.901,38.1));
#59746=CARTESIAN_POINT('',(22.2913588808463,-4.901,38.1));
#59747=CARTESIAN_POINT('',(21.1456794404232,-4.901,36.115625));
#59748=CARTESIAN_POINT('Origin',(21.1456794404232,-4.901,40.084375));
#59749=CARTESIAN_POINT('',(21.1456794404232,-4.901,40.084375));
#59750=CARTESIAN_POINT('Origin',(18.8543205595768,-4.901,40.084375));
#59751=CARTESIAN_POINT('',(18.8543205595768,-4.901,40.084375));
#59752=CARTESIAN_POINT('Origin',(17.7086411191537,-4.901,38.1));
#59753=CARTESIAN_POINT('',(17.7086411191537,-4.901,38.1));
#59754=CARTESIAN_POINT('Origin',(18.8543205595768,-4.901,36.115625));
#59755=CARTESIAN_POINT('',(18.8543205595768,-4.901,36.115625));
#59756=CARTESIAN_POINT('Origin',(21.1456794404232,-4.901,36.115625));
#59757=CARTESIAN_POINT('',(0.,0.,0.));
#59758=CARTESIAN_POINT('Origin',(39.2,8.05522481984854,-9.525));
#59759=CARTESIAN_POINT('',(36.958019684865,4.68963520761331,-8.65357747851728));
#59760=CARTESIAN_POINT('',(36.958019684865,4.95526326543997,-8.65357747851728));
#59761=CARTESIAN_POINT('',(36.958019684865,8.05522481984854,-8.65357747851728));
#59762=CARTESIAN_POINT('',(37.7316252379159,5.69997297025342,-11.430184637371));
#59763=CARTESIAN_POINT('Ctrl Pts',(37.7316252379159,5.69997297025341,-11.430184637371));
#59764=CARTESIAN_POINT('Ctrl Pts',(37.7946541587511,5.69324594371103,-11.4787626464628));
#59765=CARTESIAN_POINT('Ctrl Pts',(37.860217046903,5.68651891716864,-11.5243024976679));
#59766=CARTESIAN_POINT('Ctrl Pts',(37.9279877925796,5.67979189062625,-11.5665283217662));
#59767=CARTESIAN_POINT('Ctrl Pts',(37.9956622585872,5.67307442094918,-11.6086941570253));
#59768=CARTESIAN_POINT('Ctrl Pts',(38.0655379578993,5.6663569512721,-11.6475550673986));
#59769=CARTESIAN_POINT('Ctrl Pts',(38.1372568992143,5.65963948159503,-11.6828762814704));
#59770=CARTESIAN_POINT('Ctrl Pts',(38.20889476234,5.6529296060105,-11.718157564946));
#59771=CARTESIAN_POINT('Ctrl Pts',(38.2823713070823,5.64621973042597,-11.7499068967576));
#59772=CARTESIAN_POINT('Ctrl Pts',(38.3573021640367,5.63950985484144,-11.7779343758003));
#59773=CARTESIAN_POINT('Ctrl Pts',(38.4321873033431,5.63280407316085,-11.8059447544057));
#59774=CARTESIAN_POINT('Ctrl Pts',(38.5085245543671,5.62609829148025,-11.830237622806));
#59775=CARTESIAN_POINT('Ctrl Pts',(38.5859088393635,5.61939250979966,-11.8506708689813));
#59776=CARTESIAN_POINT('Ctrl Pts',(38.6632702320777,5.61268871186352,-11.8710980704714));
#59777=CARTESIAN_POINT('Ctrl Pts',(38.7416775892241,5.60598491392738,-11.8876677971188));
#59778=CARTESIAN_POINT('Ctrl Pts',(38.8207113660228,5.59928111599125,-11.9002879986511));
#59779=CARTESIAN_POINT('Ctrl Pts',(38.8997466029625,5.59257719420313,-11.9129084333402));
#59780=CARTESIAN_POINT('Ctrl Pts',(38.9794078178049,5.58587327241501,-11.9215791257643));
#59781=CARTESIAN_POINT('Ctrl Pts',(39.0592674844931,5.57916935062689,-11.9262595243911));
#59782=CARTESIAN_POINT('Ctrl Pts',(39.1392051954725,5.57245887731099,-11.9309444970214));
#59783=CARTESIAN_POINT('Ctrl Pts',(39.2193412750867,5.5657484039951,-11.9316313621234));
#59784=CARTESIAN_POINT('Ctrl Pts',(39.2992460045512,5.5590379306792,-11.9283316822654));
#59785=CARTESIAN_POINT('Ctrl Pts',(39.3791919454358,5.55232399639,-11.9250303005745));
#59786=CARTESIAN_POINT('Ctrl Pts',(39.4589058300058,5.5456100621008,-11.9177383230545));
#59787=CARTESIAN_POINT('Ctrl Pts',(39.537963392915,5.5388961278116,-11.9065191977915));
#59788=CARTESIAN_POINT('Ctrl Pts',(39.6171534627766,5.53217094041848,-11.8952812683553));
#59789=CARTESIAN_POINT('Ctrl Pts',(39.6956845522583,5.52544575302536,-11.880103136358));
#59790=CARTESIAN_POINT('Ctrl Pts',(39.7731433517624,5.51872056563224,-11.8610992364903));
#59791=CARTESIAN_POINT('Ctrl Pts',(39.8253287138061,5.51418968804095,-11.8482959733209));
#59792=CARTESIAN_POINT('Ctrl Pts',(39.8770276482391,5.50965881044965,-11.8337572644404));
#59793=CARTESIAN_POINT('Ctrl Pts',(39.9281186537803,5.50512793285836,-11.8175305167908));
#59794=CARTESIAN_POINT('Ctrl Pts',(40.0043885499032,5.49836412855323,-11.7933068331006));
#59795=CARTESIAN_POINT('Ctrl Pts',(40.0795843205461,5.49160032424809,-11.765229718215));
#59796=CARTESIAN_POINT('Ctrl Pts',(40.1532902141198,5.48483651994295,-11.733413618882));
#59797=CARTESIAN_POINT('Ctrl Pts',(40.2268937455063,5.47808210915803,-11.7016417055069));
#59798=CARTESIAN_POINT('Ctrl Pts',(40.2990110865368,5.47132769837312,-11.6661413046116));
#59799=CARTESIAN_POINT('Ctrl Pts',(40.3692424293285,5.4645732875882,-11.627076374887));
#59800=CARTESIAN_POINT('Ctrl Pts',(40.4393964787615,5.45782631039455,-11.5880544382122));
#59801=CARTESIAN_POINT('Ctrl Pts',(40.5076682512703,5.45107933320089,-11.5454759943738));
#59802=CARTESIAN_POINT('Ctrl Pts',(40.5736800233579,5.44433235600723,-11.4995521360115));
#59803=CARTESIAN_POINT('Ctrl Pts',(40.6396521803153,5.4375894278244,-11.4536558375763));
#59804=CARTESIAN_POINT('Ctrl Pts',(40.7033666490523,5.43084649964157,-11.404418375072));
#59805=CARTESIAN_POINT('Ctrl Pts',(40.764473347711,5.42410357145874,-11.3520949862287));
#59806=CARTESIAN_POINT('Ctrl Pts',(40.8255620129165,5.41736263320962,-11.2997870387593));
#59807=CARTESIAN_POINT('Ctrl Pts',(40.8840440839884,5.4106216949605,-11.2443952757339));
#59808=CARTESIAN_POINT('Ctrl Pts',(40.9396024696636,5.40388075671138,-11.1862152756161));
#59809=CARTESIAN_POINT('Ctrl Pts',(40.995161404406,5.39713975184354,-11.1280347005224));
#59810=CARTESIAN_POINT('Ctrl Pts',(41.0477962765987,5.3903987469757,-11.0670661705574));
#59811=CARTESIAN_POINT('Ctrl Pts',(41.0972277989088,5.38365774210786,-11.0036411408613));
#59812=CARTESIAN_POINT('Ctrl Pts',(41.1467088547655,5.37690998232205,-10.9401525552292));
#59813=CARTESIAN_POINT('Ctrl Pts',(41.1929798626493,5.37016222253623,-10.8742029201246));
#59814=CARTESIAN_POINT('Ctrl Pts',(41.2358030610351,5.36341446275041,-10.8061552759443));
#59815=CARTESIAN_POINT('Ctrl Pts',(41.2786472428939,5.35666339654565,-10.7380742882504));
#59816=CARTESIAN_POINT('Ctrl Pts',(41.3180400216499,5.34991233034089,-10.6678936488724));
#59817=CARTESIAN_POINT('Ctrl Pts',(41.3537893422957,5.34316126413612,-10.5960015935625));
#59818=CARTESIAN_POINT('Ctrl Pts',(41.3896024134546,5.33639815899114,-10.5239813356651));
#59819=CARTESIAN_POINT('Ctrl Pts',(41.4217588576558,5.32963505384615,-10.4502439903742));
#59820=CARTESIAN_POINT('Ctrl Pts',(41.4501146492602,5.32287194870117,-10.3751982178202));
#59821=CARTESIAN_POINT('Ctrl Pts',(41.4757598513906,5.31675534293357,-10.307326227751));
#59822=CARTESIAN_POINT('Ctrl Pts',(41.4982968666121,5.31063873716598,-10.2383844746568));
#59823=CARTESIAN_POINT('Ctrl Pts',(41.5176549374898,5.30452213139838,-10.1686835675463));
#59824=CARTESIAN_POINT('Ctrl Pts',(41.539001577617,5.29777719369539,-10.0918225936393));
#59825=CARTESIAN_POINT('Ctrl Pts',(41.5565610866446,5.29103225599239,-10.0137529010872));
#59826=CARTESIAN_POINT('Ctrl Pts',(41.5702003061424,5.28428731828939,-9.93488224304359));
#59827=CARTESIAN_POINT('Ctrl Pts',(41.5838198456394,5.27755211284268,-9.85612538730496));
#59828=CARTESIAN_POINT('Ctrl Pts',(41.5935302500593,5.27081690739596,-9.77657031808186));
#59829=CARTESIAN_POINT('Ctrl Pts',(41.5992484348811,5.26408170194925,-9.69663884210919));
#59830=CARTESIAN_POINT('Ctrl Pts',(41.6049599526811,5.25735434930243,-9.61680056090113));
#59831=CARTESIAN_POINT('Ctrl Pts',(41.6066884678706,5.25062699665562,-9.53658720908332));
#59832=CARTESIAN_POINT('Ctrl Pts',(41.6044023885841,5.2438996440088,-9.45642815321961));
#59833=CARTESIAN_POINT('Ctrl Pts',(41.6021177687439,5.23717658614268,-9.37632027135907));
#59834=CARTESIAN_POINT('Ctrl Pts',(41.5958236548841,5.23045352827655,-9.29626708279406));
#59835=CARTESIAN_POINT('Ctrl Pts',(41.5855405196536,5.22373047041043,-9.21669921587696));
#59836=CARTESIAN_POINT('Ctrl Pts',(41.5752607609415,5.21700962009372,-9.13715747546372));
#59837=CARTESIAN_POINT('Ctrl Pts',(41.5609946417497,5.210288769777,-9.0581012036375));
#59838=CARTESIAN_POINT('Ctrl Pts',(41.542814470651,5.20356791946028,-8.97995568940831));
#59839=CARTESIAN_POINT('Ctrl Pts',(41.5246346324385,5.19684719220502,-8.90181160605471));
#59840=CARTESIAN_POINT('Ctrl Pts',(41.502540992042,5.19012646494976,-8.82457870228018));
#59841=CARTESIAN_POINT('Ctrl Pts',(41.476656608748,5.18340573769449,-8.74867041133033));
#59842=CARTESIAN_POINT('Ctrl Pts',(41.4507468145623,5.17667841265128,-8.67268760064649));
#59843=CARTESIAN_POINT('Ctrl Pts',(41.4210389948421,5.16995108760807,-8.59803244405444));
#59844=CARTESIAN_POINT('Ctrl Pts',(41.3877054086384,5.16322376256486,-8.52510101039437));
#59845=CARTESIAN_POINT('Ctrl Pts',(41.3543560238464,5.15649324907867,-8.45213501058568));
#59846=CARTESIAN_POINT('Ctrl Pts',(41.3173776648435,5.14976273559249,-8.38089477681323));
#59847=CARTESIAN_POINT('Ctrl Pts',(41.276988728776,5.1430322221063,-8.31175197715497));
#59848=CARTESIAN_POINT('Ctrl Pts',(41.2365273114332,5.13628963015881,-8.24248509504269));
#59849=CARTESIAN_POINT('Ctrl Pts',(41.1926433434954,5.12954703821132,-8.17532356061939));
#59850=CARTESIAN_POINT('Ctrl Pts',(41.1455986367173,5.12280444626383,-8.11061006465549));
#59851=CARTESIAN_POINT('Ctrl Pts',(41.1016696402205,5.11650840748868,-8.05018246010271));
#59852=CARTESIAN_POINT('Ctrl Pts',(41.0549853224597,5.11021236871354,-7.99188928961594));
#59853=CARTESIAN_POINT('Ctrl Pts',(41.0057884671268,5.1039163299384,-7.93598113403525));
#59854=CARTESIAN_POINT('Ctrl Pts',(40.9530101637372,5.09716195016395,-7.87600295906406));
#59855=CARTESIAN_POINT('Ctrl Pts',(40.897142926318,5.0904075703895,-7.81854634138377));
#59856=CARTESIAN_POINT('Ctrl Pts',(40.8384569591934,5.08365319061505,-7.76394584487846));
#59857=CARTESIAN_POINT('Ctrl Pts',(40.7798545226603,5.07690842467788,-7.7094230639157));
#59858=CARTESIAN_POINT('Ctrl Pts',(40.7184416631837,5.07016365874072,-7.65774864502113));
#59859=CARTESIAN_POINT('Ctrl Pts',(40.6545276273748,5.06341889280355,-7.60922278810829));
#59860=CARTESIAN_POINT('Ctrl Pts',(40.5906867420979,5.05668184634788,-7.56075246973574));
#59861=CARTESIAN_POINT('Ctrl Pts',(40.5243507391328,5.04994479989221,-7.51542383191998));
#59862=CARTESIAN_POINT('Ctrl Pts',(40.4558632505349,5.04320775343655,-7.47349800381381));
#59863=CARTESIAN_POINT('Ctrl Pts',(40.3874186421023,5.03647492506029,-7.43159842555964));
#59864=CARTESIAN_POINT('Ctrl Pts',(40.3168256185414,5.02974209668404,-7.39309767046601));
#59865=CARTESIAN_POINT('Ctrl Pts',(40.2444572366038,5.02300926830778,-7.35821389488813));
#59866=CARTESIAN_POINT('Ctrl Pts',(40.1721119045171,5.01627858438585,-7.32334123004399));
#59867=CARTESIAN_POINT('Ctrl Pts',(40.0979927566051,5.00954790046392,-7.29208345902033));
#59868=CARTESIAN_POINT('Ctrl Pts',(40.0224966321684,5.002817216542,-7.26461237074884));
#59869=CARTESIAN_POINT('Ctrl Pts',(39.947001332213,4.99608660612481,-7.23714158248478));
#59870=CARTESIAN_POINT('Ctrl Pts',(39.8701295240859,4.98935599570762,-7.21345755282289));
#59871=CARTESIAN_POINT('Ctrl Pts',(39.7922957941855,4.98262538529043,-7.1936830681801));
#59872=CARTESIAN_POINT('Ctrl Pts',(39.7143856592388,4.9758881678071,-7.17388917202488));
#59873=CARTESIAN_POINT('Ctrl Pts',(39.6355121690381,4.96915095032378,-7.15801260222684));
#59874=CARTESIAN_POINT('Ctrl Pts',(39.5561022097792,4.96241373284045,-7.14612544244335));
#59875=CARTESIAN_POINT('Ctrl Pts',(39.4766544235731,4.95567330608246,-7.13423262020932));
#59876=CARTESIAN_POINT('Ctrl Pts',(39.3966701236061,4.94893287932447,-7.12633304002858));
#59877=CARTESIAN_POINT('Ctrl Pts',(39.3165809532889,4.94219245256649,-7.12244681105074));
#59878=CARTESIAN_POINT('Ctrl Pts',(39.2363492234279,4.93544002777981,-7.11855366454551));
#59879=CARTESIAN_POINT('Ctrl Pts',(39.1560127174399,4.92868760299314,-7.11868814320593));
#59880=CARTESIAN_POINT('Ctrl Pts',(39.0760025199875,4.92193517820646,-7.12281816480298));
#59881=CARTESIAN_POINT('Ctrl Pts',(39.0024407033413,4.91572696163044,-7.12661532942874));
#59882=CARTESIAN_POINT('Ctrl Pts',(38.9291549525295,4.90951874505443,-7.13378931389573));
#59883=CARTESIAN_POINT('Ctrl Pts',(38.8564731110546,4.90331052847841,-7.14427695416467));
#59884=CARTESIAN_POINT('Ctrl Pts',(38.7774012967453,4.89655650383719,-7.15568663679048));
#59885=CARTESIAN_POINT('Ctrl Pts',(38.6987526508042,4.88980247919597,-7.1710609960329));
#59886=CARTESIAN_POINT('Ctrl Pts',(38.6209549970016,4.88304845455474,-7.19035659491593));
#59887=CARTESIAN_POINT('Ctrl Pts',(38.5432678452317,4.87630402317778,-7.20962478676552));
#59888=CARTESIAN_POINT('Ctrl Pts',(38.4664297337037,4.86955959180082,-7.23280304510437));
#59889=CARTESIAN_POINT('Ctrl Pts',(38.3908610433311,4.86281516042386,-7.25979645656273));
#59890=CARTESIAN_POINT('Ctrl Pts',(38.3153784780905,4.85607841563033,-7.28675910381023));
#59891=CARTESIAN_POINT('Ctrl Pts',(38.2411628955007,4.84934167083679,-7.31752810667642));
#59892=CARTESIAN_POINT('Ctrl Pts',(38.1686207484526,4.84260492604325,-7.35195840263526));
#59893=CARTESIAN_POINT('Ctrl Pts',(38.0961238045776,4.8358723791161,-7.38636724405086));
#59894=CARTESIAN_POINT('Ctrl Pts',(38.0252986462831,4.82913983218896,-7.42443265030117));
#59895=CARTESIAN_POINT('Ctrl Pts',(37.9565318165698,4.82240728526182,-7.46596143280491));
#59896=CARTESIAN_POINT('Ctrl Pts',(37.8877866794154,4.81567686212272,-7.50747711501646));
#59897=CARTESIAN_POINT('Ctrl Pts',(37.8210989800708,4.80894643898362,-7.55245376294581));
#59898=CARTESIAN_POINT('Ctrl Pts',(37.7568294249252,4.80221601584453,-7.60065293264489));
#59899=CARTESIAN_POINT('Ctrl Pts',(37.6925603698258,4.79548564507117,-7.64885172733259));
#59900=CARTESIAN_POINT('Ctrl Pts',(37.6307097935878,4.78875527429782,-7.70027271314879));
#59901=CARTESIAN_POINT('Ctrl Pts',(37.5716070605675,4.78202490352446,-7.7546358060539));
#59902=CARTESIAN_POINT('Ctrl Pts',(37.5124459981869,4.77528789044877,-7.80905255069848));
#59903=CARTESIAN_POINT('Ctrl Pts',(37.4560385400727,4.76855087737308,-7.8664168862985));
#59904=CARTESIAN_POINT('Ctrl Pts',(37.4026783093107,4.76181386429738,-7.92641072048584));
#59905=CARTESIAN_POINT('Ctrl Pts',(37.3492925094672,4.7550736229891,-7.98643330243549));
#59906=CARTESIAN_POINT('Ctrl Pts',(37.2989571383783,4.74833338168082,-8.04908752939983));
#59907=CARTESIAN_POINT('Ctrl Pts',(37.2519248885662,4.74159314037254,-8.11402292555401));
#59908=CARTESIAN_POINT('Ctrl Pts',(37.2048086772705,4.73484086645552,-8.17907424370259));
#59909=CARTESIAN_POINT('Ctrl Pts',(37.1610076247398,4.72808859253849,-8.24641447659392));
#59910=CARTESIAN_POINT('Ctrl Pts',(37.1207304078408,4.72133631862147,-8.31566509703801));
#59911=CARTESIAN_POINT('Ctrl Pts',(37.0836846824358,4.71512578808712,-8.37935965357939));
#59912=CARTESIAN_POINT('Ctrl Pts',(37.0496196278822,4.70891525755277,-8.44466980386474));
#59913=CARTESIAN_POINT('Ctrl Pts',(37.0186616191027,4.70270472701843,-8.51128612891783));
#59914=CARTESIAN_POINT('Ctrl Pts',(36.9969454766975,4.69834822055006,-8.55801554267529));
#59915=CARTESIAN_POINT('Ctrl Pts',(36.9767154860701,4.69399171408168,-8.605477254752));
#59916=CARTESIAN_POINT('Ctrl Pts',(36.958019684865,4.68963520761331,-8.65357747851728));
#59917=CARTESIAN_POINT('',(40.6683886799113,5.7,-11.4301739104629));
#59918=CARTESIAN_POINT('Origin',(39.2,5.7,-9.525));
#59919=CARTESIAN_POINT('Ctrl Pts',(40.6683886799113,5.7,-11.4301739104629));
#59920=CARTESIAN_POINT('Ctrl Pts',(40.7334765795775,5.69309458976092,-11.3800082355372));
#59921=CARTESIAN_POINT('Ctrl Pts',(40.7960377610544,5.68618917952184,-11.3264676545935));
#59922=CARTESIAN_POINT('Ctrl Pts',(40.8557196162198,5.67928376928276,-11.2698339453555));
#59923=CARTESIAN_POINT('Ctrl Pts',(40.9153649291418,5.67238258711571,-11.2132349120301));
#59924=CARTESIAN_POINT('Ctrl Pts',(40.9721341083313,5.66548140494865,-11.1535468182329));
#59925=CARTESIAN_POINT('Ctrl Pts',(41.0257091482293,5.6585802227816,-11.0910903711063));
#59926=CARTESIAN_POINT('Ctrl Pts',(41.0792782843711,5.65167980109734,-11.0286408064316));
#59927=CARTESIAN_POINT('Ctrl Pts',(41.1296536902672,5.64477937941309,-10.9634238192556));
#59928=CARTESIAN_POINT('Ctrl Pts',(41.1765561357657,5.63787895772883,-10.895794946944));
#59929=CARTESIAN_POINT('Ctrl Pts',(41.2234574242939,5.63097870626133,-10.8281677428735));
#59930=CARTESIAN_POINT('Ctrl Pts',(41.2668856739803,5.62407845479383,-10.7581291299302));
#59931=CARTESIAN_POINT('Ctrl Pts',(41.3066044364979,5.61717820332633,-10.6860644652763));
#59932=CARTESIAN_POINT('Ctrl Pts',(41.3463319158957,5.61027643749479,-10.6139839849471));
#59933=CARTESIAN_POINT('Ctrl Pts',(41.3823480783771,5.60337467166326,-10.5398769502741));
#59934=CARTESIAN_POINT('Ctrl Pts',(41.4144624914224,5.59647290583172,-10.4641532454735));
#59935=CARTESIAN_POINT('Ctrl Pts',(41.4465917951318,5.58956793982096,-10.3883944294517));
#59936=CARTESIAN_POINT('Ctrl Pts',(41.474815580778,5.5826629738102,-10.3110178534221));
#59937=CARTESIAN_POINT('Ctrl Pts',(41.4989919990329,5.57575800779944,-10.2324522830431));
#59938=CARTESIAN_POINT('Ctrl Pts',(41.5232040150041,5.56884287481443,-10.1537710315545));
#59939=CARTESIAN_POINT('Ctrl Pts',(41.5433566342283,5.56192774182942,-10.0738977070194));
#59940=CARTESIAN_POINT('Ctrl Pts',(41.5593582631339,5.55501260884441,-9.99327505868025));
#59941=CARTESIAN_POINT('Ctrl Pts',(41.5753722850231,5.54809212020899,-9.91258996950013));
#59942=CARTESIAN_POINT('Ctrl Pts',(41.5872288468328,5.54117163157358,-9.83115483134809));
#59943=CARTESIAN_POINT('Ctrl Pts',(41.5948881055281,5.53425114293816,-9.74941904197305));
#59944=CARTESIAN_POINT('Ctrl Pts',(41.6025620627445,5.52731737352031,-9.66752639731028));
#59945=CARTESIAN_POINT('Ctrl Pts',(41.6060226033772,5.52038360410246,-9.58533238461483));
#59946=CARTESIAN_POINT('Ctrl Pts',(41.6052820075671,5.51344983468461,-9.50328805688157));
#59947=CARTESIAN_POINT('Ctrl Pts',(41.6047815801368,5.50876462263641,-9.44784994672573));
#59948=CARTESIAN_POINT('Ctrl Pts',(41.6023640754666,5.50407941058821,-9.39248015451929));
#59949=CARTESIAN_POINT('Ctrl Pts',(41.5980466400686,5.49939419854002,-9.33731607299534));
#59950=CARTESIAN_POINT('Ctrl Pts',(41.5918819269685,5.49270435018622,-9.25854923465905));
#59951=CARTESIAN_POINT('Ctrl Pts',(41.5818184205766,5.48601450183243,-9.17991116903287));
#59952=CARTESIAN_POINT('Ctrl Pts',(41.5678629811776,5.47932465347864,-9.10182409476818));
#59953=CARTESIAN_POINT('Ctrl Pts',(41.5539295969193,5.47264537774405,-9.0238604291156));
#59954=CARTESIAN_POINT('Ctrl Pts',(41.5361165702112,5.46596610200945,-8.94644649046866));
#59955=CARTESIAN_POINT('Ctrl Pts',(41.5144826692387,5.45928682627486,-8.87000158916707));
#59956=CARTESIAN_POINT('Ctrl Pts',(41.4928223421975,5.45259939172508,-8.7934633095043));
#59957=CARTESIAN_POINT('Ctrl Pts',(41.4673318464465,5.44591195717529,-8.71789691467541));
#59958=CARTESIAN_POINT('Ctrl Pts',(41.4381219784085,5.43922452262551,-8.64371516853804));
#59959=CARTESIAN_POINT('Ctrl Pts',(41.4090079777065,5.43255903636162,-8.56977688828589));
#59960=CARTESIAN_POINT('Ctrl Pts',(41.3761991319561,5.42589355009773,-8.49721463561187));
#59961=CARTESIAN_POINT('Ctrl Pts',(41.3398550403091,5.41922806383384,-8.42642212344152));
#59962=CARTESIAN_POINT('Ctrl Pts',(41.3035258815354,5.41256531625065,-8.35565869813428));
#59963=CARTESIAN_POINT('Ctrl Pts',(41.2636645767925,5.40590256866746,-8.28666399368246));
#59964=CARTESIAN_POINT('Ctrl Pts',(41.2204778808029,5.39923982108427,-8.21980956271262));
#59965=CARTESIAN_POINT('Ctrl Pts',(41.1772949733639,5.39257765799027,-8.15296099654437));
#59966=CARTESIAN_POINT('Ctrl Pts',(41.1307875134901,5.38591549489627,-8.08825273057752));
#59967=CARTESIAN_POINT('Ctrl Pts',(41.0812061733673,5.37925333180228,-8.02602825987783));
#59968=CARTESIAN_POINT('Ctrl Pts',(41.031302970757,5.37254792057542,-7.96339985247802));
#59969=CARTESIAN_POINT('Ctrl Pts',(40.9782861245363,5.36584250934857,-7.90328799802043));
#59970=CARTESIAN_POINT('Ctrl Pts',(40.9224518379415,5.35913709812172,-7.84600845434768));
#59971=CARTESIAN_POINT('Ctrl Pts',(40.8669012679019,5.35246575979685,-7.78901997116489));
#59972=CARTESIAN_POINT('Ctrl Pts',(40.8085622135957,5.34579442147197,-7.73483536801589));
#59973=CARTESIAN_POINT('Ctrl Pts',(40.7477613083866,5.3391230831471,-7.68372656113724));
#59974=CARTESIAN_POINT('Ctrl Pts',(40.6864946053458,5.33240063546926,-7.63222620792655));
#59975=CARTESIAN_POINT('Ctrl Pts',(40.6227285632886,5.32567818779141,-7.58384927473834));
#59976=CARTESIAN_POINT('Ctrl Pts',(40.5568272156725,5.31895574011357,-7.53882960166794));
#59977=CARTESIAN_POINT('Ctrl Pts',(40.4909258680564,5.31223329243572,-7.49380992859754));
#59978=CARTESIAN_POINT('Ctrl Pts',(40.422889666234,5.30551084475788,-7.45214771149533));
#59979=CARTESIAN_POINT('Ctrl Pts',(40.3531060649499,5.29878839708003,-7.41402881417679));
#59980=CARTESIAN_POINT('Ctrl Pts',(40.2829266254486,5.29202781720989,-7.37569369247206));
#59981=CARTESIAN_POINT('Ctrl Pts',(40.2107049199298,5.28526723733974,-7.3407918350856));
#59982=CARTESIAN_POINT('Ctrl Pts',(40.1368100741077,5.2785066574696,-7.30954523191055));
#59983=CARTESIAN_POINT('Ctrl Pts',(40.0630205214242,5.27175571078381,-7.278343152178));
#59984=CARTESIAN_POINT('Ctrl Pts',(39.9875629885923,5.26500476409803,-7.25078616139168));
#59985=CARTESIAN_POINT('Ctrl Pts',(39.9108314922945,5.25825381741224,-7.22705058063446));
#59986=CARTESIAN_POINT('Ctrl Pts',(39.8341884282351,5.25151065112115,-7.20334235488317));
#59987=CARTESIAN_POINT('Ctrl Pts',(39.756274761019,5.24476748483006,-7.18344692237463));
#59988=CARTESIAN_POINT('Ctrl Pts',(39.6775034161206,5.23802431853897,-7.16749211411857));
#59989=CARTESIAN_POINT('Ctrl Pts',(39.598781818412,5.23128541082152,-7.15154738194888));
#59990=CARTESIAN_POINT('Ctrl Pts',(39.5192040729623,5.22454650310408,-7.13953842555161));
#59991=CARTESIAN_POINT('Ctrl Pts',(39.4391960348999,5.21780759538663,-7.13154262597218));
#59992=CARTESIAN_POINT('Ctrl Pts',(39.3592140472713,5.21107088184208,-7.12354942980676));
#59993=CARTESIAN_POINT('Ctrl Pts',(39.2788025077089,5.20433416829753,-7.11956684145869));
#59994=CARTESIAN_POINT('Ctrl Pts',(39.1983937510459,5.19759745475299,-7.11962053630528));
#59995=CARTESIAN_POINT('Ctrl Pts',(39.1179865757866,5.19086087369978,-7.11967423009585));
#59996=CARTESIAN_POINT('Ctrl Pts',(39.037582648378,5.18412429264657,-7.1237640476089));
#59997=CARTESIAN_POINT('Ctrl Pts',(38.9576142242073,5.17738771159336,-7.13186354753989));
#59998=CARTESIAN_POINT('Ctrl Pts',(38.8775689910583,5.17064466011245,-7.13997082697036));
#59999=CARTESIAN_POINT('Ctrl Pts',(38.7979605605151,5.16390160863154,-7.15209543533618));
#60000=CARTESIAN_POINT('Ctrl Pts',(38.7192154094158,5.15715855715063,-7.16815908006993));
#60001=CARTESIAN_POINT('Ctrl Pts',(38.640433549353,5.15041236223259,-7.1842302132616));
#60002=CARTESIAN_POINT('Ctrl Pts',(38.5625162217254,5.14366616731455,-7.20424392602886));
#60003=CARTESIAN_POINT('Ctrl Pts',(38.4858766297247,5.13691997239651,-7.22807145160616));
#60004=CARTESIAN_POINT('Ctrl Pts',(38.4091027859999,5.13016195997951,-7.2519407165287));
#60005=CARTESIAN_POINT('Ctrl Pts',(38.3336115882086,5.12340394756252,-7.27963698357706));
#60006=CARTESIAN_POINT('Ctrl Pts',(38.2597978904236,5.11664593514552,-7.31098262483148));
#60007=CARTESIAN_POINT('Ctrl Pts',(38.192576579396,5.11049148863704,-7.33952875059612));
#60008=CARTESIAN_POINT('Ctrl Pts',(38.1267464800312,5.10433704212855,-7.37110078603114));
#60009=CARTESIAN_POINT('Ctrl Pts',(38.0625866948648,5.09818259562006,-7.40553216167326));
#60010=CARTESIAN_POINT('Ctrl Pts',(37.9920899471686,5.09142028396965,-7.44336427091712));
#60011=CARTESIAN_POINT('Ctrl Pts',(37.9233570740887,5.08465797231923,-7.48478487517366));
#60012=CARTESIAN_POINT('Ctrl Pts',(37.856775424105,5.07789566066882,-7.52960513103006));
#60013=CARTESIAN_POINT('Ctrl Pts',(37.7902793533566,5.07114204080451,-7.57436777817255));
#60014=CARTESIAN_POINT('Ctrl Pts',(37.7259293984589,5.0643884209402,-7.62252114485889));
#60015=CARTESIAN_POINT('Ctrl Pts',(37.6640882624756,5.05763480107589,-7.67383061851849));
#60016=CARTESIAN_POINT('Ctrl Pts',(37.6023077439674,5.05088780119645,-7.7250897979735));
#60017=CARTESIAN_POINT('Ctrl Pts',(37.5430315162217,5.04414080131701,-7.77949864537018));
#60018=CARTESIAN_POINT('Ctrl Pts',(37.4865920384997,5.03739380143757,-7.83678019740689));
#60019=CARTESIAN_POINT('Ctrl Pts',(37.4293393750993,5.03054959010443,-7.89488706781365));
#60020=CARTESIAN_POINT('Ctrl Pts',(37.3750062529722,5.0237053787713,-7.95594979801237));
#60021=CARTESIAN_POINT('Ctrl Pts',(37.3239031354747,5.01686116743817,-8.01963841575571));
#60022=CARTESIAN_POINT('Ctrl Pts',(37.2735703380596,5.0101201246336,-8.08236700163276));
#60023=CARTESIAN_POINT('Ctrl Pts',(37.2263711121376,5.00337908182904,-8.14764246220205));
#60024=CARTESIAN_POINT('Ctrl Pts',(37.1825621609754,4.99663803902448,-8.2151154592592));
#60025=CARTESIAN_POINT('Ctrl Pts',(37.1377474963441,4.98974224342706,-8.2841374206294));
#60026=CARTESIAN_POINT('Ctrl Pts',(37.0964810017983,4.98284644782964,-8.35545866392911));
#60027=CARTESIAN_POINT('Ctrl Pts',(37.05898999333,4.97595065223222,-8.42867473086733));
#60028=CARTESIAN_POINT('Ctrl Pts',(37.0214989848616,4.9690548566348,-8.50189079780555));
#60029=CARTESIAN_POINT('Ctrl Pts',(36.9877836755813,4.96215906103738,-8.57700121425903));
#60030=CARTESIAN_POINT('Ctrl Pts',(36.958019684865,4.95526326543996,-8.65357747851728));
#60031=CARTESIAN_POINT('Origin',(39.2,8.05522481984854,-9.525));
#60032=CARTESIAN_POINT('',(36.9580196850403,3.41777315288062,-8.65357747806631));
#60033=CARTESIAN_POINT('',(36.958019684865,3.68510631127449,-8.65357747851727));
#60034=CARTESIAN_POINT('',(36.958019684865,8.05522481984854,-8.65357747851728));
#60035=CARTESIAN_POINT('',(36.7946201341332,4.61461958493973,-9.52419805850888));
#60036=CARTESIAN_POINT('Ctrl Pts',(36.9580196850403,3.41777315288062,-8.65357747806631));
#60037=CARTESIAN_POINT('Ctrl Pts',(36.9593349194975,3.41808797886995,-8.65019366632357));
#60038=CARTESIAN_POINT('Ctrl Pts',(36.9606578277422,3.41840303936403,-8.64681279867953));
#60039=CARTESIAN_POINT('Ctrl Pts',(36.9877525088144,3.42482340968949,-8.57802807636569));
#60040=CARTESIAN_POINT('Ctrl Pts',(37.0163689742119,3.43101227617725,-8.5137885884489));
#60041=CARTESIAN_POINT('Ctrl Pts',(37.0889126010147,3.44545614568467,-8.36842811173175));
#60042=CARTESIAN_POINT('Ctrl Pts',(37.1347754030571,3.45374472789763,-8.28839405107078));
#60043=CARTESIAN_POINT('Ctrl Pts',(37.2429438103379,3.4715372749948,-8.12250437117899));
#60044=CARTESIAN_POINT('Ctrl Pts',(37.3065725150508,3.4810212150294,-8.03772055018812));
#60045=CARTESIAN_POINT('Ctrl Pts',(37.3923506611624,3.49248594432958,-7.93788993403964));
#60046=CARTESIAN_POINT('Ctrl Pts',(37.4094258077318,3.49471002660111,-7.91865049966739));
#60047=CARTESIAN_POINT('Ctrl Pts',(37.4356364992809,3.49803350443211,-7.89005500955978));
#60048=CARTESIAN_POINT('Ctrl Pts',(37.4445443520517,3.49914778652742,-7.88049424535983));
#60049=CARTESIAN_POINT('Ctrl Pts',(37.4610092367117,3.50117898612094,-7.86310879482112));
#60050=CARTESIAN_POINT('Ctrl Pts',(37.4685417756228,3.50209751557398,-7.8552623917427));
#60051=CARTESIAN_POINT('Ctrl Pts',(37.48625346677,3.50423280485122,-7.83706144511141));
#60052=CARTESIAN_POINT('Ctrl Pts',(37.4964735297955,3.50544644338921,-7.82674756194685));
#60053=CARTESIAN_POINT('Ctrl Pts',(37.5307854479325,3.50946283358482,-7.79274212216599));
#60054=CARTESIAN_POINT('Ctrl Pts',(37.5552844415844,3.51223675677904,-7.76946428332693));
#60055=CARTESIAN_POINT('Ctrl Pts',(37.61769324618,3.51909920502861,-7.71262007503551));
#60056=CARTESIAN_POINT('Ctrl Pts',(37.6561886041609,3.52315265981754,-7.67971877114943));
#60057=CARTESIAN_POINT('Ctrl Pts',(37.845657727897,3.54242819202665,-7.52786615872147));
#60058=CARTESIAN_POINT('Ctrl Pts',(38.0094785775956,3.55717542870145,-7.42608412121587));
#60059=CARTESIAN_POINT('Ctrl Pts',(38.2366726010001,3.57725277857447,-7.3201704644883));
#60060=CARTESIAN_POINT('Ctrl Pts',(38.2905559135131,3.5819841610232,-7.29740412773524));
#60061=CARTESIAN_POINT('Ctrl Pts',(38.3672737172541,3.58871506814573,-7.26823749867383));
#60062=CARTESIAN_POINT('Ctrl Pts',(38.389457600915,3.59066066438414,-7.26017528518951));
#60063=CARTESIAN_POINT('Ctrl Pts',(38.4302539410904,3.59423970706849,-7.24602494545069));
#60064=CARTESIAN_POINT('Ctrl Pts',(38.4488291904296,3.59586970297146,-7.2398350908971));
#60065=CARTESIAN_POINT('Ctrl Pts',(38.4868458857951,3.59920779134434,-7.22768033551739));
#60066=CARTESIAN_POINT('Ctrl Pts',(38.5062914963914,3.60091633067944,-7.22173386489734));
#60067=CARTESIAN_POINT('Ctrl Pts',(38.5555106853306,3.60524506442098,-7.20736244497045));
#60068=CARTESIAN_POINT('Ctrl Pts',(38.5853748547347,3.60787545044736,-7.19926440618985));
#60069=CARTESIAN_POINT('Ctrl Pts',(38.7220607272417,3.61993869222232,-7.16501673489835));
#60070=CARTESIAN_POINT('Ctrl Pts',(38.8304252359199,3.62957787645635,-7.14563999734203));
#60071=CARTESIAN_POINT('Ctrl Pts',(39.0273179841395,3.64721128329356,-7.12420879415173));
#60072=CARTESIAN_POINT('Ctrl Pts',(39.1153716064379,3.6551370942823,-7.11949501334781));
#60073=CARTESIAN_POINT('Ctrl Pts',(39.307920757196,3.67243488068461,-7.11977365636811));
#60074=CARTESIAN_POINT('Ctrl Pts',(39.4122516939758,3.68178656166889,-7.12672673736238));
#60075=CARTESIAN_POINT('Ctrl Pts',(39.541230949616,3.6931184791481,-7.14380871599408));
#60076=CARTESIAN_POINT('Ctrl Pts',(39.5665977783173,3.6953356931859,-7.14758192125478));
#60077=CARTESIAN_POINT('Ctrl Pts',(39.6047781775661,3.69865108382608,-7.15388677684076));
#60078=CARTESIAN_POINT('Ctrl Pts',(39.6176383821063,3.69976404308523,-7.15611809152294));
#60079=CARTESIAN_POINT('Ctrl Pts',(39.6411841973916,3.70179413122482,-7.16040113040019));
#60080=CARTESIAN_POINT('Ctrl Pts',(39.6518745538252,3.70271285660973,-7.16242075092119));
#60081=CARTESIAN_POINT('Ctrl Pts',(39.6768226299639,3.70485028175035,-7.16730947590759));
#60082=CARTESIAN_POINT('Ctrl Pts',(39.6910685874196,3.70606583953217,-7.17023544632597));
#60083=CARTESIAN_POINT('Ctrl Pts',(39.7384576614084,3.71009556289681,-7.18041745051984));
#60084=CARTESIAN_POINT('Ctrl Pts',(39.7714756696596,3.7128806429821,-7.18824586407321));
#60085=CARTESIAN_POINT('Ctrl Pts',(39.8536072924712,3.71977782728195,-7.20956409900276));
#60086=CARTESIAN_POINT('Ctrl Pts',(39.9024803365364,3.72385440760067,-7.22392023694661));
#60087=CARTESIAN_POINT('Ctrl Pts',(40.0614028939264,3.73713178791028,-7.27613896083274));
#60088=CARTESIAN_POINT('Ctrl Pts',(40.1691646058674,3.74617540026516,-7.32043357019661));
#60089=CARTESIAN_POINT('Ctrl Pts',(40.3812340085955,3.76479012319636,-7.42617061044486));
#60090=CARTESIAN_POINT('Ctrl Pts',(40.484952411685,3.77434389089163,-7.48801949957636));
#60091=CARTESIAN_POINT('Ctrl Pts',(40.6097556738044,3.78678514089852,-7.57577829045771));
#60092=CARTESIAN_POINT('Ctrl Pts',(40.6355531556078,3.78941133112884,-7.59469865661416));
#60093=CARTESIAN_POINT('Ctrl Pts',(40.6772869714902,3.79375635733544,-7.62660638747983));
#60094=CARTESIAN_POINT('Ctrl Pts',(40.6934483571942,3.79546356438347,-7.63929401707657));
#60095=CARTESIAN_POINT('Ctrl Pts',(40.7247615931006,3.79882143244092,-7.66453176978849));
#60096=CARTESIAN_POINT('Ctrl Pts',(40.7399259470194,3.80047128361934,-7.67706385931336));
#60097=CARTESIAN_POINT('Ctrl Pts',(40.775858112635,3.80443924609642,-7.70750825576055));
#60098=CARTESIAN_POINT('Ctrl Pts',(40.7964761330101,3.80676417554727,-7.72559208224059));
#60099=CARTESIAN_POINT('Ctrl Pts',(40.8703361542095,3.8152743005028,-7.79264259380783));
#60100=CARTESIAN_POINT('Ctrl Pts',(40.9216660134311,3.82154259728327,-7.84364670753645));
#60101=CARTESIAN_POINT('Ctrl Pts',(41.052376799369,3.83850553437088,-7.98579747732892));
#60102=CARTESIAN_POINT('Ctrl Pts',(41.1273159631718,3.84933562970301,-8.08073845455159));
#60103=CARTESIAN_POINT('Ctrl Pts',(41.2603235840797,3.87072742344648,-8.27813632492321));
#60104=CARTESIAN_POINT('Ctrl Pts',(41.3186549492757,3.88125845706078,-8.38005050689291));
#60105=CARTESIAN_POINT('Ctrl Pts',(41.3804161399582,3.89371021654375,-8.5089795001828));
#60106=CARTESIAN_POINT('Ctrl Pts',(41.391137924812,3.89593036170068,-8.53231326458873));
#60107=CARTESIAN_POINT('Ctrl Pts',(41.4067461188607,3.89924921716114,-8.56776699311271));
#60108=CARTESIAN_POINT('Ctrl Pts',(41.4119103814884,3.90036275410026,-8.57976143153011));
#60109=CARTESIAN_POINT('Ctrl Pts',(41.4207733757119,3.90230062786635,-8.60081694606028));
#60110=CARTESIAN_POINT('Ctrl Pts',(41.4245147252638,3.90312737405348,-8.6098590549655));
#60111=CARTESIAN_POINT('Ctrl Pts',(41.4334272387733,3.90511840487546,-8.63177650857913));
#60112=CARTESIAN_POINT('Ctrl Pts',(41.4385423554117,3.90627940840405,-8.6446741577924));
#60113=CARTESIAN_POINT('Ctrl Pts',(41.4543739723483,3.90993423855571,-8.68562366831918));
#60114=CARTESIAN_POINT('Ctrl Pts',(41.4646775074224,3.91240586714179,-8.71383375956975));
#60115=CARTESIAN_POINT('Ctrl Pts',(41.4884031191232,3.91835217647668,-8.78277205112817));
#60116=CARTESIAN_POINT('Ctrl Pts',(41.5012700970713,3.9218027230905,-8.82368150728246));
#60117=CARTESIAN_POINT('Ctrl Pts',(41.5536695550221,3.93703735084219,-9.00729735808516));
#60118=CARTESIAN_POINT('Ctrl Pts',(41.5810704989982,3.94848363400343,-9.15313334783323));
#60119=CARTESIAN_POINT('Ctrl Pts',(41.6046059863442,3.96836056127229,-9.40428041520086));
#60120=CARTESIAN_POINT('Ctrl Pts',(41.607576857524,3.97665301006434,-9.50849911267671));
#60121=CARTESIAN_POINT('Ctrl Pts',(41.6026470661362,3.98770180818317,-9.64381728935149));
#60122=CARTESIAN_POINT('Ctrl Pts',(41.6008997671245,3.99026979060772,-9.67503532655883));
#60123=CARTESIAN_POINT('Ctrl Pts',(41.5970079326382,3.99454404294112,-9.72654897681453));
#60124=CARTESIAN_POINT('Ctrl Pts',(41.5952126438631,3.99623943728665,-9.74686788054385));
#60125=CARTESIAN_POINT('Ctrl Pts',(41.5911699737425,3.99959308236003,-9.78681964440452));
#60126=CARTESIAN_POINT('Ctrl Pts',(41.5889386329375,4.0012507059347,-9.806452532119));
#60127=CARTESIAN_POINT('Ctrl Pts',(41.5829695418447,4.00527023047177,-9.85376955808061));
#60128=CARTESIAN_POINT('Ctrl Pts',(41.5789909846413,4.00763941978551,-9.88141971510631));
#60129=CARTESIAN_POINT('Ctrl Pts',(41.5623135594838,4.01655656271574,-9.98454938083769));
#60130=CARTESIAN_POINT('Ctrl Pts',(41.546497433785,4.02319864062312,-10.0594699090177));
#60131=CARTESIAN_POINT('Ctrl Pts',(41.4920029670353,4.04215576872437,-10.2678774653525));
#60132=CARTESIAN_POINT('Ctrl Pts',(41.4452962297143,4.05466308341572,-10.3989460838626));
#60133=CARTESIAN_POINT('Ctrl Pts',(41.3447781370712,4.07636089683615,-10.6187823799802));
#60134=CARTESIAN_POINT('Ctrl Pts',(41.2960434837016,4.08554313071805,-10.7094999933324));
#60135=CARTESIAN_POINT('Ctrl Pts',(41.2308728583156,4.09622103463023,-10.8141172543996));
#60136=CARTESIAN_POINT('Ctrl Pts',(41.2198828716314,4.0979745801887,-10.8312699306311));
#60137=CARTESIAN_POINT('Ctrl Pts',(41.2020950615439,4.10073709595823,-10.858270939394));
#60138=CARTESIAN_POINT('Ctrl Pts',(41.1954397237062,4.10175457274928,-10.8682112125744));
#60139=CARTESIAN_POINT('Ctrl Pts',(41.1824044956138,4.10371592447883,-10.8873696329386));
#60140=CARTESIAN_POINT('Ctrl Pts',(41.176033911898,4.10466029846762,-10.896593448935));
#60141=CARTESIAN_POINT('Ctrl Pts',(41.1599655937412,4.10700808979212,-10.9195140531975));
#60142=CARTESIAN_POINT('Ctrl Pts',(41.1501882877448,4.10840633807369,-10.9331549150289));
#60143=CARTESIAN_POINT('Ctrl Pts',(41.1105066157445,4.11396665152747,-10.9873108447007));
#60144=CARTESIAN_POINT('Ctrl Pts',(41.0794734953998,4.11806110851368,-11.0269883266445));
#60145=CARTESIAN_POINT('Ctrl Pts',(40.9092298937119,4.13941579932386,-11.231105532998));
#60146=CARTESIAN_POINT('Ctrl Pts',(40.7496410009324,4.15582606096452,-11.3772661891484));
#60147=CARTESIAN_POINT('Ctrl Pts',(40.5212009546674,4.17806399203037,-11.5360234807552));
#60148=CARTESIAN_POINT('Ctrl Pts',(40.4683169050197,4.18313063687343,-11.569788099085));
#60149=CARTESIAN_POINT('Ctrl Pts',(40.3933788918651,4.19024549251481,-11.6136072588675));
#60150=CARTESIAN_POINT('Ctrl Pts',(40.3723990322664,4.19223053260972,-11.6254556376636));
#60151=CARTESIAN_POINT('Ctrl Pts',(40.335518936243,4.19571060183271,-11.6455590071637));
#60152=CARTESIAN_POINT('Ctrl Pts',(40.319697583406,4.19720057279615,-11.653955387708));
#60153=CARTESIAN_POINT('Ctrl Pts',(40.2861509343199,4.20035464571398,-11.6712811955726));
#60154=CARTESIAN_POINT('Ctrl Pts',(40.2684060336639,4.20202003688691,-11.6801694409954));
#60155=CARTESIAN_POINT('Ctrl Pts',(40.2249991967709,4.20608795602905,-11.7012436802878));
#60156=CARTESIAN_POINT('Ctrl Pts',(40.199228098331,4.2084982093548,-11.7131962819359));
#60157=CARTESIAN_POINT('Ctrl Pts',(40.0994795088474,4.21781311161717,-11.7573300481472));
#60158=CARTESIAN_POINT('Ctrl Pts',(40.024120903696,4.22482334666033,-11.786234715184));
#60159=CARTESIAN_POINT('Ctrl Pts',(39.7996781697202,4.24563958834346,-11.8596120323593));
#60160=CARTESIAN_POINT('Ctrl Pts',(39.6475675299655,4.25969457084925,-11.8934809301705));
#60161=CARTESIAN_POINT('Ctrl Pts',(39.4116421127983,4.28096198949319,-11.9224621820517));
#60162=CARTESIAN_POINT('Ctrl Pts',(39.3295390398153,4.28825956304624,-11.9282977830992));
#60163=CARTESIAN_POINT('Ctrl Pts',(39.2275680311205,4.29708849208357,-11.9303028962588));
#60164=CARTESIAN_POINT('Ctrl Pts',(39.2078418519655,4.29878547794429,-11.9304481083016));
#60165=CARTESIAN_POINT('Ctrl Pts',(39.1762899010522,4.30148009113934,-11.9302922100469));
#60166=CARTESIAN_POINT('Ctrl Pts',(39.1644648395972,4.30248555106039,-11.9301465767236));
#60167=CARTESIAN_POINT('Ctrl Pts',(39.141339256127,4.30444261636934,-11.9296911733494));
#60168=CARTESIAN_POINT('Ctrl Pts',(39.1300390608362,4.30539455655823,-11.929388945235));
#60169=CARTESIAN_POINT('Ctrl Pts',(39.1015058901289,4.30778812908807,-11.9284244836011));
#60170=CARTESIAN_POINT('Ctrl Pts',(39.0842766229498,4.30922415578428,-11.9276565487144));
#60171=CARTESIAN_POINT('Ctrl Pts',(39.0125305263457,4.31517106733634,-11.9236851221204));
#60172=CARTESIAN_POINT('Ctrl Pts',(38.9581174383833,4.31960194301343,-11.9188106039989));
#60173=CARTESIAN_POINT('Ctrl Pts',(38.78310588815,4.33373602769284,-11.8971026306808));
#60174=CARTESIAN_POINT('Ctrl Pts',(38.6636021360547,4.34321300819339,-11.8729679713084));
#60175=CARTESIAN_POINT('Ctrl Pts',(38.424298904768,4.36270671317759,-11.805404818618));
#60176=CARTESIAN_POINT('Ctrl Pts',(38.3051017419946,4.37270165331029,-11.7613160017535));
#60177=CARTESIAN_POINT('Ctrl Pts',(38.1554727444249,4.38607733802574,-11.6920853018373));
#60178=CARTESIAN_POINT('Ctrl Pts',(38.1213825474304,4.38918277359544,-11.6753208990794));
#60179=CARTESIAN_POINT('Ctrl Pts',(38.0682080093226,4.39412910690891,-11.647588838696));
#60180=CARTESIAN_POINT('Ctrl Pts',(38.0488516975768,4.39595162432613,-11.6371538788507));
#60181=CARTESIAN_POINT('Ctrl Pts',(38.0129870886127,4.39937163025119,-11.6171798935425));
#60182=CARTESIAN_POINT('Ctrl Pts',(37.9964437406125,4.4009666780374,-11.6077070472827));
#60183=CARTESIAN_POINT('Ctrl Pts',(37.9591958376742,4.40459908865583,-11.5857866311749));
#60184=CARTESIAN_POINT('Ctrl Pts',(37.9385630447664,4.40664052514201,-11.5732219667284));
#60185=CARTESIAN_POINT('Ctrl Pts',(37.8754024078281,4.41298371717641,-11.533442984331));
#60186=CARTESIAN_POINT('Ctrl Pts',(37.8335423996164,4.41732216413543,-11.5052007011732));
#60187=CARTESIAN_POINT('Ctrl Pts',(37.7356636917833,4.42780367380336,-11.4345816941472));
#60188=CARTESIAN_POINT('Ctrl Pts',(37.6805540894529,4.43398492638125,-11.3910293111664));
#60189=CARTESIAN_POINT('Ctrl Pts',(37.5575961585515,4.44843144790128,-11.2847955448982));
#60190=CARTESIAN_POINT('Ctrl Pts',(37.4912932960137,4.45673074992079,-11.2204912259554));
#60191=CARTESIAN_POINT('Ctrl Pts',(37.3571774907485,4.47453880162299,-11.0745416338531));
#60192=CARTESIAN_POINT('Ctrl Pts',(37.2907254102811,4.48402752437495,-10.9918842848524));
#60193=CARTESIAN_POINT('Ctrl Pts',(37.2151744527485,4.49549715542414,-10.8840372471984));
#60194=CARTESIAN_POINT('Ctrl Pts',(37.2007528542799,4.49772156654922,-10.8627315516355));
#60195=CARTESIAN_POINT('Ctrl Pts',(37.1795240863556,4.50104551139799,-10.830258905755));
#60196=CARTESIAN_POINT('Ctrl Pts',(37.1724621803891,4.5021599347227,-10.8192620071867));
#60197=CARTESIAN_POINT('Ctrl Pts',(37.1596905260055,4.50419077934597,-10.7990127066486));
#60198=CARTESIAN_POINT('Ctrl Pts',(37.1539535839346,4.50510881949381,-10.7897787160039));
#60199=CARTESIAN_POINT('Ctrl Pts',(37.1407086773484,4.50724233944137,-10.7681341655149));
#60200=CARTESIAN_POINT('Ctrl Pts',(37.1332500609947,4.50845470668049,-10.7556941242143));
#60201=CARTESIAN_POINT('Ctrl Pts',(37.1088162703426,4.51246590975881,-10.7140929345523));
#60202=CARTESIAN_POINT('Ctrl Pts',(37.0923411596199,4.51523597027895,-10.6846404417925));
#60203=CARTESIAN_POINT('Ctrl Pts',(37.0223520517019,4.52734878408397,-10.5530984496911));
#60204=CARTESIAN_POINT('Ctrl Pts',(36.9755904287197,4.53639380378068,-10.4475755256196));
#60205=CARTESIAN_POINT('Ctrl Pts',(36.9096088648786,4.55166900248483,-10.2641268704389));
#60206=CARTESIAN_POINT('Ctrl Pts',(36.8863869460265,4.55789471082588,-10.1878681683283));
#60207=CARTESIAN_POINT('Ctrl Pts',(36.8434934239081,4.57180552029606,-10.0169818395727));
#60208=CARTESIAN_POINT('Ctrl Pts',(36.8256537930671,4.57950937869751,-9.92204613593157));
#60209=CARTESIAN_POINT('Ctrl Pts',(36.8097500044078,4.58987628827759,-9.7960826735058));
#60210=CARTESIAN_POINT('Ctrl Pts',(36.8065089090259,4.59237964481638,-9.76579262024283));
#60211=CARTESIAN_POINT('Ctrl Pts',(36.802251019455,4.59640768509294,-9.71731297228475));
#60212=CARTESIAN_POINT('Ctrl Pts',(36.800864061711,4.59792085650306,-9.6991584467843));
#60213=CARTESIAN_POINT('Ctrl Pts',(36.7984930904349,4.60097234035345,-9.66267491704818));
#60214=CARTESIAN_POINT('Ctrl Pts',(36.7975125202716,4.60251065399688,-9.64434692865343));
#60215=CARTESIAN_POINT('Ctrl Pts',(36.7960299714833,4.60548238504996,-9.60907372929461));
#60216=CARTESIAN_POINT('Ctrl Pts',(36.7954972013234,4.60691475386162,-9.59213083839908));
#60217=CARTESIAN_POINT('Ctrl Pts',(36.7947878054176,4.60979919286109,-9.55813616266211));
#60218=CARTESIAN_POINT('Ctrl Pts',(36.7946133512244,4.6112512407497,-9.54108538153903));
#60219=CARTESIAN_POINT('Ctrl Pts',(36.7946201936848,4.61270879799127,-9.52403471701899));
#60220=CARTESIAN_POINT('Ctrl Pts',(36.958019684865,4.68963520761331,-8.65357747851728));
#60221=CARTESIAN_POINT('Ctrl Pts',(36.9266910895544,4.68233500011651,-8.73417912956007));
#60222=CARTESIAN_POINT('Ctrl Pts',(36.8996729894311,4.6750347926197,-8.81657491459788));
#60223=CARTESIAN_POINT('Ctrl Pts',(36.8771553691407,4.6677345851229,-8.90030346144062));
#60224=CARTESIAN_POINT('Ctrl Pts',(36.8546928748826,4.66045224947351,-8.98382703002562));
#60225=CARTESIAN_POINT('Ctrl Pts',(36.8367090122413,4.65316991382412,-9.06867653828263));
#60226=CARTESIAN_POINT('Ctrl Pts',(36.8233451126604,4.64588757817474,-9.15437284113991));
#60227=CARTESIAN_POINT('Ctrl Pts',(36.8100296243597,4.63863162308812,-9.23975870558766));
#60228=CARTESIAN_POINT('Ctrl Pts',(36.8013008096218,4.6313756680015,-9.32598491874802));
#60229=CARTESIAN_POINT('Ctrl Pts',(36.7972493975383,4.62411971291489,-9.41256118655141));
#60230=CARTESIAN_POINT('Ctrl Pts',(36.7955102029823,4.62100486867674,-9.44972674032186));
#60231=CARTESIAN_POINT('Ctrl Pts',(36.7946323438184,4.6178900244386,-9.48695662627579));
#60232=CARTESIAN_POINT('Ctrl Pts',(36.7946201292839,4.61477518020045,-9.5242113593961));
#60233=CARTESIAN_POINT('',(36.7946203555469,4.88022481979722,-9.52369215796182));
#60234=CARTESIAN_POINT('Ctrl Pts',(36.958019684865,4.95526326543996,-8.65357747851728));
#60235=CARTESIAN_POINT('Ctrl Pts',(36.9288792425646,4.94851193509457,-8.72854948853697));
#60236=CARTESIAN_POINT('Ctrl Pts',(36.9035262455792,4.94176060474919,-8.80492605243814));
#60237=CARTESIAN_POINT('Ctrl Pts',(36.882075044055,4.93500927440379,-8.88228945628127));
#60238=CARTESIAN_POINT('Ctrl Pts',(36.8605859979768,4.92824603325307,-8.95978934588294));
#60239=CARTESIAN_POINT('Ctrl Pts',(36.8430126020127,4.92148279210234,-9.03827909962506));
#60240=CARTESIAN_POINT('Ctrl Pts',(36.8294181568492,4.91471955095162,-9.11733019571729));
#60241=CARTESIAN_POINT('Ctrl Pts',(36.8179322306018,4.90900529868777,-9.1841203477668));
#60242=CARTESIAN_POINT('Ctrl Pts',(36.8092858028889,4.90329104642392,-9.25131092184784));
#60243=CARTESIAN_POINT('Ctrl Pts',(36.8034880601261,4.89757679416008,-9.31864238215755));
#60244=CARTESIAN_POINT('Ctrl Pts',(36.7976195592362,4.8917928027229,-9.38679558434429));
#60245=CARTESIAN_POINT('Ctrl Pts',(36.7946575928612,4.88600881128573,-9.45520541903671));
#60246=CARTESIAN_POINT('Ctrl Pts',(36.7946203555473,4.88022481984855,-9.52369215735399));
#60247=CARTESIAN_POINT('Ctrl Pts',(36.7946203555469,4.88022481979722,-9.52369215796182));
#60248=CARTESIAN_POINT('Ctrl Pts',(36.7945774403228,4.87355888775427,-9.6026217256193));
#60249=CARTESIAN_POINT('Ctrl Pts',(36.7984237148322,4.86689295571132,-9.68170890384972));
#60250=CARTESIAN_POINT('Ctrl Pts',(36.8061793828676,4.86022702366837,-9.76053300701142));
#60251=CARTESIAN_POINT('Ctrl Pts',(36.8140937523611,4.85342468904469,-9.84097005957397));
#60252=CARTESIAN_POINT('Ctrl Pts',(36.8260793720773,4.84662235442101,-9.92113265213544));
#60253=CARTESIAN_POINT('Ctrl Pts',(36.8421016826417,4.83982001979733,-10.0005717289734));
#60254=CARTESIAN_POINT('Ctrl Pts',(36.8577660106002,4.83316966808927,-10.0782359177502));
#60255=CARTESIAN_POINT('Ctrl Pts',(36.8772884269659,4.82651931638121,-10.1552080876193));
#60256=CARTESIAN_POINT('Ctrl Pts',(36.9005843338745,4.81986896467315,-10.2310740320792));
#60257=CARTESIAN_POINT('Ctrl Pts',(36.9238685954304,4.81322193739851,-10.3069020520365));
#60258=CARTESIAN_POINT('Ctrl Pts',(36.9509224647324,4.80657491012386,-10.3816244864583));
#60259=CARTESIAN_POINT('Ctrl Pts',(36.9816109228423,4.79992788284922,-10.4548402264623));
#60260=CARTESIAN_POINT('Ctrl Pts',(37.0122940669605,4.79328200656913,-10.5280432884805));
#60261=CARTESIAN_POINT('Ctrl Pts',(37.046610364529,4.78663613028903,-10.599739732533));
#60262=CARTESIAN_POINT('Ctrl Pts',(37.084376480927,4.77999025400894,-10.6695479762532));
#60263=CARTESIAN_POINT('Ctrl Pts',(37.1236905226191,4.77307198223321,-10.7422174605904));
#60264=CARTESIAN_POINT('Ctrl Pts',(37.1667430396016,4.76615371045747,-10.8128401164677));
#60265=CARTESIAN_POINT('Ctrl Pts',(37.2132751644996,4.75923543868173,-10.8810152552262));
#60266=CARTESIAN_POINT('Ctrl Pts',(37.2580307062566,4.75258130453197,-10.9465874868011));
#60267=CARTESIAN_POINT('Ctrl Pts',(37.3060046286374,4.74592717038221,-11.0098953432796));
#60268=CARTESIAN_POINT('Ctrl Pts',(37.3569244840516,4.73927303623246,-11.0706149542857));
#60269=CARTESIAN_POINT('Ctrl Pts',(37.4078784733848,4.7326144415108,-11.1313752684374));
#60270=CARTESIAN_POINT('Ctrl Pts',(37.4617819963938,4.72595584678915,-11.1895435375494));
#60271=CARTESIAN_POINT('Ctrl Pts',(37.5183256588246,4.71929725206749,-11.2448326530894));
#60272=CARTESIAN_POINT('Ctrl Pts',(37.5749564181489,4.71262840079559,-11.3002069330845));
#60273=CARTESIAN_POINT('Ctrl Pts',(37.6342350654922,4.70595954952369,-11.3526929041604));
#60274=CARTESIAN_POINT('Ctrl Pts',(37.6958198457973,4.69929069825179,-11.4020442211367));
#60275=CARTESIAN_POINT('Ctrl Pts',(37.7029604337311,4.69851746306789,-11.4077663722392));
#60276=CARTESIAN_POINT('Ctrl Pts',(37.7101319945935,4.69774422788399,-11.4134464308331));
#60277=CARTESIAN_POINT('Ctrl Pts',(37.7173339726834,4.69697099270009,-11.4190840519473));
#60278=CARTESIAN_POINT('Ctrl Pts',(37.7802449250829,4.69021660366409,-11.4683299825981));
#60279=CARTESIAN_POINT('Ctrl Pts',(37.8457282525118,4.68346221462809,-11.514529153661));
#60280=CARTESIAN_POINT('Ctrl Pts',(37.9134568159231,4.6767078255921,-11.5574024158383));
#60281=CARTESIAN_POINT('Ctrl Pts',(37.9810889790601,4.66996305029841,-11.6002146551026));
#60282=CARTESIAN_POINT('Ctrl Pts',(38.0509596405553,4.66321827500472,-11.6397101401676));
#60283=CARTESIAN_POINT('Ctrl Pts',(38.1227096068288,4.65647349971103,-11.6756506813477));
#60284=CARTESIAN_POINT('Ctrl Pts',(38.194377455395,4.64973644380054,-11.7115500886429));
#60285=CARTESIAN_POINT('Ctrl Pts',(38.2679199194095,4.64299938789005,-11.7439024304701));
#60286=CARTESIAN_POINT('Ctrl Pts',(38.3429511939564,4.63626233197956,-11.7725142465531));
#60287=CARTESIAN_POINT('Ctrl Pts',(38.4179354919404,4.62952949409326,-11.8011081489757));
#60288=CARTESIAN_POINT('Ctrl Pts',(38.4944063157194,4.62279665620695,-11.8259660089512));
#60289=CARTESIAN_POINT('Ctrl Pts',(38.5719568429212,4.61606381832065,-11.8469420184937));
#60290=CARTESIAN_POINT('Ctrl Pts',(38.6494826702371,4.60933312484694,-11.8679113471655));
#60291=CARTESIAN_POINT('Ctrl Pts',(38.7280870684362,4.60260243137322,-11.8850011592218));
#60292=CARTESIAN_POINT('Ctrl Pts',(38.8073483679933,4.59587173789951,-11.8981155977496));
#60293=CARTESIAN_POINT('Ctrl Pts',(38.886608802285,4.58914111790222,-11.9112298931121));
#60294=CARTESIAN_POINT('Ctrl Pts',(38.9665256636284,4.58241049790493,-11.9203688265133));
#60295=CARTESIAN_POINT('Ctrl Pts',(39.0466688525193,4.57567987790765,-11.9254879719783));
#60296=CARTESIAN_POINT('Ctrl Pts',(39.1268907131434,4.56894265086679,-11.9306121425994));
#60297=CARTESIAN_POINT('Ctrl Pts',(39.2073388789196,4.56220542382593,-11.9317086130594));
#60298=CARTESIAN_POINT('Ctrl Pts',(39.2875804874595,4.55546819678507,-11.9287850574909));
#60299=CARTESIAN_POINT('Ctrl Pts',(39.3678603190795,4.54872776046696,-11.925860109287));
#60300=CARTESIAN_POINT('Ctrl Pts',(39.4479329324827,4.54198732414885,-11.9189113601794));
#60301=CARTESIAN_POINT('Ctrl Pts',(39.5273703501804,4.53524688783074,-11.9079984469619));
#60302=CARTESIAN_POINT('Ctrl Pts',(39.6069491658313,4.52849445359116,-11.8970661088482));
#60303=CARTESIAN_POINT('Ctrl Pts',(39.6858900674182,4.52174201935158,-11.8821555936922));
#60304=CARTESIAN_POINT('Ctrl Pts',(39.7637752274882,4.514989585112,-11.8633777362245));
#60305=CARTESIAN_POINT('Ctrl Pts',(39.8353821890891,4.50878145382138,-11.8461135318828));
#60306=CARTESIAN_POINT('Ctrl Pts',(39.9060966389583,4.50257332253075,-11.8255810079071));
#60307=CARTESIAN_POINT('Ctrl Pts',(39.9756079607792,4.49636519124012,-11.8019025529381));
#60308=CARTESIAN_POINT('Ctrl Pts',(40.0512315734989,4.48961116464219,-11.7761419967945));
#60309=CARTESIAN_POINT('Ctrl Pts',(40.1257099193966,4.48285713804425,-11.7465622630599));
#60310=CARTESIAN_POINT('Ctrl Pts',(40.1986304658414,4.47610311144631,-11.7132847477176));
#60311=CARTESIAN_POINT('Ctrl Pts',(40.2714474382258,4.46935867805623,-11.6800544987158));
#60312=CARTESIAN_POINT('Ctrl Pts',(40.3427105850688,4.46261424466615,-11.6431370914683));
#60313=CARTESIAN_POINT('Ctrl Pts',(40.4120241589146,4.45586981127607,-11.602703150743));
#60314=CARTESIAN_POINT('Ctrl Pts',(40.4812587373487,4.44913306439332,-11.56231529184));
#60315=CARTESIAN_POINT('Ctrl Pts',(40.548547757972,4.44239631751056,-11.5184190981792));
#60316=CARTESIAN_POINT('Ctrl Pts',(40.6135183888386,4.43565957062781,-11.4712319257517));
#60317=CARTESIAN_POINT('Ctrl Pts',(40.6784485350197,4.42892702156605,-11.4240741567301));
#60318=CARTESIAN_POINT('Ctrl Pts',(40.7410627830016,4.4221944725043,-11.3736297529507));
#60319=CARTESIAN_POINT('Ctrl Pts',(40.8010167239755,4.41546192344254,-11.3201597126581));
#60320=CARTESIAN_POINT('Ctrl Pts',(40.8609517528089,4.40873149812631,-11.2667065391953));
#60321=CARTESIAN_POINT('Ctrl Pts',(40.9182277936001,4.40200107281007,-11.2102299347198));
#60322=CARTESIAN_POINT('Ctrl Pts',(40.9725341581777,4.39527064749383,-11.1510306277845));
#60323=CARTESIAN_POINT('Ctrl Pts',(41.0268401005479,4.38854027450362,-11.0918317810972));
#60324=CARTESIAN_POINT('Ctrl Pts',(41.0781760985413,4.3818099015134,-11.0299106184793));
#60325=CARTESIAN_POINT('Ctrl Pts',(41.1262699310444,4.37507952852318,-10.9656030324674));
#60326=CARTESIAN_POINT('Ctrl Pts',(41.1744112283861,4.36834251318297,-10.9012319799145));
#60327=CARTESIAN_POINT('Ctrl Pts',(41.2193036886749,4.36160549784275,-10.8344701734186));
#60328=CARTESIAN_POINT('Ctrl Pts',(41.2607172139349,4.35486848250254,-10.7656842904593));
#60329=CARTESIAN_POINT('Ctrl Pts',(41.302150583846,4.3481282389001,-10.6968654464845));
#60330=CARTESIAN_POINT('Ctrl Pts',(41.3401014770831,4.34138799529767,-10.6260210051411));
#60331=CARTESIAN_POINT('Ctrl Pts',(41.3743859848242,4.33464775169523,-10.5535419453772));
#60332=CARTESIAN_POINT('Ctrl Pts',(41.4087316970137,4.32789547545999,-10.4809334965343));
#60333=CARTESIAN_POINT('Ctrl Pts',(41.4393977667856,4.32114319922476,-10.4066850302307));
#60334=CARTESIAN_POINT('Ctrl Pts',(41.4662487100064,4.31439092298952,-10.3312070012065));
#60335=CARTESIAN_POINT('Ctrl Pts',(41.490945282584,4.30818041191972,-10.2617849102773));
#60336=CARTESIAN_POINT('Ctrl Pts',(41.5124148755175,4.30196990084993,-10.1913231096163));
#60337=CARTESIAN_POINT('Ctrl Pts',(41.5305901900215,4.29575938978013,-10.1201489818321));
#60338=CARTESIAN_POINT('Ctrl Pts',(41.5503494618059,4.28900763997568,-10.0427721125296));
#60339=CARTESIAN_POINT('Ctrl Pts',(41.5662878541097,4.28225589017123,-9.96426632387336));
#60340=CARTESIAN_POINT('Ctrl Pts',(41.5782812986408,4.27550414036678,-9.88504306539031));
#60341=CARTESIAN_POINT('Ctrl Pts',(41.5902576260479,4.26876202670458,-9.80593287486901));
#60342=CARTESIAN_POINT('Ctrl Pts',(41.5983001183935,4.26201991304238,-9.72610770565665));
#60343=CARTESIAN_POINT('Ctrl Pts',(41.6023350939562,4.25527779938018,-9.64599190364012));
#60344=CARTESIAN_POINT('Ctrl Pts',(41.6063654371608,4.24854342600903,-9.56596807865868));
#60345=CARTESIAN_POINT('Ctrl Pts',(41.6063973838752,4.24180905263788,-9.48565474755449));
#60346=CARTESIAN_POINT('Ctrl Pts',(41.6024089049995,4.23507467926672,-9.40548264737234));
#60347=CARTESIAN_POINT('Ctrl Pts',(41.5984229310417,4.22834453534059,-9.32536089834706));
#60348=CARTESIAN_POINT('Ctrl Pts',(41.5904215668024,4.22161439141446,-9.24538066888293));
#60349=CARTESIAN_POINT('Ctrl Pts',(41.5784348642965,4.21488424748833,-9.16597278557365));
#60350=CARTESIAN_POINT('Ctrl Pts',(41.5664519945955,4.20815625555756,-9.08659029331076));
#60351=CARTESIAN_POINT('Ctrl Pts',(41.5504863869424,4.20142826362679,-9.007780244697));
#60352=CARTESIAN_POINT('Ctrl Pts',(41.530619798486,4.19470027169603,-8.92996697629017));
#60353=CARTESIAN_POINT('Ctrl Pts',(41.5107534380768,4.18797235699541,-8.85215460109645));
#60354=CARTESIAN_POINT('Ctrl Pts',(41.4869863026282,4.18124444229479,-8.77533943502138));
#60355=CARTESIAN_POINT('Ctrl Pts',(41.459450627858,4.17451652759418,-8.69993284838608));
#60356=CARTESIAN_POINT('Ctrl Pts',(41.4318878582798,4.16778199269782,-8.62445206248017));
#60357=CARTESIAN_POINT('Ctrl Pts',(41.4005493023171,4.16104745780147,-8.5503830639371));
#60358=CARTESIAN_POINT('Ctrl Pts',(41.3656160067488,4.15431292290512,-8.47811879579702));
#60359=CARTESIAN_POINT('Ctrl Pts',(41.3306660486845,4.14757517576788,-8.40582005902033));
#60360=CARTESIAN_POINT('Ctrl Pts',(41.2921181591336,4.14083742863065,-8.33532817748099));
#60361=CARTESIAN_POINT('Ctrl Pts',(41.2501989899998,4.13409968149342,-8.26701071316009));
#60362=CARTESIAN_POINT('Ctrl Pts',(41.2082049477827,4.12734989986425,-8.19857122497034));
#60363=CARTESIAN_POINT('Ctrl Pts',(41.1628278580619,4.12060011823509,-8.13231430037839));
#60364=CARTESIAN_POINT('Ctrl Pts',(41.1143371591158,4.11385033660593,-8.06857760741311));
#60365=CARTESIAN_POINT('Ctrl Pts',(41.0695644320259,4.10761808717733,-8.00972785639345));
#60366=CARTESIAN_POINT('Ctrl Pts',(41.0221379048071,4.10138583774874,-7.95302653405436));
#60367=CARTESIAN_POINT('Ctrl Pts',(40.9722975880818,4.09515358832014,-7.8987115250733));
#60368=CARTESIAN_POINT('Ctrl Pts',(40.9182918137351,4.08840047199931,-7.83985708129362));
#60369=CARTESIAN_POINT('Ctrl Pts',(40.8612512106479,4.08164735567848,-7.78358671238853));
#60370=CARTESIAN_POINT('Ctrl Pts',(40.8014527295569,4.07489423935764,-7.73022923486182));
#60371=CARTESIAN_POINT('Ctrl Pts',(40.7417394114184,4.0681507405942,-7.67694774723045));
#60372=CARTESIAN_POINT('Ctrl Pts',(40.679276361022,4.06140724183076,-7.62657121976668));
#60373=CARTESIAN_POINT('Ctrl Pts',(40.6143788556305,4.05466374306732,-7.57939330872213));
#60374=CARTESIAN_POINT('Ctrl Pts',(40.5495556344738,4.04792796317753,-7.53226939936832));
#60375=CARTESIAN_POINT('Ctrl Pts',(40.4823038716433,4.04119218328774,-7.48833710282283));
#60376=CARTESIAN_POINT('Ctrl Pts',(40.4129724165713,4.03445640339796,-7.44785030365236));
#60377=CARTESIAN_POINT('Ctrl Pts',(40.343684367905,4.02772484058387,-7.40738885208816));
#60378=CARTESIAN_POINT('Ctrl Pts',(40.2723196132366,4.02099327776977,-7.37036885037852));
#60379=CARTESIAN_POINT('Ctrl Pts',(40.1992555315112,4.01426171495568,-7.33700061079891));
#60380=CARTESIAN_POINT('Ctrl Pts',(40.1262146949032,4.00753229376801,-7.30364298722417));
#60381=CARTESIAN_POINT('Ctrl Pts',(40.0514760287572,4.00080287258034,-7.27393501205814));
#60382=CARTESIAN_POINT('Ctrl Pts',(39.9754397279329,3.99407345139267,-7.24804014687492));
#60383=CARTESIAN_POINT('Ctrl Pts',(39.8994042050589,3.98734409905574,-7.22214554662989));
#60384=CARTESIAN_POINT('Ctrl Pts',(39.8220715157349,3.98061474671881,-7.2000641278065));
#60385=CARTESIAN_POINT('Ctrl Pts',(39.743858579342,3.97388539438188,-7.18190999104258));
#60386=CARTESIAN_POINT('Ctrl Pts',(39.6655686620604,3.9671494186966,-7.16373798611456));
#60387=CARTESIAN_POINT('Ctrl Pts',(39.5863972223019,3.96041344301131,-7.14950109040008));
#60388=CARTESIAN_POINT('Ctrl Pts',(39.5067724215681,3.95367746732602,-7.13926245664674));
#60389=CARTESIAN_POINT('Ctrl Pts',(39.4271096022657,3.9469382754047,-7.12901893423816));
#60390=CARTESIAN_POINT('Ctrl Pts',(39.3469934562053,3.94019908348338,-7.12277751346746));
#60391=CARTESIAN_POINT('Ctrl Pts',(39.2668558148351,3.93345989156206,-7.12054928425997));
#60392=CARTESIAN_POINT('Ctrl Pts',(39.1865751879476,3.92670867524339,-7.11831707933645));
#60393=CARTESIAN_POINT('Ctrl Pts',(39.1062734564255,3.91995745892471,-7.12011236363538));
#60394=CARTESIAN_POINT('Ctrl Pts',(39.0263808027279,3.91320624260604,-7.12589405845874));
#60395=CARTESIAN_POINT('Ctrl Pts',(38.9527805568328,3.90698675735742,-7.13122038248223));
#60396=CARTESIAN_POINT('Ctrl Pts',(38.8795277139355,3.9007672721088,-7.13992926607577));
#60397=CARTESIAN_POINT('Ctrl Pts',(38.8069505596118,3.89454778686017,-7.15195025719846));
#60398=CARTESIAN_POINT('Ctrl Pts',(38.728148265386,3.8877948394477,-7.16500232142117));
#60399=CARTESIAN_POINT('Ctrl Pts',(38.6498508697298,3.88104189203523,-7.18200801276839));
#60400=CARTESIAN_POINT('Ctrl Pts',(38.5724850870386,3.87428894462276,-7.20291516554391));
#60401=CARTESIAN_POINT('Ctrl Pts',(38.4952294795526,3.86754561396,-7.22379254482306));
#60402=CARTESIAN_POINT('Ctrl Pts',(38.4189032966122,3.86080228329723,-7.24856023024329));
#60403=CARTESIAN_POINT('Ctrl Pts',(38.3439247610938,3.85405895263446,-7.27711474275673));
#60404=CARTESIAN_POINT('Ctrl Pts',(38.2690320282456,3.84732333879055,-7.30563657853939));
#60405=CARTESIAN_POINT('Ctrl Pts',(38.1954843114477,3.84058772494664,-7.337936463867));
#60406=CARTESIAN_POINT('Ctrl Pts',(38.1236848815208,3.83385211110273,-7.37386106675253));
#60407=CARTESIAN_POINT('Ctrl Pts',(38.0519303900041,3.82712071299951,-7.40976318485587));
#60408=CARTESIAN_POINT('Ctrl Pts',(37.9819224291752,3.82038931489629,-7.44928530894816));
#60409=CARTESIAN_POINT('Ctrl Pts',(37.9140433782879,3.81365791679308,-7.49222639935606));
#60410=CARTESIAN_POINT('Ctrl Pts',(37.8461859075688,3.80692865874192,-7.53515383789437));
#60411=CARTESIAN_POINT('Ctrl Pts',(37.7804563964344,3.80019940069076,-7.58149783497121));
#60412=CARTESIAN_POINT('Ctrl Pts',(37.7172104638034,3.79347014263961,-7.63101263580089));
#60413=CARTESIAN_POINT('Ctrl Pts',(37.6539651612174,3.78674095162415,-7.68052694337272));
#60414=CARTESIAN_POINT('Ctrl Pts',(37.5932037542561,3.7800117606087,-7.73321170334964));
#60415=CARTESIAN_POINT('Ctrl Pts',(37.5352496695307,3.77328256959324,-7.78878017474674));
#60416=CARTESIAN_POINT('Ctrl Pts',(37.477238507653,3.76654675120954,-7.84440337378078));
#60417=CARTESIAN_POINT('Ctrl Pts',(37.4220405283669,3.75981093282584,-7.90291563403494));
#60418=CARTESIAN_POINT('Ctrl Pts',(37.3699426403205,3.75307511444214,-7.96399295175109));
#60419=CARTESIAN_POINT('Ctrl Pts',(37.3178198613456,3.74633607787091,-8.02509945051856));
#60420=CARTESIAN_POINT('Ctrl Pts',(37.2688004093012,3.73959704129968,-8.08877307834769));
#60421=CARTESIAN_POINT('Ctrl Pts',(37.2231296017101,3.73285800472846,-8.15465830072746));
#60422=CARTESIAN_POINT('Ctrl Pts',(37.1773772691902,3.72610693860256,-8.22066113188945));
#60423=CARTESIAN_POINT('Ctrl Pts',(37.1349857720421,3.71935587247666,-8.28888304904211));
#60424=CARTESIAN_POINT('Ctrl Pts',(37.0961558408247,3.71260480635077,-8.35894138298974));
#60425=CARTESIAN_POINT('Ctrl Pts',(37.0603750204169,3.70638386603391,-8.42349840347501));
#60426=CARTESIAN_POINT('Ctrl Pts',(37.0276179788031,3.70016292571704,-8.4896142202192));
#60427=CARTESIAN_POINT('Ctrl Pts',(36.9980052420606,3.69394198540018,-8.55697519122324));
#60428=CARTESIAN_POINT('Ctrl Pts',(36.9839854702094,3.69099676069162,-8.5888663822794));
#60429=CARTESIAN_POINT('Ctrl Pts',(36.9706522083476,3.68805153598306,-8.62107674749401));
#60430=CARTESIAN_POINT('Ctrl Pts',(36.958019684865,3.68510631127449,-8.65357747851728));
#60431=CARTESIAN_POINT('Origin',(39.2,8.05522481984854,-9.525));
#60432=CARTESIAN_POINT('',(36.9580197803105,2.14933799730903,-8.65357723295689));
#60433=CARTESIAN_POINT('',(36.960707778965,2.41503531351511,-8.65459504792143));
#60434=CARTESIAN_POINT('',(36.958019684865,8.05522481984854,-8.65357747851728));
#60435=CARTESIAN_POINT('Ctrl Pts',(36.9580197803105,2.14933799730903,-8.65357723295689));
#60436=CARTESIAN_POINT('Ctrl Pts',(36.9800579747574,2.15411338859981,-8.59687777788607));
#60437=CARTESIAN_POINT('Ctrl Pts',(37.004249355822,2.15890857144129,-8.54100834907343));
#60438=CARTESIAN_POINT('Ctrl Pts',(37.0624888151197,2.16964011257482,-8.41939256638918));
#60439=CARTESIAN_POINT('Ctrl Pts',(37.0974851644807,2.17559155144584,-8.35420912979925));
#60440=CARTESIAN_POINT('Ctrl Pts',(37.1496303646409,2.18391232036595,-8.26698420663039));
#60441=CARTESIAN_POINT('Ctrl Pts',(37.164244466139,2.18619260383398,-8.24347018915741));
#60442=CARTESIAN_POINT('Ctrl Pts',(37.1899557644334,2.19012209252849,-8.2036507409405));
#60443=CARTESIAN_POINT('Ctrl Pts',(37.2008539021761,2.19176392095439,-8.18721955301133));
#60444=CARTESIAN_POINT('Ctrl Pts',(37.2234754037399,2.19512570663176,-8.15400676169728));
#60445=CARTESIAN_POINT('Ctrl Pts',(37.2352134364241,2.19684611030984,-8.13723718048166));
#60446=CARTESIAN_POINT('Ctrl Pts',(37.2656209013829,2.20124440430392,-8.09495460620065));
#60447=CARTESIAN_POINT('Ctrl Pts',(37.2845813141517,2.20393317322019,-8.06965695485378));
#60448=CARTESIAN_POINT('Ctrl Pts',(37.3717017419663,2.21606013277,-7.95807009910218));
#60449=CARTESIAN_POINT('Ctrl Pts',(37.4452215697634,2.22570331528963,-7.87615522060898));
#60450=CARTESIAN_POINT('Ctrl Pts',(37.6264572261133,2.24820534351681,-7.70011969644428));
#60451=CARTESIAN_POINT('Ctrl Pts',(37.7374847918337,2.2611304088081,-7.6099876023341));
#60452=CARTESIAN_POINT('Ctrl Pts',(37.9074439623172,2.27935974725653,-7.49546233371284));
#60453=CARTESIAN_POINT('Ctrl Pts',(37.9603780371533,2.28484033899742,-7.46270435203461));
#60454=CARTESIAN_POINT('Ctrl Pts',(38.0301546941842,2.29176698333998,-7.42318235417618));
#60455=CARTESIAN_POINT('Ctrl Pts',(38.0458801747725,2.2933091781783,-7.41450646901256));
#60456=CARTESIAN_POINT('Ctrl Pts',(38.0717850838821,2.29581729306574,-7.40059065787178));
#60457=CARTESIAN_POINT('Ctrl Pts',(38.0819070091284,2.29678931554823,-7.39524601580351));
#60458=CARTESIAN_POINT('Ctrl Pts',(38.1023918099541,2.2987399133193,-7.38461580272096));
#60459=CARTESIAN_POINT('Ctrl Pts',(38.112755609307,2.29971832801506,-7.37933276029649));
#60460=CARTESIAN_POINT('Ctrl Pts',(38.1399965904096,2.30226913889562,-7.36569447783877));
#60461=CARTESIAN_POINT('Ctrl Pts',(38.1569347406686,2.30383434213327,-7.35746164993201));
#60462=CARTESIAN_POINT('Ctrl Pts',(38.2340531901071,2.31087482251907,-7.32109146531131));
#60463=CARTESIAN_POINT('Ctrl Pts',(38.2952931544834,2.31623146238172,-7.29525255050626));
#60464=CARTESIAN_POINT('Ctrl Pts',(38.4982529209867,2.33348667942382,-7.21936009742986));
#60465=CARTESIAN_POINT('Ctrl Pts',(38.6435999461897,2.34509428941009,-7.18003779688679));
#60466=CARTESIAN_POINT('Ctrl Pts',(38.8897218326058,2.36480386941585,-7.13764173196709));
#60467=CARTESIAN_POINT('Ctrl Pts',(38.9887132419023,2.37274111869828,-7.12685367396695));
#60468=CARTESIAN_POINT('Ctrl Pts',(39.11823065864,2.38333124367357,-7.1208207591722));
#60469=CARTESIAN_POINT('Ctrl Pts',(39.14840478996,2.38581243819792,-7.11998402973177));
#60470=CARTESIAN_POINT('Ctrl Pts',(39.1987690096886,2.38998192404698,-7.11953562874444));
#60471=CARTESIAN_POINT('Ctrl Pts',(39.218953467677,2.39166043870823,-7.11960999609052));
#60472=CARTESIAN_POINT('Ctrl Pts',(39.2588225720517,2.39499212554522,-7.12025872635879));
#60473=CARTESIAN_POINT('Ctrl Pts',(39.2785058557154,2.39664478799011,-7.12082083248984));
#60474=CARTESIAN_POINT('Ctrl Pts',(39.3267985812795,2.40072008215193,-7.12279362081246));
#60475=CARTESIAN_POINT('Ctrl Pts',(39.3553932072862,2.40315081466832,-7.12447377285064));
#60476=CARTESIAN_POINT('Ctrl Pts',(39.4600942375036,2.41212051185402,-7.13250422627305));
#60477=CARTESIAN_POINT('Ctrl Pts',(39.5359078903738,2.41875212388985,-7.14196658403603));
#60478=CARTESIAN_POINT('Ctrl Pts',(39.80305357098,2.44262454135369,-7.18830992634035));
#60479=CARTESIAN_POINT('Ctrl Pts',(39.990190825163,2.46035041432068,-7.2447852724692));
#60480=CARTESIAN_POINT('Ctrl Pts',(40.2163447588134,2.48223817728373,-7.34425862340657));
#60481=CARTESIAN_POINT('Ctrl Pts',(40.2635356283495,2.48682772379357,-7.36687982703521));
#60482=CARTESIAN_POINT('Ctrl Pts',(40.3250359252064,2.49280761512033,-7.39886828823797));
#60483=CARTESIAN_POINT('Ctrl Pts',(40.3400334274706,2.49426574210177,-7.40687211811031));
#60484=CARTESIAN_POINT('Ctrl Pts',(40.3648150163997,2.49667344143415,-7.42043697755966));
#60485=CARTESIAN_POINT('Ctrl Pts',(40.3746469523872,2.49762822761501,-7.4259087447446));
#60486=CARTESIAN_POINT('Ctrl Pts',(40.3935000903804,2.49945773043525,-7.43657503762299));
#60487=CARTESIAN_POINT('Ctrl Pts',(40.4025264827496,2.50033309791933,-7.44175940893857));
#60488=CARTESIAN_POINT('Ctrl Pts',(40.4274594415575,2.50275036958679,-7.45629588280709));
#60489=CARTESIAN_POINT('Ctrl Pts',(40.4432929704987,2.50428465517369,-7.46577294628098));
#60490=CARTESIAN_POINT('Ctrl Pts',(40.5122530818503,2.51097088709593,-7.50813402627492));
#60491=CARTESIAN_POINT('Ctrl Pts',(40.5642014235235,2.51601821113748,-7.54290192720138));
#60492=CARTESIAN_POINT('Ctrl Pts',(40.7392940991964,2.53329113586009,-7.6702373502469));
#60493=CARTESIAN_POINT('Ctrl Pts',(40.8548647744161,2.54518214365506,-7.77257345385189));
#60494=CARTESIAN_POINT('Ctrl Pts',(41.0282355512723,2.56524862155498,-7.95864511090542));
#60495=CARTESIAN_POINT('Ctrl Pts',(41.0919438911289,2.57324798242957,-8.03622299973057));
#60496=CARTESIAN_POINT('Ctrl Pts',(41.1683185965039,2.5839084075277,-8.14207201957113));
#60497=CARTESIAN_POINT('Ctrl Pts',(41.1855525739471,2.58639471806334,-8.16693199462413));
#60498=CARTESIAN_POINT('Ctrl Pts',(41.2135041870448,2.59057037352914,-8.2089218292393));
#60499=CARTESIAN_POINT('Ctrl Pts',(41.2244833609855,2.59224987823744,-8.22587416624515));
#60500=CARTESIAN_POINT('Ctrl Pts',(41.2457372307492,2.59558167789431,-8.25961489071256));
#60501=CARTESIAN_POINT('Ctrl Pts',(41.2560219212059,2.59723344577654,-8.27639513759813));
#60502=CARTESIAN_POINT('Ctrl Pts',(41.278397678395,2.60091776456405,-8.31392903674394));
#60503=CARTESIAN_POINT('Ctrl Pts',(41.2903859627737,2.60295379484999,-8.33474111037115));
#60504=CARTESIAN_POINT('Ctrl Pts',(41.332040008047,2.61025793229785,-8.40962474668539));
#60505=CARTESIAN_POINT('Ctrl Pts',(41.3599328743526,2.615586018623,-8.46464860386458));
#60506=CARTESIAN_POINT('Ctrl Pts',(41.4645727312524,2.63750160600169,-8.69237352344908));
#60507=CARTESIAN_POINT('Ctrl Pts',(41.5229530311541,2.65462238576592,-8.87275268572227));
#60508=CARTESIAN_POINT('Ctrl Pts',(41.5693200356805,2.67594568030793,-9.10706378998762));
#60509=CARTESIAN_POINT('Ctrl Pts',(41.5774887059025,2.68037746307748,-9.15635889992386));
#60510=CARTESIAN_POINT('Ctrl Pts',(41.5885577597293,2.68769016089283,-9.23905373727676));
#60511=CARTESIAN_POINT('Ctrl Pts',(41.5923060428466,2.6905994974062,-9.27232319646403));
#60512=CARTESIAN_POINT('Ctrl Pts',(41.5966780664796,2.69471888713782,-9.3200695371077));
#60513=CARTESIAN_POINT('Ctrl Pts',(41.5978673365949,2.69595564904236,-9.33448879929634));
#60514=CARTESIAN_POINT('Ctrl Pts',(41.5997151919055,2.69810130478685,-9.35966389271286));
#60515=CARTESIAN_POINT('Ctrl Pts',(41.6004317139652,2.69901319622852,-9.37041463186073));
#60516=CARTESIAN_POINT('Ctrl Pts',(41.6018567727451,2.70102127667839,-9.39420443726168));
#60517=CARTESIAN_POINT('Ctrl Pts',(41.6025314155785,2.70211563172631,-9.40724492536064));
#60518=CARTESIAN_POINT('Ctrl Pts',(41.6042173773803,2.70534560309632,-9.44593810331292));
#60519=CARTESIAN_POINT('Ctrl Pts',(41.6049243095676,2.70746570376653,-9.47160329976444));
#60520=CARTESIAN_POINT('Ctrl Pts',(41.6065738043277,2.7191879357727,-9.61470897702045));
#60521=CARTESIAN_POINT('Ctrl Pts',(41.5993254197737,2.72843606174457,-9.73210064877853));
#60522=CARTESIAN_POINT('Ctrl Pts',(41.5672716671839,2.74712650570054,-9.96826495618314));
#60523=CARTESIAN_POINT('Ctrl Pts',(41.542016023149,2.75654285239867,-10.0866206801527));
#60524=CARTESIAN_POINT('Ctrl Pts',(41.4876540373957,2.77191385547458,-10.2717903554194));
#60525=CARTESIAN_POINT('Ctrl Pts',(41.4642320423748,2.77772352532783,-10.3400510679311));
#60526=CARTESIAN_POINT('Ctrl Pts',(41.427732551305,2.78587483961413,-10.4326405225228));
#60527=CARTESIAN_POINT('Ctrl Pts',(41.4172499502583,2.78813214641582,-10.457955610874));
#60528=CARTESIAN_POINT('Ctrl Pts',(41.3985039748555,2.79203456678415,-10.5011250030674));
#60529=CARTESIAN_POINT('Ctrl Pts',(41.390449581311,2.79367256676652,-10.5190675694235));
#60530=CARTESIAN_POINT('Ctrl Pts',(41.3735301656066,2.79703772304248,-10.5555542055835));
#60531=CARTESIAN_POINT('Ctrl Pts',(41.3646456864253,2.798765428518,-10.5740873879471));
#60532=CARTESIAN_POINT('Ctrl Pts',(41.3413130125291,2.80320631500554,-10.6212011895211));
#60533=CARTESIAN_POINT('Ctrl Pts',(41.3265300194785,2.80593080209062,-10.6496103011514));
#60534=CARTESIAN_POINT('Ctrl Pts',(41.2527059332856,2.81913178153162,-10.7848183858992));
#60535=CARTESIAN_POINT('Ctrl Pts',(41.1861720836507,2.82986548364257,-10.8872975554156));
#60536=CARTESIAN_POINT('Ctrl Pts',(41.042029753559,2.85108603930914,-11.0761751482423));
#60537=CARTESIAN_POINT('Ctrl Pts',(40.965361975656,2.86152767489654,-11.1628993664968));
#60538=CARTESIAN_POINT('Ctrl Pts',(40.8466764265417,2.87635892768922,-11.2790978506833));
#60539=CARTESIAN_POINT('Ctrl Pts',(40.8094902412796,2.88083992556557,-11.3132797330393));
#60540=CARTESIAN_POINT('Ctrl Pts',(40.7457159713271,2.88822367138462,-11.3682993823527));
#60541=CARTESIAN_POINT('Ctrl Pts',(40.7197163408817,2.89115548582568,-11.3897930341245));
#60542=CARTESIAN_POINT('Ctrl Pts',(40.6818967002887,2.89530056596648,-11.4197415729925));
#60543=CARTESIAN_POINT('Ctrl Pts',(40.6704403491649,2.89654097812276,-11.4286461517571));
#60544=CARTESIAN_POINT('Ctrl Pts',(40.6502565080986,2.89869893615567,-11.4440433273165));
#60545=CARTESIAN_POINT('Ctrl Pts',(40.6415645851369,2.89961944309052,-11.4505811584148));
#60546=CARTESIAN_POINT('Ctrl Pts',(40.6223265590673,2.90163745378703,-11.4648481993212));
#60547=CARTESIAN_POINT('Ctrl Pts',(40.6117614069294,2.90273318527324,-11.4725506749406));
#60548=CARTESIAN_POINT('Ctrl Pts',(40.5801969774094,2.9059716038225,-11.4951707299223));
#60549=CARTESIAN_POINT('Ctrl Pts',(40.5590194217999,2.90809865386876,-11.5098382239607));
#60550=CARTESIAN_POINT('Ctrl Pts',(40.4491543157507,2.91892497902682,-11.5833472463935));
#60551=CARTESIAN_POINT('Ctrl Pts',(40.3568563933049,2.92733727483172,-11.6366035236715));
#60552=CARTESIAN_POINT('Ctrl Pts',(40.177775259362,2.94300819869835,-11.7246535937927));
#60553=CARTESIAN_POINT('Ctrl Pts',(40.0919152526067,2.9502657037587,-11.7608460022553));
#60554=CARTESIAN_POINT('Ctrl Pts',(39.9064173005675,2.9657819710479,-11.8266486560817));
#60555=CARTESIAN_POINT('Ctrl Pts',(39.8065320427433,2.97404538974445,-11.8549627137646));
#60556=CARTESIAN_POINT('Ctrl Pts',(39.6753126554853,2.98500421534006,-11.8831479188507));
#60557=CARTESIAN_POINT('Ctrl Pts',(39.6453664732119,2.98751145272322,-11.8889865191699));
#60558=CARTESIAN_POINT('Ctrl Pts',(39.5953744137775,2.99171235742035,-11.8977498843862));
#60559=CARTESIAN_POINT('Ctrl Pts',(39.5753874572403,2.99339592300398,-11.9009939279241));
#60560=CARTESIAN_POINT('Ctrl Pts',(39.5359369224703,2.99672829471215,-11.9068868788602));
#60561=CARTESIAN_POINT('Ctrl Pts',(39.5164771107159,2.99837650361494,-11.9095504626825));
#60562=CARTESIAN_POINT('Ctrl Pts',(39.4733134089651,3.00204339664929,-11.9149208903469));
#60563=CARTESIAN_POINT('Ctrl Pts',(39.4495977867655,3.00406544448532,-11.9175139369221));
#60564=CARTESIAN_POINT('Ctrl Pts',(39.3659498788456,3.01122579609411,-11.9254027429996));
#60565=CARTESIAN_POINT('Ctrl Pts',(39.3058665057279,3.01642082563189,-11.9288019110123));
#60566=CARTESIAN_POINT('Ctrl Pts',(39.054815122709,3.03836252028959,-11.9335750476524));
#60567=CARTESIAN_POINT('Ctrl Pts',(38.8641699521223,3.05566399744824,-11.9144581833829));
#60568=CARTESIAN_POINT('Ctrl Pts',(38.6290865921099,3.07716316068664,-11.8621787236908));
#60569=CARTESIAN_POINT('Ctrl Pts',(38.5806876812645,3.08159348705176,-11.8498224571774));
#60570=CARTESIAN_POINT('Ctrl Pts',(38.5005527119162,3.08890408057551,-11.8266833892455));
#60571=CARTESIAN_POINT('Ctrl Pts',(38.4685948646137,3.09181275017041,-11.8167285602401));
#60572=CARTESIAN_POINT('Ctrl Pts',(38.4231341534709,3.09593137776711,-11.801519639642));
#60573=CARTESIAN_POINT('Ctrl Pts',(38.4094565463419,3.09716803149298,-11.7968061742998));
#60574=CARTESIAN_POINT('Ctrl Pts',(38.385667468893,3.09931357409833,-11.7883673052004));
#60575=CARTESIAN_POINT('Ctrl Pts',(38.3755373527822,3.10022545939116,-11.7846969689809));
#60576=CARTESIAN_POINT('Ctrl Pts',(38.3531844220573,3.10223362180757,-11.7764277338521));
#60577=CARTESIAN_POINT('Ctrl Pts',(38.3409739516825,3.10332806399974,-11.7717972174972));
#60578=CARTESIAN_POINT('Ctrl Pts',(38.3048679932787,3.10655853164049,-11.7577675487794));
#60579=CARTESIAN_POINT('Ctrl Pts',(38.2810835991834,3.10867903469059,-11.7480845791094));
#60580=CARTESIAN_POINT('Ctrl Pts',(38.1496523184013,3.12037993405315,-11.6921070144328));
#60581=CARTESIAN_POINT('Ctrl Pts',(38.0453301959829,3.12960803532082,-11.6383690251287));
#60582=CARTESIAN_POINT('Ctrl Pts',(37.8422994730021,3.14827064970736,-11.5142423013542));
#60583=CARTESIAN_POINT('Ctrl Pts',(37.7441649296903,3.15767913845184,-11.443587449918));
#60584=CARTESIAN_POINT('Ctrl Pts',(37.61410778873,3.17121318323613,-11.3342038262312));
#60585=CARTESIAN_POINT('Ctrl Pts',(37.5774445880302,3.17516038082164,-11.301396906555));
#60586=CARTESIAN_POINT('Ctrl Pts',(37.5135677938224,3.18231110088138,-11.2406106225289));
#60587=CARTESIAN_POINT('Ctrl Pts',(37.4859802322696,3.18549806088249,-11.2130489595003));
#60588=CARTESIAN_POINT('Ctrl Pts',(37.4439103533145,3.19052645065066,-11.1689236983109));
#60589=CARTESIAN_POINT('Ctrl Pts',(37.4289637705724,3.19234799799168,-11.1528103639527));
#60590=CARTESIAN_POINT('Ctrl Pts',(37.4013503441521,3.19578177623449,-11.1222108675222));
#60591=CARTESIAN_POINT('Ctrl Pts',(37.388632370381,3.19739170338147,-11.1077730110408));
#60592=CARTESIAN_POINT('Ctrl Pts',(37.3602800951101,3.20104704679235,-11.0747972902538));
#60593=CARTESIAN_POINT('Ctrl Pts',(37.3447504397159,3.20309649067993,-11.0561727354721));
#60594=CARTESIAN_POINT('Ctrl Pts',(37.2974130739272,3.20949556626997,-10.997623992221));
#60595=CARTESIAN_POINT('Ctrl Pts',(37.2665949206866,3.21388286375077,-10.956922621696));
#60596=CARTESIAN_POINT('Ctrl Pts',(37.0899392284347,3.24043460056447,-10.7075057900208));
#60597=CARTESIAN_POINT('Ctrl Pts',(36.9767368538911,3.2637794990598,-10.4777499316654));
#60598=CARTESIAN_POINT('Ctrl Pts',(36.891414135039,3.28915317443388,-10.2013801046984));
#60599=CARTESIAN_POINT('Ctrl Pts',(36.8818896588773,3.29217342893363,-10.1679802144486));
#60600=CARTESIAN_POINT('Ctrl Pts',(36.8693743213068,3.29641935880466,-10.1201908361976));
#60601=CARTESIAN_POINT('Ctrl Pts',(36.8657872940401,3.29767393292135,-10.1059640805097));
#60602=CARTESIAN_POINT('Ctrl Pts',(36.8597875743348,3.29983908640797,-10.0812151097051));
#60603=CARTESIAN_POINT('Ctrl Pts',(36.8573152090592,3.30075284748551,-10.0707081963452));
#60604=CARTESIAN_POINT('Ctrl Pts',(36.8520394891498,3.30275123796868,-10.0475908892303));
#60605=CARTESIAN_POINT('Ctrl Pts',(36.8492668711495,3.3038341714507,-10.0349740960656));
#60606=CARTESIAN_POINT('Ctrl Pts',(36.8415860633585,3.30693329365437,-9.99862829392094));
#60607=CARTESIAN_POINT('Ctrl Pts',(36.8369344027082,3.30893609846142,-9.97484572570892));
#60608=CARTESIAN_POINT('Ctrl Pts',(36.8074751123295,3.32257738167504,-9.81113353129821));
#60609=CARTESIAN_POINT('Ctrl Pts',(36.7947474293012,3.33367977743677,-9.66929336068567));
#60610=CARTESIAN_POINT('Ctrl Pts',(36.7944892164701,3.35641233410546,-9.37907680549902));
#60611=CARTESIAN_POINT('Ctrl Pts',(36.80802812903,3.36800478182511,-9.23133637198126));
#60612=CARTESIAN_POINT('Ctrl Pts',(36.84198593651,3.3830928610062,-9.04848998766378));
#60613=CARTESIAN_POINT('Ctrl Pts',(36.8497939599075,3.38619426873979,-9.01136260794192));
#60614=CARTESIAN_POINT('Ctrl Pts',(36.8635058466313,3.39113525916292,-8.95304643214434));
#60615=CARTESIAN_POINT('Ctrl Pts',(36.8688282008873,3.39295651163367,-8.9317262103934));
#60616=CARTESIAN_POINT('Ctrl Pts',(36.879310401868,3.39637473771534,-8.8920577326374));
#60617=CARTESIAN_POINT('Ctrl Pts',(36.88439772532,3.39796927828872,-8.87369194248652));
#60618=CARTESIAN_POINT('Ctrl Pts',(36.8964278011807,3.40160129842417,-8.83218566949044));
#60619=CARTESIAN_POINT('Ctrl Pts',(36.9035019326672,3.40364285899994,-8.80908582430155));
#60620=CARTESIAN_POINT('Ctrl Pts',(36.9253278805252,3.40968081381714,-8.74147030742588));
#60621=CARTESIAN_POINT('Ctrl Pts',(36.9410338389479,3.41370727263283,-8.69727835980132));
#60622=CARTESIAN_POINT('Ctrl Pts',(36.9580196850403,3.41777315288062,-8.65357747806631));
#60623=CARTESIAN_POINT('',(36.7973459100127,3.61022481984855,-9.52397861444782));
#60624=CARTESIAN_POINT('Ctrl Pts',(36.958019684865,3.68510631127449,-8.65357747851728));
#60625=CARTESIAN_POINT('Ctrl Pts',(36.9262879380075,3.67770817542144,-8.73521635066666));
#60626=CARTESIAN_POINT('Ctrl Pts',(36.8989808726309,3.67031003956838,-8.81868899500876));
#60627=CARTESIAN_POINT('Ctrl Pts',(36.8762923251079,3.66291190371533,-8.90352145165943));
#60628=CARTESIAN_POINT('Ctrl Pts',(36.8536674274252,3.65553452239341,-8.98811592162024));
#60629=CARTESIAN_POINT('Ctrl Pts',(36.8356353245951,3.6481571410715,-9.0740623070127));
#60630=CARTESIAN_POINT('Ctrl Pts',(36.8223411254775,3.64077975974958,-9.16086922568368));
#60631=CARTESIAN_POINT('Ctrl Pts',(36.8091047566171,3.63343447030892,-9.24729853105196));
#60632=CARTESIAN_POINT('Ctrl Pts',(36.8005652812803,3.62608918086826,-9.33458060440531));
#60633=CARTESIAN_POINT('Ctrl Pts',(36.7968171360163,3.6187438914276,-9.42221348991686));
#60634=CARTESIAN_POINT('Ctrl Pts',(36.7953681022262,3.61590420090125,-9.45609238288551));
#60635=CARTESIAN_POINT('Ctrl Pts',(36.7946346513946,3.6130645103749,-9.49002355151977));
#60636=CARTESIAN_POINT('Ctrl Pts',(36.7946202173455,3.61022481984855,-9.52397745573624));
#60637=CARTESIAN_POINT('Ctrl Pts',(36.79802585967,3.61022481984855,-9.52397890349931));
#60638=CARTESIAN_POINT('Ctrl Pts',(36.7998206443408,3.57126194121243,-9.98919550479405));
#60639=CARTESIAN_POINT('Ctrl Pts',(37.1539181706817,3.46543046208966,-11.2553513949631));
#60640=CARTESIAN_POINT('Ctrl Pts',(39.199922352963,3.29273038248022,-12.3631804573943));
#60641=CARTESIAN_POINT('Ctrl Pts',(41.5765986432995,3.09212458102024,-11.0764707285289));
#60642=CARTESIAN_POINT('Ctrl Pts',(41.7982659728439,2.89151877956026,-8.38294215354648));
#60643=CARTESIAN_POINT('Ctrl Pts',(39.663923518907,2.69091297810028,-6.72499042239298));
#60644=CARTESIAN_POINT('Ctrl Pts',(37.641017118746,2.53208515608523,-7.42250632947195));
#60645=CARTESIAN_POINT('Ctrl Pts',(37.0674493624832,2.44012593455684,-8.37484768228411));
#60646=CARTESIAN_POINT('Ctrl Pts',(36.9607077789649,2.41503531351511,-8.65459504792142));
#60647=CARTESIAN_POINT('Origin',(39.2,8.05522481984854,-9.525));
#60648=CARTESIAN_POINT('',(36.9547201749638,0.879636998740377,-8.65231241759342));
#60649=CARTESIAN_POINT('',(36.9580194911167,1.14613690893122,-8.65357797698964));
#60650=CARTESIAN_POINT('',(36.958019684865,8.05522481984854,-8.65357747851728));
#60651=CARTESIAN_POINT('',(36.7916962852456,2.07477346687626,-9.52369325357238));
#60652=CARTESIAN_POINT('Ctrl Pts',(36.7916962852457,2.07477346687626,-9.52369325357238));
#60653=CARTESIAN_POINT('Ctrl Pts',(36.7964605736323,2.01459014677707,-10.2374555183397));
#60654=CARTESIAN_POINT('Ctrl Pts',(37.5094020732034,1.88753822619121,-11.7525226440311));
#60655=CARTESIAN_POINT('Ctrl Pts',(40.0791495164278,1.69361770511871,-12.2235884022735));
#60656=CARTESIAN_POINT('Ctrl Pts',(41.9403077448524,1.49301190365872,-10.2639158886558));
#60657=CARTESIAN_POINT('Ctrl Pts',(41.3166585082413,1.29240610219874,-7.63422238696309));
#60658=CARTESIAN_POINT('Ctrl Pts',(38.7737033595216,1.09180030073876,-6.7190145399589));
#60659=CARTESIAN_POINT('Ctrl Pts',(37.294687387309,0.954210599585968,-7.83640380397085));
#60660=CARTESIAN_POINT('Ctrl Pts',(36.9710594620979,0.88348949891984,-8.60967633348487));
#60661=CARTESIAN_POINT('Ctrl Pts',(36.9547201749638,0.879636998740377,-8.65231241759342));
#60662=CARTESIAN_POINT('Ctrl Pts',(36.794620288083,2.0764482978049,-9.52382275830541));
#60663=CARTESIAN_POINT('Ctrl Pts',(36.7946428644169,2.08053459401905,-9.47769403564713));
#60664=CARTESIAN_POINT('Ctrl Pts',(36.795992380219,2.08458592142556,-9.43157101659339));
#60665=CARTESIAN_POINT('Ctrl Pts',(36.7995253989188,2.08986157364004,-9.37074928543718));
#60666=CARTESIAN_POINT('Ctrl Pts',(36.8005190234597,2.09113613178648,-9.3559950638613));
#60667=CARTESIAN_POINT('Ctrl Pts',(36.8024798154703,2.09333694017497,-9.33040225457211));
#60668=CARTESIAN_POINT('Ctrl Pts',(36.8033845640459,2.09426620326653,-9.31955953697378));
#60669=CARTESIAN_POINT('Ctrl Pts',(36.8053203262713,2.09609718322561,-9.29811766302057));
#60670=CARTESIAN_POINT('Ctrl Pts',(36.8063482070305,2.09699900452055,-9.28751852994192));
#60671=CARTESIAN_POINT('Ctrl Pts',(36.8087549017492,2.09896655299799,-9.26430713581487));
#60672=CARTESIAN_POINT('Ctrl Pts',(36.8101631450801,2.10003067570489,-9.25169848376381));
#60673=CARTESIAN_POINT('Ctrl Pts',(36.814422852703,2.10302222684463,-9.21611393439659));
#60674=CARTESIAN_POINT('Ctrl Pts',(36.8175064546258,2.10493765608338,-9.19316637618662));
#60675=CARTESIAN_POINT('Ctrl Pts',(36.8354221411912,2.11491213688721,-9.07301214974332));
#60676=CARTESIAN_POINT('Ctrl Pts',(36.8558750695435,2.12271844780597,-8.97672529577101));
#60677=CARTESIAN_POINT('Ctrl Pts',(36.9036373782248,2.1367776473617,-8.80456946622985));
#60678=CARTESIAN_POINT('Ctrl Pts',(36.9289561748562,2.14304029044836,-8.72835153425556));
#60679=CARTESIAN_POINT('Ctrl Pts',(36.9580197803105,2.14933799730903,-8.65357723295689));
#60680=CARTESIAN_POINT('',(36.7950466582253,2.34022481984855,-9.5271366580497));
#60681=CARTESIAN_POINT('Ctrl Pts',(36.9607077789649,2.41503531351511,-8.65459504792142));
#60682=CARTESIAN_POINT('Ctrl Pts',(36.8546204546155,2.39009848229292,-8.93262773711423));
#60683=CARTESIAN_POINT('Ctrl Pts',(36.7976786392064,2.36516165107074,-9.23032286919603));
#60684=CARTESIAN_POINT('Ctrl Pts',(36.7950466582253,2.34022481984855,-9.5271366580497));
#60685=CARTESIAN_POINT('Ctrl Pts',(36.7946209688343,2.34046868728881,-9.52715889521613));
#60686=CARTESIAN_POINT('Ctrl Pts',(36.7947400435394,2.32857689585436,-9.65982851088632));
#60687=CARTESIAN_POINT('Ctrl Pts',(36.8058349123456,2.31658147687662,-9.79226876623499));
#60688=CARTESIAN_POINT('Ctrl Pts',(36.8326453211439,2.30230139713442,-9.95201625881918));
#60689=CARTESIAN_POINT('Ctrl Pts',(36.8380214776574,2.29973526653512,-9.98081653738562));
#60690=CARTESIAN_POINT('Ctrl Pts',(36.8472368487234,2.29576207067078,-10.0256288057932));
#60691=CARTESIAN_POINT('Ctrl Pts',(36.8507163628563,2.29434017072281,-10.0417108301057));
#60692=CARTESIAN_POINT('Ctrl Pts',(36.8575826305807,2.29167626734596,-10.0719418772506));
#60693=CARTESIAN_POINT('Ctrl Pts',(36.8609332432784,2.29043256879513,-10.0860982893243));
#60694=CARTESIAN_POINT('Ctrl Pts',(36.8670133040976,2.28827123833547,-10.1107852223474));
#60695=CARTESIAN_POINT('Ctrl Pts',(36.8696860356687,2.28735060939581,-10.1213288498563));
#60696=CARTESIAN_POINT('Ctrl Pts',(36.8757206103207,2.2853351795214,-10.1444742459952));
#60697=CARTESIAN_POINT('Ctrl Pts',(36.879113528385,2.28424212113316,-10.157067269333));
#60698=CARTESIAN_POINT('Ctrl Pts',(36.8894696904373,2.28101929473666,-10.1942966639199));
#60699=CARTESIAN_POINT('Ctrl Pts',(36.8967242909894,2.27890494375835,-10.2188512116662));
#60700=CARTESIAN_POINT('Ctrl Pts',(36.9401666988732,2.26698823476297,-10.3576922777341));
#60701=CARTESIAN_POINT('Ctrl Pts',(36.9844711293871,2.25755590213781,-10.4692791894704));
#60702=CARTESIAN_POINT('Ctrl Pts',(37.0894571621821,2.23873678258408,-10.6851246198109));
#60703=CARTESIAN_POINT('Ctrl Pts',(37.1500083590448,2.22937425769,-10.7890459768646));
#60704=CARTESIAN_POINT('Ctrl Pts',(37.2454061747055,2.21595826891165,-10.9277629845139));
#60705=CARTESIAN_POINT('Ctrl Pts',(37.2739353778813,2.21208423479084,-10.9666849705437));
#60706=CARTESIAN_POINT('Ctrl Pts',(37.3268187951704,2.20511005077166,-11.0344594979671));
#60707=CARTESIAN_POINT('Ctrl Pts',(37.3507185338563,2.20202651123457,-11.0636466626651));
#60708=CARTESIAN_POINT('Ctrl Pts',(37.376616078177,2.19874870273732,-11.0937983105499));
#60709=CARTESIAN_POINT('Ctrl Pts',(37.377940737037,2.19858121299482,-11.0953366224305));
#60710=CARTESIAN_POINT('Ctrl Pts',(37.3805377062933,2.1982531833163,-11.098344744584));
#60711=CARTESIAN_POINT('Ctrl Pts',(37.3818098545768,2.19809264985278,-11.0998146934072));
#60712=CARTESIAN_POINT('Ctrl Pts',(37.384322461092,2.19777588533278,-11.1027108708453));
#60713=CARTESIAN_POINT('Ctrl Pts',(37.3855628214642,2.1976196582312,-11.1041371828893));
#60714=CARTESIAN_POINT('Ctrl Pts',(37.3880323178237,2.19730890486403,-11.1069701490903));
#60715=CARTESIAN_POINT('Ctrl Pts',(37.3892614138223,2.19715438026564,-11.1083768364957));
#60716=CARTESIAN_POINT('Ctrl Pts',(37.4038685189948,2.19531960547662,-11.1250552630066));
#60717=CARTESIAN_POINT('Ctrl Pts',(37.4174372874199,2.19363176324731,-11.1401579689667));
#60718=CARTESIAN_POINT('Ctrl Pts',(37.4444732105396,2.19029928296955,-11.169494612909));
#60719=CARTESIAN_POINT('Ctrl Pts',(37.4579263597775,2.1886553204599,-11.1837393477971));
#60720=CARTESIAN_POINT('Ctrl Pts',(37.4880158575952,2.18500837523973,-11.2148294922942));
#60721=CARTESIAN_POINT('Ctrl Pts',(37.504729710748,2.18300215677346,-11.2315966064477));
#60722=CARTESIAN_POINT('Ctrl Pts',(37.5639278293328,2.17596113548381,-11.2892555601365));
#60723=CARTESIAN_POINT('Ctrl Pts',(37.6076623265019,2.17087207545387,-11.328826292137));
#60724=CARTESIAN_POINT('Ctrl Pts',(37.7986801406776,2.14908601010405,-11.4892947424074));
#60725=CARTESIAN_POINT('Ctrl Pts',(37.9585879618252,2.13183066697992,-11.5940642144541));
#60726=CARTESIAN_POINT('Ctrl Pts',(38.1749984932429,2.11024416202486,-11.7016597976445));
#60727=CARTESIAN_POINT('Ctrl Pts',(38.2215783796094,2.10569755735421,-11.7229917733082));
#60728=CARTESIAN_POINT('Ctrl Pts',(38.3002127148904,2.09821943068981,-11.7560078408592));
#60729=CARTESIAN_POINT('Ctrl Pts',(38.3318974393323,2.09525797090332,-11.7685265627328));
#60730=CARTESIAN_POINT('Ctrl Pts',(38.3774933685387,2.09107921806147,-11.7854308952045));
#60731=CARTESIAN_POINT('Ctrl Pts',(38.3911932595905,2.08983419461535,-11.7903689943565));
#60732=CARTESIAN_POINT('Ctrl Pts',(38.4152044322017,2.08767142175088,-11.7987781764741));
#60733=CARTESIAN_POINT('Ctrl Pts',(38.4254956018953,2.08675066153383,-11.8023041597437));
#60734=CARTESIAN_POINT('Ctrl Pts',(38.4481667503727,2.08473597486478,-11.8099003285157));
#60735=CARTESIAN_POINT('Ctrl Pts',(38.4605563330619,2.08364378054945,-11.813939893098));
#60736=CARTESIAN_POINT('Ctrl Pts',(38.4965974030559,2.08049039012895,-11.8253677239408));
#60737=CARTESIAN_POINT('Ctrl Pts',(38.5203319403836,2.07844330623803,-11.8324917882686));
#60738=CARTESIAN_POINT('Ctrl Pts',(38.6953177431574,2.06353687657041,-11.8820803705232));
#60739=CARTESIAN_POINT('Ctrl Pts',(38.8503192082428,2.05133023528189,-11.910009688668));
#60740=CARTESIAN_POINT('Ctrl Pts',(39.1023961537837,2.03151271800208,-11.9303053486253));
#60741=CARTESIAN_POINT('Ctrl Pts',(39.198200580388,2.02399169609359,-11.9322837239946));
#60742=CARTESIAN_POINT('Ctrl Pts',(39.3558562700161,2.01136816840761,-11.9261269886454));
#60743=CARTESIAN_POINT('Ctrl Pts',(39.4177273710073,2.00635210580562,-11.921308734444));
#60744=CARTESIAN_POINT('Ctrl Pts',(39.5051753835021,1.9991301002889,-11.9110841569755));
#60745=CARTESIAN_POINT('Ctrl Pts',(39.5309605774057,1.99698425681486,-11.9076444568596));
#60746=CARTESIAN_POINT('Ctrl Pts',(39.5759126191522,1.99321171537021,-11.9009041864067));
#60747=CARTESIAN_POINT('Ctrl Pts',(39.5951050407562,1.99159088401517,-11.8977880141869));
#60748=CARTESIAN_POINT('Ctrl Pts',(39.634978845187,1.98820109927326,-11.8908167445802));
#60749=CARTESIAN_POINT('Ctrl Pts',(39.6556515518141,1.9864310434394,-11.8869223246682));
#60750=CARTESIAN_POINT('Ctrl Pts',(39.7099895429765,1.98174354492301,-11.8759459850876));
#60751=CARTESIAN_POINT('Ctrl Pts',(39.743557288639,1.97881220858396,-11.8684123773041));
#60752=CARTESIAN_POINT('Ctrl Pts',(39.9665430338727,1.95908893346371,-11.8133191295738));
#60753=CARTESIAN_POINT('Ctrl Pts',(40.1496872105402,1.94158340537125,-11.7435701355292));
#60754=CARTESIAN_POINT('Ctrl Pts',(40.4114493899048,1.91500294868688,-11.6054790185491));
#60755=CARTESIAN_POINT('Ctrl Pts',(40.4975245077499,1.90599068977397,-11.5529144923378));
#60756=CARTESIAN_POINT('Ctrl Pts',(40.6009303788976,1.8949959212425,-11.4804785886176));
#60757=CARTESIAN_POINT('Ctrl Pts',(40.6215713004806,1.89279258676314,-11.4655250918808));
#60758=CARTESIAN_POINT('Ctrl Pts',(40.6523918657946,1.88949375288289,-11.4424410805384));
#60759=CARTESIAN_POINT('Ctrl Pts',(40.6627487109272,1.88838367714842,-11.4345519532382));
#60760=CARTESIAN_POINT('Ctrl Pts',(40.6816425666914,1.88635645907412,-11.4199159937446));
#60761=CARTESIAN_POINT('Ctrl Pts',(40.6901982555449,1.8854377494618,-11.4131950344742));
#60762=CARTESIAN_POINT('Ctrl Pts',(40.7099156294973,1.8833184244059,-11.3974884593112));
#60763=CARTESIAN_POINT('Ctrl Pts',(40.7210430674846,1.88212074200149,-11.388460827825));
#60764=CARTESIAN_POINT('Ctrl Pts',(40.7569443769672,1.87824860134461,-11.3587984131553));
#60765=CARTESIAN_POINT('Ctrl Pts',(40.7813855826859,1.875599986479,-11.3377637334425));
#60766=CARTESIAN_POINT('Ctrl Pts',(40.9313434889073,1.85921399351496,-11.2033642007105));
#60767=CARTESIAN_POINT('Ctrl Pts',(41.0450496829803,1.84615659445709,-11.0775024878716));
#60768=CARTESIAN_POINT('Ctrl Pts',(41.1923623961085,1.8264958525073,-10.8751573614344));
#60769=CARTESIAN_POINT('Ctrl Pts',(41.2367538226658,1.82008883345694,-10.8072109784109));
#60770=CARTESIAN_POINT('Ctrl Pts',(41.3057046993631,1.80910655403755,-10.6890297457104));
#60771=CARTESIAN_POINT('Ctrl Pts',(41.3321004271938,1.80458972089338,-10.6399459078541));
#60772=CARTESIAN_POINT('Ctrl Pts',(41.3678497161436,1.79795891390863,-10.5675484016691));
#60773=CARTESIAN_POINT('Ctrl Pts',(41.3785814092291,1.79589195075207,-10.5449326001782));
#60774=CARTESIAN_POINT('Ctrl Pts',(41.3969648497864,1.79220871283113,-10.5045771845527));
#60775=CARTESIAN_POINT('Ctrl Pts',(41.4047596375407,1.79059744226602,-10.4869048323351));
#60776=CARTESIAN_POINT('Ctrl Pts',(41.4207793502108,1.7871772575346,-10.4493669463424));
#60777=CARTESIAN_POINT('Ctrl Pts',(41.4289523786941,1.78536676824761,-10.4294812894409));
#60778=CARTESIAN_POINT('Ctrl Pts',(41.450336383206,1.7804449708229,-10.3754015358862));
#60779=CARTESIAN_POINT('Ctrl Pts',(41.4630334829072,1.77731713565773,-10.3410121004777));
#60780=CARTESIAN_POINT('Ctrl Pts',(41.549789634235,1.75434161588809,-10.0884166133304));
#60781=CARTESIAN_POINT('Ctrl Pts',(41.5929222463608,1.73346997903445,-9.86089314047946));
#60782=CARTESIAN_POINT('Ctrl Pts',(41.6052362710042,1.70847865178618,-9.5811874317746));
#60783=CARTESIAN_POINT('Ctrl Pts',(41.6058837690946,1.70407382780111,-9.5315213236654));
#60784=CARTESIAN_POINT('Ctrl Pts',(41.6043955371354,1.69680023428862,-9.44854006518988));
#60785=CARTESIAN_POINT('Ctrl Pts',(41.6031050839378,1.6939033911853,-9.41522611723576));
#60786=CARTESIAN_POINT('Ctrl Pts',(41.6002635290381,1.68979846725851,-9.36753093260855));
#60787=CARTESIAN_POINT('Ctrl Pts',(41.5992747830038,1.68856391772154,-9.35312195010786));
#60788=CARTESIAN_POINT('Ctrl Pts',(41.5973146181204,1.68641249807119,-9.32788662092796));
#60789=CARTESIAN_POINT('Ctrl Pts',(41.5963995258212,1.6854927261872,-9.31705675260254));
#60790=CARTESIAN_POINT('Ctrl Pts',(41.5942180559602,1.6834719550875,-9.29317056336822));
#60791=CARTESIAN_POINT('Ctrl Pts',(41.5929182561159,1.68237277178815,-9.28011792335826));
#60792=CARTESIAN_POINT('Ctrl Pts',(41.5888108421018,1.6791786552033,-9.24203332268636));
#60793=CARTESIAN_POINT('Ctrl Pts',(41.5857166348505,1.67709839029302,-9.21703300455705));
#60794=CARTESIAN_POINT('Ctrl Pts',(41.5655314131988,1.66515052520939,-9.07259445664102));
#60795=CARTESIAN_POINT('Ctrl Pts',(41.5398635816816,1.6556590586849,-8.95451196636151));
#60796=CARTESIAN_POINT('Ctrl Pts',(41.4706339600697,1.63663195974076,-8.72190661007857));
#60797=CARTESIAN_POINT('Ctrl Pts',(41.4269877301973,1.62712194190069,-8.60779730773873));
#60798=CARTESIAN_POINT('Ctrl Pts',(41.3453788571499,1.61188543873575,-8.43505925195847));
#60799=CARTESIAN_POINT('Ctrl Pts',(41.3132094432504,1.60631773809732,-8.37392855113639));
#60800=CARTESIAN_POINT('Ctrl Pts',(41.2648701004603,1.59844866979959,-8.2909444207743));
#60801=CARTESIAN_POINT('Ctrl Pts',(41.2508909531929,1.59622379619392,-8.26784929972541));
#60802=CARTESIAN_POINT('Ctrl Pts',(41.2260987123891,1.59235970099989,-8.22840408735314));
#60803=CARTESIAN_POINT('Ctrl Pts',(41.215468751679,1.5907272275393,-8.21194150309085));
#60804=CARTESIAN_POINT('Ctrl Pts',(41.1932141706266,1.587357235067,-8.17838292145843));
#60805=CARTESIAN_POINT('Ctrl Pts',(41.1815679505563,1.58561901852911,-8.16130330117273));
#60806=CARTESIAN_POINT('Ctrl Pts',(41.1509760454334,1.58111573552117,-8.11765854293112));
#60807=CARTESIAN_POINT('Ctrl Pts',(41.1317080156562,1.57833872179343,-8.09132590019964));
#60808=CARTESIAN_POINT('Ctrl Pts',(41.0306625536036,1.56406150524204,-7.95896822861512));
#60809=CARTESIAN_POINT('Ctrl Pts',(40.9406851150666,1.55224732558697,-7.8595320174475));
#60810=CARTESIAN_POINT('Ctrl Pts',(40.750125645472,1.52889044449982,-7.68133382446457));
#60811=CARTESIAN_POINT('Ctrl Pts',(40.6505987696114,1.51740312845915,-7.60204421639064));
#60812=CARTESIAN_POINT('Ctrl Pts',(40.5008249878311,1.50138781696076,-7.50099847548984));
#60813=CARTESIAN_POINT('Ctrl Pts',(40.4553818979142,1.49668121011021,-7.47250267337171));
#60814=CARTESIAN_POINT('Ctrl Pts',(40.3942068344256,1.49057579774779,-7.43693472807056));
#60815=CARTESIAN_POINT('Ctrl Pts',(40.3793015829086,1.48910573290188,-7.42848041460376));
#60816=CARTESIAN_POINT('Ctrl Pts',(40.3544395103012,1.48668401037931,-7.41472762135667));
#60817=CARTESIAN_POINT('Ctrl Pts',(40.3445337450035,1.48572701258392,-7.40933872654418));
#60818=CARTESIAN_POINT('Ctrl Pts',(40.3241425892816,1.48377363709274,-7.39843075236286));
#60819=CARTESIAN_POINT('Ctrl Pts',(40.3136536933724,1.48277770722045,-7.39291913943464));
#60820=CARTESIAN_POINT('Ctrl Pts',(40.2854896298321,1.48012590913586,-7.3783842895138));
#60821=CARTESIAN_POINT('Ctrl Pts',(40.2677422823334,1.4784783038809,-7.36950162559412));
#60822=CARTESIAN_POINT('Ctrl Pts',(40.1730821743144,1.46980254836655,-7.3235797439198));
#60823=CARTESIAN_POINT('Ctrl Pts',(40.0943382913222,1.46297378865537,-7.29043000036356));
#60824=CARTESIAN_POINT('Ctrl Pts',(39.8701178196111,1.44413333011074,-7.20979578049084));
#60825=CARTESIAN_POINT('Ctrl Pts',(39.7216439673208,1.43231794383814,-7.1718920591141));
#60826=CARTESIAN_POINT('Ctrl Pts',(39.4914572436794,1.41381968701357,-7.13600072593955));
#60827=CARTESIAN_POINT('Ctrl Pts',(39.4117806685749,1.40738939731695,-7.12762406269919));
#60828=CARTESIAN_POINT('Ctrl Pts',(39.3035473351996,1.39852002183734,-7.12168273460529));
#60829=CARTESIAN_POINT('Ctrl Pts',(39.2752289765789,1.39618728925874,-7.12062973052066));
#60830=CARTESIAN_POINT('Ctrl Pts',(39.2270738331035,1.39219595757192,-7.11969062893248));
#60831=CARTESIAN_POINT('Ctrl Pts',(39.2072444800568,1.39054534688547,-7.11954918338567));
#60832=CARTESIAN_POINT('Ctrl Pts',(39.1671253505563,1.3871902028988,-7.11975906946439));
#60833=CARTESIAN_POINT('Ctrl Pts',(39.1468372859804,1.38548544821828,-7.12012196809199));
#60834=CARTESIAN_POINT('Ctrl Pts',(39.0958297425447,1.38117766932851,-7.12168010022112));
#60835=CARTESIAN_POINT('Ctrl Pts',(39.0651250060043,1.37856465251525,-7.12320764195388));
#60836=CARTESIAN_POINT('Ctrl Pts',(38.935328691325,1.36742857749919,-7.13216157729807));
#60837=CARTESIAN_POINT('Ctrl Pts',(38.8367324454893,1.35874062211037,-7.14513493868336));
#60838=CARTESIAN_POINT('Ctrl Pts',(38.5891036736733,1.33634060039277,-7.19346483389981));
#60839=CARTESIAN_POINT('Ctrl Pts',(38.4421211043393,1.32248009416662,-7.23701700237172));
#60840=CARTESIAN_POINT('Ctrl Pts',(38.2408367716864,1.30316217524171,-7.31819998710583));
#60841=CARTESIAN_POINT('Ctrl Pts',(38.1823746023508,1.29751290078044,-7.34454115449899));
#60842=CARTESIAN_POINT('Ctrl Pts',(38.1088234542154,1.29040976336842,-7.38128480584249));
#60843=CARTESIAN_POINT('Ctrl Pts',(38.0927095441383,1.28885389201232,-7.38956351182441));
#60844=CARTESIAN_POINT('Ctrl Pts',(38.0665414744774,1.2863294944245,-7.40338353292633));
#60845=CARTESIAN_POINT('Ctrl Pts',(38.0564311078605,1.28535471802544,-7.40881596495931));
#60846=CARTESIAN_POINT('Ctrl Pts',(38.0374174653899,1.28352312061498,-7.41920830906761));
#60847=CARTESIAN_POINT('Ctrl Pts',(38.0285061678416,1.28266534038573,-7.42415278788716));
#60848=CARTESIAN_POINT('Ctrl Pts',(38.0045508123893,1.28036045163073,-7.43764436599053));
#60849=CARTESIAN_POINT('Ctrl Pts',(37.9895666910195,1.2789198076572,-7.44629762567028));
#60850=CARTESIAN_POINT('Ctrl Pts',(37.9308171218171,1.27327009498406,-7.48107594702161));
#60851=CARTESIAN_POINT('Ctrl Pts',(37.8877895037524,1.26912945984383,-7.50842980071317));
#60852=CARTESIAN_POINT('Ctrl Pts',(37.7222553254481,1.25305002445776,-7.6212087952406));
#60853=CARTESIAN_POINT('Ctrl Pts',(37.6069383231159,1.24149802493233,-7.71659951976353));
#60854=CARTESIAN_POINT('Ctrl Pts',(37.4460946917407,1.22363652651139,-7.87705317692599));
#60855=CARTESIAN_POINT('Ctrl Pts',(37.3936895317247,1.21747970701409,-7.93466874949074));
#60856=CARTESIAN_POINT('Ctrl Pts',(37.3096939639634,1.20687369954705,-8.03653327829339));
#60857=CARTESIAN_POINT('Ctrl Pts',(37.2766410287909,1.20247743860365,-8.07949679830634));
#60858=CARTESIAN_POINT('Ctrl Pts',(37.2306305190634,1.19599026716638,-8.14367783178097));
#60859=CARTESIAN_POINT('Ctrl Pts',(37.2165043843074,1.19394344969863,-8.16403999542309));
#60860=CARTESIAN_POINT('Ctrl Pts',(37.1919482985418,1.19028258389804,-8.20063098099402));
#60861=CARTESIAN_POINT('Ctrl Pts',(37.1813940562603,1.18867332143248,-8.21677412790836));
#60862=CARTESIAN_POINT('Ctrl Pts',(37.159413160891,1.18524317847799,-8.25129417979092));
#60863=CARTESIAN_POINT('Ctrl Pts',(37.1480381649779,1.18342058771624,-8.26970173809325));
#60864=CARTESIAN_POINT('Ctrl Pts',(37.1177171145653,1.17842825877582,-8.32028224180602));
#60865=CARTESIAN_POINT('Ctrl Pts',(37.0992701728661,1.17524116478516,-8.35274544119012));
#60866=CARTESIAN_POINT('Ctrl Pts',(37.03491536889,1.16354744521854,-8.47239857175206));
#60867=CARTESIAN_POINT('Ctrl Pts',(36.9936571723966,1.15489698158361,-8.56188992607809));
#60868=CARTESIAN_POINT('Ctrl Pts',(36.9580194911167,1.14613690893122,-8.65357797698964));
#60869=CARTESIAN_POINT('Origin',(39.2,8.05522481984854,-9.525));
#60870=CARTESIAN_POINT('',(36.9580196850438,-0.392176638896471,-8.65357747805726));
#60871=CARTESIAN_POINT('',(36.958019684865,-0.127039975641408,-8.65357747851736));
#60872=CARTESIAN_POINT('',(36.958019684865,8.05522481984854,-8.65357747851728));
#60873=CARTESIAN_POINT('',(36.7978958045452,0.804628829011641,-9.52411276591516));
#60874=CARTESIAN_POINT('Ctrl Pts',(36.9580196850438,-0.392176638896471,
-8.65357747805726));
#60875=CARTESIAN_POINT('Ctrl Pts',(36.9824700011476,-0.386309940922915,
-8.59067214107231));
#60876=CARTESIAN_POINT('Ctrl Pts',(37.0095550481929,-0.380366550251713,
-8.52882859886102));
#60877=CARTESIAN_POINT('Ctrl Pts',(37.0798337986663,-0.366146063000361,
-8.38513105426349));
#60878=CARTESIAN_POINT('Ctrl Pts',(37.1252210655968,-0.357829720603997,
-8.30446870225221));
#60879=CARTESIAN_POINT('Ctrl Pts',(37.2323529907576,-0.33999812850501,-8.13739264459349));
#60880=CARTESIAN_POINT('Ctrl Pts',(37.2954118399697,-0.330502896895357,
-8.05203097106307));
#60881=CARTESIAN_POINT('Ctrl Pts',(37.3805242936423,-0.319026760440954,
-7.95146162160763));
#60882=CARTESIAN_POINT('Ctrl Pts',(37.3974598869159,-0.316802027590474,
-7.93208940090425));
#60883=CARTESIAN_POINT('Ctrl Pts',(37.4234620368301,-0.31347777291652,-7.90329207603053));
#60884=CARTESIAN_POINT('Ctrl Pts',(37.4322992181859,-0.312363354983257,
-7.89366383116365));
#60885=CARTESIAN_POINT('Ctrl Pts',(37.4486347512679,-0.31033201845608,-7.87615464087459));
#60886=CARTESIAN_POINT('Ctrl Pts',(37.4561084298851,-0.309413486556029,
-7.86825214501251));
#60887=CARTESIAN_POINT('Ctrl Pts',(37.4736824395626,-0.307278330162745,
-7.84992048601222));
#60888=CARTESIAN_POINT('Ctrl Pts',(37.4838239626568,-0.30606482531752,-7.83953165580069));
#60889=CARTESIAN_POINT('Ctrl Pts',(37.517871957053,-0.302049447567075,-7.80527935389552));
#60890=CARTESIAN_POINT('Ctrl Pts',(37.5421883520759,-0.299276382565353,
-7.78182624570433));
#60891=CARTESIAN_POINT('Ctrl Pts',(37.604144891096,-0.292416607127595,-7.72453900275184));
#60892=CARTESIAN_POINT('Ctrl Pts',(37.6423748838302,-0.288364930964759,
-7.69136478226724));
#60893=CARTESIAN_POINT('Ctrl Pts',(37.8324258291359,-0.268912148770531,
-7.53668458011679));
#60894=CARTESIAN_POINT('Ctrl Pts',(37.9975466935135,-0.25399723009004,-7.43268887387241));
#60895=CARTESIAN_POINT('Ctrl Pts',(38.2248916447087,-0.233846072046994,
-7.32539546500609));
#60896=CARTESIAN_POINT('Ctrl Pts',(38.2772383296457,-0.229235395443278,
-7.30292746624488));
#60897=CARTESIAN_POINT('Ctrl Pts',(38.3521120456911,-0.222647549127527,
-7.273892537794));
#60898=CARTESIAN_POINT('Ctrl Pts',(38.3740159980717,-0.220721217710182,
-7.26576359349363));
#60899=CARTESIAN_POINT('Ctrl Pts',(38.4144336636024,-0.217166047922567,
-7.25143020885292));
#60900=CARTESIAN_POINT('Ctrl Pts',(38.4329113786508,-0.2155404876216,-7.24512959491965));
#60901=CARTESIAN_POINT('Ctrl Pts',(38.4708711083746,-0.212199246849162,
-7.23269961397555));
#60902=CARTESIAN_POINT('Ctrl Pts',(38.4903585290173,-0.210483008232813,
-7.22659208842799));
#60903=CARTESIAN_POINT('Ctrl Pts',(38.5399795687589,-0.20610907898399,-7.21173163143301));
#60904=CARTESIAN_POINT('Ctrl Pts',(38.5702100891409,-0.203440751933646,
-7.20331914704168));
#60905=CARTESIAN_POINT('Ctrl Pts',(38.7141037477106,-0.190715810032737,
-7.16629377441332));
#60906=CARTESIAN_POINT('Ctrl Pts',(38.8295751616615,-0.180422588450311,
-7.14542717721622));
#60907=CARTESIAN_POINT('Ctrl Pts',(39.0970803739772,-0.156427354476174,
-7.11703077089765));
#60908=CARTESIAN_POINT('Ctrl Pts',(39.249247079007,-0.14265958054726,-7.11533550900872));
#60909=CARTESIAN_POINT('Ctrl Pts',(39.4487782514335,-0.124947326710104,
-7.13203034026109));
#60910=CARTESIAN_POINT('Ctrl Pts',(39.4968704293992,-0.120707318125235,
-7.13751947798899));
#60911=CARTESIAN_POINT('Ctrl Pts',(39.5615883129148,-0.115066374116952,
-7.14689241725424));
#60912=CARTESIAN_POINT('Ctrl Pts',(39.5783825476538,-0.11360851904779,-7.14950668664864));
#60913=CARTESIAN_POINT('Ctrl Pts',(39.6051482703157,-0.111296011342877,
-7.1539642359262));
#60914=CARTESIAN_POINT('Ctrl Pts',(39.6151378246616,-0.110435375569327,
-7.15569286195205));
#60915=CARTESIAN_POINT('Ctrl Pts',(39.6364936746104,-0.108601134750289,
-7.15952756702325));
#60916=CARTESIAN_POINT('Ctrl Pts',(39.6478563971483,-0.107628623607068,
-7.16165253841174));
#60917=CARTESIAN_POINT('Ctrl Pts',(39.6773554991746,-0.105111699880287,
-7.16738963757558));
#60918=CARTESIAN_POINT('Ctrl Pts',(39.6954668118991,-0.103574134305051,
-7.17112923115936));
#60919=CARTESIAN_POINT('Ctrl Pts',(39.7807839217993,-0.0963596716489415,
-7.18977377814061));
#60920=CARTESIAN_POINT('Ctrl Pts',(39.8473803774488,-0.0908119398858467,
-7.20735195952669));
#60921=CARTESIAN_POINT('Ctrl Pts',(40.089742885649,-0.0706168713194944,
-7.28258940027681));
#60922=CARTESIAN_POINT('Ctrl Pts',(40.2594373998762,-0.0564204594033885,
-7.35759490718814));
#60923=CARTESIAN_POINT('Ctrl Pts',(40.4781839297072,-0.0361935463108925,
-7.48616878476222));
#60924=CARTESIAN_POINT('Ctrl Pts',(40.535971204172,-0.0306493270394711,
-7.52355896645561));
#60925=CARTESIAN_POINT('Ctrl Pts',(40.6146472762807,-0.0227501733217693,
-7.57939153025153));
#60926=CARTESIAN_POINT('Ctrl Pts',(40.6369431528341,-0.0204700991323039,
-7.5957997819905));
#60927=CARTESIAN_POINT('Ctrl Pts',(40.674469987915,-0.0165570758753307,
-7.62442844014172));
#60928=CARTESIAN_POINT('Ctrl Pts',(40.6898447821298,-0.0149316442030096,
-7.63645651957838));
#60929=CARTESIAN_POINT('Ctrl Pts',(40.7210033522578,-0.0115903008130991,
-7.66144991700499));
#60930=CARTESIAN_POINT('Ctrl Pts',(40.7367717251884,-0.00987382761739585,
-7.67443178483092));
#60931=CARTESIAN_POINT('Ctrl Pts',(40.7763509682222,-0.00549852460097494,
-7.70787150371802));
#60932=CARTESIAN_POINT('Ctrl Pts',(40.7999294223589,-0.00282904475207008,
-7.72859692986818));
#60933=CARTESIAN_POINT('Ctrl Pts',(40.9097713077327,0.00991763226400466,
-7.82902584926393));
#60934=CARTESIAN_POINT('Ctrl Pts',(40.990512393684,0.0202324733536286,-7.9145023387958));
#60935=CARTESIAN_POINT('Ctrl Pts',(41.1611749597574,0.0443321356235607,
-8.12393604805064));
#60936=CARTESIAN_POINT('Ctrl Pts',(41.2461699790002,0.0581845503089543,
-8.25127477728285));
#60937=CARTESIAN_POINT('Ctrl Pts',(41.3409912235909,0.075887375701987,-8.42761140179743));
#60938=CARTESIAN_POINT('Ctrl Pts',(41.3622272930147,0.0800440322162215,
-8.47006913568574));
#60939=CARTESIAN_POINT('Ctrl Pts',(41.389295523635,0.0855937102356448,-8.52844444831731));
#60940=CARTESIAN_POINT('Ctrl Pts',(41.3962350805101,0.087041422994478,-8.54383264497544));
#60941=CARTESIAN_POINT('Ctrl Pts',(41.4074756941205,0.0894272976914303,
-8.56947522406712));
#60942=CARTESIAN_POINT('Ctrl Pts',(41.4118685649977,0.0903706465163295,
-8.57968840545864));
#60943=CARTESIAN_POINT('Ctrl Pts',(41.4208148339292,0.0923143529480128,
-8.60089182727806));
#60944=CARTESIAN_POINT('Ctrl Pts',(41.4253577904836,0.0933141033867259,
-8.61188600670741));
#60945=CARTESIAN_POINT('Ctrl Pts',(41.4373402732732,0.0959870570085815,
-8.64150487203092));
#60946=CARTESIAN_POINT('Ctrl Pts',(41.4446289781568,0.0976517695544874,
-8.66019021114716));
#60947=CARTESIAN_POINT('Ctrl Pts',(41.486120137049,0.107376546012066,-8.77061709439323));
#60948=CARTESIAN_POINT('Ctrl Pts',(41.5149340903055,0.115171272698597,-8.86429986033626));
#60949=CARTESIAN_POINT('Ctrl Pts',(41.5852992690839,0.138756574336345,-9.15520772328607));
#60950=CARTESIAN_POINT('Ctrl Pts',(41.6078737843295,0.154268658548737,-9.35607415626702));
#60951=CARTESIAN_POINT('Ctrl Pts',(41.6046596616596,0.173637730729523,-9.59467472712521));
#60952=CARTESIAN_POINT('Ctrl Pts',(41.6032910858076,0.176686573432366,-9.63193135170431));
#60953=CARTESIAN_POINT('Ctrl Pts',(41.5997490696134,0.181562940191475,-9.69093393179105));
#60954=CARTESIAN_POINT('Ctrl Pts',(41.5981440539688,0.183372951168642,-9.71270907902687));
#60955=CARTESIAN_POINT('Ctrl Pts',(41.5947335376811,0.186636444317341,-9.75172597356677));
#60956=CARTESIAN_POINT('Ctrl Pts',(41.593037622082,0.188086427460028,-9.76897600185936));
#60957=CARTESIAN_POINT('Ctrl Pts',(41.5886036386034,0.191516053599071,-9.80956601547673));
#60958=CARTESIAN_POINT('Ctrl Pts',(41.5857097125691,0.193500403577372,-9.83288673675066));
#60959=CARTESIAN_POINT('Ctrl Pts',(41.5760233404407,0.199473986966623,-9.90257361123265));
#60960=CARTESIAN_POINT('Ctrl Pts',(41.5682176100226,0.203493951617044,-9.94878466795191));
#60961=CARTESIAN_POINT('Ctrl Pts',(41.5467265996124,0.213029429211386,-10.0567152127004));
#60962=CARTESIAN_POINT('Ctrl Pts',(41.5319485023178,0.218574214077954,-10.1181792385115));
#60963=CARTESIAN_POINT('Ctrl Pts',(41.4876280889811,0.233017307224677,-10.2750505902207));
#60964=CARTESIAN_POINT('Ctrl Pts',(41.4545347448964,0.241985899040003,-10.3693273678396));
#60965=CARTESIAN_POINT('Ctrl Pts',(41.3691192749965,0.261705276006662,-10.5714633515747));
#60966=CARTESIAN_POINT('Ctrl Pts',(41.3143933968707,0.27243248852972,-10.6780445073195));
#60967=CARTESIAN_POINT('Ctrl Pts',(41.2411710375347,0.284593398051113,-10.797753290145));
#60968=CARTESIAN_POINT('Ctrl Pts',(41.2301587551715,0.28637319423434,-10.8152463558918));
#60969=CARTESIAN_POINT('Ctrl Pts',(41.2123838781288,0.289167327081202,-10.8426906748621));
#60970=CARTESIAN_POINT('Ctrl Pts',(41.2057701304724,0.290190487643724,-10.8527363408446));
#60971=CARTESIAN_POINT('Ctrl Pts',(41.1928658067752,0.292154745363263,-10.8720203106328));
#60972=CARTESIAN_POINT('Ctrl Pts',(41.1865857964016,0.293096413512395,-10.8812649900538));
#60973=CARTESIAN_POINT('Ctrl Pts',(41.1708198874341,0.295426242104155,-10.9041292074058));
#60974=CARTESIAN_POINT('Ctrl Pts',(41.1612567654965,0.296809408614601,-10.9176953532194));
#60975=CARTESIAN_POINT('Ctrl Pts',(41.1230613070618,0.30222214882506,-10.9707052361892));
#60976=CARTESIAN_POINT('Ctrl Pts',(41.0933709212187,0.306188584640413,-11.0093772795345));
#60977=CARTESIAN_POINT('Ctrl Pts',(40.9149465872621,0.328864566832165,-11.2277033991101));
#60978=CARTESIAN_POINT('Ctrl Pts',(40.7418904270486,0.346557674353927,-11.3858685475675));
#60979=CARTESIAN_POINT('Ctrl Pts',(40.5050211573478,0.369555531288926,-11.5462776182279));
#60980=CARTESIAN_POINT('Ctrl Pts',(40.4603214599847,0.37384323098138,-11.5744468652348));
#60981=CARTESIAN_POINT('Ctrl Pts',(40.3935398772801,0.380201068956179,-11.6135206399911));
#60982=CARTESIAN_POINT('Ctrl Pts',(40.372158094503,0.382229664439735,-11.6255954424682));
#60983=CARTESIAN_POINT('Ctrl Pts',(40.333675384848,0.385870823140411,-11.6465570510323));
#60984=CARTESIAN_POINT('Ctrl Pts',(40.3166451726377,0.387478800552697,-11.6555698091852));
#60985=CARTESIAN_POINT('Ctrl Pts',(40.2801360714548,0.390919999374295,-11.6743332584336));
#60986=CARTESIAN_POINT('Ctrl Pts',(40.2606294615052,0.39275506398798,-11.6840258143623));
#60987=CARTESIAN_POINT('Ctrl Pts',(40.2067160574572,0.397819051268324,-11.7099076725914));
#60988=CARTESIAN_POINT('Ctrl Pts',(40.1720543541811,0.401066183175113,-11.7255473722306));
#60989=CARTESIAN_POINT('Ctrl Pts',(40.0218683204445,0.415108976259383,-11.7890721410653));
#60990=CARTESIAN_POINT('Ctrl Pts',(39.9030946461116,0.426162127174695,-11.8287226728999));
#60991=CARTESIAN_POINT('Ctrl Pts',(39.6430213372514,0.4501628036776,-11.8935524061029));
#60992=CARTESIAN_POINT('Ctrl Pts',(39.5014329263022,0.463111148670782,-11.9157006862557));
#60993=CARTESIAN_POINT('Ctrl Pts',(39.3194317485095,0.479167022081036,-11.9277356497144));
#60994=CARTESIAN_POINT('Ctrl Pts',(39.2800913958472,0.482601360258549,-11.9293686125491));
#60995=CARTESIAN_POINT('Ctrl Pts',(39.2249594707982,0.487349163607097,-11.9303021869398));
#60996=CARTESIAN_POINT('Ctrl Pts',(39.2091904619028,0.488699681721397,-11.9304141353327));
#60997=CARTESIAN_POINT('Ctrl Pts',(39.1823878354658,0.490981278396629,-11.9303408249749));
#60998=CARTESIAN_POINT('Ctrl Pts',(39.1713547688906,0.491916455400143,-11.9302347383789));
#60999=CARTESIAN_POINT('Ctrl Pts',(39.1479670375202,0.493889945139972,-11.9298488945948));
#61000=CARTESIAN_POINT('Ctrl Pts',(39.1356132440575,0.494927221829795,-11.9295498542697));
#61001=CARTESIAN_POINT('Ctrl Pts',(39.1010458726237,0.497816634971966,-11.928446500116));
#61002=CARTESIAN_POINT('Ctrl Pts',(39.0788395460799,0.499657773728774,-11.9274294475609));
#61003=CARTESIAN_POINT('Ctrl Pts',(39.0281202733096,0.503835276764671,-11.9244014067842));
#61004=CARTESIAN_POINT('Ctrl Pts',(38.9996222175465,0.506162513253759,-11.9221897467921));
#61005=CARTESIAN_POINT('Ctrl Pts',(38.9027021559795,0.514030219286462,-11.9129274327818));
#61006=CARTESIAN_POINT('Ctrl Pts',(38.8345418315237,0.51948362721814,-11.9034501952042));
#61007=CARTESIAN_POINT('Ctrl Pts',(38.5965967997216,0.538531406987109,-11.8598927667114));
#61008=CARTESIAN_POINT('Ctrl Pts',(38.430191248427,0.551908901786091,-11.810434407625));
#61009=CARTESIAN_POINT('Ctrl Pts',(38.221578067747,0.57008933036705,-11.7230357771963));
#61010=CARTESIAN_POINT('Ctrl Pts',(38.1733143215142,0.574397474585507,-11.7009104915031));
#61011=CARTESIAN_POINT('Ctrl Pts',(38.1038153656843,0.580779744308204,-11.6662233178907));
#61012=CARTESIAN_POINT('Ctrl Pts',(38.0819762340619,0.582811853122353,-11.6549015979669));
#61013=CARTESIAN_POINT('Ctrl Pts',(38.0433436712948,0.586456862575836,-11.6341160474144));
#61014=CARTESIAN_POINT('Ctrl Pts',(38.0264828563667,0.588065139428848,-11.6247813772293));
#61015=CARTESIAN_POINT('Ctrl Pts',(37.9908315759203,0.591504347642001,-11.6044802122961));
#61016=CARTESIAN_POINT('Ctrl Pts',(37.9720742208278,0.593337096927028,-11.5934594376596));
#61017=CARTESIAN_POINT('Ctrl Pts',(37.9210618495814,0.59838751319231,-11.5625490249103));
#61018=CARTESIAN_POINT('Ctrl Pts',(37.8891247562829,0.60162322527827,-11.5421501102595));
#61019=CARTESIAN_POINT('Ctrl Pts',(37.7547637053739,0.615565577340072,-11.4517922430212));
#61020=CARTESIAN_POINT('Ctrl Pts',(37.6573679612897,0.626525287533903,-11.3747332061649));
#61021=CARTESIAN_POINT('Ctrl Pts',(37.4629229628616,0.650242182224442,-11.1948132043292));
#61022=CARTESIAN_POINT('Ctrl Pts',(37.3680944350712,0.66299928217291,-11.0901956551537));
#61023=CARTESIAN_POINT('Ctrl Pts',(37.2577079335957,0.679110347746528,-10.9445434203887));
#61024=CARTESIAN_POINT('Ctrl Pts',(37.2333185744732,0.682763709147642,-10.9105564821617));
#61025=CARTESIAN_POINT('Ctrl Pts',(37.2007516761759,0.687759552711926,-10.8625799532121));
#61026=CARTESIAN_POINT('Ctrl Pts',(37.1918118811615,0.689144059206279,-10.8491202797258));
#61027=CARTESIAN_POINT('Ctrl Pts',(37.17702136369,0.691455775454915,-10.8263574110851));
#61028=CARTESIAN_POINT('Ctrl Pts',(37.171097670997,0.692387515470001,-10.8171025642644));
#61029=CARTESIAN_POINT('Ctrl Pts',(37.1587568771471,0.694340720973326,-10.7975278438001));
#61030=CARTESIAN_POINT('Ctrl Pts',(37.1523542336184,0.69536128154118,-10.7871994435548));
#61031=CARTESIAN_POINT('Ctrl Pts',(37.1349689942243,0.698153793312059,-10.7586740270223));
#61032=CARTESIAN_POINT('Ctrl Pts',(37.1241485069163,0.699915902906804,-10.7403786790968));
#61033=CARTESIAN_POINT('Ctrl Pts',(37.1001631665927,0.703883551118638,-10.6985690279299));
#61034=CARTESIAN_POINT('Ctrl Pts',(37.0871478758857,0.706081234605045,-10.6749717612468));
#61035=CARTESIAN_POINT('Ctrl Pts',(36.9856066340711,0.723639599210348,-10.483326841681));
#61036=CARTESIAN_POINT('Ctrl Pts',(36.9168640608305,0.738199076413479,-10.3055353225338));
#61037=CARTESIAN_POINT('Ctrl Pts',(36.8463076368886,0.760677509060627,-10.0298996586911));
#61038=CARTESIAN_POINT('Ctrl Pts',(36.8282856007341,0.768228739507843,-9.93701768949147));
#61039=CARTESIAN_POINT('Ctrl Pts',(36.8117639586395,0.778424370763315,-9.81327213209202));
#61040=CARTESIAN_POINT('Ctrl Pts',(36.8083202880956,0.780916403195077,-9.78314763349859));
#61041=CARTESIAN_POINT('Ctrl Pts',(36.803722874488,0.784931877966725,-9.7348567409574));
#61042=CARTESIAN_POINT('Ctrl Pts',(36.8022042626951,0.78644397149213,-9.71672761464688));
#61043=CARTESIAN_POINT('Ctrl Pts',(36.7995672211515,0.78949419751867,-9.68028090056927));
#61044=CARTESIAN_POINT('Ctrl Pts',(36.7984524928712,0.791032339025779,-9.66196428390763));
#61045=CARTESIAN_POINT('Ctrl Pts',(36.7965860796382,0.794217919156763,-9.62416865368595));
#61046=CARTESIAN_POINT('Ctrl Pts',(36.7958614032487,0.795866078219987,-9.60468973575619));
#61047=CARTESIAN_POINT('Ctrl Pts',(36.7948625149559,0.79925576469566,-9.56479334059602));
#61048=CARTESIAN_POINT('Ctrl Pts',(36.7946114035323,0.800997857916507,-9.54437702317166));
#61049=CARTESIAN_POINT('Ctrl Pts',(36.794620224509,0.802747783846628,-9.52396074128696));
#61050=CARTESIAN_POINT('Ctrl Pts',(36.9547201749638,0.879636998740377,-8.65231241759342));
#61051=CARTESIAN_POINT('Ctrl Pts',(36.8488865264236,0.85468339172866,-8.92847699586774));
#61052=CARTESIAN_POINT('Ctrl Pts',(36.797182863997,0.829729784716943,-9.22613963971494));
#61053=CARTESIAN_POINT('Ctrl Pts',(36.7981523919191,0.804776177705222,-9.52412467452362));
#61054=CARTESIAN_POINT('Ctrl Pts',(36.9580194911167,1.14613690893122,-8.65357797698964));
#61055=CARTESIAN_POINT('Ctrl Pts',(36.931497086075,1.13961745573623,-8.72181439239125));
#61056=CARTESIAN_POINT('Ctrl Pts',(36.9080875735724,1.13303884220261,-8.79126758483645));
#61057=CARTESIAN_POINT('Ctrl Pts',(36.8537945688819,1.11534357173267,-8.98052894869805));
#61058=CARTESIAN_POINT('Ctrl Pts',(36.8289170938238,1.10424056888671,-9.10179610595467));
#61059=CARTESIAN_POINT('Ctrl Pts',(36.8106549506259,1.09154891176514,-9.2468077204081));
#61060=CARTESIAN_POINT('Ctrl Pts',(36.8081535430804,1.08960531823904,-9.26920448033023));
#61061=CARTESIAN_POINT('Ctrl Pts',(36.8047622553276,1.08661506383349,-9.30399474367018));
#61062=CARTESIAN_POINT('Ctrl Pts',(36.8036530847002,1.08555749068718,-9.3163647688518));
#61063=CARTESIAN_POINT('Ctrl Pts',(36.8017415028711,1.08357241212548,-9.33971556002907));
#61064=CARTESIAN_POINT('Ctrl Pts',(36.8009186294136,1.08264394199766,-9.3506935807053));
#61065=CARTESIAN_POINT('Ctrl Pts',(36.7991103191695,1.08040760889664,-9.37726454413118));
#61066=CARTESIAN_POINT('Ctrl Pts',(36.7982013707649,1.07910387186094,-9.39286215799357));
#61067=CARTESIAN_POINT('Ctrl Pts',(36.7955819084487,1.07461743869307,-9.44686803163611));
#61068=CARTESIAN_POINT('Ctrl Pts',(36.7946401158394,1.07147232060647,-9.48531022708832));
#61069=CARTESIAN_POINT('Ctrl Pts',(36.7945880042618,1.06327879496806,-9.5865254092814));
#61070=CARTESIAN_POINT('Ctrl Pts',(36.7970122625023,1.05828745084736,-9.64927173968473));
#61071=CARTESIAN_POINT('Ctrl Pts',(36.8182794592562,1.03668275355598,-9.9222148897046));
#61072=CARTESIAN_POINT('Ctrl Pts',(36.8622730995552,1.02046588534418,-10.1294824763955));
#61073=CARTESIAN_POINT('Ctrl Pts',(36.944649832248,1.00041379659953,-10.3619712761099));
#61074=CARTESIAN_POINT('Ctrl Pts',(36.9573086736758,0.997492653788696,-10.3953221510601));
#61075=CARTESIAN_POINT('Ctrl Pts',(36.9787022358353,0.992788718018505,-10.4481157897272));
#61076=CARTESIAN_POINT('Ctrl Pts',(36.9869622719098,0.99102167626982,-10.4677462394215));
#61077=CARTESIAN_POINT('Ctrl Pts',(37.0032280064555,0.987631200569094,-10.5050105651657));
#61078=CARTESIAN_POINT('Ctrl Pts',(37.011188175541,0.98600941231694,-10.5226625932093));
#61079=CARTESIAN_POINT('Ctrl Pts',(37.0300934318465,0.982240755306312,-10.563270256354));
#61080=CARTESIAN_POINT('Ctrl Pts',(37.0411909849412,0.980088835354502,-10.5861518126627));
#61081=CARTESIAN_POINT('Ctrl Pts',(37.078878893681,0.972969568630612,-10.6608199056665));
#61082=CARTESIAN_POINT('Ctrl Pts',(37.1069842886146,0.967951156116989,-10.7118132157487));
#61083=CARTESIAN_POINT('Ctrl Pts',(37.1814726844309,0.955313878702441,-10.8360731726929));
#61084=CARTESIAN_POINT('Ctrl Pts',(37.2300172231052,0.9476310280052,-10.9079425935613));
#61085=CARTESIAN_POINT('Ctrl Pts',(37.3620071422727,0.928074053871764,-11.0822595598534));
#61086=CARTESIAN_POINT('Ctrl Pts',(37.4502121535132,0.916132655189497,-11.1807531457853));
#61087=CARTESIAN_POINT('Ctrl Pts',(37.5846427592641,0.899718576544822,-11.3080587770194));
#61088=CARTESIAN_POINT('Ctrl Pts',(37.6244371430778,0.895051909162368,-11.3433180219806));
#61089=CARTESIAN_POINT('Ctrl Pts',(37.6788849975739,0.888947786310866,-11.3884296576259));
#61090=CARTESIAN_POINT('Ctrl Pts',(37.6925217464467,0.887441386799851,-11.399478676957));
#61091=CARTESIAN_POINT('Ctrl Pts',(37.7143020319535,0.885072099187608,-11.4167344606176));
#61092=CARTESIAN_POINT('Ctrl Pts',(37.7223659751232,0.884202708591631,-11.42303988959));
#61093=CARTESIAN_POINT('Ctrl Pts',(37.7395108808127,0.882371148720978,-11.4362704899073));
#61094=CARTESIAN_POINT('Ctrl Pts',(37.748601407989,0.881409921539475,-11.4431828624648));
#61095=CARTESIAN_POINT('Ctrl Pts',(37.7720198548643,0.878957876791219,-11.4607282809352));
#61096=CARTESIAN_POINT('Ctrl Pts',(37.7864178834406,0.877473255002006,-11.4712674355299));
#61097=CARTESIAN_POINT('Ctrl Pts',(37.8504876459113,0.870960520825029,-11.517079466595));
#61098=CARTESIAN_POINT('Ctrl Pts',(37.9013767640468,0.866032843728939,-11.5506217745362));
#61099=CARTESIAN_POINT('Ctrl Pts',(38.0699645791256,0.850287557906748,-11.6527734637443));
#61100=CARTESIAN_POINT('Ctrl Pts',(38.1922289829027,0.83973084262256,-11.7133332450156));
#61101=CARTESIAN_POINT('Ctrl Pts',(38.4282320924356,0.819797415686219,-11.806231135488));
#61102=CARTESIAN_POINT('Ctrl Pts',(38.5404832272685,0.810487041138136,-11.8411763419449));
#61103=CARTESIAN_POINT('Ctrl Pts',(38.6858968992707,0.798311590755273,-11.875014599526));
#61104=CARTESIAN_POINT('Ctrl Pts',(38.7171069230509,0.795692590205841,-11.8816257021449));
#61105=CARTESIAN_POINT('Ctrl Pts',(38.7685971577293,0.791356630002007,-11.89146694032));
#61106=CARTESIAN_POINT('Ctrl Pts',(38.7888043833915,0.789651208671667,-11.8950616663796));
#61107=CARTESIAN_POINT('Ctrl Pts',(38.8284688122384,0.78629480625426,-11.9015951829009));
#61108=CARTESIAN_POINT('Ctrl Pts',(38.8479210047945,0.784644614771989,-11.9045546681911));
#61109=CARTESIAN_POINT('Ctrl Pts',(38.894612694088,0.78067238914831,-11.9110733706935));
#61110=CARTESIAN_POINT('Ctrl Pts',(38.9218804886875,0.778343491570431,-11.9144051435304));
#61111=CARTESIAN_POINT('Ctrl Pts',(39.0215358530242,0.769794833078296,-11.924852859251));
#61112=CARTESIAN_POINT('Ctrl Pts',(39.0941715674575,0.763490941589336,-11.9291508291074));
#61113=CARTESIAN_POINT('Ctrl Pts',(39.2874950089218,0.746504737494365,-11.9318127549201));
#61114=CARTESIAN_POINT('Ctrl Pts',(39.4080491253668,0.735688967729816,-11.9243983943415));
#61115=CARTESIAN_POINT('Ctrl Pts',(39.6433356995204,0.714344709284184,-11.8920597535195));
#61116=CARTESIAN_POINT('Ctrl Pts',(39.7578444580982,0.703846678325236,-11.8677193155008));
#61117=CARTESIAN_POINT('Ctrl Pts',(39.8948022764581,0.691425745187621,-11.827989836002));
#61118=CARTESIAN_POINT('Ctrl Pts',(39.9193505607167,0.689205273583825,-11.8204405502506));
#61119=CARTESIAN_POINT('Ctrl Pts',(39.9561917559453,0.685886206390024,-11.8084617265558));
#61120=CARTESIAN_POINT('Ctrl Pts',(39.9685761930975,0.684772777451614,-11.8043231645117));
#61121=CARTESIAN_POINT('Ctrl Pts',(39.991212882229,0.682742581488666,-11.7965530788199));
#61122=CARTESIAN_POINT('Ctrl Pts',(40.0014746956405,0.681824209814641,-11.7929527194456));
#61123=CARTESIAN_POINT('Ctrl Pts',(40.0253850803141,0.679688613981469,-11.7843811937629));
#61124=CARTESIAN_POINT('Ctrl Pts',(40.0390135735113,0.678474517842431,-11.7793558205919));
#61125=CARTESIAN_POINT('Ctrl Pts',(40.0842337468289,0.67445387157678,-11.7622144246559));
#61126=CARTESIAN_POINT('Ctrl Pts',(40.1156171058574,0.671676237836499,-11.7495546435479));
#61127=CARTESIAN_POINT('Ctrl Pts',(40.1933565295819,0.664801978521204,-11.7162710525721));
#61128=CARTESIAN_POINT('Ctrl Pts',(40.2393482880734,0.660740582615042,-11.6948345430988));
#61129=CARTESIAN_POINT('Ctrl Pts',(40.4470362875822,0.642269918515834,-11.5899117401693));
#61130=CARTESIAN_POINT('Ctrl Pts',(40.5996065638879,0.628285018782427,-11.4897046267061));
#61131=CARTESIAN_POINT('Ctrl Pts',(40.7900920616115,0.608497383711214,-11.3310478186682));
#61132=CARTESIAN_POINT('Ctrl Pts',(40.839000286265,0.603177589844435,-11.2867826504993));
#61133=CARTESIAN_POINT('Ctrl Pts',(40.9054510360189,0.595545403892491,-11.2214762248616));
#61134=CARTESIAN_POINT('Ctrl Pts',(40.9245507798935,0.593301084920462,-11.2020567381452));
#61135=CARTESIAN_POINT('Ctrl Pts',(40.9567115186256,0.5894303392864,-11.168227183308));
#61136=CARTESIAN_POINT('Ctrl Pts',(40.969935390187,0.587811022602961,-11.1539750162615));
#61137=CARTESIAN_POINT('Ctrl Pts',(40.9967765133129,0.584465175529347,-11.1243340146422));
#61138=CARTESIAN_POINT('Ctrl Pts',(41.0103721882208,0.582737928504908,-11.1089279065688));
#61139=CARTESIAN_POINT('Ctrl Pts',(41.0446417329438,0.578298383789974,-11.0690772919074));
#61140=CARTESIAN_POINT('Ctrl Pts',(41.0650272926808,0.575574788170089,-11.044391586039));
#61141=CARTESIAN_POINT('Ctrl Pts',(41.1660983478821,0.56163317071988,-10.9169010003618));
#61142=CARTESIAN_POINT('Ctrl Pts',(41.2387876780221,0.550116091301752,-10.8080682098474));
#61143=CARTESIAN_POINT('Ctrl Pts',(41.3671108956774,0.526493088775805,-10.5772768944705));
#61144=CARTESIAN_POINT('Ctrl Pts',(41.4221355103943,0.514420389180119,-10.4554682798378));
#61145=CARTESIAN_POINT('Ctrl Pts',(41.4839277549893,0.498059328967464,-10.2814095348409));
#61146=CARTESIAN_POINT('Ctrl Pts',(41.4995323106832,0.493561301659272,-10.232554629738));
#61147=CARTESIAN_POINT('Ctrl Pts',(41.5183088518674,0.487639593660438,-10.1665587078539));
#61148=CARTESIAN_POINT('Ctrl Pts',(41.5228728702454,0.486151842494649,-10.149832130141));
#61149=CARTESIAN_POINT('Ctrl Pts',(41.5298335486495,0.483804465048132,-10.1231910728997));
#61150=CARTESIAN_POINT('Ctrl Pts',(41.5323485765599,0.482938537249089,-10.1133086380542));
#61151=CARTESIAN_POINT('Ctrl Pts',(41.5375585471286,0.481106435461196,-10.0922781605082));
#61152=CARTESIAN_POINT('Ctrl Pts',(41.5402367708715,0.480141259110742,-10.0811261945271));
#61153=CARTESIAN_POINT('Ctrl Pts',(41.5469302725944,0.477666016140122,-10.0523499350229));
#61154=CARTESIAN_POINT('Ctrl Pts',(41.5508269567604,0.476162377851029,-10.0346982815993));
#61155=CARTESIAN_POINT('Ctrl Pts',(41.567536756906,0.469409647644259,-9.95473212708788));
#61156=CARTESIAN_POINT('Ctrl Pts',(41.5780750841111,0.464270379605273,-9.8919615525581));
#61157=CARTESIAN_POINT('Ctrl Pts',(41.6050938043786,0.447207772394857,-9.6797784097128));
#61158=CARTESIAN_POINT('Ctrl Pts',(41.6100663027085,0.435596808906464,-9.5292592531869));
#61159=CARTESIAN_POINT('Ctrl Pts',(41.5947911571082,0.415720391052272,-9.2776243602733));
#61160=CARTESIAN_POINT('Ctrl Pts',(41.5821764409379,0.407608865056097,-9.17650255170654));
#61161=CARTESIAN_POINT('Ctrl Pts',(41.5573949042475,0.396762706005806,-9.04592787262659));
#61162=CARTESIAN_POINT('Ctrl Pts',(41.5510017888084,0.394207114800862,-9.01547939421215));
#61163=CARTESIAN_POINT('Ctrl Pts',(41.5394497731286,0.389948026440219,-8.96531934443248));
#61164=CARTESIAN_POINT('Ctrl Pts',(41.5346275994517,0.388255246085189,-8.94553335221888));
#61165=CARTESIAN_POINT('Ctrl Pts',(41.5246284642194,0.384902662719987,-8.90665820935601));
#61166=CARTESIAN_POINT('Ctrl Pts',(41.5194661256437,0.38324344755222,-8.88756693776711));
#61167=CARTESIAN_POINT('Ctrl Pts',(41.5064155079617,0.379212868604969,-8.84156241715001));
#61168=CARTESIAN_POINT('Ctrl Pts',(41.4982909982984,0.376834113934977,-8.81471993612044));
#61169=CARTESIAN_POINT('Ctrl Pts',(41.4659547714421,0.367824455153892,-8.7142546247587));
#61170=CARTESIAN_POINT('Ctrl Pts',(41.4386617536935,0.361096822711199,-8.64168247565026));
#61171=CARTESIAN_POINT('Ctrl Pts',(41.3513717925894,0.341729295698674,-8.43975316925643));
#61172=CARTESIAN_POINT('Ctrl Pts',(41.2833176047823,0.328885492880572,-8.31423943031549));
#61173=CARTESIAN_POINT('Ctrl Pts',(41.1503174577058,0.307297902265517,-8.11370695861565));
#61174=CARTESIAN_POINT('Ctrl Pts',(41.0911058448527,0.298547611843039,-8.03529875912544));
#61175=CARTESIAN_POINT('Ctrl Pts',(41.0140577857044,0.288284610935066,-7.94529766504272));
#61176=CARTESIAN_POINT('Ctrl Pts',(41.0006594516044,0.286536993946662,-7.93004208831295));
#61177=CARTESIAN_POINT('Ctrl Pts',(40.9790724930371,0.283781694225559,-7.90608161793796));
#61178=CARTESIAN_POINT('Ctrl Pts',(40.9710098137012,0.282765576183815,-7.89726540179209));
#61179=CARTESIAN_POINT('Ctrl Pts',(40.955250996482,0.280805100121044,-7.88028948614087));
#61180=CARTESIAN_POINT('Ctrl Pts',(40.9475629732705,0.279860258803079,-7.87212299345442));
#61181=CARTESIAN_POINT('Ctrl Pts',(40.9282028452735,0.27750881054963,-7.85184405988391));
#61182=CARTESIAN_POINT('Ctrl Pts',(40.9164599475162,0.276107409992372,-7.83979936731374));
#61183=CARTESIAN_POINT('Ctrl Pts',(40.8688081342409,0.270514288907428,-7.79193782578148));
#61184=CARTESIAN_POINT('Ctrl Pts',(40.8318937219044,0.26639119406009,-7.75713433582304));
#61185=CARTESIAN_POINT('Ctrl Pts',(40.6356944470844,0.245348286152978,-7.58354222953039));
#61186=CARTESIAN_POINT('Ctrl Pts',(40.4597301492004,0.229241347136703,-7.46500715640543));
#61187=CARTESIAN_POINT('Ctrl Pts',(40.2119203975778,0.207147685941844,-7.34184771826776));
#61188=CARTESIAN_POINT('Ctrl Pts',(40.1521497673295,0.201866458749272,-7.31512530147421));
#61189=CARTESIAN_POINT('Ctrl Pts',(40.0661634733594,0.194281990729688,-7.28081858676874));
#61190=CARTESIAN_POINT('Ctrl Pts',(40.0407909482435,0.192045716922526,-7.27118992851656));
#61191=CARTESIAN_POINT('Ctrl Pts',(39.9968036298373,0.188168282405154,-7.25534323093124));
#61192=CARTESIAN_POINT('Ctrl Pts',(39.9782652062557,0.186533998757501,-7.24891979606678));
#61193=CARTESIAN_POINT('Ctrl Pts',(39.9400801356731,0.183166165369478,-7.23620997399349));
#61194=CARTESIAN_POINT('Ctrl Pts',(39.9204271161451,0.18143197211041,-7.22994812609138));
#61195=CARTESIAN_POINT('Ctrl Pts',(39.8696992266563,0.176952038417327,-7.21450095748407));
#61196=CARTESIAN_POINT('Ctrl Pts',(39.8385159451596,0.174194589989077,-7.20568974745903));
#61197=CARTESIAN_POINT('Ctrl Pts',(39.6692608333936,0.159200137456038,-7.16153661189935));
#61198=CARTESIAN_POINT('Ctrl Pts',(39.5284590780057,0.146602489050096,-7.13789619750786));
#61199=CARTESIAN_POINT('Ctrl Pts',(39.2316565917541,0.119918833242445,-7.11482422195453));
#61200=CARTESIAN_POINT('Ctrl Pts',(39.0760825424865,0.105859956512213,-7.11780230178375));
#61201=CARTESIAN_POINT('Ctrl Pts',(38.8952221482782,0.0899841896783604,
-7.13885599581126));
#61202=CARTESIAN_POINT('Ctrl Pts',(38.8686250107536,0.087662376952385,-7.14240403222418));
#61203=CARTESIAN_POINT('Ctrl Pts',(38.8289587467098,0.0842239900019295,
-7.14837262108122));
#61204=CARTESIAN_POINT('Ctrl Pts',(38.8158424248945,0.0830910239869222,
-7.15045745605491));
#61205=CARTESIAN_POINT('Ctrl Pts',(38.7931119884368,0.0811352851711953,
-7.15426373059113));
#61206=CARTESIAN_POINT('Ctrl Pts',(38.7834904289672,0.080309892642764,-7.15593518445652));
#61207=CARTESIAN_POINT('Ctrl Pts',(38.7604869363426,0.078342252599258,-7.16007582335779));
#61208=CARTESIAN_POINT('Ctrl Pts',(38.747115371639,0.0772030533942414,-7.16260002641951));
#61209=CARTESIAN_POINT('Ctrl Pts',(38.7057430978238,0.0736903687322396,
-7.17077423232197));
#61210=CARTESIAN_POINT('Ctrl Pts',(38.6778197155968,0.0713367144824334,
-7.1768098846533));
#61211=CARTESIAN_POINT('Ctrl Pts',(38.6110495141226,0.0657350235790357,
-7.19249237627467));
#61212=CARTESIAN_POINT('Ctrl Pts',(38.5723220729515,0.0625075765481499,
-7.20261429749493));
#61213=CARTESIAN_POINT('Ctrl Pts',(38.4118897982779,0.0491577277687317,
-7.24885228531607));
#61214=CARTESIAN_POINT('Ctrl Pts',(38.2928827228701,0.0392953291842206,
-7.29360830832483));
#61215=CARTESIAN_POINT('Ctrl Pts',(38.0620097516238,0.0192826051881944,
-7.40197459379847));
#61216=CARTESIAN_POINT('Ctrl Pts',(37.9506102434301,0.00916016733974761,
-7.46556396654334));
#61217=CARTESIAN_POINT('Ctrl Pts',(37.8180708158714,-0.00391720617964832,
-7.55594635420535));
#61218=CARTESIAN_POINT('Ctrl Pts',(37.7917022806951,-0.00657355479567719,
-7.57471851691715));
#61219=CARTESIAN_POINT('Ctrl Pts',(37.74916931706,-0.0109548781684845,-7.60631075595678));
#61220=CARTESIAN_POINT('Ctrl Pts',(37.732776213449,-0.0126678208351297,
-7.61881732490205));
#61221=CARTESIAN_POINT('Ctrl Pts',(37.7021860981284,-0.0159118838279119,
-7.64278341897208));
#61222=CARTESIAN_POINT('Ctrl Pts',(37.6879546520026,-0.0174411100794713,
-7.65419681178444));
#61223=CARTESIAN_POINT('Ctrl Pts',(37.6721906704758,-0.0191580517055498,
-7.66713664863116));
#61224=CARTESIAN_POINT('Ctrl Pts',(37.6705283701373,-0.0193393915737116,
-7.66850488470314));
#61225=CARTESIAN_POINT('Ctrl Pts',(37.6674937781192,-0.0196709654131965,
-7.67100949332569));
#61226=CARTESIAN_POINT('Ctrl Pts',(37.6661209059832,-0.0198211711323544,
-7.67214516385033));
#61227=CARTESIAN_POINT('Ctrl Pts',(37.6635148027179,-0.0201066840401274,
-7.67430587224538));
#61228=CARTESIAN_POINT('Ctrl Pts',(37.6622813316036,-0.0202419795431571,
-7.67533062067546));
#61229=CARTESIAN_POINT('Ctrl Pts',(37.6598686792253,-0.0205069335144982,
-7.67733909567683));
#61230=CARTESIAN_POINT('Ctrl Pts',(37.6586894131674,-0.0206365878128918,
-7.67832271972343));
#61231=CARTESIAN_POINT('Ctrl Pts',(37.6563243952665,-0.0208969092564838,
-7.68029922112771));
#61232=CARTESIAN_POINT('Ctrl Pts',(37.6551386574814,-0.0210275769871849,
-7.68129211408394));
#61233=CARTESIAN_POINT('Ctrl Pts',(37.6375881172503,-0.0229638888616028,
-7.69601710492904));
#61234=CARTESIAN_POINT('Ctrl Pts',(37.6214065876006,-0.0247781902902664,
-7.70996498740579));
#61235=CARTESIAN_POINT('Ctrl Pts',(37.5818338529958,-0.0292890038655323,
-7.74500472350681));
#61236=CARTESIAN_POINT('Ctrl Pts',(37.5586677400258,-0.0319953373275242,
-7.76634338810736));
#61237=CARTESIAN_POINT('Ctrl Pts',(37.4684631894485,-0.0428021174569438,
-7.85276713110247));
#61238=CARTESIAN_POINT('Ctrl Pts',(37.4048302304242,-0.0510375769064575,
-7.92127191653282));
#61239=CARTESIAN_POINT('Ctrl Pts',(37.249159825575,-0.0728423739289821,
-8.1097639877308));
#61240=CARTESIAN_POINT('Ctrl Pts',(37.1641577386255,-0.086537618455635,
-8.23503236025419));
#61241=CARTESIAN_POINT('Ctrl Pts',(37.0677904145058,-0.104258679145249,
-8.41056944947567));
#61242=CARTESIAN_POINT('Ctrl Pts',(37.0454418929366,-0.108570958311494,
-8.45441443371193));
#61243=CARTESIAN_POINT('Ctrl Pts',(37.017161210074,-0.11429063109198,-8.51437648914323));
#61244=CARTESIAN_POINT('Ctrl Pts',(37.0100349983504,-0.115756911868296,
-8.52991286469083));
#61245=CARTESIAN_POINT('Ctrl Pts',(36.9989403949401,-0.11807912908377,-8.55479762854446));
#61246=CARTESIAN_POINT('Ctrl Pts',(36.9948647301536,-0.118941137877828,
-8.56409704952668));
#61247=CARTESIAN_POINT('Ctrl Pts',(36.9862867939414,-0.120774321060462,
-8.58401130839614));
#61248=CARTESIAN_POINT('Ctrl Pts',(36.9818016782924,-0.121744432152582,
-8.59463335223591));
#61249=CARTESIAN_POINT('Ctrl Pts',(36.9707615799654,-0.124162937434917,
-8.62131321394616));
#61250=CARTESIAN_POINT('Ctrl Pts',(36.9643034256454,-0.125605804264154,
-8.63741078235361));
#61251=CARTESIAN_POINT('Ctrl Pts',(36.958019684865,-0.127039975641411,-8.65357747851736));
#61252=CARTESIAN_POINT('Origin',(39.2,8.05522481984854,-9.525));
#61253=CARTESIAN_POINT('',(36.9580197773588,-1.66076081124402,-8.65357724055094));
#61254=CARTESIAN_POINT('',(36.9580196842388,-1.39337735599387,-8.65357748012833));
#61255=CARTESIAN_POINT('',(36.958019684865,8.05522481984854,-8.65357747851728));
#61256=CARTESIAN_POINT('Ctrl Pts',(36.9580197773588,-1.66076081124402,-8.65357724055094));
#61257=CARTESIAN_POINT('Ctrl Pts',(36.9766488117873,-1.65672078778712,-8.60564880822258));
#61258=CARTESIAN_POINT('Ctrl Pts',(36.9968186458683,-1.6526640807411,-8.5583076754036));
#61259=CARTESIAN_POINT('Ctrl Pts',(37.0508280242562,-1.6424719350196,-8.44204107296676));
#61260=CARTESIAN_POINT('Ctrl Pts',(37.0864609765807,-1.63630295383903,-8.37404785157304));
#61261=CARTESIAN_POINT('Ctrl Pts',(37.1394253456699,-1.62773492932436,-8.2837640407794));
#61262=CARTESIAN_POINT('Ctrl Pts',(37.1539909881947,-1.62543263236425,-8.25989857947043));
#61263=CARTESIAN_POINT('Ctrl Pts',(37.1795579860137,-1.62147711970216,-8.21960440162423));
#61264=CARTESIAN_POINT('Ctrl Pts',(37.190352247854,-1.61983153500462,-8.20304710237475));
#61265=CARTESIAN_POINT('Ctrl Pts',(37.2126966282331,-1.61647248174447,-8.16967930526093));
#61266=CARTESIAN_POINT('Ctrl Pts',(37.2242589418237,-1.61475866209417,-8.15287898010722));
#61267=CARTESIAN_POINT('Ctrl Pts',(37.2540704193083,-1.61039891078306,-8.11072032099696));
#61268=CARTESIAN_POINT('Ctrl Pts',(37.2726020115671,-1.60774248286012,-8.08556756311285));
#61269=CARTESIAN_POINT('Ctrl Pts',(37.3548060377018,-1.59617842274454,-7.97842712010962));
#61270=CARTESIAN_POINT('Ctrl Pts',(37.423249407921,-1.58708985601911,-7.90026018662994));
#61271=CARTESIAN_POINT('Ctrl Pts',(37.6012974123963,-1.56466771010006,-7.72166160899465));
#61272=CARTESIAN_POINT('Ctrl Pts',(37.7155753632623,-1.55122298613764,-7.62648481102988));
#61273=CARTESIAN_POINT('Ctrl Pts',(37.8732631973737,-1.53419916170227,-7.51814570967567));
#61274=CARTESIAN_POINT('Ctrl Pts',(37.9092813482138,-1.53040540932297,-7.49479297976078));
#61275=CARTESIAN_POINT('Ctrl Pts',(37.971549393283,-1.52402605819973,-7.45674832044312));
#61276=CARTESIAN_POINT('Ctrl Pts',(37.9974844834706,-1.52141988073497,-7.44156231588705));
#61277=CARTESIAN_POINT('Ctrl Pts',(38.035805085137,-1.51764951415879,-7.42007820455439));
#61278=CARTESIAN_POINT('Ctrl Pts',(38.0479700605679,-1.51646421217904,-7.41339572543235));
#61279=CARTESIAN_POINT('Ctrl Pts',(38.0688104796859,-1.51445414223008,-7.40218135838208));
#61280=CARTESIAN_POINT('Ctrl Pts',(38.0774565761698,-1.51362622209264,-7.39759665534387));
#61281=CARTESIAN_POINT('Ctrl Pts',(38.0977023927963,-1.51170154169669,-7.38701885458659));
#61282=CARTESIAN_POINT('Ctrl Pts',(38.1093232671032,-1.51060732096031,-7.3810672394568));
#61283=CARTESIAN_POINT('Ctrl Pts',(38.1439288064997,-1.50737817668478,-7.36369826652627));
#61284=CARTESIAN_POINT('Ctrl Pts',(38.1670493450435,-1.50525875690302,-7.35255330232061));
#61285=CARTESIAN_POINT('Ctrl Pts',(38.297321213849,-1.49350260381528,-7.29230760790032));
#61286=CARTESIAN_POINT('Ctrl Pts',(38.4078048335977,-1.48422260090457,-7.25075745143956));
#61287=CARTESIAN_POINT('Ctrl Pts',(38.6369965082939,-1.46548734462016,-7.1833073124018));
#61288=CARTESIAN_POINT('Ctrl Pts',(38.7554949949892,-1.45605799133323,-7.15795316794812));
#61289=CARTESIAN_POINT('Ctrl Pts',(38.946442035062,-1.44070609476772,-7.13194698285513));
#61290=CARTESIAN_POINT('Ctrl Pts',(39.0178800615771,-1.43493045182367,-7.12545318927569));
#61291=CARTESIAN_POINT('Ctrl Pts',(39.1168104360454,-1.42681871763883,-7.12090347068267));
#61292=CARTESIAN_POINT('Ctrl Pts',(39.1441435869574,-1.42456583577932,-7.12011319119244));
#61293=CARTESIAN_POINT('Ctrl Pts',(39.1911397853741,-1.42066861417859,-7.11955599150702));
#61294=CARTESIAN_POINT('Ctrl Pts',(39.2107978927907,-1.41903133753692,-7.11956391921353));
#61295=CARTESIAN_POINT('Ctrl Pts',(39.24856677444,-1.41587080542725,-7.12004212700813));
#61296=CARTESIAN_POINT('Ctrl Pts',(39.2666767424749,-1.41434878359187,-7.12047608120949));
#61297=CARTESIAN_POINT('Ctrl Pts',(39.3146419236564,-1.41029915895054,-7.12216770379771));
#61298=CARTESIAN_POINT('Ctrl Pts',(39.344480562112,-1.40776091913265,-7.12377718470187));
#61299=CARTESIAN_POINT('Ctrl Pts',(39.46315474601,-1.39758477488507,-7.13239829563719));
#61300=CARTESIAN_POINT('Ctrl Pts',(39.5515892562966,-1.38981672839708,-7.14378724075549));
#61301=CARTESIAN_POINT('Ctrl Pts',(39.799559249943,-1.36750168420545,-7.18983598010339));
#61302=CARTESIAN_POINT('Ctrl Pts',(39.9564914263345,-1.3527127722752,-7.23585687535715));
#61303=CARTESIAN_POINT('Ctrl Pts',(40.1684505844484,-1.33232977448233,-7.32221033155718));
#61304=CARTESIAN_POINT('Ctrl Pts',(40.2283249637459,-1.326528564027,-7.34951647222082));
#61305=CARTESIAN_POINT('Ctrl Pts',(40.3032950888115,-1.31926664362761,-7.38749535137323));
#61306=CARTESIAN_POINT('Ctrl Pts',(40.3194857285393,-1.317698520319,-7.39593026376321));
#61307=CARTESIAN_POINT('Ctrl Pts',(40.3457246639721,-1.31515922787757,-7.40998217938844));
#61308=CARTESIAN_POINT('Ctrl Pts',(40.3558310438408,-1.31418167787483,-7.4154882073428));
#61309=CARTESIAN_POINT('Ctrl Pts',(40.3747953825199,-1.31234880729299,-7.42599732488529));
#61310=CARTESIAN_POINT('Ctrl Pts',(40.3836617978339,-1.31149249314473,-7.43098443624007));
#61311=CARTESIAN_POINT('Ctrl Pts',(40.4074259078356,-1.30919825212118,-7.44455025554639));
#61312=CARTESIAN_POINT('Ctrl Pts',(40.4222641254231,-1.3077666801506,-7.4532328986108));
#61313=CARTESIAN_POINT('Ctrl Pts',(40.4798920833177,-1.30220518078551,-7.4877888112491));
#61314=CARTESIAN_POINT('Ctrl Pts',(40.5219675957105,-1.29814099102921,-7.51483686261072));
#61315=CARTESIAN_POINT('Ctrl Pts',(40.6869677085935,-1.28205523210234,-7.62833036786038));
#61316=CARTESIAN_POINT('Ctrl Pts',(40.8025216512016,-1.27043253054818,-7.7248997682733));
#61317=CARTESIAN_POINT('Ctrl Pts',(40.9905344433623,-1.24943710216797,-7.91457186834187));
#61318=CARTESIAN_POINT('Ctrl Pts',(41.0665915785064,-1.24017176125122,-8.00338169173194));
#61319=CARTESIAN_POINT('Ctrl Pts',(41.1545022838283,-1.22808684187491,-8.12258890456953));
#61320=CARTESIAN_POINT('Ctrl Pts',(41.1726158571275,-1.2255116862948,-8.14818390656078));
#61321=CARTESIAN_POINT('Ctrl Pts',(41.2016896353693,-1.22122862236032,-8.19101783612297));
#61322=CARTESIAN_POINT('Ctrl Pts',(41.2129401670582,-1.21953167951824,-8.2080559464638));
#61323=CARTESIAN_POINT('Ctrl Pts',(41.2345226787362,-1.21619606606693,-8.24166386036473));
#61324=CARTESIAN_POINT('Ctrl Pts',(41.2448724917561,-1.2145582120095,-8.25822037352323));
#61325=CARTESIAN_POINT('Ctrl Pts',(41.2671678639451,-1.21094310288419,-8.29487139297771));
#61326=CARTESIAN_POINT('Ctrl Pts',(41.2790242017547,-1.20896282708215,-8.31501749882002));
#61327=CARTESIAN_POINT('Ctrl Pts',(41.3193171015431,-1.20202413738088,-8.38582359597382));
#61328=CARTESIAN_POINT('Ctrl Pts',(41.3462082035547,-1.19701304880252,-8.43733415735116));
#61329=CARTESIAN_POINT('Ctrl Pts',(41.4543816984186,-1.17507832928614,-8.6642068304185));
#61330=CARTESIAN_POINT('Ctrl Pts',(41.5162214034485,-1.15757111050607,-8.84802263022129));
#61331=CARTESIAN_POINT('Ctrl Pts',(41.5656647877552,-1.13579929414333,-9.08677098868994));
#61332=CARTESIAN_POINT('Ctrl Pts',(41.5743624743452,-1.13130748550425,-9.13664691923469));
#61333=CARTESIAN_POINT('Ctrl Pts',(41.5862308485587,-1.12390814916167,-9.22021062556128));
#61334=CARTESIAN_POINT('Ctrl Pts',(41.5902764816189,-1.1209714126182,-9.25375673613673));
#61335=CARTESIAN_POINT('Ctrl Pts',(41.595048507954,-1.11682070853175,-9.30182659587809));
#61336=CARTESIAN_POINT('Ctrl Pts',(41.5963519511122,-1.11557949832043,-9.31628707989927));
#61337=CARTESIAN_POINT('Ctrl Pts',(41.5984027586263,-1.1134206729372,-9.34160028372474));
#61338=CARTESIAN_POINT('Ctrl Pts',(41.5992075576521,-1.11250008842168,-9.35244750587373));
#61339=CARTESIAN_POINT('Ctrl Pts',(41.6008172606843,-1.11048253215298,-9.37633867575441));
#61340=CARTESIAN_POINT('Ctrl Pts',(41.6015894919113,-1.10938732634205,-9.3893841994733));
#61341=CARTESIAN_POINT('Ctrl Pts',(41.6035661750105,-1.10615214223569,-9.42812715203864));
#61342=CARTESIAN_POINT('Ctrl Pts',(41.6044648137248,-1.10402775436498,-9.45383942144602));
#61343=CARTESIAN_POINT('Ctrl Pts',(41.60695111997,-1.09324755761583,-9.58543716331371));
#61344=CARTESIAN_POINT('Ctrl Pts',(41.6019580386535,-1.08487582065179,-9.691343368924));
#61345=CARTESIAN_POINT('Ctrl Pts',(41.5795849289382,-1.06931382989583,-9.88822827717988));
#61346=CARTESIAN_POINT('Ctrl Pts',(41.5639095814976,-1.06212387074988,-9.97919216090846));
#61347=CARTESIAN_POINT('Ctrl Pts',(41.5193049728559,-1.04658145069881,-10.1712968150664));
#61348=CARTESIAN_POINT('Ctrl Pts',(41.4888932636008,-1.03822097813879,-10.271885571013));
#61349=CARTESIAN_POINT('Ctrl Pts',(41.4412610993584,-1.02715265863564,-10.3988066243859));
#61350=CARTESIAN_POINT('Ctrl Pts',(41.4299640774878,-1.02463805584239,-10.4272468479339));
#61351=CARTESIAN_POINT('Ctrl Pts',(41.4102884945814,-1.02042825487334,-10.4741514359711));
#61352=CARTESIAN_POINT('Ctrl Pts',(41.4022132483537,-1.01874325094457,-10.4927398586336));
#61353=CARTESIAN_POINT('Ctrl Pts',(41.3858568728235,-1.01541062257731,-10.5291254501065));
#61354=CARTESIAN_POINT('Ctrl Pts',(41.3775908493757,-1.01376361973527,-10.5469277038824));
#61355=CARTESIAN_POINT('Ctrl Pts',(41.3588209290888,-1.01010267730889,-10.5860898421337));
#61356=CARTESIAN_POINT('Ctrl Pts',(41.3482161034861,-1.00808541351048,-10.6073986983403));
#61357=CARTESIAN_POINT('Ctrl Pts',(41.3098746085859,-1.00096362995335,-10.6816567535784));
#61358=CARTESIAN_POINT('Ctrl Pts',(41.2804846055716,-0.995803201024133,
-10.7337217191006));
#61359=CARTESIAN_POINT('Ctrl Pts',(41.1489059759915,-0.973851654072483,
-10.9477756001797));
#61360=CARTESIAN_POINT('Ctrl Pts',(41.0295074101418,-0.956499724058424,
-11.098342645472));
#61361=CARTESIAN_POINT('Ctrl Pts',(40.8580982236152,-0.934951438980654,
-11.2682889457144));
#61362=CARTESIAN_POINT('Ctrl Pts',(40.8215519556371,-0.930521510929797,
-11.3023339647333));
#61363=CARTESIAN_POINT('Ctrl Pts',(40.7587857770584,-0.923211493610641,
-11.3572553577535));
#61364=CARTESIAN_POINT('Ctrl Pts',(40.7331425864996,-0.920303007053459,
-11.3787656100313));
#61365=CARTESIAN_POINT('Ctrl Pts',(40.6957824768088,-0.916184589791054,
-11.4087985521356));
#61366=CARTESIAN_POINT('Ctrl Pts',(40.6844259905158,-0.914947966871668,
-11.4177603425062));
#61367=CARTESIAN_POINT('Ctrl Pts',(40.664471159105,-0.912802462096916,-11.4332172968114));
#61368=CARTESIAN_POINT('Ctrl Pts',(40.6559090716544,-0.911890584082797,
-11.4397579015594));
#61369=CARTESIAN_POINT('Ctrl Pts',(40.6368726519571,-0.909882422397098,
-11.4540983510461));
#61370=CARTESIAN_POINT('Ctrl Pts',(40.6263783841342,-0.908787973804472,
-11.4618707224961));
#61371=CARTESIAN_POINT('Ctrl Pts',(40.5950627594769,-0.905557433024289,
-11.4846714457539));
#61372=CARTESIAN_POINT('Ctrl Pts',(40.5740626014759,-0.903436864613035,
-11.4994529385751));
#61373=CARTESIAN_POINT('Ctrl Pts',(40.4559784833714,-0.891739579041574,
-11.5797726455348));
#61374=CARTESIAN_POINT('Ctrl Pts',(40.3544314217979,-0.882514873260403,
-11.6384967681672));
#61375=CARTESIAN_POINT('Ctrl Pts',(40.1403425388874,-0.863857246839099,
-11.7422475800258));
#61376=CARTESIAN_POINT('Ctrl Pts',(40.0278851281187,-0.85445035687532,-11.7866443225055));
#61377=CARTESIAN_POINT('Ctrl Pts',(39.8433689980804,-0.839065197000954,
-11.8438745786727));
#61378=CARTESIAN_POINT('Ctrl Pts',(39.7732366405281,-0.833230515409785,
-11.8621993639853));
#61379=CARTESIAN_POINT('Ctrl Pts',(39.6755562385137,-0.825050117861934,
-11.8830610912064));
#61380=CARTESIAN_POINT('Ctrl Pts',(39.6486274099998,-0.822789573756093,
-11.8883322169841));
#61381=CARTESIAN_POINT('Ctrl Pts',(39.6022457284012,-0.818883344256368,
-11.896589845375));
#61382=CARTESIAN_POINT('Ctrl Pts',(39.5828350998348,-0.81724480938281,-11.8998004671481));
#61383=CARTESIAN_POINT('Ctrl Pts',(39.5430830818689,-0.813880157117593,
-11.9058756492042));
#61384=CARTESIAN_POINT('Ctrl Pts',(39.5227400764741,-0.812153505219321,
-11.908718449196));
#61385=CARTESIAN_POINT('Ctrl Pts',(39.4706528571842,-0.807718762567634,
-11.915318327187));
#61386=CARTESIAN_POINT('Ctrl Pts',(39.4388666646208,-0.804999427771179,
-11.9187036532854));
#61387=CARTESIAN_POINT('Ctrl Pts',(39.2879351167644,-0.792018143778195,
-11.9317422740328));
#61388=CARTESIAN_POINT('Ctrl Pts',(39.1682663773695,-0.781510328802102,
-11.9331371720131));
#61389=CARTESIAN_POINT('Ctrl Pts',(38.9316588599438,-0.760347580343208,
-11.9182553937519));
#61390=CARTESIAN_POINT('Ctrl Pts',(38.8150118849167,-0.749726470199695,
-11.9022802890558));
#61391=CARTESIAN_POINT('Ctrl Pts',(38.6502345517776,-0.734682243548663,
-11.8672637779487));
#61392=CARTESIAN_POINT('Ctrl Pts',(38.6008110087779,-0.73016617352328,-11.8551104984827));
#61393=CARTESIAN_POINT('Ctrl Pts',(38.5191540891722,-0.722731874027611,
-11.8322606021942));
#61394=CARTESIAN_POINT('Ctrl Pts',(38.4866955948103,-0.719784115191778,
-11.8224333093868));
#61395=CARTESIAN_POINT('Ctrl Pts',(38.4406307911765,-0.71562082447408,-11.8074159831629));
#61396=CARTESIAN_POINT('Ctrl Pts',(38.4268487619857,-0.71437783381426,-11.8027843426559));
#61397=CARTESIAN_POINT('Ctrl Pts',(38.4028291182034,-0.712217075456797,
-11.7944690725746));
#61398=CARTESIAN_POINT('Ctrl Pts',(38.3925733104857,-0.711296319885992,
-11.7908405607466));
#61399=CARTESIAN_POINT('Ctrl Pts',(38.3700658375248,-0.70927978409319,-11.7827051661761));
#61400=CARTESIAN_POINT('Ctrl Pts',(38.3578257878058,-0.708185755673206,
-11.7781679813425));
#61401=CARTESIAN_POINT('Ctrl Pts',(38.3216441983335,-0.704957789828243,
-11.7644200185411));
#61402=CARTESIAN_POINT('Ctrl Pts',(38.2978113614097,-0.702839339278392,
-11.7549252801234));
#61403=CARTESIAN_POINT('Ctrl Pts',(38.1776224562475,-0.692172910258089,
-11.7048008008837));
#61404=CARTESIAN_POINT('Ctrl Pts',(38.0838249194648,-0.683901816976493,
-11.6582947693905));
#61405=CARTESIAN_POINT('Ctrl Pts',(37.9167866956374,-0.668733845661413,
-11.5614302098471));
#61406=CARTESIAN_POINT('Ctrl Pts',(37.842740648434,-0.661833368137556,-11.5128459108845));
#61407=CARTESIAN_POINT('Ctrl Pts',(37.683433909221,-0.646244850846359,-11.3952599248691));
#61408=CARTESIAN_POINT('Ctrl Pts',(37.599882706456,-0.637536988788356,-11.3242955190626));
#61409=CARTESIAN_POINT('Ctrl Pts',(37.4993221124513,-0.626077509836954,
-11.2263239470278));
#61410=CARTESIAN_POINT('Ctrl Pts',(37.4776003240274,-0.623537950713253,
-11.2043295180832));
#61411=CARTESIAN_POINT('Ctrl Pts',(37.4423063224035,-0.619297982495971,
-11.1671872987514));
#61412=CARTESIAN_POINT('Ctrl Pts',(37.4284911242284,-0.617608083252113,
-11.1522745430868));
#61413=CARTESIAN_POINT('Ctrl Pts',(37.4017413189407,-0.614274413073817,
-11.1226552113002));
#61414=CARTESIAN_POINT('Ctrl Pts',(37.3887940170948,-0.612631345239832,
-11.1079621907212));
#61415=CARTESIAN_POINT('Ctrl Pts',(37.3577461479169,-0.608617170194724,
-11.0718484420184));
#61416=CARTESIAN_POINT('Ctrl Pts',(37.3398384696034,-0.606238524660221,
-11.0502666310931));
#61417=CARTESIAN_POINT('Ctrl Pts',(37.2776769512682,-0.597748231625329,
-10.972628203479));
#61418=CARTESIAN_POINT('Ctrl Pts',(37.2355511506408,-0.591556756191932,
-10.9149251180755));
#61419=CARTESIAN_POINT('Ctrl Pts',(37.0954417969937,-0.569301551086183,
-10.7038889284044));
#61420=CARTESIAN_POINT('Ctrl Pts',(37.0123487271616,-0.552802870997992,
-10.5414212515693));
#61421=CARTESIAN_POINT('Ctrl Pts',(36.9320531266636,-0.532457693614852,
-10.3277584322718));
#61422=CARTESIAN_POINT('Ctrl Pts',(36.9169950902045,-0.528349990465802,
-10.2838763381606));
#61423=CARTESIAN_POINT('Ctrl Pts',(36.8937773224602,-0.521508468361763,
-10.2092507123473));
#61424=CARTESIAN_POINT('Ctrl Pts',(36.8849412486945,-0.518750335067983,
-10.178731858202));
#61425=CARTESIAN_POINT('Ctrl Pts',(36.873038928146,-0.514804431214643,-10.1343489801836));
#61426=CARTESIAN_POINT('Ctrl Pts',(36.8694871069858,-0.513592814716964,
-10.1206204293313));
#61427=CARTESIAN_POINT('Ctrl Pts',(36.8636825334453,-0.511553911240571,
-10.0973372897143));
#61428=CARTESIAN_POINT('Ctrl Pts',(36.8613665767668,-0.510723209795483,
-10.0877992572794));
#61429=CARTESIAN_POINT('Ctrl Pts',(36.8561579064997,-0.508814332869713,
-10.0657603925521));
#61430=CARTESIAN_POINT('Ctrl Pts',(36.8533067302849,-0.507738480842667,
-10.0532502082991));
#61431=CARTESIAN_POINT('Ctrl Pts',(36.8454483200985,-0.50468006837751,-10.017449790817));
#61432=CARTESIAN_POINT('Ctrl Pts',(36.8406865762645,-0.502710359357819,
-9.99410628726866));
#61433=CARTESIAN_POINT('Ctrl Pts',(36.8087011117947,-0.488547564514565,
-9.82447233019233));
#61434=CARTESIAN_POINT('Ctrl Pts',(36.7947531159001,-0.476947183049444,
-9.67598271019004));
#61435=CARTESIAN_POINT('Ctrl Pts',(36.794494922637,-0.45416971615562,-9.38520611973058));
#61436=CARTESIAN_POINT('Ctrl Pts',(36.8069304179357,-0.443038497416284,
-9.24356173204293));
#61437=CARTESIAN_POINT('Ctrl Pts',(36.8384305508979,-0.428442930832616,
-9.06642904939711));
#61438=CARTESIAN_POINT('Ctrl Pts',(36.8459709416617,-0.425335770726453,
-9.0291729571566));
#61439=CARTESIAN_POINT('Ctrl Pts',(36.8592619787915,-0.420387694474125,
-8.97066976464539));
#61440=CARTESIAN_POINT('Ctrl Pts',(36.8644272279409,-0.418565198507036,
-8.94929499398913));
#61441=CARTESIAN_POINT('Ctrl Pts',(36.8746141487335,-0.415145883826236,
-8.90953537515891));
#61442=CARTESIAN_POINT('Ctrl Pts',(36.8795627175104,-0.413551512429558,
-8.89113342465414));
#61443=CARTESIAN_POINT('Ctrl Pts',(36.8912736753095,-0.409921562622533,
-8.84956069051287));
#61444=CARTESIAN_POINT('Ctrl Pts',(36.8981671433941,-0.407881922372731,
-8.82642937929033));
#61445=CARTESIAN_POINT('Ctrl Pts',(36.9205263324678,-0.40154826374691,-8.75532945902034));
#61446=CARTESIAN_POINT('Ctrl Pts',(36.9371513812334,-0.39721769157694,-8.70774345322431));
#61447=CARTESIAN_POINT('Ctrl Pts',(36.9561742884834,-0.392620226322211,
-8.65833649288737));
#61448=CARTESIAN_POINT('Ctrl Pts',(36.9570951029448,-0.392398486495653,
-8.65595622638362));
#61449=CARTESIAN_POINT('Ctrl Pts',(36.9580196850438,-0.392176638896471,
-8.65357747805726));
#61450=CARTESIAN_POINT('',(36.7946201876944,-0.197865522983575,-9.52404976188649));
#61451=CARTESIAN_POINT('Ctrl Pts',(36.958019684865,-0.127039975641411,-8.65357747851736));
#61452=CARTESIAN_POINT('Ctrl Pts',(36.9576505343558,-0.127124228813632,
-8.65452722236091));
#61453=CARTESIAN_POINT('Ctrl Pts',(36.957281985783,-0.127208451975847,-8.65547720477834));
#61454=CARTESIAN_POINT('Ctrl Pts',(36.9326587191942,-0.132842740466077,
-8.71906671381011));
#61455=CARTESIAN_POINT('Ctrl Pts',(36.9110349057488,-0.138260333134959,
-8.78270226913262));
#61456=CARTESIAN_POINT('Ctrl Pts',(36.8275328646549,-0.161858681809033,
-9.0670115969281));
#61457=CARTESIAN_POINT('Ctrl Pts',(36.7947106993761,-0.179316343464792,
-9.29493353410961));
#61458=CARTESIAN_POINT('Ctrl Pts',(36.7946201876944,-0.197865522983575,
-9.52404976188649));
#61459=CARTESIAN_POINT('Ctrl Pts',(36.7946201867286,-0.197865721158756,
-9.52405220971134));
#61460=CARTESIAN_POINT('Ctrl Pts',(36.7946053573966,-0.200912647768918,
-9.56168730295258));
#61461=CARTESIAN_POINT('Ctrl Pts',(36.7954737972968,-0.203982368590893,
-9.59931586672318));
#61462=CARTESIAN_POINT('Ctrl Pts',(36.7981130034701,-0.208649764404742,
-9.65598270848096));
#61463=CARTESIAN_POINT('Ctrl Pts',(36.799228538166,-0.210227559088422,-9.67504652365907));
#61464=CARTESIAN_POINT('Ctrl Pts',(36.8018618542569,-0.213336360028488,
-9.71241294165262));
#61465=CARTESIAN_POINT('Ctrl Pts',(36.8033625044052,-0.214866737667036,
-9.73071546403343));
#61466=CARTESIAN_POINT('Ctrl Pts',(36.806768924481,-0.217928317746531,-9.76713592921464));
#61467=CARTESIAN_POINT('Ctrl Pts',(36.8086712600725,-0.21945931457882,-9.78525296839222));
#61468=CARTESIAN_POINT('Ctrl Pts',(36.8143052509201,-0.223568639754768,
-9.8336130752302));
#61469=CARTESIAN_POINT('Ctrl Pts',(36.8184060107029,-0.226158207996919,
-9.86380872622567));
#61470=CARTESIAN_POINT('Ctrl Pts',(36.8378881747162,-0.237028004862082,
-9.98933175290926));
#61471=CARTESIAN_POINT('Ctrl Pts',(36.8584267388163,-0.245463278208587,
-10.0837537458843));
#61472=CARTESIAN_POINT('Ctrl Pts',(36.9352444489017,-0.27061354709357,-10.3566897523803));
#61473=CARTESIAN_POINT('Ctrl Pts',(37.0067255259323,-0.287644922256015,
-10.5301709218145));
#61474=CARTESIAN_POINT('Ctrl Pts',(37.102620144272,-0.305013488540014,-10.7026920129553));
#61475=CARTESIAN_POINT('Ctrl Pts',(37.1077230256865,-0.305924935593701,
-10.7117340930467));
#61476=CARTESIAN_POINT('Ctrl Pts',(37.1288018071162,-0.309637505508219,
-10.7485261570884));
#61477=CARTESIAN_POINT('Ctrl Pts',(37.1452735711858,-0.312418034000643,
-10.775990730988));
#61478=CARTESIAN_POINT('Ctrl Pts',(37.169846521585,-0.316389535127212,-10.8151674456714));
#61479=CARTESIAN_POINT('Ctrl Pts',(37.1775100073349,-0.317604770564152,
-10.827148011701));
#61480=CARTESIAN_POINT('Ctrl Pts',(37.1906428809246,-0.319647519920078,
-10.8472833641629));
#61481=CARTESIAN_POINT('Ctrl Pts',(37.1960565391385,-0.320478485633885,
-10.8554735801572));
#61482=CARTESIAN_POINT('Ctrl Pts',(37.2086415065548,-0.322384763966443,
-10.8742620293065));
#61483=CARTESIAN_POINT('Ctrl Pts',(37.2158474516946,-0.323457784807811,
-10.8848365200646));
#61484=CARTESIAN_POINT('Ctrl Pts',(37.2366213090029,-0.32650071958759,-10.9148047430386));
#61485=CARTESIAN_POINT('Ctrl Pts',(37.2503920499149,-0.328457978449773,
-10.9340571588975));
#61486=CARTESIAN_POINT('Ctrl Pts',(37.3539473428187,-0.342770627150016,
-11.0744088952655));
#61487=CARTESIAN_POINT('Ctrl Pts',(37.4546696463228,-0.354515939781619,
-11.1870514656135));
#61488=CARTESIAN_POINT('Ctrl Pts',(37.6705368546013,-0.377567625247281,
-11.3870360840493));
#61489=CARTESIAN_POINT('Ctrl Pts',(37.7842793401836,-0.388825747650711,
-11.4749135738255));
#61490=CARTESIAN_POINT('Ctrl Pts',(37.9360640296467,-0.403456676568694,
-11.5718666985317));
#61491=CARTESIAN_POINT('Ctrl Pts',(37.9674106723213,-0.40645763295396,-11.5908946444739));
#61492=CARTESIAN_POINT('Ctrl Pts',(38.0178090738067,-0.411258939073821,
-11.6199319525411));
#61493=CARTESIAN_POINT('Ctrl Pts',(38.0365822569716,-0.413042339281843,
-11.6304154850886));
#61494=CARTESIAN_POINT('Ctrl Pts',(38.0724808193418,-0.416444752873385,
-11.649835638358));
#61495=CARTESIAN_POINT('Ctrl Pts',(38.0895783333149,-0.41806191553107,-11.6588204396461));
#61496=CARTESIAN_POINT('Ctrl Pts',(38.1287045597515,-0.421756382498635,
-11.6787838233279));
#61497=CARTESIAN_POINT('Ctrl Pts',(38.1507969293118,-0.423837996102882,
-11.6896319543115));
#61498=CARTESIAN_POINT('Ctrl Pts',(38.2225815847382,-0.430590315132939,
-11.7235236679048));
#61499=CARTESIAN_POINT('Ctrl Pts',(38.2728918989524,-0.435305675767486,
-11.7452077867128));
#61500=CARTESIAN_POINT('Ctrl Pts',(38.4834671916888,-0.454990944258609,
-11.8275620359684));
#61501=CARTESIAN_POINT('Ctrl Pts',(38.6492302437649,-0.470415778572469,
-11.8727320550079));
#61502=CARTESIAN_POINT('Ctrl Pts',(38.9175154726389,-0.49479893497931,-11.915845696525));
#61503=CARTESIAN_POINT('Ctrl Pts',(39.0175946853595,-0.503757827397114,
-11.9255570379214));
#61504=CARTESIAN_POINT('Ctrl Pts',(39.1381264955444,-0.514203001909242,
-11.929668414367));
#61505=CARTESIAN_POINT('Ctrl Pts',(39.1582623957683,-0.515936293450766,
-11.9301021948969));
#61506=CARTESIAN_POINT('Ctrl Pts',(39.1903133701821,-0.518674362851683,
-11.9303899885594));
#61507=CARTESIAN_POINT('Ctrl Pts',(39.2022254061207,-0.519687404601256,
-11.9304084672761));
#61508=CARTESIAN_POINT('Ctrl Pts',(39.2252407626419,-0.521635254040958,
-11.9302731935022));
#61509=CARTESIAN_POINT('Ctrl Pts',(39.2363436250541,-0.522570609573691,
-11.9301310529033));
#61510=CARTESIAN_POINT('Ctrl Pts',(39.2642566712128,-0.524912165465525,
-11.9295803698446));
#61511=CARTESIAN_POINT('Ctrl Pts',(39.2810647851144,-0.526313082427744,
-11.9290724250489));
#61512=CARTESIAN_POINT('Ctrl Pts',(39.3447909552646,-0.531594927491448,
-11.9264774701724));
#61513=CARTESIAN_POINT('Ctrl Pts',(39.3916534784455,-0.535418245935625,
-11.9231927032467));
#61514=CARTESIAN_POINT('Ctrl Pts',(39.5745100014636,-0.5502063709147,-11.9049803670079));
#61515=CARTESIAN_POINT('Ctrl Pts',(39.7092341211597,-0.560829435828447,
-11.8798358654208));
#61516=CARTESIAN_POINT('Ctrl Pts',(39.9609430511587,-0.581313284455666,
-11.8102306586759));
#61517=CARTESIAN_POINT('Ctrl Pts',(40.0780204781558,-0.591124493440695,
-11.767852498431));
#61518=CARTESIAN_POINT('Ctrl Pts',(40.2244078901485,-0.604179258208205,
-11.7016402381282));
#61519=CARTESIAN_POINT('Ctrl Pts',(40.2571817054246,-0.607154820870015,
-11.6859120330034));
#61520=CARTESIAN_POINT('Ctrl Pts',(40.3086962757693,-0.611925147577697,
-11.6597377002693));
#61521=CARTESIAN_POINT('Ctrl Pts',(40.3276763228127,-0.613703347318205,
-11.6497725831843));
#61522=CARTESIAN_POINT('Ctrl Pts',(40.3635120359704,-0.617101868061932,
-11.6303423229333));
#61523=CARTESIAN_POINT('Ctrl Pts',(40.3803918338899,-0.618720402820227,
-11.6209250050183));
#61524=CARTESIAN_POINT('Ctrl Pts',(40.4186056635731,-0.622426442660438,
-11.5989972931124));
#61525=CARTESIAN_POINT('Ctrl Pts',(40.4398635495797,-0.624518357516609,
-11.5863594580735));
#61526=CARTESIAN_POINT('Ctrl Pts',(40.5081912624154,-0.631344201179292,
-11.5442992857618));
#61527=CARTESIAN_POINT('Ctrl Pts',(40.5544347895556,-0.636124172988199,
-11.5135772087535));
#61528=CARTESIAN_POINT('Ctrl Pts',(40.7619700160412,-0.658349672976315,
-11.3651018753242));
#61529=CARTESIAN_POINT('Ctrl Pts',(40.9092524343812,-0.67644388810793,-11.2291585271754));
#61530=CARTESIAN_POINT('Ctrl Pts',(41.0701860122219,-0.698715351924136,
-11.0385203742085));
#61531=CARTESIAN_POINT('Ctrl Pts',(41.1011629268085,-0.703139428860597,
-10.9994218754691));
#61532=CARTESIAN_POINT('Ctrl Pts',(41.1508404815142,-0.710440860098934,
-10.9325482556356));
#61533=CARTESIAN_POINT('Ctrl Pts',(41.1702168998764,-0.713346538475557,
-10.9052957565473));
#61534=CARTESIAN_POINT('Ctrl Pts',(41.1971508153015,-0.717461569454214,
-10.8656903497441));
#61535=CARTESIAN_POINT('Ctrl Pts',(41.2051737986094,-0.718697561762455,
-10.8536610037202));
#61536=CARTESIAN_POINT('Ctrl Pts',(41.2190374425463,-0.720850539350313,
-10.8324627705233));
#61537=CARTESIAN_POINT('Ctrl Pts',(41.224925099825,-0.721770441437652,-10.8233256332378));
#61538=CARTESIAN_POINT('Ctrl Pts',(41.2377742678239,-0.723790347913513,
-10.8030847798643));
#61539=CARTESIAN_POINT('Ctrl Pts',(41.2447072421128,-0.724888548124252,
-10.7919636892401));
#61540=CARTESIAN_POINT('Ctrl Pts',(41.2646689946504,-0.728076920661878,
-10.7593526273752));
#61541=CARTESIAN_POINT('Ctrl Pts',(41.2774528568608,-0.730152503672205,
-10.7377135873744));
#61542=CARTESIAN_POINT('Ctrl Pts',(41.3499770859726,-0.742153955825786,
-10.6104392256674));
#61543=CARTESIAN_POINT('Ctrl Pts',(41.4020020328193,-0.751698734821834,
-10.5005898186922));
#61544=CARTESIAN_POINT('Ctrl Pts',(41.4893446289732,-0.770800223097494,
-10.2731322296154));
#61545=CARTESIAN_POINT('Ctrl Pts',(41.5244039337821,-0.780331317865127,
-10.1558284251204));
#61546=CARTESIAN_POINT('Ctrl Pts',(41.5649356343947,-0.795540738594206,
-9.96953473797695));
#61547=CARTESIAN_POINT('Ctrl Pts',(41.576618492484,-0.801057260919085,-9.90211354609797));
#61548=CARTESIAN_POINT('Ctrl Pts',(41.5888722589813,-0.808866554803386,
-9.80760635322329));
#61549=CARTESIAN_POINT('Ctrl Pts',(41.5918840865321,-0.811084440338512,
-9.78086601767553));
#61550=CARTESIAN_POINT('Ctrl Pts',(41.5963115129302,-0.814940373396231,
-9.73458895123191));
#61551=CARTESIAN_POINT('Ctrl Pts',(41.5979382776531,-0.816571751584984,
-9.71507462851267));
#61552=CARTESIAN_POINT('Ctrl Pts',(41.6007942883378,-0.819943145534581,
-9.67489418340964));
#61553=CARTESIAN_POINT('Ctrl Pts',(41.6019953383351,-0.82168389241997,-9.65422777706805));
#61554=CARTESIAN_POINT('Ctrl Pts',(41.6044082540926,-0.826201848283641,
-9.60081356017237));
#61555=CARTESIAN_POINT('Ctrl Pts',(41.6052178610343,-0.828991155719367,
-9.56805301227879));
#61556=CARTESIAN_POINT('Ctrl Pts',(41.605941310765,-0.843495569729395,-9.39890608698164));
#61557=CARTESIAN_POINT('Ctrl Pts',(41.5949246430416,-0.85553726854043,-9.2627482777573));
#61558=CARTESIAN_POINT('Ctrl Pts',(41.5526758034803,-0.878480180511616,
-9.01009392742088));
#61559=CARTESIAN_POINT('Ctrl Pts',(41.5241086247796,-0.889307105895066,
-8.89354782693177));
#61560=CARTESIAN_POINT('Ctrl Pts',(41.4692227238634,-0.905031672464801,
-8.72514823451885));
#61561=CARTESIAN_POINT('Ctrl Pts',(41.4495288153869,-0.910067874675566,
-8.67132786937599));
#61562=CARTESIAN_POINT('Ctrl Pts',(41.421331086298,-0.916525026755497,-8.60204412674338));
#61563=CARTESIAN_POINT('Ctrl Pts',(41.4145555721029,-0.918027428613019,
-8.5859030868021));
#61564=CARTESIAN_POINT('Ctrl Pts',(41.4030971195696,-0.920487709156965,
-8.55941994165993));
#61565=CARTESIAN_POINT('Ctrl Pts',(41.3985162347687,-0.921451268390977,
-8.54903475772972));
#61566=CARTESIAN_POINT('Ctrl Pts',(41.3896391063731,-0.923280448040879,
-8.52928940986313));
#61567=CARTESIAN_POINT('Ctrl Pts',(41.3853560029217,-0.924146866066089,
-8.5199238096804));
#61568=CARTESIAN_POINT('Ctrl Pts',(41.3734715017932,-0.926508209634124,
-8.49437187352784));
#61569=CARTESIAN_POINT('Ctrl Pts',(41.3657493326646,-0.927996095842519,
-8.47824186606038));
#61570=CARTESIAN_POINT('Ctrl Pts',(41.3329967440013,-0.934125112776471,
-8.41174298324939));
#61571=CARTESIAN_POINT('Ctrl Pts',(41.3063811123615,-0.938682184443969,
-8.36216886040706));
#61572=CARTESIAN_POINT('Ctrl Pts',(41.205358581952,-0.954736419501301,-8.18887819950842));
#61573=CARTESIAN_POINT('Ctrl Pts',(41.1215883563601,-0.965908567940397,
-8.07097498289049));
#61574=CARTESIAN_POINT('Ctrl Pts',(40.9528513914953,-0.986319857665062,
-7.87374664616077));
#61575=CARTESIAN_POINT('Ctrl Pts',(40.8717742230785,-0.995464373094813,
-7.79171098901711));
#61576=CARTESIAN_POINT('Ctrl Pts',(40.7616287364414,-1.00741361345873,-7.69520607401032));
#61577=CARTESIAN_POINT('Ctrl Pts',(40.7377186189714,-1.00998115489312,-7.67506719327893));
#61578=CARTESIAN_POINT('Ctrl Pts',(40.6975718811212,-1.0142547146104,-7.64256876468201));
#61579=CARTESIAN_POINT('Ctrl Pts',(40.6815577889091,-1.0159498628641,-7.62993922009585));
#61580=CARTESIAN_POINT('Ctrl Pts',(40.6498969706008,-1.01928424301281,-7.60561645421251));
#61581=CARTESIAN_POINT('Ctrl Pts',(40.6342645473025,-1.02092268072654,-7.59390715357581));
#61582=CARTESIAN_POINT('Ctrl Pts',(40.5995804165374,-1.02454188416313,-7.56858083986925));
#61583=CARTESIAN_POINT('Ctrl Pts',(40.5804691861955,-1.02652570207412,-7.55504923535757));
#61584=CARTESIAN_POINT('Ctrl Pts',(40.5130158612209,-1.03349413892013,-7.50875283754199));
#61585=CARTESIAN_POINT('Ctrl Pts',(40.4636847893441,-1.0385320505671,-7.47747398344665));
#61586=CARTESIAN_POINT('Ctrl Pts',(40.2457495452007,-1.06056219493239,-7.3501667855864));
#61587=CARTESIAN_POINT('Ctrl Pts',(40.0670215108104,-1.07814177149365,-7.2729468234314));
#61588=CARTESIAN_POINT('Ctrl Pts',(39.8331383965522,-1.0999115758875,-7.20390549084329));
#61589=CARTESIAN_POINT('Ctrl Pts',(39.7848388150505,-1.10433957284662,-7.19126732271379));
#61590=CARTESIAN_POINT('Ctrl Pts',(39.703566695604,-1.1116466695497,-7.17268356400458));
#61591=CARTESIAN_POINT('Ctrl Pts',(39.6708011300013,-1.11455414447533,-7.16590723786521));
#61592=CARTESIAN_POINT('Ctrl Pts',(39.6236823162561,-1.11867123011215,-7.15718341403897));
#61593=CARTESIAN_POINT('Ctrl Pts',(39.6094381139956,-1.11990751535879,-7.15467880801584));
#61594=CARTESIAN_POINT('Ctrl Pts',(39.5845464694439,-1.12205245815724,-7.15053311603004));
#61595=CARTESIAN_POINT('Ctrl Pts',(39.5739093965699,-1.12296411012867,-7.14883486428573));
#61596=CARTESIAN_POINT('Ctrl Pts',(39.550355274989,-1.12497176329352,-7.14523644896894));
#61597=CARTESIAN_POINT('Ctrl Pts',(39.537433703855,-1.12606593042892,-7.14336990751086));
#61598=CARTESIAN_POINT('Ctrl Pts',(39.4990620529146,-1.12929555090181,-7.13814563339019));
#61599=CARTESIAN_POINT('Ctrl Pts',(39.473571627328,-1.13141548994492,-7.13508983333882));
#61600=CARTESIAN_POINT('Ctrl Pts',(39.3436302962096,-1.14211574274377,-7.12161885937475));
#61601=CARTESIAN_POINT('Ctrl Pts',(39.2386134845332,-1.15041701082927,-7.1176392808032));
#61602=CARTESIAN_POINT('Ctrl Pts',(39.0440595157305,-1.16570462074215,-7.12300711738369));
#61603=CARTESIAN_POINT('Ctrl Pts',(38.9546683189064,-1.17269337024186,-7.13048553867086));
#61604=CARTESIAN_POINT('Ctrl Pts',(38.7588125346317,-1.18826846636985,-7.15795529539105));
#61605=CARTESIAN_POINT('Ctrl Pts',(38.6528703029104,-1.19687127925715,-7.18017781563946));
#61606=CARTESIAN_POINT('Ctrl Pts',(38.5191269931278,-1.20821225126242,-7.21779075354095));
#61607=CARTESIAN_POINT('Ctrl Pts',(38.4896264740927,-1.21074414275716,-7.22670240442171));
#61608=CARTESIAN_POINT('Ctrl Pts',(38.4409845819695,-1.21497455657757,-7.24242231831666));
#61609=CARTESIAN_POINT('Ctrl Pts',(38.4217430439486,-1.2166626638189,-7.248910956196));
#61610=CARTESIAN_POINT('Ctrl Pts',(38.3841035401946,-1.21999520008425,-7.26213683279161));
#61611=CARTESIAN_POINT('Ctrl Pts',(38.3657011508643,-1.22163894915328,-7.26885680231301));
#61612=CARTESIAN_POINT('Ctrl Pts',(38.3252554976667,-1.22528483647101,-7.28418876108049));
#61613=CARTESIAN_POINT('Ctrl Pts',(38.3032533988015,-1.22729020349183,-7.29290269027924));
#61614=CARTESIAN_POINT('Ctrl Pts',(38.2269475550794,-1.23432485861037,-7.32443388244236));
#61615=CARTESIAN_POINT('Ctrl Pts',(38.1733608057895,-1.23940827397468,-7.34891797104746));
#61616=CARTESIAN_POINT('Ctrl Pts',(37.9484489849288,-1.26138498917086,-7.4618383863218));
#61617=CARTESIAN_POINT('Ctrl Pts',(37.7872063104668,-1.27885290517371,-7.56872582852436));
#61618=CARTESIAN_POINT('Ctrl Pts',(37.6024725410414,-1.3005139505713,-7.7260417104039));
#61619=CARTESIAN_POINT('Ctrl Pts',(37.565480506542,-1.30494282118066,-7.75958457165736));
#61620=CARTESIAN_POINT('Ctrl Pts',(37.5054832969046,-1.31225118042522,-7.81749144157899));
#61621=CARTESIAN_POINT('Ctrl Pts',(37.4818953403318,-1.31515905563696,-7.84122773360221));
#61622=CARTESIAN_POINT('Ctrl Pts',(37.4488304221853,-1.31927659904696,-7.87591927996711));
#61623=CARTESIAN_POINT('Ctrl Pts',(37.4389464305759,-1.32051294954357,-7.88647857213508));
#61624=CARTESIAN_POINT('Ctrl Pts',(37.4218015959474,-1.32266631420537,-7.90512916143797));
#61625=CARTESIAN_POINT('Ctrl Pts',(37.4144995258508,-1.32358624891081,-7.9131814079284));
#61626=CARTESIAN_POINT('Ctrl Pts',(37.3985167688542,-1.32560594205811,-7.93104806818547));
#61627=CARTESIAN_POINT('Ctrl Pts',(37.3898613553141,-1.32670389922644,-7.94088425147982));
#61628=CARTESIAN_POINT('Ctrl Pts',(37.3648493224462,-1.32989085242544,-7.96978112858113));
#61629=CARTESIAN_POINT('Ctrl Pts',(37.3487096585906,-1.33196527864428,-7.98902865579706));
#61630=CARTESIAN_POINT('Ctrl Pts',(37.2561180866606,-1.34399791499374,-8.10303011362031));
#61631=CARTESIAN_POINT('Ctrl Pts',(37.1866365644862,-1.35357236251748,-8.20323918168507));
#61632=CARTESIAN_POINT('Ctrl Pts',(37.0631122753071,-1.3727165111079,-8.41389676733031));
#61633=CARTESIAN_POINT('Ctrl Pts',(37.0093448284768,-1.3822605754664,-8.52406698298727));
#61634=CARTESIAN_POINT('Ctrl Pts',(36.9621199005609,-1.39247710230569,-8.6430831418719));
#61635=CARTESIAN_POINT('Ctrl Pts',(36.9600605302133,-1.39292702021548,-8.64832682800744));
#61636=CARTESIAN_POINT('Ctrl Pts',(36.9580196842388,-1.39337735599387,-8.65357748012833));
#61637=CARTESIAN_POINT('Origin',(39.2,8.05522481984854,-9.525));
#61638=CARTESIAN_POINT('',(36.9580196848651,-2.92826949524753,-8.65357747851701));
#61639=CARTESIAN_POINT('',(36.9580195936563,-2.66377399804174,-8.65357771317761));
#61640=CARTESIAN_POINT('',(36.958019684865,8.05522481984854,-8.65357747851728));
#61641=CARTESIAN_POINT('',(36.7946202453594,-1.73347969461058,-9.5239135539112));
#61642=CARTESIAN_POINT('Ctrl Pts',(36.9580196848651,-2.92826949524753,-8.65357747851701));
#61643=CARTESIAN_POINT('Ctrl Pts',(36.9664653728173,-2.92624276699562,-8.63184856324372));
#61644=CARTESIAN_POINT('Ctrl Pts',(36.9752269914618,-2.92422984141651,-8.61024232509335));
#61645=CARTESIAN_POINT('Ctrl Pts',(36.9892742616844,-2.92113977904251,-8.57699796488788));
#61646=CARTESIAN_POINT('Ctrl Pts',(36.9943405140941,-2.92005102057367,-8.56526961916314));
#61647=CARTESIAN_POINT('Ctrl Pts',(37.0034676301304,-2.91813485665858,-8.54459446895908));
#61648=CARTESIAN_POINT('Ctrl Pts',(37.0074900351129,-2.91730531288517,-8.5356317579994));
#61649=CARTESIAN_POINT('Ctrl Pts',(37.017485748034,-2.91527966775965,-8.51371970917388));
#61650=CARTESIAN_POINT('Ctrl Pts',(37.0235194860318,-2.91408718298861,-8.50079841331756));
#61651=CARTESIAN_POINT('Ctrl Pts',(37.0435661262645,-2.9102194960717,-8.45884569215036));
#61652=CARTESIAN_POINT('Ctrl Pts',(37.0580485277825,-2.9075702850619,-8.43004052439141));
#61653=CARTESIAN_POINT('Ctrl Pts',(37.095221097092,-2.90109180436795,-8.35966720667705));
#61654=CARTESIAN_POINT('Ctrl Pts',(37.1185685129722,-2.89729274726006,-8.31846016148965));
#61655=CARTESIAN_POINT('Ctrl Pts',(37.2435567488603,-2.87811586658396,-8.1123021849734));
#61656=CARTESIAN_POINT('Ctrl Pts',(37.3636391382386,-2.86326336563732,-7.95937922375053));
#61657=CARTESIAN_POINT('Ctrl Pts',(37.5441880177366,-2.84286010390754,-7.77917553621361));
#61658=CARTESIAN_POINT('Ctrl Pts',(37.5892465045135,-2.83790254744708,-7.73751898765698));
#61659=CARTESIAN_POINT('Ctrl Pts',(37.6540693593975,-2.83090830098266,-7.68203312371446));
#61660=CARTESIAN_POINT('Ctrl Pts',(37.672526041737,-2.82893163471598,-7.66670732234453));
#61661=CARTESIAN_POINT('Ctrl Pts',(37.7065307022072,-2.82531383602521,-7.63931989059333));
#61662=CARTESIAN_POINT('Ctrl Pts',(37.7220035478372,-2.82367643426488,-7.62716795851445));
#61663=CARTESIAN_POINT('Ctrl Pts',(37.7536658787209,-2.82034210491862,-7.60292330453891));
#61664=CARTESIAN_POINT('Ctrl Pts',(37.7698621260741,-2.81864490211231,-7.59084208972367));
#61665=CARTESIAN_POINT('Ctrl Pts',(37.8107157083519,-2.81438325135221,-7.56116198944534));
#61666=CARTESIAN_POINT('Ctrl Pts',(37.8355561856122,-2.81180926190135,-7.54382270553107));
#61667=CARTESIAN_POINT('Ctrl Pts',(37.9445028502849,-2.80058784207084,-7.47079596702018));
#61668=CARTESIAN_POINT('Ctrl Pts',(38.0317257077326,-2.79176908765631,-7.41996873533486));
#61669=CARTESIAN_POINT('Ctrl Pts',(38.2619070864816,-2.76890460173019,-7.30455504405558));
#61670=CARTESIAN_POINT('Ctrl Pts',(38.4084608139233,-2.75470114299569,-7.24819170548262));
#61671=CARTESIAN_POINT('Ctrl Pts',(38.6169736417083,-2.73547180093228,-7.19058466916527));
#61672=CARTESIAN_POINT('Ctrl Pts',(38.6750767191795,-2.73021770336873,-7.17683651840131));
#61673=CARTESIAN_POINT('Ctrl Pts',(38.7514989067389,-2.72348681315844,-7.16173293385599));
#61674=CARTESIAN_POINT('Ctrl Pts',(38.7694012363258,-2.72192282034742,-7.15840556429335));
#61675=CARTESIAN_POINT('Ctrl Pts',(38.7975485828191,-2.71948545994758,-7.15350402334867));
#61676=CARTESIAN_POINT('Ctrl Pts',(38.8077684023428,-2.71860495829989,-7.15179231906073));
#61677=CARTESIAN_POINT('Ctrl Pts',(38.8291490599112,-2.71677262092749,-7.1483531900643));
#61678=CARTESIAN_POINT('Ctrl Pts',(38.8403115577687,-2.71582156509879,-7.14663822891784));
#61679=CARTESIAN_POINT('Ctrl Pts',(38.8685144605889,-2.71343177425542,-7.14250834868005));
#61680=CARTESIAN_POINT('Ctrl Pts',(38.8855699726061,-2.71199861653465,-7.1401975045989));
#61681=CARTESIAN_POINT('Ctrl Pts',(38.9565513242016,-2.70607844864992,-7.13135504436753));
#61682=CARTESIAN_POINT('Ctrl Pts',(39.0106708441463,-2.7016706182777,-7.12646729269734));
#61683=CARTESIAN_POINT('Ctrl Pts',(39.1887397394359,-2.68737452911187,-7.11645121725453));
#61684=CARTESIAN_POINT('Ctrl Pts',(39.3129275007018,-2.67772471675513,-7.11907267182811));
#61685=CARTESIAN_POINT('Ctrl Pts',(39.5712985918954,-2.65736934076381,-7.1445852796714));
#61686=CARTESIAN_POINT('Ctrl Pts',(39.7048426646519,-2.64668031436939,-7.16929143069441));
#61687=CARTESIAN_POINT('Ctrl Pts',(39.8672748190431,-2.63295702023391,-7.21379316767112));
#61688=CARTESIAN_POINT('Ctrl Pts',(39.8987838047482,-2.63026109697771,-7.22312387587738));
#61689=CARTESIAN_POINT('Ctrl Pts',(39.9498356927374,-2.62583137524336,-7.23938655451934));
#61690=CARTESIAN_POINT('Ctrl Pts',(39.9694983159628,-2.62411013766482,-7.24593118267668));
#61691=CARTESIAN_POINT('Ctrl Pts',(40.0075684337532,-2.62074647802022,-7.25915148570652));
#61692=CARTESIAN_POINT('Ctrl Pts',(40.0259838635023,-2.61910507676171,-7.26579950561746));
#61693=CARTESIAN_POINT('Ctrl Pts',(40.0694717464178,-2.61519353128294,-7.28210152035425));
#61694=CARTESIAN_POINT('Ctrl Pts',(40.0944670806706,-2.61291707238434,-7.29195203284477));
#61695=CARTESIAN_POINT('Ctrl Pts',(40.1821788643497,-2.60482458605003,-7.32822760537779));
#61696=CARTESIAN_POINT('Ctrl Pts',(40.2439273765639,-2.59893596088992,-7.35689068994492));
#61697=CARTESIAN_POINT('Ctrl Pts',(40.4131363967936,-2.58223816940257,-7.44434085920711));
#61698=CARTESIAN_POINT('Ctrl Pts',(40.517438459337,-2.57127273776156,-7.50876795016922));
#61699=CARTESIAN_POINT('Ctrl Pts',(40.7147154683156,-2.54933728009476,-7.65248977998178));
#61700=CARTESIAN_POINT('Ctrl Pts',(40.807491256365,-2.53839960018896,-7.73150186352585));
#61701=CARTESIAN_POINT('Ctrl Pts',(40.9117321389102,-2.52561446213817,-7.83489435834114));
#61702=CARTESIAN_POINT('Ctrl Pts',(40.9292904688979,-2.52344255234437,-7.85286405449222));
#61703=CARTESIAN_POINT('Ctrl Pts',(40.9555753484473,-2.5201669920687,-7.88062173948637));
#61704=CARTESIAN_POINT('Ctrl Pts',(40.9645080515691,-2.51904942333253,-7.89021070825897));
#61705=CARTESIAN_POINT('Ctrl Pts',(40.9807081918234,-2.51701525817689,-7.90788853235642));
#61706=CARTESIAN_POINT('Ctrl Pts',(40.9879995196439,-2.51609701343918,-7.91595404300137));
#61707=CARTESIAN_POINT('Ctrl Pts',(41.0048652849821,-2.51396627634168,-7.93486681390024));
#61708=CARTESIAN_POINT('Ctrl Pts',(41.0143969252349,-2.51275685806353,-7.94575142024874));
#61709=CARTESIAN_POINT('Ctrl Pts',(41.0456542870581,-2.50877054488772,-7.98210218902052));
#61710=CARTESIAN_POINT('Ctrl Pts',(41.0669479077926,-2.5060218916989,-8.00793729603912));
#61711=CARTESIAN_POINT('Ctrl Pts',(41.1186546487436,-2.49923795336438,-8.073410419126));
#61712=CARTESIAN_POINT('Ctrl Pts',(41.1483863159832,-2.49523671239902,-8.11356828170441));
#61713=CARTESIAN_POINT('Ctrl Pts',(41.2845579303251,-2.4762548398736,-8.31000410456368));
#61714=CARTESIAN_POINT('Ctrl Pts',(41.3735731068426,-2.46174208633795,-8.47753651898351));
#61715=CARTESIAN_POINT('Ctrl Pts',(41.4643539576898,-2.44169702180377,-8.71115438372618));
#61716=CARTESIAN_POINT('Ctrl Pts',(41.4844404553355,-2.43672199061006,-8.769371691334));
#61717=CARTESIAN_POINT('Ctrl Pts',(41.5092245938589,-2.42970823274468,-8.85127071592052));
#61718=CARTESIAN_POINT('Ctrl Pts',(41.5158339833155,-2.42773002566563,-8.87435243718446));
#61719=CARTESIAN_POINT('Ctrl Pts',(41.5272300326589,-2.4241102978097,-8.91652602202451));
#61720=CARTESIAN_POINT('Ctrl Pts',(41.5321300329015,-2.4224725216615,-8.93558531726609));
#61721=CARTESIAN_POINT('Ctrl Pts',(41.5415846756019,-2.4191383403646,-8.97432570660355));
#61722=CARTESIAN_POINT('Ctrl Pts',(41.5461263243038,-2.41744166828029,-8.99400829800271));
#61723=CARTESIAN_POINT('Ctrl Pts',(41.5568514513319,-2.41318317526516,-9.04331549837358));
#61724=CARTESIAN_POINT('Ctrl Pts',(41.5627245618393,-2.41061184314709,-9.07300311041458));
#61725=CARTESIAN_POINT('Ctrl Pts',(41.585671952114,-2.39942692152061,-9.20170807812199));
#61726=CARTESIAN_POINT('Ctrl Pts',(41.5970903521582,-2.39064343958362,-9.30161606706494));
#61727=CARTESIAN_POINT('Ctrl Pts',(41.6101511949565,-2.36797890325715,-9.55655650687202));
#61728=CARTESIAN_POINT('Ctrl Pts',(41.6031251808397,-2.35394546735695,-9.71157448205063));
#61729=CARTESIAN_POINT('Ctrl Pts',(41.5725456807447,-2.33469187519421,-9.92584653321972));
#61730=CARTESIAN_POINT('Ctrl Pts',(41.5614963006179,-2.32926228636641,-9.98650603050376));
#61731=CARTESIAN_POINT('Ctrl Pts',(41.5441425361879,-2.3223471705312,-10.0646168257901));
#61732=CARTESIAN_POINT('Ctrl Pts',(41.5399519925439,-2.32076858925726,-10.0825081027486));
#61733=CARTESIAN_POINT('Ctrl Pts',(41.5330705031569,-2.31831396969641,-10.110442571015));
#61734=CARTESIAN_POINT('Ctrl Pts',(41.530518902818,-2.31743063422273,-10.120518793134));
#61735=CARTESIAN_POINT('Ctrl Pts',(41.5250660502517,-2.31559780037572,-10.1414800844415));
#61736=CARTESIAN_POINT('Ctrl Pts',(41.5221535172115,-2.31464904203977,-10.152361845463));
#61737=CARTESIAN_POINT('Ctrl Pts',(41.5146369025587,-2.31227357597721,-10.1796756005211));
#61738=CARTESIAN_POINT('Ctrl Pts',(41.5099340742804,-2.31085230544626,-10.1960802907195));
#61739=CARTESIAN_POINT('Ctrl Pts',(41.4899306766198,-2.3050580412098,-10.2631542951848));
#61740=CARTESIAN_POINT('Ctrl Pts',(41.4731329754585,-2.30076006393799,-10.3133666062595));
#61741=CARTESIAN_POINT('Ctrl Pts',(41.4094935063357,-2.28610593610075,-10.4845948003884));
#61742=CARTESIAN_POINT('Ctrl Pts',(41.3545290712239,-2.27602299799529,-10.6023549900762));
#61743=CARTESIAN_POINT('Ctrl Pts',(41.224796689076,-2.25545787020721,-10.8302182485688));
#61744=CARTESIAN_POINT('Ctrl Pts',(41.1498779020061,-2.24500363664712,-10.9396960260322));
#61745=CARTESIAN_POINT('Ctrl Pts',(41.0458839470394,-2.23156636100812,-11.0676006297233));
#61746=CARTESIAN_POINT('Ctrl Pts',(41.0249237004292,-2.22890540409381,-11.0923409121332));
#61747=CARTESIAN_POINT('Ctrl Pts',(40.9898172083265,-2.22451820304751,-11.1321194935414));
#61748=CARTESIAN_POINT('Ctrl Pts',(40.9759655788389,-2.22280404991682,-11.1474132991636));
#61749=CARTESIAN_POINT('Ctrl Pts',(40.9485604466947,-2.2194435690897,-11.1769002307601));
#61750=CARTESIAN_POINT('Ctrl Pts',(40.9350265830803,-2.21779815786197,-11.1911094548241));
#61751=CARTESIAN_POINT('Ctrl Pts',(40.9023663495596,-2.21385938040228,-11.2245699815404));
#61752=CARTESIAN_POINT('Ctrl Pts',(40.8830855038397,-2.21155945620201,-11.2436658684604));
#61753=CARTESIAN_POINT('Ctrl Pts',(40.8128577232127,-2.2032676124161,-11.310904792846));
#61754=CARTESIAN_POINT('Ctrl Pts',(40.7601401834865,-2.197198175024,-11.3571371331581));
#61755=CARTESIAN_POINT('Ctrl Pts',(40.6106240806905,-2.18037584143536,-11.4771235659106));
#61756=CARTESIAN_POINT('Ctrl Pts',(40.5101357256124,-2.16947669416102,-11.5459366131396));
#61757=CARTESIAN_POINT('Ctrl Pts',(40.301652213206,-2.14782815261958,-11.6665982058393));
#61758=CARTESIAN_POINT('Ctrl Pts',(40.1941041194259,-2.13711040178768,-11.7185914528014));
#61759=CARTESIAN_POINT('Ctrl Pts',(40.0592039390597,-2.12447776094982,-11.7718385071051));
#61760=CARTESIAN_POINT('Ctrl Pts',(40.0351246759671,-2.12225335079219,-11.7808992936535));
#61761=CARTESIAN_POINT('Ctrl Pts',(39.9986006098808,-2.11892947689036,-11.7939779135871));
#61762=CARTESIAN_POINT('Ctrl Pts',(39.9862618326821,-2.11781512190141,-11.7982831019128));
#61763=CARTESIAN_POINT('Ctrl Pts',(39.963589417827,-2.11578384163529,-11.8059871669111));
#61764=CARTESIAN_POINT('Ctrl Pts',(39.9532673270887,-2.11486530375233,-11.8094166868403));
#61765=CARTESIAN_POINT('Ctrl Pts',(39.9291130923358,-2.11273005798033,-11.8172604183601));
#61766=CARTESIAN_POINT('Ctrl Pts',(39.9152637173031,-2.11151647065862,-11.8216195972571));
#61767=CARTESIAN_POINT('Ctrl Pts',(39.8690597536677,-2.10750050452594,-11.8357040735817));
#61768=CARTESIAN_POINT('Ctrl Pts',(39.8365379253333,-2.10472694514075,-11.844873721473));
#61769=CARTESIAN_POINT('Ctrl Pts',(39.754838541676,-2.09786563033089,-11.8660614816636));
#61770=CARTESIAN_POINT('Ctrl Pts',(39.7054531441479,-2.09381292943713,-11.8772186485999));
#61771=CARTESIAN_POINT('Ctrl Pts',(39.4661579753392,-2.07446602569077,-11.9233944656592));
#61772=CARTESIAN_POINT('Ctrl Pts',(39.2728558584254,-2.05965121769397,-11.937017957914));
#61773=CARTESIAN_POINT('Ctrl Pts',(39.0218807210343,-2.03951784346619,-11.9244817984788));
#61774=CARTESIAN_POINT('Ctrl Pts',(38.9638894331802,-2.03480822620075,-11.9194707450422));
#61775=CARTESIAN_POINT('Ctrl Pts',(38.8829261398952,-2.02811658586329,-11.9095050237585));
#61776=CARTESIAN_POINT('Ctrl Pts',(38.8597550139834,-2.02618810323699,-11.9063091594301));
#61777=CARTESIAN_POINT('Ctrl Pts',(38.8173305032682,-2.02263027375656,-11.8998259655057));
#61778=CARTESIAN_POINT('Ctrl Pts',(38.7980632795936,-2.02100422417672,-11.8966410216942));
#61779=CARTESIAN_POINT('Ctrl Pts',(38.7587410099753,-2.01766336751817,-11.8896479848832));
#61780=CARTESIAN_POINT('Ctrl Pts',(38.738691453329,-2.01594801491461,-11.8858184933378));
#61781=CARTESIAN_POINT('Ctrl Pts',(38.6879995138643,-2.01157927621064,-11.8754658846545));
#61782=CARTESIAN_POINT('Ctrl Pts',(38.6574323365234,-2.00891530506851,-11.8685986227104));
#61783=CARTESIAN_POINT('Ctrl Pts',(38.5140423517725,-1.99627151080999,-11.8334289772844));
#61784=CARTESIAN_POINT('Ctrl Pts',(38.4032537273423,-1.98605892900503,-11.7975687999894));
#61785=CARTESIAN_POINT('Ctrl Pts',(38.1579448335647,-1.96244969054331,-11.6980196570026));
#61786=CARTESIAN_POINT('Ctrl Pts',(38.025847369609,-1.94899394759567,-11.6295803707578));
#61787=CARTESIAN_POINT('Ctrl Pts',(37.8572415864665,-1.93124302197841,-11.5213827466607));
#61788=CARTESIAN_POINT('Ctrl Pts',(37.8144940996683,-1.926690331076,-11.4919567071594));
#61789=CARTESIAN_POINT('Ctrl Pts',(37.7587147158962,-1.92070918204399,-11.4508381951773));
#61790=CARTESIAN_POINT('Ctrl Pts',(37.7448134211079,-1.91921509494791,-11.4403558675428));
#61791=CARTESIAN_POINT('Ctrl Pts',(37.7229401471301,-1.91686013758172,-11.4234866127209));
#61792=CARTESIAN_POINT('Ctrl Pts',(37.7148933041467,-1.91599289866046,-11.417198547114));
#61793=CARTESIAN_POINT('Ctrl Pts',(37.6981944043813,-1.91419174307319,-11.4039773311442));
#61794=CARTESIAN_POINT('Ctrl Pts',(37.689549736058,-1.91325851486829,-11.397035221777));
#61795=CARTESIAN_POINT('Ctrl Pts',(37.6808576116197,-1.91231897341353,-11.3899555928775));
#61796=CARTESIAN_POINT('Ctrl Pts',(37.6807620905259,-1.91230864828542,-11.3898777799084));
#61797=CARTESIAN_POINT('Ctrl Pts',(37.6805720138282,-1.91228810209954,-11.389722916177));
#61798=CARTESIAN_POINT('Ctrl Pts',(37.680477458109,-1.91227788103222,-11.3896458655634));
#61799=CARTESIAN_POINT('Ctrl Pts',(37.6802891539906,-1.91225752587798,-11.389492398362));
#61800=CARTESIAN_POINT('Ctrl Pts',(37.6801954054617,-1.91224739177946,-11.389415981869));
#61801=CARTESIAN_POINT('Ctrl Pts',(37.6800085642005,-1.91222719418937,-11.3892636599806));
#61802=CARTESIAN_POINT('Ctrl Pts',(37.6799154714304,-1.91221713069567,-11.3891877547155));
#61803=CARTESIAN_POINT('Ctrl Pts',(37.6797297960113,-1.91219705857215,-11.3890363369682));
#61804=CARTESIAN_POINT('Ctrl Pts',(37.679637213312,-1.9121870499384,-11.388960824569));
#61805=CARTESIAN_POINT('Ctrl Pts',(37.6794524171043,-1.91216707230296,-11.3888100779622));
#61806=CARTESIAN_POINT('Ctrl Pts',(37.6793602035171,-1.91215710329381,-11.388734843779));
#61807=CARTESIAN_POINT('Ctrl Pts',(37.6791760082763,-1.9121371900711,-11.388584541869));
#61808=CARTESIAN_POINT('Ctrl Pts',(37.6790840265824,-1.91212724585386,-11.388509474164));
#61809=CARTESIAN_POINT('Ctrl Pts',(37.6789001608187,-1.91210736769551,-11.3883593957452));
#61810=CARTESIAN_POINT('Ctrl Pts',(37.6788082767311,-1.91209743375276,-11.3882843850383));
#61811=CARTESIAN_POINT('Ctrl Pts',(37.6786244737886,-1.91207756182977,-11.3881343125841));
#61812=CARTESIAN_POINT('Ctrl Pts',(37.6785325550223,-1.91206762385897,-11.3880592508979));
#61813=CARTESIAN_POINT('Ctrl Pts',(37.6783485518263,-1.91204772972628,-11.3879089695442));
#61814=CARTESIAN_POINT('Ctrl Pts',(37.678256467438,-1.91203777356833,-11.3878337498669));
#61815=CARTESIAN_POINT('Ctrl Pts',(37.678072002762,-1.91201782897752,-11.3876830459998));
#61816=CARTESIAN_POINT('Ctrl Pts',(37.6779796224312,-1.91200784053904,-11.3876075616987));
#61817=CARTESIAN_POINT('Ctrl Pts',(37.6777944352413,-1.91198781725927,-11.3874562216022));
#61818=CARTESIAN_POINT('Ctrl Pts',(37.6777016284151,-1.91197778242016,-11.3873803657248));
#61819=CARTESIAN_POINT('Ctrl Pts',(37.6775154567291,-1.91195765211476,-11.3872281746459));
#61820=CARTESIAN_POINT('Ctrl Pts',(37.6774220919557,-1.91194755665603,-11.3871518393728));
#61821=CARTESIAN_POINT('Ctrl Pts',(37.6772346713447,-1.91192729072041,-11.3869985802919));
#61822=CARTESIAN_POINT('Ctrl Pts',(37.6771406155851,-1.91191712024974,-11.386921656371));
#61823=CARTESIAN_POINT('Ctrl Pts',(37.6769516777556,-1.91189668965792,-11.3867671088341));
#61824=CARTESIAN_POINT('Ctrl Pts',(37.6768567957277,-1.91188642953864,-11.3866894850396));
#61825=CARTESIAN_POINT('Ctrl Pts',(37.6766660667654,-1.9118658046532,-11.3865334237115));
#61826=CARTESIAN_POINT('Ctrl Pts',(37.6765702200224,-1.91185543990459,-11.3864549860839));
#61827=CARTESIAN_POINT('Ctrl Pts',(37.6763774194694,-1.91183459037666,-11.3862971799787));
#61828=CARTESIAN_POINT('Ctrl Pts',(37.6762804658257,-1.91182410561168,-11.386217811347));
#61829=CARTESIAN_POINT('Ctrl Pts',(37.6760853047773,-1.91180300017491,-11.3860580222541));
#61830=CARTESIAN_POINT('Ctrl Pts',(37.6759870975043,-1.91179237951316,-11.3859776015683));
#61831=CARTESIAN_POINT('Ctrl Pts',(37.6757892770115,-1.91177098581065,-11.3858155827238));
#61832=CARTESIAN_POINT('Ctrl Pts',(37.6756896639658,-1.91176021278392,-11.38573398433));
#61833=CARTESIAN_POINT('Ctrl Pts',(37.6754888735132,-1.91173849720324,-11.3855694791457));
#61834=CARTESIAN_POINT('Ctrl Pts',(37.6753876963203,-1.91172755466701,-11.3854865721039));
#61835=CARTESIAN_POINT('Ctrl Pts',(37.6751836118604,-1.91170548212725,-11.3853193125284));
#61836=CARTESIAN_POINT('Ctrl Pts',(37.6750807048995,-1.9116943521507,-11.3852349597659));
#61837=CARTESIAN_POINT('Ctrl Pts',(37.674872987354,-1.91167188593989,-11.3850646650235));
#61838=CARTESIAN_POINT('Ctrl Pts',(37.6747681769798,-1.91166054972149,-11.3849787226788));
#61839=CARTESIAN_POINT('Ctrl Pts',(37.6745564695882,-1.91163765120927,-11.3848050970572));
#61840=CARTESIAN_POINT('Ctrl Pts',(37.6744495728697,-1.91162608894006,-11.3847174134254));
#61841=CARTESIAN_POINT('Ctrl Pts',(37.6742334994584,-1.91160271738989,-11.3845401448127));
#61842=CARTESIAN_POINT('Ctrl Pts',(37.6741243231037,-1.91159090813684,-11.3844505594398));
#61843=CARTESIAN_POINT('Ctrl Pts',(37.6739034856184,-1.91156702043832,-11.3842693172484));
#61844=CARTESIAN_POINT('Ctrl Pts',(37.6737918248025,-1.9115549420172,-11.3841776599426));
#61845=CARTESIAN_POINT('Ctrl Pts',(37.6735658003481,-1.91153049236507,-11.383992092622));
#61846=CARTESIAN_POINT('Ctrl Pts',(37.6734514371607,-1.91151812117205,-11.3838981821476));
#61847=CARTESIAN_POINT('Ctrl Pts',(37.6732197757027,-1.91149306081659,-11.3837079152298));
#61848=CARTESIAN_POINT('Ctrl Pts',(37.6731024778537,-1.91148037168769,-11.3836115582087));
#61849=CARTESIAN_POINT('Ctrl Pts',(37.6728646984584,-1.91145464852692,-11.3834161911434));
#61850=CARTESIAN_POINT('Ctrl Pts',(37.6727442174409,-1.91144161453875,-11.3833171805046));
#61851=CARTESIAN_POINT('Ctrl Pts',(37.6724998052689,-1.91141517279187,-11.3831162840996));
#61852=CARTESIAN_POINT('Ctrl Pts',(37.6723758746551,-1.91140176507653,-11.383014397631));
#61853=CARTESIAN_POINT('Ctrl Pts',(37.672124276753,-1.91137454482717,-11.3828075104909));
#61854=CARTESIAN_POINT('Ctrl Pts',(37.6719966100824,-1.91136073234305,-11.3827025090483));
#61855=CARTESIAN_POINT('Ctrl Pts',(37.6717372312687,-1.91133266909251,-11.3824891340739));
#61856=CARTESIAN_POINT('Ctrl Pts',(37.6716055198197,-1.91131841838221,-11.3823807596848));
#61857=CARTESIAN_POINT('Ctrl Pts',(37.6713377177761,-1.91128944251635,-11.382160359898));
#61858=CARTESIAN_POINT('Ctrl Pts',(37.6712016279954,-1.91127471742755,-11.3820483335731));
#61859=CARTESIAN_POINT('Ctrl Pts',(37.6709247080476,-1.91124475364979,-11.3818203276637));
#61860=CARTESIAN_POINT('Ctrl Pts',(37.6707838787709,-1.91122951503322,-11.3817043470239));
#61861=CARTESIAN_POINT('Ctrl Pts',(37.6704970877951,-1.91119848170252,-11.3814681041495));
#61862=CARTESIAN_POINT('Ctrl Pts',(37.670351127072,-1.91118268706699,-11.3813478407125));
#61863=CARTESIAN_POINT('Ctrl Pts',(37.6598043104844,-1.91004137149638,-11.3726557677545));
#61864=CARTESIAN_POINT('Ctrl Pts',(37.6494753144209,-1.90892164225766,-11.3639964171444));
#61865=CARTESIAN_POINT('Ctrl Pts',(37.6228578172749,-1.90602923860117,-11.3412978423569));
#61866=CARTESIAN_POINT('Ctrl Pts',(37.6066833820632,-1.90426482305452,-11.3271258444942));
#61867=CARTESIAN_POINT('Ctrl Pts',(37.5580263708135,-1.89892789937115,-11.2833254106963));
#61868=CARTESIAN_POINT('Ctrl Pts',(37.5261624223116,-1.89539244610117,-11.2530202457781));
#61869=CARTESIAN_POINT('Ctrl Pts',(37.3841109016649,-1.87933886847407,-11.1102991313864));
#61870=CARTESIAN_POINT('Ctrl Pts',(37.2842900034165,-1.86719485430491,-10.98810867134));
#61871=CARTESIAN_POINT('Ctrl Pts',(37.1450319382862,-1.8473294967471,-10.7787169325692));
#61872=CARTESIAN_POINT('Ctrl Pts',(37.0975896976733,-1.83981856266237,-10.6974193935182));
#61873=CARTESIAN_POINT('Ctrl Pts',(37.041125139902,-1.8296328697583,-10.586158143817));
#61874=CARTESIAN_POINT('Ctrl Pts',(37.0277453371089,-1.82710787684022,-10.5584925129879));
#61875=CARTESIAN_POINT('Ctrl Pts',(37.0064165061389,-1.82288552130397,-10.5121454682452));
#61876=CARTESIAN_POINT('Ctrl Pts',(36.998167129205,-1.82119848394521,-10.493605531908));
#61877=CARTESIAN_POINT('Ctrl Pts',(36.9823190822093,-1.81784636247049,-10.4567391357089));
#61878=CARTESIAN_POINT('Ctrl Pts',(36.9747106167337,-1.81618176325454,-10.4384186228191));
#61879=CARTESIAN_POINT('Ctrl Pts',(36.9567774487533,-1.81211867296545,-10.3936828127058));
#61880=CARTESIAN_POINT('Ctrl Pts',(36.9466919244674,-1.80971249992294,-10.3671756422357));
#61881=CARTESIAN_POINT('Ctrl Pts',(36.9098711324064,-1.80043818132898,-10.2650017162407));
#61882=CARTESIAN_POINT('Ctrl Pts',(36.88646303448,-1.79346564706005,-10.1882016251892));
#61883=CARTESIAN_POINT('Ctrl Pts',(36.8188134371045,-1.76896488256168,-9.91858272938146));
#61884=CARTESIAN_POINT('Ctrl Pts',(36.79453095014,-1.75095276175637,-9.72161219272226));
#61885=CARTESIAN_POINT('Ctrl Pts',(36.7946202453594,-1.73347969461058,-9.5239135539112));
#61886=CARTESIAN_POINT('Ctrl Pts',(36.7946202468458,-1.73347940418795,-9.52391026792988));
#61887=CARTESIAN_POINT('Ctrl Pts',(36.7946344625094,-1.73070610749909,-9.49253184906575));
#61888=CARTESIAN_POINT('Ctrl Pts',(36.795262680684,-1.72795021806407,-9.46115461872356));
#61889=CARTESIAN_POINT('Ctrl Pts',(36.7973688972366,-1.72331785970742,-9.40798124892672));
#61890=CARTESIAN_POINT('Ctrl Pts',(36.7985300327825,-1.72142919267939,-9.38617745568329));
#61891=CARTESIAN_POINT('Ctrl Pts',(36.8007365148464,-1.71859228728138,-9.35320547625162));
#61892=CARTESIAN_POINT('Ctrl Pts',(36.8015632918785,-1.71763362666677,-9.34202458687445));
#61893=CARTESIAN_POINT('Ctrl Pts',(36.803298813536,-1.71580295378608,-9.3205929167618));
#61894=CARTESIAN_POINT('Ctrl Pts',(36.8041952284393,-1.71493031388628,-9.31034132242188));
#61895=CARTESIAN_POINT('Ctrl Pts',(36.8062797047938,-1.71304789857974,-9.28814528731163));
#61896=CARTESIAN_POINT('Ctrl Pts',(36.807491421384,-1.71203943054874,-9.27620344206196));
#61897=CARTESIAN_POINT('Ctrl Pts',(36.8110206344547,-1.70931649849967,-9.2438362211175));
#61898=CARTESIAN_POINT('Ctrl Pts',(36.8135107129493,-1.70761107990901,-9.22343002628025));
#61899=CARTESIAN_POINT('Ctrl Pts',(36.8290603689129,-1.69803963448877,-9.10829682506911));
#61900=CARTESIAN_POINT('Ctrl Pts',(36.8474995805345,-1.6904238516734,-9.01436967149383));
#61901=CARTESIAN_POINT('Ctrl Pts',(36.8950757831786,-1.67546929328564,-8.8307195249898));
#61902=CARTESIAN_POINT('Ctrl Pts',(36.9239747888601,-1.66814404694808,-8.74116755198875));
#61903=CARTESIAN_POINT('Ctrl Pts',(36.9580197773588,-1.66076081124402,-8.65357724055094));
#61904=CARTESIAN_POINT('Ctrl Pts',(36.9580196842388,-1.39337735599387,-8.65357748012833));
#61905=CARTESIAN_POINT('Ctrl Pts',(36.9354256370871,-1.39836298839272,-8.71170704163551));
#61906=CARTESIAN_POINT('Ctrl Pts',(36.9151020359567,-1.40340071692287,-8.77069031601384));
#61907=CARTESIAN_POINT('Ctrl Pts',(36.8893389379021,-1.41071202753157,-8.85610567809243));
#61908=CARTESIAN_POINT('Ctrl Pts',(36.8820153155817,-1.41292563059602,-8.88194398141236));
#61909=CARTESIAN_POINT('Ctrl Pts',(36.8701045771221,-1.41677656756617,-8.92681660418947));
#61910=CARTESIAN_POINT('Ctrl Pts',(36.8653143095039,-1.41840728033982,-8.94579473795547));
#61911=CARTESIAN_POINT('Ctrl Pts',(36.8559311967046,-1.42177956399955,-8.98497808214362));
#61912=CARTESIAN_POINT('Ctrl Pts',(36.8513667805432,-1.42352188679338,-9.00518833288039));
#61913=CARTESIAN_POINT('Ctrl Pts',(36.8402404833912,-1.42804897583517,-9.05759488245969));
#61914=CARTESIAN_POINT('Ctrl Pts',(36.8340764540001,-1.43084593498062,-9.08987005912552));
#61915=CARTESIAN_POINT('Ctrl Pts',(36.8058539071643,-1.4453010036866,-9.25605067704835));
#61916=CARTESIAN_POINT('Ctrl Pts',(36.7944993087424,-1.45728194703566,-9.39149864706067));
#61917=CARTESIAN_POINT('Ctrl Pts',(36.7947506351827,-1.4823801582391,-9.67174675506811));
#61918=CARTESIAN_POINT('Ctrl Pts',(36.8079169078777,-1.49547128377747,-9.81603466411999));
#61919=CARTESIAN_POINT('Ctrl Pts',(36.8407188207255,-1.51148310714002,-9.99516141886595));
#61920=CARTESIAN_POINT('Ctrl Pts',(36.8483365229027,-1.51475187508347,-10.0318912923841));
#61921=CARTESIAN_POINT('Ctrl Pts',(36.8599675980825,-1.51918286360673,-10.0820426839337));
#61922=CARTESIAN_POINT('Ctrl Pts',(36.8632431253265,-1.52037981282759,-10.0956273137069));
#61923=CARTESIAN_POINT('Ctrl Pts',(36.8693283278617,-1.52251462448257,-10.1199330256061));
#61924=CARTESIAN_POINT('Ctrl Pts',(36.8720940520591,-1.5234548102879,-10.1306646499237));
#61925=CARTESIAN_POINT('Ctrl Pts',(36.8779960483429,-1.52539982215356,-10.1529278494931));
#61926=CARTESIAN_POINT('Ctrl Pts',(36.8811442408619,-1.52640397280442,-10.1644558023411));
#61927=CARTESIAN_POINT('Ctrl Pts',(36.8898764202107,-1.52910285820684,-10.1955182602469));
#61928=CARTESIAN_POINT('Ctrl Pts',(36.8956223641844,-1.53078881324802,-10.2150068743711));
#61929=CARTESIAN_POINT('Ctrl Pts',(36.9329782404033,-1.5412269056329,-10.3360325445979));
#61930=CARTESIAN_POINT('Ctrl Pts',(36.9710505007605,-1.54966505044021,-10.435468295947));
#61931=CARTESIAN_POINT('Ctrl Pts',(37.0942065879777,-1.57280177115797,-10.7026033335539));
#61932=CARTESIAN_POINT('Ctrl Pts',(37.1925163442957,-1.58731497773826,-10.8633264326893));
#61933=CARTESIAN_POINT('Ctrl Pts',(37.3331441732392,-1.60575739049916,-11.0423305949706));
#61934=CARTESIAN_POINT('Ctrl Pts',(37.3585510134031,-1.60901349930625,-11.0730659161128));
#61935=CARTESIAN_POINT('Ctrl Pts',(37.3993924418764,-1.61414428746227,-11.1200442834265));
#61936=CARTESIAN_POINT('Ctrl Pts',(37.4143108253912,-1.61599813701964,-11.1367282483374));
#61937=CARTESIAN_POINT('Ctrl Pts',(37.4424540770675,-1.61946018151433,-11.1673318225476));
#61938=CARTESIAN_POINT('Ctrl Pts',(37.4556171176741,-1.62106569745999,-11.1813060710724));
#61939=CARTESIAN_POINT('Ctrl Pts',(37.4853891562887,-1.62466795420364,-11.2121643279134));
#61940=CARTESIAN_POINT('Ctrl Pts',(37.502082858152,-1.62666823785331,-11.2289633528868));
#61941=CARTESIAN_POINT('Ctrl Pts',(37.5532685898059,-1.6327456209977,-11.2789729436592));
#61942=CARTESIAN_POINT('Ctrl Pts',(37.5885045820825,-1.63685508614768,-11.3114006400929));
#61943=CARTESIAN_POINT('Ctrl Pts',(37.651450254769,-1.64407698332831,-11.36595119996));
#61944=CARTESIAN_POINT('Ctrl Pts',(37.6787262022231,-1.64716977918694,-11.3885539734979));
#61945=CARTESIAN_POINT('Ctrl Pts',(37.8009510669318,-1.66087046116954,-11.4853663294297));
#61946=CARTESIAN_POINT('Ctrl Pts',(37.9008917329016,-1.67167630738012,-11.5529758131937));
#61947=CARTESIAN_POINT('Ctrl Pts',(38.1066492551813,-1.69298065015975,-11.6706996522756));
#61948=CARTESIAN_POINT('Ctrl Pts',(38.2119196680619,-1.7034488563966,-11.7211661802767));
#61949=CARTESIAN_POINT('Ctrl Pts',(38.3443515980746,-1.71584211478487,-11.7731944917434));
#61950=CARTESIAN_POINT('Ctrl Pts',(38.3684081827518,-1.71806305358278,-11.7822035510426));
#61951=CARTESIAN_POINT('Ctrl Pts',(38.4049063010458,-1.7213826721538,-11.79520912374));
#61952=CARTESIAN_POINT('Ctrl Pts',(38.4172426366712,-1.72249619230846,-11.7994921169922));
#61953=CARTESIAN_POINT('Ctrl Pts',(38.4399159224885,-1.72452646966998,-11.8071576210448));
#61954=CARTESIAN_POINT('Ctrl Pts',(38.450241414443,-1.72544483254174,-11.8105706696711));
#61955=CARTESIAN_POINT('Ctrl Pts',(38.4744103819586,-1.72758029826213,-11.818378201045));
#61956=CARTESIAN_POINT('Ctrl Pts',(38.4882710398223,-1.72879427442747,-11.8227175167785));
#61957=CARTESIAN_POINT('Ctrl Pts',(38.5345412352799,-1.73281406386245,-11.8367443038493));
#61958=CARTESIAN_POINT('Ctrl Pts',(38.5671176333956,-1.73559097755429,-11.8458742640354));
#61959=CARTESIAN_POINT('Ctrl Pts',(38.6489809543544,-1.74246299308248,-11.8669654306159));
#61960=CARTESIAN_POINT('Ctrl Pts',(38.6984752944038,-1.746522894857,-11.8780613726533));
#61961=CARTESIAN_POINT('Ctrl Pts',(38.9288038499066,-1.76513775701105,-11.9220988967067));
#61962=CARTESIAN_POINT('Ctrl Pts',(39.1126792892105,-1.77925943271524,-11.9358107217498));
#61963=CARTESIAN_POINT('Ctrl Pts',(39.3610149520364,-1.79910932381833,-11.9258578691793));
#61964=CARTESIAN_POINT('Ctrl Pts',(39.4255669656827,-1.80433491048928,-11.9206549194566));
#61965=CARTESIAN_POINT('Ctrl Pts',(39.5139569544387,-1.81163058072937,-11.9099265974573));
#61966=CARTESIAN_POINT('Ctrl Pts',(39.5380415866579,-1.81363284598129,-11.9066321385393));
#61967=CARTESIAN_POINT('Ctrl Pts',(39.5798244948633,-1.81713393019966,-11.9002702542273));
#61968=CARTESIAN_POINT('Ctrl Pts',(39.5975463563447,-1.81862752589069,-11.8973684969909));
#61969=CARTESIAN_POINT('Ctrl Pts',(39.6347244610432,-1.82178011856938,-11.8908527322555));
#61970=CARTESIAN_POINT('Ctrl Pts',(39.6541718153818,-1.82344032822295,-11.8871965244019));
#61971=CARTESIAN_POINT('Ctrl Pts',(39.7011274850626,-1.82747723417374,-11.8777673398156));
#61972=CARTESIAN_POINT('Ctrl Pts',(39.7285833194806,-1.82986137889642,-11.8717514657487));
#61973=CARTESIAN_POINT('Ctrl Pts',(39.8318503485237,-1.83892281442052,-11.8472204549441));
#61974=CARTESIAN_POINT('Ctrl Pts',(39.9068420736578,-1.84569830953144,-11.8255030185572));
#61975=CARTESIAN_POINT('Ctrl Pts',(40.1173958753497,-1.86530042950953,-11.7532599267183));
#61976=CARTESIAN_POINT('Ctrl Pts',(40.2496336645344,-1.87833784048335,-11.6941054946587));
#61977=CARTESIAN_POINT('Ctrl Pts',(40.4590725505517,-1.89986802355464,-11.5767584324833));
#61978=CARTESIAN_POINT('Ctrl Pts',(40.5395569030974,-1.90837720178088,-11.5251420582463));
#61979=CARTESIAN_POINT('Ctrl Pts',(40.6331192346114,-1.9184055121647,-11.4569502238248));
#61980=CARTESIAN_POINT('Ctrl Pts',(40.6493217785344,-1.92014726594701,-11.4448252194433));
#61981=CARTESIAN_POINT('Ctrl Pts',(40.6748325410936,-1.92289551425998,-11.425227432942));
#61982=CARTESIAN_POINT('Ctrl Pts',(40.6842410042701,-1.92391037378258,-11.4178877361122));
#61983=CARTESIAN_POINT('Ctrl Pts',(40.7023928297122,-1.92587027855501,-11.4035086394899));
#61984=CARTESIAN_POINT('Ctrl Pts',(40.7111421295302,-1.92681579067688,-11.3964775972933));
#61985=CARTESIAN_POINT('Ctrl Pts',(40.7329136821619,-1.92917154631027,-11.3787294847783));
#61986=CARTESIAN_POINT('Ctrl Pts',(40.7458734189018,-1.93057654161082,-11.3679359137715));
#61987=CARTESIAN_POINT('Ctrl Pts',(40.7976477931776,-1.93620573199632,-11.3238849187817));
#61988=CARTESIAN_POINT('Ctrl Pts',(40.8355148700228,-1.94036017627709,-11.2895275830551));
#61989=CARTESIAN_POINT('Ctrl Pts',(41.0211343156769,-1.96109816410334,-11.1099979059487));
#61990=CARTESIAN_POINT('Ctrl Pts',(41.1507942656646,-1.97690506165441,-10.9473795008363));
#61991=CARTESIAN_POINT('Ctrl Pts',(41.2932414433865,-1.99884887525265,-10.7119380842193));
#61992=CARTESIAN_POINT('Ctrl Pts',(41.3259712167862,-2.00433281922097,-10.6522650865879));
#61993=CARTESIAN_POINT('Ctrl Pts',(41.3683466101453,-2.01216068958093,-10.5665785765661));
#61994=CARTESIAN_POINT('Ctrl Pts',(41.3801411820427,-2.01443161730616,-10.5416598509604));
#61995=CARTESIAN_POINT('Ctrl Pts',(41.3995417128316,-2.01833358070243,-10.4987809584939));
#61996=CARTESIAN_POINT('Ctrl Pts',(41.4073624753316,-2.01995720175415,-10.4809204763705));
#61997=CARTESIAN_POINT('Ctrl Pts',(41.4229392324247,-2.02329890525174,-10.4441367132439));
#61998=CARTESIAN_POINT('Ctrl Pts',(41.4306727149896,-2.02501758605054,-10.4252057053825));
#61999=CARTESIAN_POINT('Ctrl Pts',(41.4497147799718,-2.02940715560897,-10.3768395313447));
#62000=CARTESIAN_POINT('Ctrl Pts',(41.4606872815429,-2.03208884147254,-10.3472773198119));
#62001=CARTESIAN_POINT('Ctrl Pts',(41.5106577153121,-2.04507996463358,-10.2040782653042));
#62002=CARTESIAN_POINT('Ctrl Pts',(41.5416796829331,-2.05563892933301,-10.0878615881593));
#62003=CARTESIAN_POINT('Ctrl Pts',(41.5941176475927,-2.080948976505,-9.80920087827473));
#62004=CARTESIAN_POINT('Ctrl Pts',(41.6078939154356,-2.09578973691369,-9.64590621584614));
#62005=CARTESIAN_POINT('Ctrl Pts',(41.6043494751469,-2.11341254458692,-9.44545540700976));
#62006=CARTESIAN_POINT('Ctrl Pts',(41.6028402356556,-2.11663885183464,-9.40845397303233));
#62007=CARTESIAN_POINT('Ctrl Pts',(41.5995880797562,-2.12102470331362,-9.3575960468872));
#62008=CARTESIAN_POINT('Ctrl Pts',(41.5985782165692,-2.12221802162794,-9.34370023849328));
#62009=CARTESIAN_POINT('Ctrl Pts',(41.5965492504183,-2.12434829859078,-9.31877874167206));
#62010=CARTESIAN_POINT('Ctrl Pts',(41.5955746539301,-2.12528755123094,-9.30774987464945));
#62011=CARTESIAN_POINT('Ctrl Pts',(41.5933880483643,-2.12723320957397,-9.28481289772041));
#62012=CARTESIAN_POINT('Ctrl Pts',(41.5921632596322,-2.12823891720237,-9.27290646049651));
#62013=CARTESIAN_POINT('Ctrl Pts',(41.5886100828805,-2.13094673076198,-9.24072687975029));
#62014=CARTESIAN_POINT('Ctrl Pts',(41.5861124432792,-2.13263995759401,-9.22047277969937));
#62015=CARTESIAN_POINT('Ctrl Pts',(41.5685248427174,-2.14337434136815,-9.09139570734533));
#62016=CARTESIAN_POINT('Ctrl Pts',(41.5462496757756,-2.15207996590962,-8.98366592118261));
#62017=CARTESIAN_POINT('Ctrl Pts',(41.4642866789329,-2.1760245993849,-8.69026564864504));
#62018=CARTESIAN_POINT('Ctrl Pts',(41.3893173865677,-2.19108400072141,-8.50978802863563));
#62019=CARTESIAN_POINT('Ctrl Pts',(41.2764386195138,-2.20973427371325,-8.31032128866595));
#62020=CARTESIAN_POINT('Ctrl Pts',(41.2588153264992,-2.21255997117743,-8.2806845562019));
#62021=CARTESIAN_POINT('Ctrl Pts',(41.2294156768879,-2.21714749667915,-8.23357901947776));
#62022=CARTESIAN_POINT('Ctrl Pts',(41.2180357110752,-2.21889495896355,-8.21586748230387));
#62023=CARTESIAN_POINT('Ctrl Pts',(41.1957039674352,-2.22227247162443,-8.18209402412461));
#62024=CARTESIAN_POINT('Ctrl Pts',(41.1847870216604,-2.22390113145698,-8.16601095770644));
#62025=CARTESIAN_POINT('Ctrl Pts',(41.1588293177958,-2.22772342382359,-8.12874954503866));
#62026=CARTESIAN_POINT('Ctrl Pts',(41.1436383406724,-2.22992258341988,-8.10767945891436));
#62027=CARTESIAN_POINT('Ctrl Pts',(41.0911707992034,-2.23739692539579,-8.03733637333358));
#62028=CARTESIAN_POINT('Ctrl Pts',(41.0523413229925,-2.24273056479687,-7.98925906429054));
#62029=CARTESIAN_POINT('Ctrl Pts',(40.9491417263286,-2.25644126994007,-7.87109465461216));
#62030=CARTESIAN_POINT('Ctrl Pts',(40.8823881354727,-2.26489818720462,-7.80323750689409));
#62031=CARTESIAN_POINT('Ctrl Pts',(40.6966582791728,-2.28732542619751,-7.6355745287832));
#62032=CARTESIAN_POINT('Ctrl Pts',(40.5717246510495,-2.3013741157912,-7.54300783761762));
#62033=CARTESIAN_POINT('Ctrl Pts',(40.4156489836125,-2.31725091756192,-7.44924084858929));
#62034=CARTESIAN_POINT('Ctrl Pts',(40.3923264097295,-2.31958217706309,-7.4357569738719));
#62035=CARTESIAN_POINT('Ctrl Pts',(40.3571557353439,-2.32303165796025,-7.41620402605447));
#62036=CARTESIAN_POINT('Ctrl Pts',(40.3454768364831,-2.3241664197728,-7.40983742979284));
#62037=CARTESIAN_POINT('Ctrl Pts',(40.3251334747504,-2.32612386422545,-7.39896543916571));
#62038=CARTESIAN_POINT('Ctrl Pts',(40.3164937971642,-2.32694918579274,-7.39441559640595));
#62039=CARTESIAN_POINT('Ctrl Pts',(40.2957681838185,-2.3289148945865,-7.38366173423172));
#62040=CARTESIAN_POINT('Ctrl Pts',(40.2836570399592,-2.33005225329119,-7.37750729265034));
#62041=CARTESIAN_POINT('Ctrl Pts',(40.2460296137541,-2.33355307338476,-7.35878580301019));
#62042=CARTESIAN_POINT('Ctrl Pts',(40.2203408611949,-2.33589689503679,-7.3465678479241));
#62043=CARTESIAN_POINT('Ctrl Pts',(40.1582137255434,-2.341470158285,-7.31835950666183));
#62044=CARTESIAN_POINT('Ctrl Pts',(40.1215826676185,-2.34467928882815,-7.30281152178092));
#62045=CARTESIAN_POINT('Ctrl Pts',(39.9679886953997,-2.35788810388624,-7.24207077879041));
#62046=CARTESIAN_POINT('Ctrl Pts',(39.8479625707221,-2.36763325367105,-7.20514624656529));
#62047=CARTESIAN_POINT('Ctrl Pts',(39.5984317758117,-2.38769407506172,-7.14927127095438));
#62048=CARTESIAN_POINT('Ctrl Pts',(39.4691803748756,-2.39798716371336,-7.13118100414007));
#62049=CARTESIAN_POINT('Ctrl Pts',(39.3069221817447,-2.41123768163434,-7.12178127007212));
#62050=CARTESIAN_POINT('Ctrl Pts',(39.2746995679688,-2.41388420389332,-7.12056401769166));
#62051=CARTESIAN_POINT('Ctrl Pts',(39.2218729167627,-2.41825358681938,-7.11963128956889));
#62052=CARTESIAN_POINT('Ctrl Pts',(39.2012789840869,-2.41996454602607,-7.11953219375207));
#62053=CARTESIAN_POINT('Ctrl Pts',(39.1610507722784,-2.4233230595095,-7.11985520035455));
#62054=CARTESIAN_POINT('Ctrl Pts',(39.1414178785351,-2.424969739521,-7.12025331149883));
#62055=CARTESIAN_POINT('Ctrl Pts',(39.0945670538021,-2.42891871644202,-7.12177740173451));
#62056=CARTESIAN_POINT('Ctrl Pts',(39.0673596977489,-2.43122766808379,-7.12312544414426));
#62057=CARTESIAN_POINT('Ctrl Pts',(38.9694148568078,-2.43960023071285,-7.12964748534889));
#62058=CARTESIAN_POINT('Ctrl Pts',(38.8988988122134,-2.44574341489144,-7.13748684132852));
#62059=CARTESIAN_POINT('Ctrl Pts',(38.7090014954281,-2.46261534773028,-7.16714403137755));
#62060=CARTESIAN_POINT('Ctrl Pts',(38.5907635621021,-2.47348623060971,-7.19489504817484));
#62061=CARTESIAN_POINT('Ctrl Pts',(38.3624381580267,-2.49500663398945,-7.26705569780629));
#62062=CARTESIAN_POINT('Ctrl Pts',(38.2525068895249,-2.50562488060572,-7.3109347388435));
#62063=CARTESIAN_POINT('Ctrl Pts',(38.1229257724841,-2.51818335390956,-7.37408471277485));
#62064=CARTESIAN_POINT('Ctrl Pts',(38.099797539035,-2.52042615344324,-7.38582254720096));
#62065=CARTESIAN_POINT('Ctrl Pts',(38.0652721476315,-2.52377155811467,-7.40405270471365));
#62066=CARTESIAN_POINT('Ctrl Pts',(38.0537317984729,-2.52488933430596,-7.41026740148545));
#62067=CARTESIAN_POINT('Ctrl Pts',(38.0327147843226,-2.52692343195401,-7.42180806478828));
#62068=CARTESIAN_POINT('Ctrl Pts',(38.0232229468893,-2.52784140635958,-7.42710418057828));
#62069=CARTESIAN_POINT('Ctrl Pts',(38.0011912566868,-2.52997090004405,-7.43959368388815));
#62070=CARTESIAN_POINT('Ctrl Pts',(37.98867986344,-2.53117935419479,-7.44683603498378));
#62071=CARTESIAN_POINT('Ctrl Pts',(37.9474673805177,-2.53515986955682,-7.47119097752929));
#62072=CARTESIAN_POINT('Ctrl Pts',(37.9190559102334,-2.53790379616859,-7.4887897857489));
#62073=CARTESIAN_POINT('Ctrl Pts',(37.8492145453966,-2.5446733380307,-7.53409206046493));
#62074=CARTESIAN_POINT('Ctrl Pts',(37.8082601834648,-2.54866509090709,-7.56250240611284));
#62075=CARTESIAN_POINT('Ctrl Pts',(37.6035272261156,-2.56890073061624,-7.71416243576407));
#62076=CARTESIAN_POINT('Ctrl Pts',(37.4551105380146,-2.58459463482503,-7.85670108677201));
#62077=CARTESIAN_POINT('Ctrl Pts',(37.2939689892477,-2.60525876972259,-8.0568042251627));
#62078=CARTESIAN_POINT('Ctrl Pts',(37.2627002843915,-2.60947809950996,-8.09831780018695));
#62079=CARTESIAN_POINT('Ctrl Pts',(37.2187585996923,-2.61575387748888,-8.16076723482489));
#62080=CARTESIAN_POINT('Ctrl Pts',(37.2050199784685,-2.61777034515942,-8.18093781830759));
#62081=CARTESIAN_POINT('Ctrl Pts',(37.1809979725102,-2.62139791857132,-8.21738602482849));
#62082=CARTESIAN_POINT('Ctrl Pts',(37.1705984735088,-2.62300456653339,-8.23358492580686));
#62083=CARTESIAN_POINT('Ctrl Pts',(37.1488032331037,-2.62645176634228,-8.26844800201589));
#62084=CARTESIAN_POINT('Ctrl Pts',(37.137465440381,-2.62829424585961,-8.28714612220379));
#62085=CARTESIAN_POINT('Ctrl Pts',(37.1068939142424,-2.63340311367296,-8.33915051827059));
#62086=CARTESIAN_POINT('Ctrl Pts',(37.0882025395988,-2.63668826477832,-8.37276599575652));
#62087=CARTESIAN_POINT('Ctrl Pts',(37.0630312599879,-2.64135273174106,-8.42070665348625));
#62088=CARTESIAN_POINT('Ctrl Pts',(37.0558727333429,-2.64270898144565,-8.43467095264946));
#62089=CARTESIAN_POINT('Ctrl Pts',(37.0290185542012,-2.64791282186277,-8.48834329229399));
#62090=CARTESIAN_POINT('Ctrl Pts',(37.0102863311945,-2.65178986437691,-8.5285206339614));
#62091=CARTESIAN_POINT('Ctrl Pts',(36.9805864919526,-2.6583773523619,-8.59710872023852));
#62092=CARTESIAN_POINT('Ctrl Pts',(36.9690327684355,-2.6610708467856,-8.62524320482257));
#62093=CARTESIAN_POINT('Ctrl Pts',(36.9580195936563,-2.66377399804174,-8.6535777131776));
#62094=CARTESIAN_POINT('Origin',(39.2,8.05522481984854,-9.525));
#62095=CARTESIAN_POINT('',(36.9580197210495,-4.20212274557561,-8.6535773854226));
#62096=CARTESIAN_POINT('',(36.958019684865,-3.93706097182542,-8.65357747851738));
#62097=CARTESIAN_POINT('',(36.958019684865,8.05522481984854,-8.65357747851728));
#62098=CARTESIAN_POINT('Ctrl Pts',(36.9580197210495,-4.20212274557561,-8.6535773854226));
#62099=CARTESIAN_POINT('Ctrl Pts',(36.9789532980316,-4.19708807503762,-8.5997198586879));
#62100=CARTESIAN_POINT('Ctrl Pts',(37.0018239103819,-4.19199730962815,-8.54662594563398));
#62101=CARTESIAN_POINT('Ctrl Pts',(37.0916764201578,-4.17337218780608,-8.35713803797883));
#62102=CARTESIAN_POINT('Ctrl Pts',(37.1696154487098,-4.15960777636597,-8.22636041517477));
#62103=CARTESIAN_POINT('Ctrl Pts',(37.2849661016787,-4.14223190600434,-8.06884894340515));
#62104=CARTESIAN_POINT('Ctrl Pts',(37.3115110053874,-4.13840032077303,-8.03458376386272));
#62105=CARTESIAN_POINT('Ctrl Pts',(37.3575349248862,-4.13204850734918,-7.97837977122856));
#62106=CARTESIAN_POINT('Ctrl Pts',(37.3765149164632,-4.12950594958048,-7.95604682548239));
#62107=CARTESIAN_POINT('Ctrl Pts',(37.3961206506064,-4.12696006776533,-7.93381416893564));
#62108=CARTESIAN_POINT('Ctrl Pts',(37.3963418037651,-4.12693136029805,-7.93356348938964));
#62109=CARTESIAN_POINT('Ctrl Pts',(37.396770574418,-4.12687572206829,-7.93307767730098));
#62110=CARTESIAN_POINT('Ctrl Pts',(37.3969781856565,-4.12684879090518,-7.93284253925882));
#62111=CARTESIAN_POINT('Ctrl Pts',(37.3973810455607,-4.12679654957534,-7.93238644472681));
#62112=CARTESIAN_POINT('Ctrl Pts',(37.3975762888425,-4.12677123906741,-7.93216548354789));
#62113=CARTESIAN_POINT('Ctrl Pts',(37.3979554642376,-4.12672209971508,-7.93173652127962));
#62114=CARTESIAN_POINT('Ctrl Pts',(37.3981393917136,-4.12669827057739,-7.93152851616316));
#62115=CARTESIAN_POINT('Ctrl Pts',(37.3984968794887,-4.12665196905311,-7.93112437129432));
#62116=CARTESIAN_POINT('Ctrl Pts',(37.3986704358203,-4.12662949640833,-7.93092822802543));
#62117=CARTESIAN_POINT('Ctrl Pts',(37.3990080304409,-4.12658579566507,-7.93054682376255));
#62118=CARTESIAN_POINT('Ctrl Pts',(37.3991720652657,-4.12656456734618,-7.93036155975378));
#62119=CARTESIAN_POINT('Ctrl Pts',(37.399491382033,-4.12652325427702,-7.93000102951215));
#62120=CARTESIAN_POINT('Ctrl Pts',(37.3996466609611,-4.12650316933541,-7.92982576066363));
#62121=CARTESIAN_POINT('Ctrl Pts',(37.3999491566322,-4.12646405198008,-7.92948442347234));
#62122=CARTESIAN_POINT('Ctrl Pts',(37.4000963707636,-4.12644501939719,-7.92931835283063));
#62123=CARTESIAN_POINT('Ctrl Pts',(37.4003833614409,-4.12640792452409,-7.92899469205353));
#62124=CARTESIAN_POINT('Ctrl Pts',(37.4005231357204,-4.12638986208348,-7.92883709988783));
#62125=CARTESIAN_POINT('Ctrl Pts',(37.400795812539,-4.12635463307465,-7.9285297446195));
#62126=CARTESIAN_POINT('Ctrl Pts',(37.4009287130801,-4.12633746637561,-7.92837997974711));
#62127=CARTESIAN_POINT('Ctrl Pts',(37.4011881559276,-4.12630396138085,-7.92808768858419));
#62128=CARTESIAN_POINT('Ctrl Pts',(37.4013146964558,-4.12628762297255,-7.92794516075973));
#62129=CARTESIAN_POINT('Ctrl Pts',(37.4015618860504,-4.12625571328808,-7.92766680755142));
#62130=CARTESIAN_POINT('Ctrl Pts',(37.4016825335585,-4.1262401419111,-7.92753098080234));
#62131=CARTESIAN_POINT('Ctrl Pts',(37.4019183621226,-4.12620971054969,-7.92726554208972));
#62132=CARTESIAN_POINT('Ctrl Pts',(37.402033541816,-4.12619485047391,-7.92713592890028));
#62133=CARTESIAN_POINT('Ctrl Pts',(37.4022588224155,-4.12616579091573,-7.92688247294624));
#62134=CARTESIAN_POINT('Ctrl Pts',(37.4023689220844,-4.12615159135594,-7.9267586291266));
#62135=CARTESIAN_POINT('Ctrl Pts',(37.4025843967646,-4.1261238064618,-7.92651630637436));
#62136=CARTESIAN_POINT('Ctrl Pts',(37.4026897707014,-4.12611022105525,-7.9263978264747));
#62137=CARTESIAN_POINT('Ctrl Pts',(37.4028961179395,-4.12608362207376,-7.92616586083553));
#62138=CARTESIAN_POINT('Ctrl Pts',(37.4029970902966,-4.12607060843263,-7.92605237421858));
#62139=CARTESIAN_POINT('Ctrl Pts',(37.4031949313833,-4.12604511415044,-7.92583005561599));
#62140=CARTESIAN_POINT('Ctrl Pts',(37.4032917991996,-4.12603263345914,-7.92572122292435));
#62141=CARTESIAN_POINT('Ctrl Pts',(37.4034817037152,-4.12600816947204,-7.92550790089866));
#62142=CARTESIAN_POINT('Ctrl Pts',(37.4035747397182,-4.12599618611548,-7.92540341079524));
#62143=CARTESIAN_POINT('Ctrl Pts',(37.4037572312183,-4.12597268407591,-7.92519848790906));
#62144=CARTESIAN_POINT('Ctrl Pts',(37.4038466859547,-4.12596116535579,-7.92509805458804));
#62145=CARTESIAN_POINT('Ctrl Pts',(37.4040222456106,-4.12593856248687,-7.92490098216027));
#62146=CARTESIAN_POINT('Ctrl Pts',(37.4041083498745,-4.12592747830098,-7.92480434253722));
#62147=CARTESIAN_POINT('Ctrl Pts',(37.4042774211697,-4.12590571677697,-7.92461461521679));
#62148=CARTESIAN_POINT('Ctrl Pts',(37.4043603877018,-4.12589503939356,-7.92452152695062));
#62149=CARTESIAN_POINT('Ctrl Pts',(37.404523379876,-4.12587406588367,-7.92433867871771));
#62150=CARTESIAN_POINT('Ctrl Pts',(37.4046034050206,-4.12586376972224,-7.92424891828947));
#62151=CARTESIAN_POINT('Ctrl Pts',(37.4047606960075,-4.1258435350015,-7.92407251904498));
#62152=CARTESIAN_POINT('Ctrl Pts',(37.4048379613342,-4.12583359641893,-7.9239858798844));
#62153=CARTESIAN_POINT('Ctrl Pts',(37.404989900738,-4.12581405497549,-7.92381553201053));
#62154=CARTESIAN_POINT('Ctrl Pts',(37.4050645743881,-4.12580445208829,-7.92373182293949));
#62155=CARTESIAN_POINT('Ctrl Pts',(37.4052114862019,-4.12578556176535,-7.92356715816415));
#62156=CARTESIAN_POINT('Ctrl Pts',(37.4052837240181,-4.12577627430047,-7.92348620208951));
#62157=CARTESIAN_POINT('Ctrl Pts',(37.4054259088033,-4.12575799600863,-7.92332687896706));
#62158=CARTESIAN_POINT('Ctrl Pts',(37.4054958554343,-4.12574900515794,-7.92324851160655));
#62159=CARTESIAN_POINT('Ctrl Pts',(37.4056335923282,-4.12573130261066,-7.92309421320107));
#62160=CARTESIAN_POINT('Ctrl Pts',(37.4057013822441,-4.1257225908974,-7.92301828191442));
#62161=CARTESIAN_POINT('Ctrl Pts',(37.405834930789,-4.12570543037012,-7.9228687136911));
#62162=CARTESIAN_POINT('Ctrl Pts',(37.4059006891946,-4.12569698152888,-7.92279507642928));
#62163=CARTESIAN_POINT('Ctrl Pts',(37.4060302913383,-4.12568033159704,-7.92264996396258));
#62164=CARTESIAN_POINT('Ctrl Pts',(37.4060941348202,-4.12567213048822,-7.92257848851863));
#62165=CARTESIAN_POINT('Ctrl Pts',(37.4063742785057,-4.1256361478853,-7.92226489368904));
#62166=CARTESIAN_POINT('Ctrl Pts',(37.4065906236066,-4.12560836938242,-7.92202281411367));
#62167=CARTESIAN_POINT('Ctrl Pts',(37.4070197056029,-4.12555329469829,-7.92154288796625));
#62168=CARTESIAN_POINT('Ctrl Pts',(37.4072324408335,-4.12552599840483,-7.92130503990681));
#62169=CARTESIAN_POINT('Ctrl Pts',(37.4076545540634,-4.12547185498491,-7.92083328628819));
#62170=CARTESIAN_POINT('Ctrl Pts',(37.4078639305308,-4.12544500775653,-7.92059937937601));
#62171=CARTESIAN_POINT('Ctrl Pts',(37.408279568603,-4.12539173051828,-7.92013522822932));
#62172=CARTESIAN_POINT('Ctrl Pts',(37.4084858288202,-4.12536530041351,-7.9199049827445));
#62173=CARTESIAN_POINT('Ctrl Pts',(37.4088954689702,-4.12531282656845,-7.91944788432453));
#62174=CARTESIAN_POINT('Ctrl Pts',(37.4090988476085,-4.12528678274524,-7.91922103028201));
#62175=CARTESIAN_POINT('Ctrl Pts',(37.4095029521103,-4.1252350516049,-7.91877045344044));
#62176=CARTESIAN_POINT('Ctrl Pts',(37.4097036768239,-4.12520936420876,-7.91854672960435));
#62177=CARTESIAN_POINT('Ctrl Pts',(37.4101026946897,-4.1251583169552,-7.91810215976993));
#62178=CARTESIAN_POINT('Ctrl Pts',(37.4103009867938,-4.12513295702687,-7.91788131283897));
#62179=CARTESIAN_POINT('Ctrl Pts',(37.4106953551029,-4.12508253653221,-7.91744225042664));
#62180=CARTESIAN_POINT('Ctrl Pts',(37.4108914303394,-4.12505747590474,-7.91722403412944));
#62181=CARTESIAN_POINT('Ctrl Pts',(37.411281575669,-4.12500762653886,-7.91678999284851));
#62182=CARTESIAN_POINT('Ctrl Pts',(37.4114756449382,-4.12498283773977,-7.91657416708302));
#62183=CARTESIAN_POINT('Ctrl Pts',(37.4118619849529,-4.12493350515906,-7.91614467208328));
#62184=CARTESIAN_POINT('Ctrl Pts',(37.4120542549334,-4.12490896132732,-7.91593100218758));
#62185=CARTESIAN_POINT('Ctrl Pts',(37.4124371995275,-4.12486009232179,-7.91550558871456));
#62186=CARTESIAN_POINT('Ctrl Pts',(37.4126278734531,-4.12483576710535,-7.91529384456808));
#62187=CARTESIAN_POINT('Ctrl Pts',(37.4130078262841,-4.12478730939674,-7.91487205619463));
#62188=CARTESIAN_POINT('Ctrl Pts',(37.413197104596,-4.1247631768665,-7.91466201146434));
#62189=CARTESIAN_POINT('Ctrl Pts',(37.4135744644207,-4.12471507893278,-7.91424339855288));
#62190=CARTESIAN_POINT('Ctrl Pts',(37.4137625454601,-4.12469111349204,-7.91403482990027));
#62191=CARTESIAN_POINT('Ctrl Pts',(37.4141377076009,-4.12464332437634,-7.9136189479316));
#62192=CARTESIAN_POINT('Ctrl Pts',(37.4143247882613,-4.12461950067569,-7.91341163426885));
#62193=CARTESIAN_POINT('Ctrl Pts',(37.4146981457748,-4.12457196983409,-7.91299804251065));
#62194=CARTESIAN_POINT('Ctrl Pts',(37.4148844223006,-4.12454826266832,-7.91279176409969));
#62195=CARTESIAN_POINT('Ctrl Pts',(37.4152563676823,-4.12450093975039,-7.9123800236916));
#62196=CARTESIAN_POINT('Ctrl Pts',(37.4154420362939,-4.12447732397798,-7.91217456144169));
#62197=CARTESIAN_POINT('Ctrl Pts',(37.4232564042349,-4.12348368463005,-7.90353012589604));
#62198=CARTESIAN_POINT('Ctrl Pts',(37.4309451422223,-4.12251783323578,-7.89514500987252));
#62199=CARTESIAN_POINT('Ctrl Pts',(37.4456939952901,-4.12068791537491,-7.87928767812337));
#62200=CARTESIAN_POINT('Ctrl Pts',(37.4527429698742,-4.11982301981645,-7.87180567157449));
#62201=CARTESIAN_POINT('Ctrl Pts',(37.4721094199341,-4.11747224703073,-7.85151174655619));
#62202=CARTESIAN_POINT('Ctrl Pts',(37.4845216177477,-4.11599329814897,-7.83879041372696));
#62203=CARTESIAN_POINT('Ctrl Pts',(37.5360401854048,-4.10996089118094,-7.78714650611917));
#62204=CARTESIAN_POINT('Ctrl Pts',(37.5763427167114,-4.10548819150956,-7.74943379609983));
#62205=CARTESIAN_POINT('Ctrl Pts',(37.7273906266859,-4.08942938825138,-7.61754123706096));
#62206=CARTESIAN_POINT('Ctrl Pts',(37.8453168031938,-4.0781803242236,-7.53205818744956));
#62207=CARTESIAN_POINT('Ctrl Pts',(38.0694773198436,-4.0576705845938,-7.39871157345516));
#62208=CARTESIAN_POINT('Ctrl Pts',(38.1728153415629,-4.04850673717436,-7.34691141991696));
#62209=CARTESIAN_POINT('Ctrl Pts',(38.3083603316237,-4.03653548916244,-7.29076410946533));
#62210=CARTESIAN_POINT('Ctrl Pts',(38.3374873760493,-4.03396641541602,-7.27935908827136));
#62211=CARTESIAN_POINT('Ctrl Pts',(38.3859662548256,-4.02969071972083,-7.2614589136261));
#62212=CARTESIAN_POINT('Ctrl Pts',(38.4051938102531,-4.02799498496983,-7.25463609629372));
#62213=CARTESIAN_POINT('Ctrl Pts',(38.4429969215956,-4.0246597396339,-7.24176087722895));
#62214=CARTESIAN_POINT('Ctrl Pts',(38.4615640599161,-4.02302102643937,-7.23568856055004));
#62215=CARTESIAN_POINT('Ctrl Pts',(38.5066943711579,-4.01903516255755,-7.22153498079274));
#62216=CARTESIAN_POINT('Ctrl Pts',(38.533326840471,-4.01668073174756,-7.21368640179291));
#62217=CARTESIAN_POINT('Ctrl Pts',(38.6269740611915,-4.00839000467793,-7.1878417468308));
#62218=CARTESIAN_POINT('Ctrl Pts',(38.6946198085465,-4.00237884242127,-7.17228746770328));
#62219=CARTESIAN_POINT('Ctrl Pts',(38.9370248085948,-3.98074145434473,-7.12748564819134));
#62220=CARTESIAN_POINT('Ctrl Pts',(39.1142241427494,-3.96469829245018,-7.11463501322177));
#62221=CARTESIAN_POINT('Ctrl Pts',(39.3419571608479,-3.94434636171703,-7.12327529256033));
#62222=CARTESIAN_POINT('Ctrl Pts',(39.3926488281336,-3.93983766250709,-7.12680889811879));
#62223=CARTESIAN_POINT('Ctrl Pts',(39.4768897713274,-3.93241398179583,-7.13536987425918));
#62224=CARTESIAN_POINT('Ctrl Pts',(39.5105121545372,-3.92946956844607,-7.13950578936547));
#62225=CARTESIAN_POINT('Ctrl Pts',(39.5584214068598,-3.92531009738881,-7.14642937226976));
#62226=CARTESIAN_POINT('Ctrl Pts',(39.572785858242,-3.9240676465764,-7.14863831186475));
#62227=CARTESIAN_POINT('Ctrl Pts',(39.5978661219795,-3.92190747460796,-7.15272813032605));
#62228=CARTESIAN_POINT('Ctrl Pts',(39.6085904291999,-3.92098677119622,-7.15455169739799));
#62229=CARTESIAN_POINT('Ctrl Pts',(39.6321604145059,-3.91896992730147,-7.15872427187156));
#62230=CARTESIAN_POINT('Ctrl Pts',(39.6449998090439,-3.91787554289805,-7.16110519697268));
#62231=CARTESIAN_POINT('Ctrl Pts',(39.6830238145486,-3.91464539556117,-7.16847712354815));
#62232=CARTESIAN_POINT('Ctrl Pts',(39.7081496906942,-3.91252515076306,-7.17376710518071));
#62233=CARTESIAN_POINT('Ctrl Pts',(39.8476157956945,-3.90081039849542,-7.20547048767433));
#62234=CARTESIAN_POINT('Ctrl Pts',(39.9600043482237,-3.89156929710719,-7.23982501214804));
#62235=CARTESIAN_POINT('Ctrl Pts',(40.1821008901161,-3.87288869501962,-7.32592555854827));
#62236=CARTESIAN_POINT('Ctrl Pts',(40.2912961120957,-3.86347518291296,-7.37802043881677));
#62237=CARTESIAN_POINT('Ctrl Pts',(40.4587820104216,-3.84809993948118,-7.4740152401336));
#62238=CARTESIAN_POINT('Ctrl Pts',(40.5197957522134,-3.84228277520531,-7.51273561472188));
#62239=CARTESIAN_POINT('Ctrl Pts',(40.601429497215,-3.83412274406667,-7.5698530321968));
#62240=CARTESIAN_POINT('Ctrl Pts',(40.623617538979,-3.83186446423351,-7.58594938708644));
#62241=CARTESIAN_POINT('Ctrl Pts',(40.6612462270892,-3.82796089790422,-7.61424117298881));
#62242=CARTESIAN_POINT('Ctrl Pts',(40.6768215897679,-3.82632273607092,-7.62625363069703));
#62243=CARTESIAN_POINT('Ctrl Pts',(40.7083639971057,-3.82295772860053,-7.65120351795884));
#62244=CARTESIAN_POINT('Ctrl Pts',(40.7243160120375,-3.82123033818843,-7.66415722232842));
#62245=CARTESIAN_POINT('Ctrl Pts',(40.7646849044199,-3.81679129434476,-7.69780584585513));
#62246=CARTESIAN_POINT('Ctrl Pts',(40.7888574283734,-3.81406835349167,-7.71878595194835));
#62247=CARTESIAN_POINT('Ctrl Pts',(40.902561207357,-3.80093673596931,-7.82152198169018));
#62248=CARTESIAN_POINT('Ctrl Pts',(40.9862292686534,-3.7902744661659,-7.90947304005815));
#62249=CARTESIAN_POINT('Ctrl Pts',(41.1360785131185,-3.76912174865601,-8.09292674472192));
#62250=CARTESIAN_POINT('Ctrl Pts',(41.2026961828504,-3.75867414896264,-8.18767392563903));
#62251=CARTESIAN_POINT('Ctrl Pts',(41.2884630035128,-3.74379354084922,-8.33052483261265));
#62252=CARTESIAN_POINT('Ctrl Pts',(41.3132956997025,-3.73927123387884,-8.37503014862045));
#62253=CARTESIAN_POINT('Ctrl Pts',(41.3522846385682,-3.73182795137076,-8.45044165359566));
#62254=CARTESIAN_POINT('Ctrl Pts',(41.3672330422283,-3.72887736385733,-8.48091854167637));
#62255=CARTESIAN_POINT('Ctrl Pts',(41.3876592106449,-3.72471084396812,-8.52489418294807));
#62256=CARTESIAN_POINT('Ctrl Pts',(41.3936664613343,-3.72346739723268,-8.53814035615214));
#62257=CARTESIAN_POINT('Ctrl Pts',(41.4039565948475,-3.72130614328152,-8.56138875891427));
#62258=CARTESIAN_POINT('Ctrl Pts',(41.4082922898067,-3.72038534344726,-8.57136669613979));
#62259=CARTESIAN_POINT('Ctrl Pts',(41.4176797458634,-3.71836906705837,-8.59337787694358));
#62260=CARTESIAN_POINT('Ctrl Pts',(41.4227014780813,-3.71727533869861,-8.6054232500178));
#62261=CARTESIAN_POINT('Ctrl Pts',(41.4372956597136,-3.71404921102,-8.64124771232734));
#62262=CARTESIAN_POINT('Ctrl Pts',(41.446586738446,-3.71193227226104,-8.66514061495986));
#62263=CARTESIAN_POINT('Ctrl Pts',(41.4970891370262,-3.70002740262558,-8.80142323874056));
#62264=CARTESIAN_POINT('Ctrl Pts',(41.5302531445201,-3.69060819809469,-8.91663295014179));
#62265=CARTESIAN_POINT('Ctrl Pts',(41.5795598851495,-3.6716749720438,-9.15302170123694));
#62266=CARTESIAN_POINT('Ctrl Pts',(41.5953331973741,-3.66218667001029,-9.27390318868021));
#62267=CARTESIAN_POINT('Ctrl Pts',(41.6056477328739,-3.64691727851862,-9.46514441927643));
#62268=CARTESIAN_POINT('Ctrl Pts',(41.6063713049834,-3.6412916789275,-9.5349577772375));
#62269=CARTESIAN_POINT('Ctrl Pts',(41.603161503988,-3.63335473955565,-9.63177995159698));
#62270=CARTESIAN_POINT('Ctrl Pts',(41.6018061915692,-3.63112173070182,-9.65884345281451));
#62271=CARTESIAN_POINT('Ctrl Pts',(41.5986820619398,-3.62724781452777,-9.70544976210793));
#62272=CARTESIAN_POINT('Ctrl Pts',(41.5971307299884,-3.62561374461683,-9.72500491589962));
#62273=CARTESIAN_POINT('Ctrl Pts',(41.5934560399586,-3.62224438149663,-9.7650987547253));
#62274=CARTESIAN_POINT('Ctrl Pts',(41.5913070512718,-3.62050842646071,-9.78563337631017));
#62275=CARTESIAN_POINT('Ctrl Pts',(41.5850971754671,-3.61601959108896,-9.83840028087918));
#62276=CARTESIAN_POINT('Ctrl Pts',(41.5806472896948,-3.61325491722198,-9.87058144189002));
#62277=CARTESIAN_POINT('Ctrl Pts',(41.5546636602376,-3.59906743619407,-10.0340225821006));
#62278=CARTESIAN_POINT('Ctrl Pts',(41.5229243160786,-3.58733485692584,-10.1634004617121));
#62279=CARTESIAN_POINT('Ctrl Pts',(41.4397342668789,-3.5639057257455,-10.4115834273111));
#62280=CARTESIAN_POINT('Ctrl Pts',(41.38906134793,-3.55225883200327,-10.530212122753));
#62281=CARTESIAN_POINT('Ctrl Pts',(41.3044020437448,-3.53613381855175,-10.6912633289709));
#62282=CARTESIAN_POINT('Ctrl Pts',(41.2781152029641,-3.5314689899327,-10.7374835902885));
#62283=CARTESIAN_POINT('Ctrl Pts',(41.241380125343,-3.52540818747297,-10.7973647791941));
#62284=CARTESIAN_POINT('Ctrl Pts',(41.232289214171,-3.52394220675367,-10.811835478693));
#62285=CARTESIAN_POINT('Ctrl Pts',(41.2169484883616,-3.52152518065634,-10.8356863570752));
#62286=CARTESIAN_POINT('Ctrl Pts',(41.2107857371713,-3.52056883923298,-10.8451214614957));
#62287=CARTESIAN_POINT('Ctrl Pts',(41.1979975565682,-3.51861459285457,-10.8644026759656));
#62288=CARTESIAN_POINT('Ctrl Pts',(41.1913651909022,-3.51761715534665,-10.874243662093));
#62289=CARTESIAN_POINT('Ctrl Pts',(41.1734040759166,-3.51495744543523,-10.9004730781691));
#62290=CARTESIAN_POINT('Ctrl Pts',(41.1619437664537,-3.51330351901142,-10.9167710200746));
#62291=CARTESIAN_POINT('Ctrl Pts',(41.0992797668646,-3.50447627766161,-11.003574229932));
#62292=CARTESIAN_POINT('Ctrl Pts',(41.0444692965066,-3.49751093621642,-11.0714095880769));
#62293=CARTESIAN_POINT('Ctrl Pts',(40.8846771709227,-3.47865809106085,-11.2485544594732));
#62294=CARTESIAN_POINT('Ctrl Pts',(40.7728772744397,-3.46695311311918,-11.3511530322382));
#62295=CARTESIAN_POINT('Ctrl Pts',(40.5886163438648,-3.44859799728784,-11.4906942505506));
#62296=CARTESIAN_POINT('Ctrl Pts',(40.5227118546039,-3.44219487720637,-11.5356317897003));
#62297=CARTESIAN_POINT('Ctrl Pts',(40.4305574262115,-3.43335649572197,-11.5919742074555));
#62298=CARTESIAN_POINT('Ctrl Pts',(40.4061531640495,-3.43102656147433,-11.6063092902611));
#62299=CARTESIAN_POINT('Ctrl Pts',(40.3642324192192,-3.42703826180018,-11.6299486750692));
#62300=CARTESIAN_POINT('Ctrl Pts',(40.3468429684908,-3.42538784940246,-11.6394732693829));
#62301=CARTESIAN_POINT('Ctrl Pts',(40.3135084569087,-3.42223043731733,-11.6571991702451));
#62302=CARTESIAN_POINT('Ctrl Pts',(40.2975854649628,-3.42072492796014,-11.6654393229157));
#62303=CARTESIAN_POINT('Ctrl Pts',(40.2599826738543,-3.41717497124717,-11.6843688683312));
#62304=CARTESIAN_POINT('Ctrl Pts',(40.2382313287017,-3.41512561719827,-11.6949107803947));
#62305=CARTESIAN_POINT('Ctrl Pts',(40.1586343863733,-3.40763832580429,-11.7320171384849));
#62306=CARTESIAN_POINT('Ctrl Pts',(40.0999044484281,-3.40213595380182,-11.7566081498705));
#62307=CARTESIAN_POINT('Ctrl Pts',(39.8395409974984,-3.37781560464478,-11.8536765858123));
#62308=CARTESIAN_POINT('Ctrl Pts',(39.6297153904147,-3.35828807712093,-11.9013562233397));
#62309=CARTESIAN_POINT('Ctrl Pts',(39.3662266600683,-3.33487102026445,-11.9251584059604));
#62310=CARTESIAN_POINT('Ctrl Pts',(39.315910056715,-3.33045426489502,-11.92811413104));
#62311=CARTESIAN_POINT('Ctrl Pts',(39.2487535190368,-3.32466078183622,-11.9299444488401));
#62312=CARTESIAN_POINT('Ctrl Pts',(39.2319688775182,-3.32322125668894,-11.9302261323537));
#62313=CARTESIAN_POINT('Ctrl Pts',(39.203971489103,-3.3208355938826,-11.9304028458654));
#62314=CARTESIAN_POINT('Ctrl Pts',(39.192760209582,-3.31988443656194,-11.9303952341023));
#62315=CARTESIAN_POINT('Ctrl Pts',(39.1695866833123,-3.31792748318182,-11.9302174695783));
#62316=CARTESIAN_POINT('Ctrl Pts',(39.1576249854969,-3.31692227211632,-11.9300364702339));
#62317=CARTESIAN_POINT('Ctrl Pts',(39.1253015719838,-3.31421802620232,-11.929306128465));
#62318=CARTESIAN_POINT('Ctrl Pts',(39.1049440355746,-3.31252782769893,-11.9285873736268));
#62319=CARTESIAN_POINT('Ctrl Pts',(38.9821664579536,-3.30239865618982,-11.9226900813933));
#62320=CARTESIAN_POINT('Ctrl Pts',(38.8801392831532,-3.29425047794686,-11.9112239274528));
#62321=CARTESIAN_POINT('Ctrl Pts',(38.642176440827,-3.27522646572246,-11.8689363942833));
#62322=CARTESIAN_POINT('Ctrl Pts',(38.5075848497028,-3.26443893238458,-11.832761937829));
#62323=CARTESIAN_POINT('Ctrl Pts',(38.3281371996946,-3.24925494190907,-11.7674091258753));
#62324=CARTESIAN_POINT('Ctrl Pts',(38.2799888757992,-3.24509938972881,-11.7480884658683));
#62325=CARTESIAN_POINT('Ctrl Pts',(38.195365669695,-3.23761217076366,-11.7109113409418));
#62326=CARTESIAN_POINT('Ctrl Pts',(38.1586469364684,-3.23429958007016,-11.6936590199096));
#62327=CARTESIAN_POINT('Ctrl Pts',(38.1024537088755,-3.22911822697883,-11.6655004186826));
#62328=CARTESIAN_POINT('Ctrl Pts',(38.0826639351457,-3.22727144536265,-11.655237064939));
#62329=CARTESIAN_POINT('Ctrl Pts',(38.0460929002093,-3.22381542298499,-11.6356208393992));
#62330=CARTESIAN_POINT('Ctrl Pts',(38.0292753689502,-3.22220877718984,-11.6263390291594));
#62331=CARTESIAN_POINT('Ctrl Pts',(37.9918657211441,-3.21859455072907,-11.6051036926888));
#62332=CARTESIAN_POINT('Ctrl Pts',(37.9713366046455,-3.21658332158825,-11.5930439989078));
#62333=CARTESIAN_POINT('Ctrl Pts',(37.9188063603266,-3.21136233349886,-11.5611272115355));
#62334=CARTESIAN_POINT('Ctrl Pts',(37.8870877743804,-3.20813676855155,-11.5408205056273));
#62335=CARTESIAN_POINT('Ctrl Pts',(37.7015898215468,-3.1888214035706,-11.4158266596755));
#62336=CARTESIAN_POINT('Ctrl Pts',(37.5599258705225,-3.17211393290507,-11.2943469481661));
#62337=CARTESIAN_POINT('Ctrl Pts',(37.3619322857455,-3.14592592451253,-11.0801647532617));
#62338=CARTESIAN_POINT('Ctrl Pts',(37.2953531773402,-3.1364814058271,-10.99787355272));
#62339=CARTESIAN_POINT('Ctrl Pts',(37.2226968545233,-3.12556214046695,-10.8948676548096));
#62340=CARTESIAN_POINT('Ctrl Pts',(37.2112046415306,-3.12381451709613,-10.8781290502756));
#62341=CARTESIAN_POINT('Ctrl Pts',(37.1932876076326,-3.12105905805202,-10.8513110799374));
#62342=CARTESIAN_POINT('Ctrl Pts',(37.1867239308571,-3.12004278821597,-10.8413264014068));
#62343=CARTESIAN_POINT('Ctrl Pts',(37.1742136133922,-3.11809304228882,-10.8219831859109));
#62344=CARTESIAN_POINT('Ctrl Pts',(37.1682568693557,-3.11715898007068,-10.8126318296403));
#62345=CARTESIAN_POINT('Ctrl Pts',(37.1534816677931,-3.11482682043273,-10.7890787537873));
#62346=CARTESIAN_POINT('Ctrl Pts',(37.1447459419464,-3.113433911843,-10.7748252619129));
#62347=CARTESIAN_POINT('Ctrl Pts',(37.1124406828129,-3.10822440847756,-10.7208601254948));
#62348=CARTESIAN_POINT('Ctrl Pts',(37.089865838044,-3.10446340398562,-10.6805604532745));
#62349=CARTESIAN_POINT('Ctrl Pts',(37.0047867861053,-3.08968072914683,-10.5178618188161));
#62350=CARTESIAN_POINT('Ctrl Pts',(36.9516559067394,-3.07900914396076,-10.3908474136524));
#62351=CARTESIAN_POINT('Ctrl Pts',(36.8825491351842,-3.06127033496665,-10.1754973039318));
#62352=CARTESIAN_POINT('Ctrl Pts',(36.8601353947718,-3.05428303189767,-10.089585621727));
#62353=CARTESIAN_POINT('Ctrl Pts',(36.8307823746546,-3.042438842247,-9.94470751144883));
#62354=CARTESIAN_POINT('Ctrl Pts',(36.8211857251668,-3.03765424644014,-9.88636977665981));
#62355=CARTESIAN_POINT('Ctrl Pts',(36.8105290415511,-3.03070536141989,-9.80237242937044));
#62356=CARTESIAN_POINT('Ctrl Pts',(36.8077153209344,-3.02859489614765,-9.77695403948363));
#62357=CARTESIAN_POINT('Ctrl Pts',(36.803482019121,-3.02486238548882,-9.73219638518592));
#62358=CARTESIAN_POINT('Ctrl Pts',(36.8018900041445,-3.02324581532336,-9.71287542717288));
#62359=CARTESIAN_POINT('Ctrl Pts',(36.7990436704656,-3.01984290016081,-9.67235227839468));
#62360=CARTESIAN_POINT('Ctrl Pts',(36.7978362967326,-3.01805524697543,-9.65114860662235));
#62361=CARTESIAN_POINT('Ctrl Pts',(36.7953671146356,-3.01326727402373,-9.59460110868981));
#62362=CARTESIAN_POINT('Ctrl Pts',(36.7946038128975,-3.01025195933057,-9.55924216341062));
#62363=CARTESIAN_POINT('Ctrl Pts',(36.7946876540845,-2.99476145035167,-9.37898726240768));
#62364=CARTESIAN_POINT('Ctrl Pts',(36.8078466843381,-2.9819201258553,-9.23442382642469));
#62365=CARTESIAN_POINT('Ctrl Pts',(36.8612781675293,-2.95529196437138,-8.94248823477183));
#62366=CARTESIAN_POINT('Ctrl Pts',(36.9027354158672,-2.94154878406301,-8.79594354544676));
#62367=CARTESIAN_POINT('Ctrl Pts',(36.9578377979202,-2.92831315340977,-8.65404554251884));
#62368=CARTESIAN_POINT('Ctrl Pts',(36.9579287230691,-2.92829132352758,-8.65381150340287));
#62369=CARTESIAN_POINT('Ctrl Pts',(36.9580196848651,-2.92826949524753,-8.65357747851701));
#62370=CARTESIAN_POINT('',(36.7946197192388,-2.74169975326257,-9.52385327436721));
#62371=CARTESIAN_POINT('Ctrl Pts',(36.9580195936563,-2.66377399804174,-8.6535777131776));
#62372=CARTESIAN_POINT('Ctrl Pts',(36.9106737021466,-2.67539490742279,-8.77538841585373));
#62373=CARTESIAN_POINT('Ctrl Pts',(36.8733187052698,-2.68721056326922,-8.90089459411834));
#62374=CARTESIAN_POINT('Ctrl Pts',(36.8303325329871,-2.70583740325456,-9.1048144841857));
#62375=CARTESIAN_POINT('Ctrl Pts',(36.8180044735395,-2.71271559683368,-9.18151787871706));
#62376=CARTESIAN_POINT('Ctrl Pts',(36.807248568324,-2.72112334906031,-9.27807134423992));
#62377=CARTESIAN_POINT('Ctrl Pts',(36.8053253359953,-2.7228005750893,-9.29747746650217));
#62378=CARTESIAN_POINT('Ctrl Pts',(36.8026196285361,-2.72547115943757,-9.32863572539961));
#62379=CARTESIAN_POINT('Ctrl Pts',(36.8016871328292,-2.72647212326772,-9.34037339463035));
#62380=CARTESIAN_POINT('Ctrl Pts',(36.8001093748583,-2.72832928820449,-9.36226861014263));
#62381=CARTESIAN_POINT('Ctrl Pts',(36.7994423303061,-2.72918664107325,-9.37242411577258));
#62382=CARTESIAN_POINT('Ctrl Pts',(36.7981671699529,-2.73099370122103,-9.39392352102553));
#62383=CARTESIAN_POINT('Ctrl Pts',(36.7975749109306,-2.73194255546792,-9.40526824213702));
#62384=CARTESIAN_POINT('Ctrl Pts',(36.7963438206684,-2.73421507975633,-9.43256250741328));
#62385=CARTESIAN_POINT('Ctrl Pts',(36.7957833186636,-2.73553484179597,-9.44851531670021));
#62386=CARTESIAN_POINT('Ctrl Pts',(36.7948835136303,-2.73847568131273,-9.48426287400214));
#62387=CARTESIAN_POINT('Ctrl Pts',(36.7946296861135,-2.74009288458285,-9.50405873585586));
#62388=CARTESIAN_POINT('Ctrl Pts',(36.7946202719557,-2.74170095028303,-9.52385618472513));
#62389=CARTESIAN_POINT('Ctrl Pts',(36.7946202733782,-2.74170070761246,-9.52385319712528));
#62390=CARTESIAN_POINT('Ctrl Pts',(36.7945125912583,-2.76004636507561,-9.74971275308896));
#62391=CARTESIAN_POINT('Ctrl Pts',(36.8262150259338,-2.77719279965518,-9.97450095176669));
#62392=CARTESIAN_POINT('Ctrl Pts',(36.9086202717484,-2.80088393047634,-10.2602076959855));
#62393=CARTESIAN_POINT('Ctrl Pts',(36.9314513592635,-2.80663604223582,-10.327892697815));
#62394=CARTESIAN_POINT('Ctrl Pts',(36.9671251313568,-2.81472008084598,-10.4199123671693));
#62395=CARTESIAN_POINT('Ctrl Pts',(36.9774259244323,-2.81696956957016,-10.4451970872159));
#62396=CARTESIAN_POINT('Ctrl Pts',(36.9958756686948,-2.82086250300826,-10.4883664363795));
#62397=CARTESIAN_POINT('Ctrl Pts',(37.0038177320463,-2.82249892060106,-10.5063370248979));
#62398=CARTESIAN_POINT('Ctrl Pts',(37.0205257432503,-2.82586444395748,-10.5429234929812));
#62399=CARTESIAN_POINT('Ctrl Pts',(37.0293121810437,-2.82759413184188,-10.5615281519121));
#62400=CARTESIAN_POINT('Ctrl Pts',(37.0524373007287,-2.8320478809966,-10.6089100720238));
#62401=CARTESIAN_POINT('Ctrl Pts',(37.067115781493,-2.83478338386549,-10.6375157469185));
#62402=CARTESIAN_POINT('Ctrl Pts',(37.1430241382827,-2.84850018615683,-10.7784203447903));
#62403=CARTESIAN_POINT('Ctrl Pts',(37.2125589543476,-2.85976644912611,-10.8859846288075));
#62404=CARTESIAN_POINT('Ctrl Pts',(37.3677845594014,-2.88259505763972,-11.08867539929));
#62405=CARTESIAN_POINT('Ctrl Pts',(37.4531878349822,-2.89411994025935,-11.1835360473055));
#62406=CARTESIAN_POINT('Ctrl Pts',(37.5748101924931,-2.90900413707591,-11.2987582923131));
#62407=CARTESIAN_POINT('Ctrl Pts',(37.6046024864356,-2.91254260614131,-11.3256020068992));
#62408=CARTESIAN_POINT('Ctrl Pts',(37.650423930098,-2.91781138372669,-11.3648577600313));
#62409=CARTESIAN_POINT('Ctrl Pts',(37.6659603131952,-2.91956907524939,-11.377831586249));
#62410=CARTESIAN_POINT('Ctrl Pts',(37.6938765430166,-2.92267420502874,-11.4005514397745));
#62411=CARTESIAN_POINT('Ctrl Pts',(37.7061916685781,-2.92402610656255,-11.4103747055352));
#62412=CARTESIAN_POINT('Ctrl Pts',(37.7187457928655,-2.92538555859961,-11.4201883682473));
#62413=CARTESIAN_POINT('Ctrl Pts',(37.7188886944257,-2.92540103059182,-11.4203000495419));
#62414=CARTESIAN_POINT('Ctrl Pts',(37.7191742267598,-2.92543194040184,-11.4205231484909));
#62415=CARTESIAN_POINT('Ctrl Pts',(37.7193168574513,-2.92544737822079,-11.4206345661887));
#62416=CARTESIAN_POINT('Ctrl Pts',(37.7196021645189,-2.92547825396057,-11.4208573854247));
#62417=CARTESIAN_POINT('Ctrl Pts',(37.7197448409393,-2.92549369188551,-11.4209687869902));
#62418=CARTESIAN_POINT('Ctrl Pts',(37.7200305625532,-2.92552460278646,-11.4211918261474));
#62419=CARTESIAN_POINT('Ctrl Pts',(37.7201736077866,-2.92554007575513,-11.4213034636454));
#62420=CARTESIAN_POINT('Ctrl Pts',(37.7204603997792,-2.92557109269399,-11.421527233924));
#62421=CARTESIAN_POINT('Ctrl Pts',(37.7206041466505,-2.92558663665323,-11.4216393665453));
#62422=CARTESIAN_POINT('Ctrl Pts',(37.7208926876854,-2.92561783288506,-11.4218643959884));
#62423=CARTESIAN_POINT('Ctrl Pts',(37.7210374820546,-2.92563348514481,-11.4219772925957));
#62424=CARTESIAN_POINT('Ctrl Pts',(37.7213284807267,-2.92566493706534,-11.4222041315706));
#62425=CARTESIAN_POINT('Ctrl Pts',(37.7214746852202,-2.92568073669882,-11.4223180735748));
#62426=CARTESIAN_POINT('Ctrl Pts',(37.7217688877519,-2.92571252466894,-11.4225473006952));
#62427=CARTESIAN_POINT('Ctrl Pts',(37.7219168861233,-2.92572851297974,-11.4226625854104));
#62428=CARTESIAN_POINT('Ctrl Pts',(37.7222150858603,-2.925760722342,-11.422894814835));
#62429=CARTESIAN_POINT('Ctrl Pts',(37.7223652876605,-2.92577694336323,-11.4230117590589));
#62430=CARTESIAN_POINT('Ctrl Pts',(37.7311257906304,-2.92672287608498,-11.429830847469));
#62431=CARTESIAN_POINT('Ctrl Pts',(37.7397819318189,-2.92764871883772,-11.4364746177967));
#62432=CARTESIAN_POINT('Ctrl Pts',(37.7567689312453,-2.92944804862587,-11.4493297514159));
#62433=CARTESIAN_POINT('Ctrl Pts',(37.7650952612827,-2.93032193515376,-11.4555463769337));
#62434=CARTESIAN_POINT('Ctrl Pts',(37.7882492186177,-2.93273065242486,-11.4726010829805));
#62435=CARTESIAN_POINT('Ctrl Pts',(37.8031615332257,-2.93425795194307,-11.4833239283069));
#62436=CARTESIAN_POINT('Ctrl Pts',(37.868586402283,-2.9408621797548,-11.5292406743148));
#62437=CARTESIAN_POINT('Ctrl Pts',(37.9203218509282,-2.94583762920622,-11.5626624850716));
#62438=CARTESIAN_POINT('Ctrl Pts',(38.1065169523827,-2.96311522128256,-11.6730541846325));
#62439=CARTESIAN_POINT('Ctrl Pts',(38.2470692183789,-2.97507219921551,-11.7389942489519));
#62440=CARTESIAN_POINT('Ctrl Pts',(38.4876521710619,-2.99522155030195,-11.8246761388048));
#62441=CARTESIAN_POINT('Ctrl Pts',(38.5843186943765,-3.00323510386928,-11.8524196137286));
#62442=CARTESIAN_POINT('Ctrl Pts',(38.7119768916635,-3.01391124669849,-11.880547061124));
#62443=CARTESIAN_POINT('Ctrl Pts',(38.7416452834822,-3.0163983692474,-11.8864993753687));
#62444=CARTESIAN_POINT('Ctrl Pts',(38.791289166463,-3.02057471908716,-11.8954886121179));
#62445=CARTESIAN_POINT('Ctrl Pts',(38.8112054589267,-3.02225409348217,-11.8988364641464));
#62446=CARTESIAN_POINT('Ctrl Pts',(38.850601760986,-3.02558510999255,-11.9049497603531));
#62447=CARTESIAN_POINT('Ctrl Pts',(38.8700782442013,-3.02723622045584,-11.9077277597645));
#62448=CARTESIAN_POINT('Ctrl Pts',(38.9179120423565,-3.03130325382365,-11.9139527583822));
#62449=CARTESIAN_POINT('Ctrl Pts',(38.9463001317429,-3.0337272063567,-11.9171340103329));
#62450=CARTESIAN_POINT('Ctrl Pts',(39.050078705026,-3.04263028380864,-11.9268957445653));
#62451=CARTESIAN_POINT('Ctrl Pts',(39.1257036524631,-3.04920019853352,-11.9304224195146));
#62452=CARTESIAN_POINT('Ctrl Pts',(39.3970729025622,-3.07308627547469,-11.9302688873136));
#62453=CARTESIAN_POINT('Ctrl Pts',(39.592011822878,-3.09089771757061,-11.9062746803096));
#62454=CARTESIAN_POINT('Ctrl Pts',(39.8325940921913,-3.11286321237424,-11.8462948462959));
#62455=CARTESIAN_POINT('Ctrl Pts',(39.8828908118675,-3.11744883283595,-11.8319994102766));
#62456=CARTESIAN_POINT('Ctrl Pts',(39.9488701921998,-3.12342428717553,-11.8108991843903));
#62457=CARTESIAN_POINT('Ctrl Pts',(39.9649994062981,-3.12488179196278,-11.8055520395921));
#62458=CARTESIAN_POINT('Ctrl Pts',(39.9917098663996,-3.12728859259921,-11.796381727355));
#62459=CARTESIAN_POINT('Ctrl Pts',(40.0023231263142,-3.12824309705897,-11.792654534464));
#62460=CARTESIAN_POINT('Ctrl Pts',(40.0241026973336,-3.13019758625375,-11.7848338676353));
#62461=CARTESIAN_POINT('Ctrl Pts',(40.0352654538315,-3.13119706866889,-11.7807318115428));
#62462=CARTESIAN_POINT('Ctrl Pts',(40.0651637042264,-3.13386920599787,-11.7694925123443));
#62463=CARTESIAN_POINT('Ctrl Pts',(40.0838417246682,-3.13553337626812,-11.7622033344472));
#62464=CARTESIAN_POINT('Ctrl Pts',(40.1860640249784,-3.14462451426257,-11.7208305122501));
#62465=CARTESIAN_POINT('Ctrl Pts',(40.2677420373222,-3.15182808097302,-11.682295863224));
#62466=CARTESIAN_POINT('Ctrl Pts',(40.4779120656208,-3.1707065911303,-11.5682699367938));
#62467=CARTESIAN_POINT('Ctrl Pts',(40.6018787005989,-3.18222158329457,-11.4852927418002));
#62468=CARTESIAN_POINT('Ctrl Pts',(40.7787623865758,-3.20032910513542,-11.3414857126284));
#62469=CARTESIAN_POINT('Ctrl Pts',(40.8376383747717,-3.20668397014376,-11.2885898687909));
#62470=CARTESIAN_POINT('Ctrl Pts',(40.9138401663082,-3.21546638591471,-11.2130170859233));
#62471=CARTESIAN_POINT('Ctrl Pts',(40.933530992621,-3.21779040565194,-11.1927889434943));
#62472=CARTESIAN_POINT('Ctrl Pts',(40.9664265139555,-3.22177138350558,-11.1577837434004));
#62473=CARTESIAN_POINT('Ctrl Pts',(40.9798132625443,-3.22342045517352,-11.143181103333));
#62474=CARTESIAN_POINT('Ctrl Pts',(41.0049737547915,-3.22657716867864,-11.1150454044706));
#62475=CARTESIAN_POINT('Ctrl Pts',(41.0167795265731,-3.22808333805738,-11.1015426598486));
#62476=CARTESIAN_POINT('Ctrl Pts',(41.0471846758565,-3.23202943847918,-11.0659719677585));
#62477=CARTESIAN_POINT('Ctrl Pts',(41.0655392514378,-3.23447899622937,-11.0436997654892));
#62478=CARTESIAN_POINT('Ctrl Pts',(41.1323949476538,-3.24366252086882,-10.959533215383));
#62479=CARTESIAN_POINT('Ctrl Pts',(41.1782473047807,-3.25049536623026,-10.8956095295234));
#62480=CARTESIAN_POINT('Ctrl Pts',(41.3247542283779,-3.27430112158797,-10.6686574124892));
#62481=CARTESIAN_POINT('Ctrl Pts',(41.409024172745,-3.2917250180917,-10.4959443470384));
#62482=CARTESIAN_POINT('Ctrl Pts',(41.4892366481062,-3.31336340570383,-10.2652888262993));
#62483=CARTESIAN_POINT('Ctrl Pts',(41.5049123780111,-3.31798912518039,-10.2149362451749));
#62484=CARTESIAN_POINT('Ctrl Pts',(41.5234491569062,-3.32400770370209,-10.1476775219903));
#62485=CARTESIAN_POINT('Ctrl Pts',(41.5278019821482,-3.32546941382646,-10.1312023295843));
#62486=CARTESIAN_POINT('Ctrl Pts',(41.5347393171738,-3.32788120684464,-10.1037676518486));
#62487=CARTESIAN_POINT('Ctrl Pts',(41.5374225516675,-3.32883654233937,-10.0928340528802));
#62488=CARTESIAN_POINT('Ctrl Pts',(41.5424358324578,-3.3306655171095,-10.0717681300744));
#62489=CARTESIAN_POINT('Ctrl Pts',(41.544777099896,-3.33153982056055,-10.0616389677891));
#62490=CARTESIAN_POINT('Ctrl Pts',(41.5510784718428,-3.33395115290408,-10.033548175126));
#62491=CARTESIAN_POINT('Ctrl Pts',(41.5548984717067,-3.33548062314349,-10.0155552758631));
#62492=CARTESIAN_POINT('Ctrl Pts',(41.5706655284014,-3.34211212739278,-9.93685631979261));
#62493=CARTESIAN_POINT('Ctrl Pts',(41.5804755878746,-3.34711163142915,-9.87573978007214));
#62494=CARTESIAN_POINT('Ctrl Pts',(41.606512469333,-3.36438811380741,-9.66083274944916));
#62495=CARTESIAN_POINT('Ctrl Pts',(41.6102684935216,-3.37632344124629,-9.50591696153514));
#62496=CARTESIAN_POINT('Ctrl Pts',(41.5918945590781,-3.39644548904117,-9.25154476645736));
#62497=CARTESIAN_POINT('Ctrl Pts',(41.5783956055124,-3.40445427168342,-9.15194845928137));
#62498=CARTESIAN_POINT('Ctrl Pts',(41.5527848385508,-3.41512501698208,-9.02382964780018));
#62499=CARTESIAN_POINT('Ctrl Pts',(41.5462956488388,-3.41761175062244,-8.99427899859305));
#62500=CARTESIAN_POINT('Ctrl Pts',(41.5345484472633,-3.42178763145481,-8.94522046040301));
#62501=CARTESIAN_POINT('Ctrl Pts',(41.529598745462,-3.42346693059095,-8.92564167616314));
#62502=CARTESIAN_POINT('Ctrl Pts',(41.5193413489712,-3.42679793810188,-8.88711621115025));
#62503=CARTESIAN_POINT('Ctrl Pts',(41.5140465259434,-3.42844911613836,-8.86816771717611));
#62504=CARTESIAN_POINT('Ctrl Pts',(41.5004944834659,-3.4325165758252,-8.82186824289984));
#62505=CARTESIAN_POINT('Ctrl Pts',(41.4919814756648,-3.43494089104611,-8.79459607041152));
#62506=CARTESIAN_POINT('Ctrl Pts',(41.4591412638438,-3.44384763244424,-8.69562306084226));
#62507=CARTESIAN_POINT('Ctrl Pts',(41.4319208252656,-3.45042095062522,-8.62493767753455));
#62508=CARTESIAN_POINT('Ctrl Pts',(41.3225690784297,-3.47430592029768,-8.3765945579448));
#62509=CARTESIAN_POINT('Ctrl Pts',(41.2221811910276,-3.49211226025945,-8.20784244334291));
#62510=CARTESIAN_POINT('Ctrl Pts',(41.0704901137421,-3.51407344239522,-8.01177417749548));
#62511=CARTESIAN_POINT('Ctrl Pts',(41.0371595847783,-3.51865958328926,-7.97147774174081));
#62512=CARTESIAN_POINT('Ctrl Pts',(40.991287933232,-3.52463559765534,-7.91956261177279));
#62513=CARTESIAN_POINT('Ctrl Pts',(40.9799018011249,-3.52609315729551,-7.90694830225337));
#62514=CARTESIAN_POINT('Ctrl Pts',(40.9607575803957,-3.52850002302619,-7.88618573055764));
#62515=CARTESIAN_POINT('Ctrl Pts',(40.9530744781089,-3.52945453830076,-7.87796953166388));
#62516=CARTESIAN_POINT('Ctrl Pts',(40.9371506181777,-3.5314090222328,-7.86117846804725));
#62517=CARTESIAN_POINT('Ctrl Pts',(40.9289034376554,-3.53240848881143,-7.85261030779499));
#62518=CARTESIAN_POINT('Ctrl Pts',(40.9065836142058,-3.53508053544583,-7.82976337805812));
#62519=CARTESIAN_POINT('Ctrl Pts',(40.8923950237439,-3.5367446318517,-7.81559834997993));
#62520=CARTESIAN_POINT('Ctrl Pts',(40.8134010540452,-3.54583385263985,-7.73868343140284));
#62521=CARTESIAN_POINT('Ctrl Pts',(40.7452736921767,-3.55303569001522,-7.67943134571003));
#62522=CARTESIAN_POINT('Ctrl Pts',(40.5563197333229,-3.57191400639663,-7.53291225900167));
#62523=CARTESIAN_POINT('Ctrl Pts',(40.430457359045,-3.58343037638657,-7.45280509602672));
#62524=CARTESIAN_POINT('Ctrl Pts',(40.2276077006718,-3.60153969653769,-7.34873389792574));
#62525=CARTESIAN_POINT('Ctrl Pts',(40.1554872207818,-3.60789491485214,-7.31611938790898));
#62526=CARTESIAN_POINT('Ctrl Pts',(40.0556341662975,-3.61667773817527,-7.27676958468121));
#62527=CARTESIAN_POINT('Ctrl Pts',(40.0291918070063,-3.61900179903486,-7.26688338687173));
#62528=CARTESIAN_POINT('Ctrl Pts',(39.9839078222573,-3.62298282572918,-7.25085534501553));
#62529=CARTESIAN_POINT('Ctrl Pts',(39.9651526129791,-3.62463190463479,-7.24447663567411));
#62530=CARTESIAN_POINT('Ctrl Pts',(39.9292706200044,-3.62778861751208,-7.23276549992536));
#62531=CARTESIAN_POINT('Ctrl Pts',(39.9121587003754,-3.62929477889295,-7.22739155016619));
#62532=CARTESIAN_POINT('Ctrl Pts',(39.8718071370074,-3.63284913272507,-7.21521333208578));
#62533=CARTESIAN_POINT('Ctrl Pts',(39.8485221213355,-3.63490226679751,-7.20856777637765));
#62534=CARTESIAN_POINT('Ctrl Pts',(39.7632576842616,-3.64243068491006,-7.18561957829622));
#62535=CARTESIAN_POINT('Ctrl Pts',(39.7007394313206,-3.64797138817349,-7.17144558562971));
#62536=CARTESIAN_POINT('Ctrl Pts',(39.42778098935,-3.67227257358065,-7.12092852591869));
#62537=CARTESIAN_POINT('Ctrl Pts',(39.2135934214388,-3.69173420860046,-7.11020470266322));
#62538=CARTESIAN_POINT('Ctrl Pts',(38.9505265241898,-3.71510047949061,-7.13205896541279));
#62539=CARTESIAN_POINT('Ctrl Pts',(38.9003329110166,-3.71952800606988,-7.13782500768089));
#62540=CARTESIAN_POINT('Ctrl Pts',(38.8337349334314,-3.7253329289799,-7.14760962759376));
#62541=CARTESIAN_POINT('Ctrl Pts',(38.8171416878524,-3.72677343218744,-7.15022534880261));
#62542=CARTESIAN_POINT('Ctrl Pts',(38.7895212741357,-3.7291600898002,-7.15487640756048));
#62543=CARTESIAN_POINT('Ctrl Pts',(38.7784787424096,-3.73011127537068,-7.15681536185065));
#62544=CARTESIAN_POINT('Ctrl Pts',(38.7556902579504,-3.73206757209957,-7.16098123923111));
#62545=CARTESIAN_POINT('Ctrl Pts',(38.7439466901258,-3.73307210490017,-7.16321862868808));
#62546=CARTESIAN_POINT('Ctrl Pts',(38.7122700655126,-3.73577318129861,-7.16949875931177));
#62547=CARTESIAN_POINT('Ctrl Pts',(38.6923701824208,-3.7374609208376,-7.17370702881564));
#62548=CARTESIAN_POINT('Ctrl Pts',(38.5748486350137,-3.74738727405593,-7.2001212139168));
#62549=CARTESIAN_POINT('Ctrl Pts',(38.4786229707858,-3.7553492313819,-7.22815504570517));
#62550=CARTESIAN_POINT('Ctrl Pts',(38.2517901766377,-3.77433805778187,-7.30990982442521));
#62551=CARTESIAN_POINT('Ctrl Pts',(38.1236307310857,-3.78526474956412,-7.36927397041474));
#62552=CARTESIAN_POINT('Ctrl Pts',(37.9345660810682,-3.80259913358369,-7.47793534515349));
#62553=CARTESIAN_POINT('Ctrl Pts',(37.8696160611345,-3.80879682619454,-7.5195391838841));
#62554=CARTESIAN_POINT('Ctrl Pts',(37.7839579303474,-3.81739773492141,-7.58040192927074));
#62555=CARTESIAN_POINT('Ctrl Pts',(37.7614209034836,-3.81970316909896,-7.5970148210287));
#62556=CARTESIAN_POINT('Ctrl Pts',(37.7234746200217,-3.8236621004384,-7.62602223874005));
#62557=CARTESIAN_POINT('Ctrl Pts',(37.7079184488684,-3.82530792758393,-7.63822064582628));
#62558=CARTESIAN_POINT('Ctrl Pts',(37.6785056797047,-3.82846504808786,-7.66187596252465));
#62559=CARTESIAN_POINT('Ctrl Pts',(37.6646236602856,-3.82997492937238,-7.67329926726274));
#62560=CARTESIAN_POINT('Ctrl Pts',(37.628605194894,-3.83394588123036,-7.70362182102778));
#62561=CARTESIAN_POINT('Ctrl Pts',(37.6066821654292,-3.83641681969319,-7.72276854355615));
#62562=CARTESIAN_POINT('Ctrl Pts',(37.5248935003285,-3.84584778474228,-7.79685841203626));
#62563=CARTESIAN_POINT('Ctrl Pts',(37.467484766387,-3.85291415342636,-7.85441838956483));
#62564=CARTESIAN_POINT('Ctrl Pts',(37.2984397129121,-3.87519073521511,-8.04200962359141));
#62565=CARTESIAN_POINT('Ctrl Pts',(37.1976999510234,-3.89072343726094,-8.18113360016381));
#62566=CARTESIAN_POINT('Ctrl Pts',(37.0793087148385,-3.91195051591422,-8.38789393332895));
#62567=CARTESIAN_POINT('Ctrl Pts',(37.0484565784658,-3.91786258999103,-8.44740792370253));
#62568=CARTESIAN_POINT('Ctrl Pts',(37.0123700360756,-3.92523959975757,-8.52476764381252));
#62569=CARTESIAN_POINT('Ctrl Pts',(37.0048033112149,-3.9268159811864,-8.54148528931296));
#62570=CARTESIAN_POINT('Ctrl Pts',(36.9927957553069,-3.9293650671299,-8.56884351078396));
#62571=CARTESIAN_POINT('Ctrl Pts',(36.9882389937428,-3.93034424281718,-8.5794318752999));
#62572=CARTESIAN_POINT('Ctrl Pts',(36.9798112609118,-3.93217730941835,-8.59940936172578));
#62573=CARTESIAN_POINT('Ctrl Pts',(36.9759233210151,-3.9330322179764,-8.60879096011471));
#62574=CARTESIAN_POINT('Ctrl Pts',(36.9673099539575,-3.9349479872454,-8.62995296428858));
#62575=CARTESIAN_POINT('Ctrl Pts',(36.9626180963518,-3.93600691130961,-8.64174676749004));
#62576=CARTESIAN_POINT('Ctrl Pts',(36.958019684865,-3.93706097182542,-8.65357747851738));
#62577=CARTESIAN_POINT('Origin',(39.2,8.05522481984854,-9.525));
#62578=CARTESIAN_POINT('',(36.9580198925264,-5.47085833376936,-8.6535769442499));
#62579=CARTESIAN_POINT('',(36.9580195978366,-5.20345233470371,-8.65357770242256));
#62580=CARTESIAN_POINT('',(36.958019684865,8.05522481984854,-8.65357747851728));
#62581=CARTESIAN_POINT('',(36.7946209885083,-4.27538907091946,-9.5271273713836));
#62582=CARTESIAN_POINT('Ctrl Pts',(36.9580198925264,-5.47085833376936,-8.65357694424991));
#62583=CARTESIAN_POINT('Ctrl Pts',(36.9952595237356,-5.46277457665365,-8.55776755312851));
#62584=CARTESIAN_POINT('Ctrl Pts',(37.0386247691785,-5.45461778154573,-8.46438559009306));
#62585=CARTESIAN_POINT('Ctrl Pts',(37.1056162592304,-5.44325209572759,-8.34145253667686));
#62586=CARTESIAN_POINT('Ctrl Pts',(37.124108616556,-5.44021917316755,-8.30930985803724));
#62587=CARTESIAN_POINT('Ctrl Pts',(37.1546361376661,-5.43536238716226,-8.25897690494473));
#62588=CARTESIAN_POINT('Ctrl Pts',(37.1661890441466,-5.43355579258796,-8.24049981009226));
#62589=CARTESIAN_POINT('Ctrl Pts',(37.1873822729682,-5.43029518366753,-8.20760732089903));
#62590=CARTESIAN_POINT('Ctrl Pts',(37.1969306018763,-5.42884462881036,-8.19313418882667));
#62591=CARTESIAN_POINT('Ctrl Pts',(37.2198200133046,-5.42540924812751,-8.15924188951536));
#62592=CARTESIAN_POINT('Ctrl Pts',(37.2332913346773,-5.42341966520666,-8.13991338286865));
#62593=CARTESIAN_POINT('Ctrl Pts',(37.2745907558289,-5.41741263346382,-8.08247485069053));
#62594=CARTESIAN_POINT('Ctrl Pts',(37.3032568255642,-5.41336393379002,-8.04498505828743));
#62595=CARTESIAN_POINT('Ctrl Pts',(37.37324146227,-5.40374446103385,-7.95883314863532));
#62596=CARTESIAN_POINT('Ctrl Pts',(37.4154297141937,-5.39814367745725,-7.91092662909951));
#62597=CARTESIAN_POINT('Ctrl Pts',(37.5275699675128,-5.38374392300581,-7.7933632983783));
#62598=CARTESIAN_POINT('Ctrl Pts',(37.5999952297682,-5.37487933463865,-7.7262309232486));
#62599=CARTESIAN_POINT('Ctrl Pts',(37.7689183410649,-5.35526201927055,-7.58794683865562));
#62600=CARTESIAN_POINT('Ctrl Pts',(37.8670423877495,-5.3445326041192,-7.5191583393165));
#62601=CARTESIAN_POINT('Ctrl Pts',(37.987653042601,-5.33236951226657,-7.44738236265103));
#62602=CARTESIAN_POINT('Ctrl Pts',(38.0055520857263,-5.33058960973234,-7.43704059898525));
#62603=CARTESIAN_POINT('Ctrl Pts',(38.0340735883837,-5.32779534910148,-7.42104819530141));
#62604=CARTESIAN_POINT('Ctrl Pts',(38.0446083734972,-5.3267721658066,-7.4152446106881));
#62605=CARTESIAN_POINT('Ctrl Pts',(38.0650152825358,-5.32480789650844,-7.40420120493602));
#62606=CARTESIAN_POINT('Ctrl Pts',(38.0748810290998,-5.32386623922299,-7.39895081242697));
#62607=CARTESIAN_POINT('Ctrl Pts',(38.0994878188598,-5.32153648255053,-7.38607472921195));
#62608=CARTESIAN_POINT('Ctrl Pts',(38.1142722791227,-5.32015337640034,-7.37853226471361));
#62609=CARTESIAN_POINT('Ctrl Pts',(38.1727709749811,-5.3147412159474,-7.34944757971296));
#62610=CARTESIAN_POINT('Ctrl Pts',(38.2170612757656,-5.31077528231635,-7.32908101242674));
#62611=CARTESIAN_POINT('Ctrl Pts',(38.4767628571486,-5.28809341421452,-7.21909339367113));
#62612=CARTESIAN_POINT('Ctrl Pts',(38.7036803471764,-5.27039467113278,-7.1598443529106));
#62613=CARTESIAN_POINT('Ctrl Pts',(38.9880514015228,-5.24739370287977,-7.12839485222316));
#62614=CARTESIAN_POINT('Ctrl Pts',(39.0406820737562,-5.24310974667196,-7.12432187748376));
#62615=CARTESIAN_POINT('Ctrl Pts',(39.1179236018891,-5.23675638333033,-7.12089539046101));
#62616=CARTESIAN_POINT('Ctrl Pts',(39.1424609282994,-5.23472843251291,-7.12018302710016));
#62617=CARTESIAN_POINT('Ctrl Pts',(39.1862693323847,-5.23108797961879,-7.1195820243055));
#62618=CARTESIAN_POINT('Ctrl Pts',(39.205536581584,-5.22948005637867,-7.11954921694751));
#62619=CARTESIAN_POINT('Ctrl Pts',(39.2465870623378,-5.22603848844538,-7.11997250568584));
#62620=CARTESIAN_POINT('Ctrl Pts',(39.2683677092172,-5.22420299588322,-7.12049310832679));
#62621=CARTESIAN_POINT('Ctrl Pts',(39.3281588657947,-5.21913649896992,-7.12273525508449));
#62622=CARTESIAN_POINT('Ctrl Pts',(39.3661385737245,-5.21588725495576,-7.12506287165176));
#62623=CARTESIAN_POINT('Ctrl Pts',(39.5288318176334,-5.2018258112237,-7.13891382610556));
#62624=CARTESIAN_POINT('Ctrl Pts',(39.6525768907362,-5.19075529625799,-7.15926507153355));
#62625=CARTESIAN_POINT('Ctrl Pts',(39.9134242802172,-5.16670180232868,-7.22338184221743));
#62626=CARTESIAN_POINT('Ctrl Pts',(40.0493555975232,-5.15371784252894,-7.27000139908325));
#62627=CARTESIAN_POINT('Ctrl Pts',(40.2158631063779,-5.13767180753853,-7.34431447983958));
#62628=CARTESIAN_POINT('Ctrl Pts',(40.251010849335,-5.13427769872927,-7.36103514827078));
#62629=CARTESIAN_POINT('Ctrl Pts',(40.2997452158124,-5.12957566174219,-7.38568708782715));
#62630=CARTESIAN_POINT('Ctrl Pts',(40.3136812338339,-5.12823156394618,-7.39290867312603));
#62631=CARTESIAN_POINT('Ctrl Pts',(40.3372818086305,-5.12595736250596,-7.40543294322179));
#62632=CARTESIAN_POINT('Ctrl Pts',(40.3469821986928,-5.12502322657124,-7.41066646918281));
#62633=CARTESIAN_POINT('Ctrl Pts',(40.3675108099487,-5.12304799989191,-7.42192487603242));
#62634=CARTESIAN_POINT('Ctrl Pts',(40.3783289376723,-5.12200798176452,-7.4279669997374));
#62635=CARTESIAN_POINT('Ctrl Pts',(40.4085615156707,-5.11910257882854,-7.44516028503417));
#62636=CARTESIAN_POINT('Ctrl Pts',(40.4278683714197,-5.11724838786384,-7.45649968585288));
#62637=CARTESIAN_POINT('Ctrl Pts',(40.5679614385546,-5.1037811565107,-7.5414327513729));
#62638=CARTESIAN_POINT('Ctrl Pts',(40.6822254997664,-5.09271595196789,-7.6252952056509));
#62639=CARTESIAN_POINT('Ctrl Pts',(40.9029700060062,-5.06968870244783,-7.8194222510935));
#62640=CARTESIAN_POINT('Ctrl Pts',(41.0076219690653,-5.05776539702349,-7.93076135256273));
#62641=CARTESIAN_POINT('Ctrl Pts',(41.1242252562459,-5.04232431529775,-8.08117046470317));
#62642=CARTESIAN_POINT('Ctrl Pts',(41.1467125382999,-5.03922875957192,-8.11163644286042));
#62643=CARTESIAN_POINT('Ctrl Pts',(41.1810900905479,-5.03429495010918,-8.16058906959175));
#62644=CARTESIAN_POINT('Ctrl Pts',(41.1934627916882,-5.03247493448336,-8.17873064876448));
#62645=CARTESIAN_POINT('Ctrl Pts',(41.2151457588537,-5.02920285032391,-8.21147785722361));
#62646=CARTESIAN_POINT('Ctrl Pts',(41.224550052118,-5.02775439584812,-8.22601966829421));
#62647=CARTESIAN_POINT('Ctrl Pts',(41.2462528638732,-5.02434090257683,-8.26038684822782));
#62648=CARTESIAN_POINT('Ctrl Pts',(41.2584213571337,-5.02237129796934,-8.28029174476192));
#62649=CARTESIAN_POINT('Ctrl Pts',(41.2936888652565,-5.01649130197676,-8.33991320992022));
#62650=CARTESIAN_POINT('Ctrl Pts',(41.3159402087058,-5.01255161034865,-8.3801156471563));
#62651=CARTESIAN_POINT('Ctrl Pts',(41.4023414680293,-4.99625099492513,-8.54735258917987));
#62652=CARTESIAN_POINT('Ctrl Pts',(41.4562992913907,-4.98356939668883,-8.67930324580215));
#62653=CARTESIAN_POINT('Ctrl Pts',(41.5379166258791,-4.95872118621878,-8.94358269746234));
#62654=CARTESIAN_POINT('Ctrl Pts',(41.5667385457816,-4.94661212878722,-9.0750488606894));
#62655=CARTESIAN_POINT('Ctrl Pts',(41.5876930035189,-4.9327602439805,-9.232787721622));
#62656=CARTESIAN_POINT('Ctrl Pts',(41.5905743522289,-4.93062030754814,-9.25738029599692));
#62657=CARTESIAN_POINT('Ctrl Pts',(41.5943917267559,-4.92738289666199,-9.29497620979715));
#62658=CARTESIAN_POINT('Ctrl Pts',(41.5956025465786,-4.92627196598824,-9.30794897289716));
#62659=CARTESIAN_POINT('Ctrl Pts',(41.5976311401401,-4.92424373154533,-9.33177403046012));
#62660=CARTESIAN_POINT('Ctrl Pts',(41.5984807336038,-4.92332485333288,-9.34262253342965));
#62661=CARTESIAN_POINT('Ctrl Pts',(41.6002959705358,-4.92118467918,-9.36801401929874));
#62662=CARTESIAN_POINT('Ctrl Pts',(41.60120311266,-4.91996655436588,-9.38256057705231));
#62663=CARTESIAN_POINT('Ctrl Pts',(41.603792244002,-4.91591810771237,-9.43119050885038));
#62664=CARTESIAN_POINT('Ctrl Pts',(41.6048812931098,-4.91311724508659,-9.46530332553512));
#62665=CARTESIAN_POINT('Ctrl Pts',(41.6057899080726,-4.90617069602086,-9.55077329097243));
#62666=CARTESIAN_POINT('Ctrl Pts',(41.6046916533188,-4.90206119574809,-9.60212462268245));
#62667=CARTESIAN_POINT('Ctrl Pts',(41.5921734991456,-4.88345330538711,-9.83628950761009));
#62668=CARTESIAN_POINT('Ctrl Pts',(41.561542776729,-4.86937780776652,-10.0174565033301));
#62669=CARTESIAN_POINT('Ctrl Pts',(41.4927417446297,-4.84960001703423,-10.2553022208268));
#62670=CARTESIAN_POINT('Ctrl Pts',(41.4723552008387,-4.84439769625684,-10.3164584799679));
#62671=CARTESIAN_POINT('Ctrl Pts',(41.4409484308044,-4.83712957474374,-10.3994093952956));
#62672=CARTESIAN_POINT('Ctrl Pts',(41.4320144919434,-4.83513091732007,-10.4219687182125));
#62673=CARTESIAN_POINT('Ctrl Pts',(41.4158801731828,-4.83163405031406,-10.4609755415955));
#62674=CARTESIAN_POINT('Ctrl Pts',(41.4088339336347,-4.83014102781194,-10.4774850515771));
#62675=CARTESIAN_POINT('Ctrl Pts',(41.3936262066864,-4.82698755311929,-10.5120406464656));
#62676=CARTESIAN_POINT('Ctrl Pts',(41.3854253287289,-4.82532587034114,-10.5300677862163));
#62677=CARTESIAN_POINT('Ctrl Pts',(41.3650183403392,-4.82128117877937,-10.5734954156536));
#62678=CARTESIAN_POINT('Ctrl Pts',(41.3525869398724,-4.81889065602758,-10.5987859990957));
#62679=CARTESIAN_POINT('Ctrl Pts',(41.3037872305908,-4.80977035477408,-10.6938101943024));
#62680=CARTESIAN_POINT('Ctrl Pts',(41.2644550852237,-4.80294069384992,-10.7619560504568));
#62681=CARTESIAN_POINT('Ctrl Pts',(41.1422397220461,-4.78306905905059,-10.9515905637411));
#62682=CARTESIAN_POINT('Ctrl Pts',(41.0514678854628,-4.76980822234398,-11.0675674287773));
#62683=CARTESIAN_POINT('Ctrl Pts',(40.8872396364637,-4.74834047988365,-11.2418684736214));
#62684=CARTESIAN_POINT('Ctrl Pts',(40.8199436590886,-4.74010445566711,-11.3055060466609));
#62685=CARTESIAN_POINT('Ctrl Pts',(40.7337333010786,-4.73034423420925,-11.3780841019535));
#62686=CARTESIAN_POINT('Ctrl Pts',(40.7181638346249,-4.72861091387313,-11.3908609757667));
#62687=CARTESIAN_POINT('Ctrl Pts',(40.6931314230891,-4.72587265826061,-11.4108826648556));
#62688=CARTESIAN_POINT('Ctrl Pts',(40.6837724260908,-4.72485945997,-11.4182549429006));
#62689=CARTESIAN_POINT('Ctrl Pts',(40.6654777278209,-4.72289990739667,-11.432447066174));
#62690=CARTESIAN_POINT('Ctrl Pts',(40.6565484084893,-4.72195311119634,-11.4392742813818));
#62691=CARTESIAN_POINT('Ctrl Pts',(40.6340441756963,-4.719590040886,-11.4562320246187));
#62692=CARTESIAN_POINT('Ctrl Pts',(40.6204091094291,-4.71817908314182,-11.4662825253065));
#62693=CARTESIAN_POINT('Ctrl Pts',(40.5646861562773,-4.71249127626714,-11.5064548175052));
#62694=CARTESIAN_POINT('Ctrl Pts',(40.5217336504703,-4.70828601789915,-11.5353613484773));
#62695=CARTESIAN_POINT('Ctrl Pts',(40.3083314051909,-4.68806546734245,-11.6691790076998));
#62696=CARTESIAN_POINT('Ctrl Pts',(40.1261723761242,-4.67276760209691,-11.7539277827152));
#62697=CARTESIAN_POINT('Ctrl Pts',(39.8663984223725,-4.65105265712098,-11.8373689801358));
#62698=CARTESIAN_POINT('Ctrl Pts',(39.796223232101,-4.64520364297387,-11.8564487235966));
#62699=CARTESIAN_POINT('Ctrl Pts',(39.6977666161631,-4.63694724543407,-11.8784819443695));
#62700=CARTESIAN_POINT('Ctrl Pts',(39.6701304420351,-4.63462454706768,-11.8841579215339));
#62701=CARTESIAN_POINT('Ctrl Pts',(39.6231230971082,-4.63066117815669,-11.892953647643));
#62702=CARTESIAN_POINT('Ctrl Pts',(39.6038014291256,-4.62902852061959,-11.8963249441562));
#62703=CARTESIAN_POINT('Ctrl Pts',(39.5644161244845,-4.62569197211084,-11.9027016952473));
#62704=CARTESIAN_POINT('Ctrl Pts',(39.5443514265039,-4.62398769773444,-11.9056903419996));
#62705=CARTESIAN_POINT('Ctrl Pts',(39.4938340991769,-4.61968412972374,-11.9125629495981));
#62706=CARTESIAN_POINT('Ctrl Pts',(39.4633413708639,-4.61707488978525,-11.916118242847));
#62707=CARTESIAN_POINT('Ctrl Pts',(39.326923574192,-4.60534388986004,-11.9293828957315));
#62708=CARTESIAN_POINT('Ctrl Pts',(39.220508077027,-4.59603007609643,-11.9326418632413));
#62709=CARTESIAN_POINT('Ctrl Pts',(39.0231904332455,-4.57846898434809,-11.9256024560702));
#62710=CARTESIAN_POINT('Ctrl Pts',(38.932401549067,-4.57027540034288,-11.9171837952093));
#62711=CARTESIAN_POINT('Ctrl Pts',(38.7380049948022,-4.55261422397464,-11.8879515325751));
#62712=CARTESIAN_POINT('Ctrl Pts',(38.6348290555813,-4.54316669485518,-11.8654200449498));
#62713=CARTESIAN_POINT('Ctrl Pts',(38.5087643842345,-4.53173863575749,-11.8290630747263));
#62714=CARTESIAN_POINT('Ctrl Pts',(38.4841869540101,-4.52951655122016,-11.8215463577246));
#62715=CARTESIAN_POINT('Ctrl Pts',(38.4473048195213,-4.5261954216782,-11.8096167153856));
#62716=CARTESIAN_POINT('Ctrl Pts',(38.4349088871332,-4.52508152047773,-11.8054953813695));
#62717=CARTESIAN_POINT('Ctrl Pts',(38.4122528865247,-4.52305064552759,-11.797757301889));
#62718=CARTESIAN_POINT('Ctrl Pts',(38.4019832868098,-4.52213206422272,-11.7941717881331));
#62719=CARTESIAN_POINT('Ctrl Pts',(38.3780566166997,-4.51999617280301,-11.7856355331143));
#62720=CARTESIAN_POINT('Ctrl Pts',(38.3644195373108,-4.51878198989379,-11.780630568632));
#62721=CARTESIAN_POINT('Ctrl Pts',(38.3191782179908,-4.51476177276066,-11.7635598645217));
#62722=CARTESIAN_POINT('Ctrl Pts',(38.2877813708595,-4.51198464128137,-11.7509503132214));
#62723=CARTESIAN_POINT('Ctrl Pts',(38.2100120615735,-4.50511219978048,-11.7177946156581));
#62724=CARTESIAN_POINT('Ctrl Pts',(38.1640023430201,-4.50105209090411,-11.696435927314));
#62725=CARTESIAN_POINT('Ctrl Pts',(37.9546189820863,-4.48244504208671,-11.5910638029214));
#62726=CARTESIAN_POINT('Ctrl Pts',(37.8005388598102,-4.46833085895413,-11.4899694158746));
#62727=CARTESIAN_POINT('Ctrl Pts',(37.6096948390994,-4.44848469402268,-11.3308188746062));
#62728=CARTESIAN_POINT('Ctrl Pts',(37.5616287664727,-4.44325427505207,-11.2873253492816));
#62729=CARTESIAN_POINT('Ctrl Pts',(37.4980196805413,-4.43595253749243,-11.2249139679507));
#62730=CARTESIAN_POINT('Ctrl Pts',(37.480918748672,-4.43394917370213,-11.207618218903));
#62731=CARTESIAN_POINT('Ctrl Pts',(37.4516485250698,-4.4304464830367,-11.1771025294082));
#62732=CARTESIAN_POINT('Ctrl Pts',(37.4393593986464,-4.42895238789145,-11.163999781525));
#62733=CARTESIAN_POINT('Ctrl Pts',(37.4138420416727,-4.42579904189795,-11.1361748440464));
#62734=CARTESIAN_POINT('Ctrl Pts',(37.4006465266495,-4.42413858034533,-11.1214246484365));
#62735=CARTESIAN_POINT('Ctrl Pts',(37.3871262788759,-4.42240529599392,-11.1059308695077));
#62736=CARTESIAN_POINT('Ctrl Pts',(37.3866179060256,-4.42234007536982,-11.1053477225455));
#62737=CARTESIAN_POINT('Ctrl Pts',(37.3857177958894,-4.42222451311658,-11.1043142133637));
#62738=CARTESIAN_POINT('Ctrl Pts',(37.3853259444945,-4.42217417615615,-11.1038639501106));
#62739=CARTESIAN_POINT('Ctrl Pts',(37.3846231171822,-4.42208384040779,-11.1030557476077));
#62740=CARTESIAN_POINT('Ctrl Pts',(37.3843120793003,-4.4220438441541,-11.1026978620292));
#62741=CARTESIAN_POINT('Ctrl Pts',(37.3837486536747,-4.42197136088832,-11.1020491874478));
#62742=CARTESIAN_POINT('Ctrl Pts',(37.383496229809,-4.42193887535067,-11.1017584296713));
#62743=CARTESIAN_POINT('Ctrl Pts',(37.3820164477946,-4.42174836615,-11.1000530961666));
#62744=CARTESIAN_POINT('Ctrl Pts',(37.3807906758085,-4.42159027790435,-11.0986371521305));
#62745=CARTESIAN_POINT('Ctrl Pts',(37.3783399345589,-4.42127364151454,-11.0957995009524));
#62746=CARTESIAN_POINT('Ctrl Pts',(37.377114972979,-4.42111509320416,-11.0943777889452));
#62747=CARTESIAN_POINT('Ctrl Pts',(37.3746449761036,-4.42079482551441,-11.0915042735329));
#62748=CARTESIAN_POINT('Ctrl Pts',(37.3734000061919,-4.42063310363375,-11.0900524160025));
#62749=CARTESIAN_POINT('Ctrl Pts',(37.3708695737756,-4.42030379758371,-11.0870943471385));
#62750=CARTESIAN_POINT('Ctrl Pts',(37.3695842372668,-4.42013620848173,-11.0855880305159));
#62751=CARTESIAN_POINT('Ctrl Pts',(37.3669519858763,-4.41979234805102,-11.082495506436));
#62752=CARTESIAN_POINT('Ctrl Pts',(37.3656052668289,-4.41961606901278,-11.0809091353632));
#62753=CARTESIAN_POINT('Ctrl Pts',(37.3390630774199,-4.4161348498314,-11.0495613366961));
#62754=CARTESIAN_POINT('Ctrl Pts',(37.314594590791,-4.41280120192612,-11.0191952891368));
#62755=CARTESIAN_POINT('Ctrl Pts',(37.2602283217251,-4.40509534935517,-10.9482628167489));
#62756=CARTESIAN_POINT('Ctrl Pts',(37.2308465062441,-4.40070602922078,-10.9073259314246));
#62757=CARTESIAN_POINT('Ctrl Pts',(37.1298366205566,-4.38477112304315,-10.7568301094805));
#62758=CARTESIAN_POINT('Ctrl Pts',(37.0658975076619,-4.37300947777917,-10.6423993981754));
#62759=CARTESIAN_POINT('Ctrl Pts',(36.968135221261,-4.35184891748952,-10.4281019737769));
#62760=CARTESIAN_POINT('Ctrl Pts',(36.9309424719433,-4.34247395595559,-10.3301063844806));
#62761=CARTESIAN_POINT('Ctrl Pts',(36.8927321453947,-4.33111874617036,-10.2054602809163));
#62762=CARTESIAN_POINT('Ctrl Pts',(36.8856052751858,-4.32890040588748,-10.1808112266383));
#62763=CARTESIAN_POINT('Ctrl Pts',(36.8754490160686,-4.32558369539335,-10.1434545867036));
#62764=CARTESIAN_POINT('Ctrl Pts',(36.8721267631786,-4.3244705253407,-10.1308296546545));
#62765=CARTESIAN_POINT('Ctrl Pts',(36.8662246097815,-4.32244030236372,-10.1076351500212));
#62766=CARTESIAN_POINT('Ctrl Pts',(36.863613491522,-4.32152165002608,-10.0970746310514));
#62767=CARTESIAN_POINT('Ctrl Pts',(36.8585622955632,-4.31970234639919,-10.0760337452753));
#62768=CARTESIAN_POINT('Ctrl Pts',(36.8561208120645,-4.31880161382848,-10.0655544173153));
#62769=CARTESIAN_POINT('Ctrl Pts',(36.8505669167431,-4.31670032244282,-10.0409706731652));
#62770=CARTESIAN_POINT('Ctrl Pts',(36.847511012862,-4.31550271040201,-10.0268537072932));
#62771=CARTESIAN_POINT('Ctrl Pts',(36.8376137773697,-4.31147540321102,-9.97905451557714));
#62772=CARTESIAN_POINT('Ctrl Pts',(36.8313668298997,-4.30867371131835,-9.94525159629413));
#62773=CARTESIAN_POINT('Ctrl Pts',(36.805178275617,-4.29550206162921,-9.78430988895812));
#62774=CARTESIAN_POINT('Ctrl Pts',(36.79473479356,-4.28547290397762,-9.65583208521157));
#62775=CARTESIAN_POINT('Ctrl Pts',(36.7946209411353,-4.27538918813332,-9.52712780995419));
#62776=CARTESIAN_POINT('Ctrl Pts',(36.7946209407417,-4.27538915327001,-9.52712736497368));
#62777=CARTESIAN_POINT('Ctrl Pts',(36.7944991403118,-4.2645992395797,-9.38940948057675));
#62778=CARTESIAN_POINT('Ctrl Pts',(36.8062043998384,-4.25377919108456,-9.25194856682721));
#62779=CARTESIAN_POINT('Ctrl Pts',(36.8342255556644,-4.24039179038781,-9.08944994601524));
#62780=CARTESIAN_POINT('Ctrl Pts',(36.8393010269769,-4.23817159305936,-9.06273079798787));
#62781=CARTESIAN_POINT('Ctrl Pts',(36.8488385541642,-4.23431700667048,-9.01678537028102));
#62782=CARTESIAN_POINT('Ctrl Pts',(36.8530863144503,-4.23268922636811,-8.99751695765488));
#62783=CARTESIAN_POINT('Ctrl Pts',(36.8620704505594,-4.22941312977994,-8.9590226425274));
#62784=CARTESIAN_POINT('Ctrl Pts',(36.8668081349445,-4.22776489093062,-8.93979865086665));
#62785=CARTESIAN_POINT('Ctrl Pts',(36.8768942240024,-4.22440746598798,-8.90094357887893));
#62786=CARTESIAN_POINT('Ctrl Pts',(36.882255469653,-4.22269799330744,-8.88131754658095));
#62787=CARTESIAN_POINT('Ctrl Pts',(36.8964109360524,-4.21836377810118,-8.83196968524037));
#62788=CARTESIAN_POINT('Ctrl Pts',(36.9055316201117,-4.21572879034417,-8.80234638053156));
#62789=CARTESIAN_POINT('Ctrl Pts',(36.928440781962,-4.20945597332542,-8.73275060355609));
#62790=CARTESIAN_POINT('Ctrl Pts',(36.9427123752434,-4.20580426847111,-8.69295984675209));
#62791=CARTESIAN_POINT('Ctrl Pts',(36.9580197210495,-4.20212274557561,-8.6535773854226));
#62792=CARTESIAN_POINT('Ctrl Pts',(36.958019684865,-3.93706097182542,-8.65357747851738));
#62793=CARTESIAN_POINT('Ctrl Pts',(36.9564218065497,-3.93742724188324,-8.65768847133716));
#62794=CARTESIAN_POINT('Ctrl Pts',(36.9548352114531,-3.93779292469071,-8.66180392061865));
#62795=CARTESIAN_POINT('Ctrl Pts',(36.9356569182194,-3.94223798500041,-8.71196086723292));
#62796=CARTESIAN_POINT('Ctrl Pts',(36.9194713198563,-3.94624560074252,-8.75853270417446));
#62797=CARTESIAN_POINT('Ctrl Pts',(36.864362832756,-3.96105178130554,-8.93435194880606));
#62798=CARTESIAN_POINT('Ctrl Pts',(36.8349046012429,-3.97153258611843,-9.06631020610886));
#62799=CARTESIAN_POINT('Ctrl Pts',(36.8020319549446,-3.99062091621821,-9.30741523895724));
#62800=CARTESIAN_POINT('Ctrl Pts',(36.7946666042369,-3.99916619663588,-9.41563278385659));
#62801=CARTESIAN_POINT('Ctrl Pts',(36.7946011773878,-4.01150833552565,-9.56844855980404));
#62802=CARTESIAN_POINT('Ctrl Pts',(36.79581582193,-4.01513154800105,-9.61291598123295));
#62803=CARTESIAN_POINT('Ctrl Pts',(36.7995453838213,-4.02071170174965,-9.68061040585967));
#62804=CARTESIAN_POINT('Ctrl Pts',(36.8011670843105,-4.02264131717661,-9.70387852562828));
#62805=CARTESIAN_POINT('Ctrl Pts',(36.8047387400157,-4.02617713335041,-9.7462338917954));
#62806=CARTESIAN_POINT('Ctrl Pts',(36.8065792194015,-4.02777981633833,-9.76532865064845));
#62807=CARTESIAN_POINT('Ctrl Pts',(36.8110939448816,-4.03129326098282,-9.80694911871452));
#62808=CARTESIAN_POINT('Ctrl Pts',(36.813858820439,-4.03320669280442,-9.82946287332989));
#62809=CARTESIAN_POINT('Ctrl Pts',(36.8227271522041,-4.03873986384661,-9.89410526243208));
#62810=CARTESIAN_POINT('Ctrl Pts',(36.829630747841,-4.04238389676091,-9.93611312735005));
#62811=CARTESIAN_POINT('Ctrl Pts',(36.8614024510447,-4.05696273351156,-10.1018316111671));
#62812=CARTESIAN_POINT('Ctrl Pts',(36.8948696593243,-4.06814853415373,-10.2236684158856));
#62813=CARTESIAN_POINT('Ctrl Pts',(36.9918764428223,-4.09374584844926,-10.492181194954));
#62814=CARTESIAN_POINT('Ctrl Pts',(37.0607889311303,-4.10817963761743,-10.6363206319144));
#62815=CARTESIAN_POINT('Ctrl Pts',(37.1552599489578,-4.12400390981974,-10.7920472700935));
#62816=CARTESIAN_POINT('Ctrl Pts',(37.1673374996701,-4.1259674127758,-10.8113335241509));
#62817=CARTESIAN_POINT('Ctrl Pts',(37.186524970979,-4.12899317869822,-10.841028104447));
#62818=CARTESIAN_POINT('Ctrl Pts',(37.193445637932,-4.13006646650255,-10.8515561723586));
#62819=CARTESIAN_POINT('Ctrl Pts',(37.2065400300636,-4.13206314469821,-10.8711390617977));
#62820=CARTESIAN_POINT('Ctrl Pts',(37.2126931040418,-4.13298768399567,-10.8802063809301));
#62821=CARTESIAN_POINT('Ctrl Pts',(37.2275675907473,-4.1351907750014,-10.9018066099371));
#62822=CARTESIAN_POINT('Ctrl Pts',(37.2363467351261,-4.13646552409189,-10.9142990834695));
#62823=CARTESIAN_POINT('Ctrl Pts',(37.2677527313933,-4.14094014904069,-10.9580964062999));
#62824=CARTESIAN_POINT('Ctrl Pts',(37.291015541257,-4.14410148039958,-10.9889411361014));
#62825=CARTESIAN_POINT('Ctrl Pts',(37.3532668438202,-4.15221677799298,-11.0674726166837));
#62826=CARTESIAN_POINT('Ctrl Pts',(37.3933628543573,-4.15711703858195,-11.1142478033346));
#62827=CARTESIAN_POINT('Ctrl Pts',(37.5749194330834,-4.17821304081308,-11.3102840389316));
#62828=CARTESIAN_POINT('Ctrl Pts',(37.7333766102004,-4.19401602400693,-11.4425862530464));
#62829=CARTESIAN_POINT('Ctrl Pts',(37.9397928596778,-4.21385915489795,-11.5742118208705));
#62830=CARTESIAN_POINT('Ctrl Pts',(37.9733701704987,-4.21706308320526,-11.5944854528791));
#62831=CARTESIAN_POINT('Ctrl Pts',(38.0267432277663,-4.22212980257689,-11.6249562509932));
#62832=CARTESIAN_POINT('Ctrl Pts',(38.0462115668302,-4.22397262192054,-11.6357154930785));
#62833=CARTESIAN_POINT('Ctrl Pts',(38.0827640763653,-4.22742462980712,-11.6552595545121));
#62834=CARTESIAN_POINT('Ctrl Pts',(38.0998098367328,-4.22903126480804,-11.6641127688518));
#62835=CARTESIAN_POINT('Ctrl Pts',(38.1382644873064,-4.2326499394892,-11.6835041069582));
#62836=CARTESIAN_POINT('Ctrl Pts',(38.1597275238272,-4.23466567556183,-11.6939295437685));
#62837=CARTESIAN_POINT('Ctrl Pts',(38.2256085560158,-4.2408433961207,-11.7247277326397));
#62838=CARTESIAN_POINT('Ctrl Pts',(38.2704924972094,-4.245039358591,-11.7440664361145));
#62839=CARTESIAN_POINT('Ctrl Pts',(38.3498379074304,-4.25244119461422,-11.7754236517792));
#62840=CARTESIAN_POINT('Ctrl Pts',(38.3840434342024,-4.25562704870653,-11.7880503317101));
#62841=CARTESIAN_POINT('Ctrl Pts',(38.5448530055747,-4.27058084470239,-11.8432921579502));
#62842=CARTESIAN_POINT('Ctrl Pts',(38.6745687372117,-4.28259348784099,-11.8760871752182));
#62843=CARTESIAN_POINT('Ctrl Pts',(38.9061979690985,-4.30368191199174,-11.9145153563092));
#62844=CARTESIAN_POINT('Ctrl Pts',(39.0070345721715,-4.31273991162085,-11.924765014113));
#62845=CARTESIAN_POINT('Ctrl Pts',(39.1334064398001,-4.32375321629474,-11.9295900213183));
#62846=CARTESIAN_POINT('Ctrl Pts',(39.1586009642749,-4.3259319174706,-11.9301557423096));
#62847=CARTESIAN_POINT('Ctrl Pts',(39.1969194403864,-4.32921541775753,-11.9304138002995));
#62848=CARTESIAN_POINT('Ctrl Pts',(39.2100386630119,-4.33033423550841,-11.9303948304914));
#62849=CARTESIAN_POINT('Ctrl Pts',(39.2340252845103,-4.33236927472427,-11.9301638911338));
#62850=CARTESIAN_POINT('Ctrl Pts',(39.2448919407255,-4.33328716068351,-11.9299856107112));
#62851=CARTESIAN_POINT('Ctrl Pts',(39.2701931227031,-4.33541522225661,-11.9293989605366));
#62852=CARTESIAN_POINT('Ctrl Pts',(39.2846257302597,-4.33662234756427,-11.9289342657371));
#62853=CARTESIAN_POINT('Ctrl Pts',(39.3323416217746,-4.34059345891391,-11.9269676514473));
#62854=CARTESIAN_POINT('Ctrl Pts',(39.3655998126963,-4.34332949194643,-11.9249041516008));
#62855=CARTESIAN_POINT('Ctrl Pts',(39.4482560315581,-4.35007460462585,-11.9180490863296));
#62856=CARTESIAN_POINT('Ctrl Pts',(39.4975703308239,-4.35405013662522,-11.9124186127147));
#62857=CARTESIAN_POINT('Ctrl Pts',(39.7739691187715,-4.37623661433595,-11.8721619495239));
#62858=CARTESIAN_POINT('Ctrl Pts',(39.9953332907939,-4.39376263930941,-11.8066782966727));
#62859=CARTESIAN_POINT('Ctrl Pts',(40.2377413160252,-4.41542617959691,-11.6953271627589));
#62860=CARTESIAN_POINT('Ctrl Pts',(40.2710620332021,-4.4184592724644,-11.679078192295));
#62861=CARTESIAN_POINT('Ctrl Pts',(40.3231685859487,-4.42329978124538,-11.6521603460662));
#62862=CARTESIAN_POINT('Ctrl Pts',(40.34221001533,-4.42508975479324,-11.6419967001463));
#62863=CARTESIAN_POINT('Ctrl Pts',(40.3780117755566,-4.42849720944141,-11.6222633582596));
#62864=CARTESIAN_POINT('Ctrl Pts',(40.3947988349424,-4.43011275915449,-11.6127454430817));
#62865=CARTESIAN_POINT('Ctrl Pts',(40.4329614073952,-4.43382775217469,-11.5904970419608));
#62866=CARTESIAN_POINT('Ctrl Pts',(40.4542571842657,-4.43593176825608,-11.5776350572525));
#62867=CARTESIAN_POINT('Ctrl Pts',(40.5217924048129,-4.44270704139511,-11.535402519815));
#62868=CARTESIAN_POINT('Ctrl Pts',(40.5672260931139,-4.44742270445586,-11.5047841381315));
#62869=CARTESIAN_POINT('Ctrl Pts',(40.6756056243339,-4.45907604189103,-11.4262351695994));
#62870=CARTESIAN_POINT('Ctrl Pts',(40.7373053370498,-4.46606497161795,-11.3767011093379));
#62871=CARTESIAN_POINT('Ctrl Pts',(40.9135520980542,-4.4870885101725,-11.2203176539786));
#62872=CARTESIAN_POINT('Ctrl Pts',(41.0202307834518,-4.50129192912323,-11.1052288843261));
#62873=CARTESIAN_POINT('Ctrl Pts',(41.1413958517441,-4.51896084423093,-10.9458244190945));
#62874=CARTESIAN_POINT('Ctrl Pts',(41.1668721583249,-4.52277885190597,-10.9103427267695));
#62875=CARTESIAN_POINT('Ctrl Pts',(41.2005591177537,-4.52795503193203,-10.8606214054747));
#62876=CARTESIAN_POINT('Ctrl Pts',(41.2096095654249,-4.52935925031895,-10.8469647359009));
#62877=CARTESIAN_POINT('Ctrl Pts',(41.224516117627,-4.53169380532353,-10.8239645783502));
#62878=CARTESIAN_POINT('Ctrl Pts',(41.2304486495963,-4.53262887763718,-10.8146715823945));
#62879=CARTESIAN_POINT('Ctrl Pts',(41.2427370307949,-4.53457793323102,-10.7951274843059));
#62880=CARTESIAN_POINT('Ctrl Pts',(41.2490800114608,-4.53559111150193,-10.7848688541453));
#62881=CARTESIAN_POINT('Ctrl Pts',(41.2661696795052,-4.53834182694285,-10.7567588763515));
#62882=CARTESIAN_POINT('Ctrl Pts',(41.2767623626784,-4.54007000108603,-10.7388143404077));
#62883=CARTESIAN_POINT('Ctrl Pts',(41.3523452624266,-4.55259195563401,-10.6068863960687));
#62884=CARTESIAN_POINT('Ctrl Pts',(41.4081562780743,-4.56290474507926,-10.4878736187829));
#62885=CARTESIAN_POINT('Ctrl Pts',(41.5121044935809,-4.58623992287144,-10.2089091159635));
#62886=CARTESIAN_POINT('Ctrl Pts',(41.5538707783974,-4.59920569414261,-10.0473430206926));
#62887=CARTESIAN_POINT('Ctrl Pts',(41.5841763996209,-4.61574373888441,-9.84585705659293));
#62888=CARTESIAN_POINT('Ctrl Pts',(41.5888682028853,-4.61879654446586,-9.80882171248753));
#62889=CARTESIAN_POINT('Ctrl Pts',(41.5949362017491,-4.62367751744164,-9.74996794998442));
#62890=CARTESIAN_POINT('Ctrl Pts',(41.5968801361547,-4.62548810816445,-9.72821303334206));
#62891=CARTESIAN_POINT('Ctrl Pts',(41.5998344743201,-4.62875167249049,-9.68915746990398));
#62892=CARTESIAN_POINT('Ctrl Pts',(41.6009546848394,-4.63020113705926,-9.67186642585032));
#62893=CARTESIAN_POINT('Ctrl Pts',(41.6031524725772,-4.6336282191167,-9.63112371557899));
#62894=CARTESIAN_POINT('Ctrl Pts',(41.6040736937177,-4.63561052642731,-9.60766583750798));
#62895=CARTESIAN_POINT('Ctrl Pts',(41.6058019721924,-4.64157261216605,-9.53746364425242));
#62896=CARTESIAN_POINT('Ctrl Pts',(41.6055897198507,-4.64558295179576,-9.49070826565345));
#62897=CARTESIAN_POINT('Ctrl Pts',(41.6018940251512,-4.65509067382821,-9.38103369510855));
#62898=CARTESIAN_POINT('Ctrl Pts',(41.5973003456823,-4.66061709172731,-9.31818874583957));
#62899=CARTESIAN_POINT('Ctrl Pts',(41.5790538141281,-4.67505029371285,-9.15629572517049));
#62900=CARTESIAN_POINT('Ctrl Pts',(41.5616841746118,-4.68402822547005,-9.05778999729089));
#62901=CARTESIAN_POINT('Ctrl Pts',(41.5101155328111,-4.70377987384432,-8.84412573069977));
#62902=CARTESIAN_POINT('Ctrl Pts',(41.4733146077423,-4.71453011837482,-8.72984507182877));
#62903=CARTESIAN_POINT('Ctrl Pts',(41.4203489949477,-4.72671357120512,-8.59961851977961));
#62904=CARTESIAN_POINT('Ctrl Pts',(41.4123112988146,-4.72849422096922,-8.58056400502867));
#62905=CARTESIAN_POINT('Ctrl Pts',(41.3992114667894,-4.73128922753371,-8.5505942740487));
#62906=CARTESIAN_POINT('Ctrl Pts',(41.3943117289174,-4.73231241989635,-8.53960989943921));
#62907=CARTESIAN_POINT('Ctrl Pts',(41.3847024096533,-4.73427633109521,-8.51849459985349));
#62908=CARTESIAN_POINT('Ctrl Pts',(41.3800043490762,-4.7352176243638,-8.50835906737563));
#62909=CARTESIAN_POINT('Ctrl Pts',(41.3681573826961,-4.73754590696035,-8.48326035263044));
#62910=CARTESIAN_POINT('Ctrl Pts',(41.3609238339825,-4.73892791427912,-8.46833725327713));
#62911=CARTESIAN_POINT('Ctrl Pts',(41.331869824326,-4.74433121611485,-8.40994411295681));
#62912=CARTESIAN_POINT('Ctrl Pts',(41.3088855035372,-4.74828964392965,-8.36706155623103));
#62913=CARTESIAN_POINT('Ctrl Pts',(41.1672900725772,-4.77111524213714,-8.12110519626352));
#62914=CARTESIAN_POINT('Ctrl Pts',(41.0207138722834,-4.78894811431386,-7.93560725214195));
#62915=CARTESIAN_POINT('Ctrl Pts',(40.811969595921,-4.81202067723423,-7.7389229671705));
#62916=CARTESIAN_POINT('Ctrl Pts',(40.7732758317323,-4.81621252134748,-7.70474739205083));
#62917=CARTESIAN_POINT('Ctrl Pts',(40.7147596743687,-4.82245539356396,-7.65632433428605));
#62918=CARTESIAN_POINT('Ctrl Pts',(40.6957700971007,-4.82446706209007,-7.64108987935604));
#62919=CARTESIAN_POINT('Ctrl Pts',(40.6613613997418,-4.82808942084773,-7.61433358509546));
#62920=CARTESIAN_POINT('Ctrl Pts',(40.6460287923643,-4.82969570512639,-7.60270346307054));
#62921=CARTESIAN_POINT('Ctrl Pts',(40.612948656071,-4.83314584986249,-7.57823117003711));
#62922=CARTESIAN_POINT('Ctrl Pts',(40.5951620646422,-4.83499167404586,-7.56544506908707));
#62923=CARTESIAN_POINT('Ctrl Pts',(40.5455164226411,-4.84012022623625,-7.53077526693075));
#62924=CARTESIAN_POINT('Ctrl Pts',(40.5133022234595,-4.84342195938408,-7.50941481727415));
#62925=CARTESIAN_POINT('Ctrl Pts',(40.3704926554486,-4.85795708181521,-7.41959844697226));
#62926=CARTESIAN_POINT('Ctrl Pts',(40.2549807598847,-4.86947029226611,-7.35941154830786));
#62927=CARTESIAN_POINT('Ctrl Pts',(39.9934437539558,-4.89491209466127,-7.24904518125998));
#62928=CARTESIAN_POINT('Ctrl Pts',(39.846276212584,-4.90884573141768,-7.202962795462));
#62929=CARTESIAN_POINT('Ctrl Pts',(39.6681453080884,-4.92473587916687,-7.16544787544363));
#62930=CARTESIAN_POINT('Ctrl Pts',(39.6404824135889,-4.92717564696432,-7.16012754913506));
#62931=CARTESIAN_POINT('Ctrl Pts',(39.5993983104324,-4.93075220465543,-7.152971948227));
#62932=CARTESIAN_POINT('Ctrl Pts',(39.586046079463,-4.93190728298411,-7.15076232438096));
#62933=CARTESIAN_POINT('Ctrl Pts',(39.5619653031494,-4.93397654154886,-7.14698578818419));
#62934=CARTESIAN_POINT('Ctrl Pts',(39.5512440914666,-4.93489278253082,-7.14537858598069));
#62935=CARTESIAN_POINT('Ctrl Pts',(39.5267198560311,-4.93697733938558,-7.1418715555689));
#62936=CARTESIAN_POINT('Ctrl Pts',(39.5129106971364,-4.93814306941781,-7.14001908354762));
#62937=CARTESIAN_POINT('Ctrl Pts',(39.4689617319374,-4.941829873964,-7.13451171623176));
#62938=CARTESIAN_POINT('Ctrl Pts',(39.4387668859735,-4.94432819959118,-7.13130718789372));
#62939=CARTESIAN_POINT('Ctrl Pts',(39.365146423466,-4.95035361701698,-7.12490106727131));
#62940=CARTESIAN_POINT('Ctrl Pts',(39.3216778229234,-4.95385571865512,-7.1223049965251));
#62941=CARTESIAN_POINT('Ctrl Pts',(39.1245985597038,-4.96958066501487,-7.11589777760175));
#62942=CARTESIAN_POINT('Ctrl Pts',(38.970905686005,-4.98144414186177,-7.12562927223598));
#62943=CARTESIAN_POINT('Ctrl Pts',(38.7217970732718,-5.00135344755902,-7.16557146069848));
#62944=CARTESIAN_POINT('Ctrl Pts',(38.6254742698223,-5.00922042062027,-7.18715970774608));
#62945=CARTESIAN_POINT('Ctrl Pts',(38.501276458948,-5.01977662080017,-7.22313545468633));
#62946=CARTESIAN_POINT('Ctrl Pts',(38.4719634357677,-5.02229860799912,-7.23223800610766));
#62947=CARTESIAN_POINT('Ctrl Pts',(38.4235834731627,-5.02651704906705,-7.24828270131149));
#62948=CARTESIAN_POINT('Ctrl Pts',(38.4044151946945,-5.02820321309416,-7.25490990348813));
#62949=CARTESIAN_POINT('Ctrl Pts',(38.3666689297738,-5.03155443799323,-7.26849700187981));
#62950=CARTESIAN_POINT('Ctrl Pts',(38.348088689092,-5.03321902216912,-7.27544592838382));
#62951=CARTESIAN_POINT('Ctrl Pts',(38.3031430452642,-5.03728355112441,-7.29289207140762));
#62952=CARTESIAN_POINT('Ctrl Pts',(38.2768740375155,-5.0396911963857,-7.30362733621964));
#62953=CARTESIAN_POINT('Ctrl Pts',(38.1768930945831,-5.04898322311293,-7.34656586147726));
#62954=CARTESIAN_POINT('Ctrl Pts',(38.1046323412267,-5.05597253412571,-7.38199052181724));
#62955=CARTESIAN_POINT('Ctrl Pts',(37.8991843539477,-5.0766757088816,-7.49581594495521));
#62956=CARTESIAN_POINT('Ctrl Pts',(37.7716121605515,-5.09063484665905,-7.58350344839258));
#62957=CARTESIAN_POINT('Ctrl Pts',(37.5893836504235,-5.11192937486515,-7.73649729246795));
#62958=CARTESIAN_POINT('Ctrl Pts',(37.5282573426784,-5.1193421076161,-7.7934957793787));
#62959=CARTESIAN_POINT('Ctrl Pts',(37.456478262848,-5.12828472555001,-7.86778075301754));
#62960=CARTESIAN_POINT('Ctrl Pts',(37.4429177273388,-5.12998541335302,-7.88216536275201));
#62961=CARTESIAN_POINT('Ctrl Pts',(37.4215261642184,-5.13268424704774,-7.9054248249398));
#62962=CARTESIAN_POINT('Ctrl Pts',(37.4135810143153,-5.13369027154547,-7.9141926997654));
#62963=CARTESIAN_POINT('Ctrl Pts',(37.3981832076199,-5.13564653529233,-7.9314390199572));
#62964=CARTESIAN_POINT('Ctrl Pts',(37.3907250121288,-5.13659712412946,-7.9399118701817));
#62965=CARTESIAN_POINT('Ctrl Pts',(37.3831467253694,-5.13756653716907,-7.94864433006089));
#62966=CARTESIAN_POINT('Ctrl Pts',(37.3829669224932,-5.13758953956821,-7.94885158854521));
#62967=CARTESIAN_POINT('Ctrl Pts',(37.382607045393,-5.13763558319315,-7.94926656171896));
#62968=CARTESIAN_POINT('Ctrl Pts',(37.3824269712959,-5.13765862441054,-7.94947427653505));
#62969=CARTESIAN_POINT('Ctrl Pts',(37.3820663591634,-5.13770477035167,-7.94989038542191));
#62970=CARTESIAN_POINT('Ctrl Pts',(37.3818858213655,-5.1377278750573,-7.9500987796467));
#62971=CARTESIAN_POINT('Ctrl Pts',(37.381524090612,-5.13777417249707,-7.95051646943799));
#62972=CARTESIAN_POINT('Ctrl Pts',(37.3813428979343,-5.1377973652125,-7.95072576526779));
#62973=CARTESIAN_POINT('Ctrl Pts',(37.3809796666208,-5.13784386315861,-7.95114548049473));
#62974=CARTESIAN_POINT('Ctrl Pts',(37.38079762837,-5.13786716836146,-7.95135590018896));
#62975=CARTESIAN_POINT('Ctrl Pts',(37.3804325149379,-5.13791391580972,-7.95177808619828));
#62976=CARTESIAN_POINT('Ctrl Pts',(37.3802494402194,-5.13793735802204,-7.95198985288091));
#62977=CARTESIAN_POINT('Ctrl Pts',(37.3798820620862,-5.13798440413703,-7.95241495747763));
#62978=CARTESIAN_POINT('Ctrl Pts',(37.3796977591661,-5.13800800800739,-7.95262829588671));
#62979=CARTESIAN_POINT('Ctrl Pts',(37.3793277311396,-5.13805540232662,-7.95305677119684));
#62980=CARTESIAN_POINT('Ctrl Pts',(37.3791420066629,-5.13807919273088,-7.95327190860566));
#62981=CARTESIAN_POINT('Ctrl Pts',(37.37876893984,-5.1381269853071,-7.9537042123882));
#62982=CARTESIAN_POINT('Ctrl Pts',(37.378581598213,-5.13815098742822,-7.95392137934151));
#62983=CARTESIAN_POINT('Ctrl Pts',(37.378205098543,-5.13819922901521,-7.95435797670007));
#62984=CARTESIAN_POINT('Ctrl Pts',(37.3780159412777,-5.13822346842822,-7.95457740779998));
#62985=CARTESIAN_POINT('Ctrl Pts',(37.3776356081895,-5.13827221065856,-7.95501877283076));
#62986=CARTESIAN_POINT('Ctrl Pts',(37.3774444332266,-5.13829671341825,-7.95524070755223));
#62987=CARTESIAN_POINT('Ctrl Pts',(37.3770598582648,-5.13834600898041,-7.95568732499344));
#62988=CARTESIAN_POINT('Ctrl Pts',(37.376866459262,-5.13837080171387,-7.95591200854696));
#62989=CARTESIAN_POINT('Ctrl Pts',(37.3764772248428,-5.13842070451432,-7.95636437530127));
#62990=CARTESIAN_POINT('Ctrl Pts',(37.3762813905294,-5.13844581450502,-7.95659205942394));
#62991=CARTESIAN_POINT('Ctrl Pts',(37.3758870684821,-5.13849637985814,-7.95705068634192));
#62992=CARTESIAN_POINT('Ctrl Pts',(37.3756885819548,-5.13852183513785,-7.95728163016382));
#62993=CARTESIAN_POINT('Ctrl Pts',(37.375288732162,-5.1385731199437,-7.95774704372643));
#62994=CARTESIAN_POINT('Ctrl Pts',(37.3750873701966,-5.1385989493825,-7.9579815146248));
#62995=CARTESIAN_POINT('Ctrl Pts',(37.374681539083,-5.13865101232452,-7.95845425881746));
#62996=CARTESIAN_POINT('Ctrl Pts',(37.374477071377,-5.13867724573001,-7.95869253335952));
#62997=CARTESIAN_POINT('Ctrl Pts',(37.3740647904667,-5.13873014746429,-7.95917317148005));
#62998=CARTESIAN_POINT('Ctrl Pts',(37.3738569788701,-5.13875681568255,-7.95941553638736));
#62999=CARTESIAN_POINT('Ctrl Pts',(37.3734377633411,-5.13881061902815,-7.95990465287597));
#63000=CARTESIAN_POINT('Ctrl Pts',(37.3732263611292,-5.13883775403959,-7.96015140594851));
#63001=CARTESIAN_POINT('Ctrl Pts',(37.3727997081077,-5.1388925242028,-7.96064960853773));
#63002=CARTESIAN_POINT('Ctrl Pts',(37.3725844591586,-5.13892015923054,-7.96090105969881));
#63003=CARTESIAN_POINT('Ctrl Pts',(37.3723012094811,-5.13895652879637,-7.96123208675578));
#63004=CARTESIAN_POINT('Ctrl Pts',(37.3722331622188,-5.13896526645575,-7.96131162245678));
#63005=CARTESIAN_POINT('Ctrl Pts',(37.3720947385011,-5.13898304150204,-7.96147343767126));
#63006=CARTESIAN_POINT('Ctrl Pts',(37.3720243623906,-5.13899207886688,-7.96155571751681));
#63007=CARTESIAN_POINT('Ctrl Pts',(37.371881134098,-5.13901047225392,-7.96172319498457));
#63008=CARTESIAN_POINT('Ctrl Pts',(37.3718082822899,-5.13901982825256,-7.96180839297852));
#63009=CARTESIAN_POINT('Ctrl Pts',(37.3716599441049,-5.13903887933764,-7.96198189456902));
#63010=CARTESIAN_POINT('Ctrl Pts',(37.3715844581852,-5.13904857439234,-7.96207019852269));
#63011=CARTESIAN_POINT('Ctrl Pts',(37.3714306807572,-5.13906832563774,-7.96225011481478));
#63012=CARTESIAN_POINT('Ctrl Pts',(37.3713523897163,-5.13907838179826,-7.9623417275917));
#63013=CARTESIAN_POINT('Ctrl Pts',(37.3711928169677,-5.13909887911991,-7.96252848110824));
#63014=CARTESIAN_POINT('Ctrl Pts',(37.3711115358281,-5.13910932024114,-7.96262362227367));
#63015=CARTESIAN_POINT('Ctrl Pts',(37.3709457826479,-5.13913061330774,-7.96281767027519));
#63016=CARTESIAN_POINT('Ctrl Pts',(37.3708613111888,-5.13914146521513,-7.96291657763994));
#63017=CARTESIAN_POINT('Ctrl Pts',(37.3706889600457,-5.13916360788668,-7.96311841619834));
#63018=CARTESIAN_POINT('Ctrl Pts',(37.370601081077,-5.13917489859979,-7.96322134789813));
#63019=CARTESIAN_POINT('Ctrl Pts',(37.3704216791747,-5.13919794929695,-7.96343151535327));
#63020=CARTESIAN_POINT('Ctrl Pts',(37.3703301569516,-5.13920970923524,-7.96353875177282));
#63021=CARTESIAN_POINT('Ctrl Pts',(37.3701432120181,-5.13923373148482,-7.96375783380939));
#63022=CARTESIAN_POINT('Ctrl Pts',(37.3700477901319,-5.13924599374111,-7.96386968013115));
#63023=CARTESIAN_POINT('Ctrl Pts',(37.3698527665755,-5.13927105667535,-7.96409831445133));
#63024=CARTESIAN_POINT('Ctrl Pts',(37.3697531658085,-5.13928385729427,-7.96421510325992));
#63025=CARTESIAN_POINT('Ctrl Pts',(37.3695494798791,-5.1393100362787,-7.96445398544944));
#63026=CARTESIAN_POINT('Ctrl Pts',(37.3694453957187,-5.13932341457948,-7.96457607975107));
#63027=CARTESIAN_POINT('Ctrl Pts',(37.3692324101243,-5.13935079191195,-7.96482596981878));
#63028=CARTESIAN_POINT('Ctrl Pts',(37.3691235098844,-5.13936479086227,-7.96495376653987));
#63029=CARTESIAN_POINT('Ctrl Pts',(37.3689005280116,-5.13939345652417,-7.9652154959622));
#63030=CARTESIAN_POINT('Ctrl Pts',(37.3687864477202,-5.13940812314472,-7.9653494297442));
#63031=CARTESIAN_POINT('Ctrl Pts',(37.3685527067653,-5.13943817569377,-7.96562390983597));
#63032=CARTESIAN_POINT('Ctrl Pts',(37.3684330475777,-5.13945356152467,-7.96576445741302));
#63033=CARTESIAN_POINT('Ctrl Pts',(37.3681877109628,-5.13948510908146,-7.96605268859481));
#63034=CARTESIAN_POINT('Ctrl Pts',(37.3680620351538,-5.1395012707038,-7.96620037369759));
#63035=CARTESIAN_POINT('Ctrl Pts',(37.3678041836314,-5.13953443210911,-7.96650345637212));
#63036=CARTESIAN_POINT('Ctrl Pts',(37.3676720098507,-5.13955143176251,-7.96665885553446));
#63037=CARTESIAN_POINT('Ctrl Pts',(37.3674006321143,-5.13958633780094,-7.96697800162658));
#63038=CARTESIAN_POINT('Ctrl Pts',(37.3672614303116,-5.13960424404488,-7.96714175042555));
#63039=CARTESIAN_POINT('Ctrl Pts',(37.3669754114797,-5.13964103894506,-7.96747829752053));
#63040=CARTESIAN_POINT('Ctrl Pts',(37.3668285969074,-5.1396599274408,-7.96765109795586));
#63041=CARTESIAN_POINT('Ctrl Pts',(37.366526705891,-5.13969877052325,-7.96800652487232));
#63042=CARTESIAN_POINT('Ctrl Pts',(37.3663716323022,-5.13971872492129,-7.9681891537585));
#63043=CARTESIAN_POINT('Ctrl Pts',(37.3660525074491,-5.13975979247258,-7.96856509829356));
#63044=CARTESIAN_POINT('Ctrl Pts',(37.3658884594421,-5.13978090541262,-7.96875841673723));
#63045=CARTESIAN_POINT('Ctrl Pts',(37.3655505918557,-5.13982439286459,-7.96915669632795));
#63046=CARTESIAN_POINT('Ctrl Pts',(37.3653767760338,-5.13984676713109,-7.96936166069798));
#63047=CARTESIAN_POINT('Ctrl Pts',(37.3650184907207,-5.13989289152661,-7.96978429585711));
#63048=CARTESIAN_POINT('Ctrl Pts',(37.3648340256011,-5.13991664136932,-7.97000197034912));
#63049=CARTESIAN_POINT('Ctrl Pts',(37.3644534599163,-5.13996564418464,-7.97045121155202));
#63050=CARTESIAN_POINT('Ctrl Pts',(37.3642573644202,-5.13999089682653,-7.97068278257198));
#63051=CARTESIAN_POINT('Ctrl Pts',(37.3638524433131,-5.14004304721613,-7.97116114124246));
#63052=CARTESIAN_POINT('Ctrl Pts',(37.3636436235842,-5.14006994458271,-7.97140793394487));
#63053=CARTESIAN_POINT('Ctrl Pts',(37.3632120311691,-5.14012554311096,-7.97191821818251));
#63054=CARTESIAN_POINT('Ctrl Pts',(37.3629892653949,-5.14015424382399,-7.97218171558891));
#63055=CARTESIAN_POINT('Ctrl Pts',(37.3625284125873,-5.14021362672004,-7.97272707104065));
#63056=CARTESIAN_POINT('Ctrl Pts',(37.3622903336792,-5.14024430837654,-7.97300893596624));
#63057=CARTESIAN_POINT('Ctrl Pts',(37.3617973209124,-5.14030785244359,-7.97359289313026));
#63058=CARTESIAN_POINT('Ctrl Pts',(37.3615423966214,-5.14034071423669,-7.97389499348669));
#63059=CARTESIAN_POINT('Ctrl Pts',(37.3610139712229,-5.14040884247556,-7.97452152210394));
#63060=CARTESIAN_POINT('Ctrl Pts',(37.360740481402,-5.14044410819761,-7.97484596000798));
#63061=CARTESIAN_POINT('Ctrl Pts',(37.3601729885504,-5.14051729629013,-7.97551953201326));
#63062=CARTESIAN_POINT('Ctrl Pts',(37.3598789989865,-5.14055521779636,-7.97586867749637));
#63063=CARTESIAN_POINT('Ctrl Pts',(37.3363556790367,-5.14358999101517,-8.003821395009));
#63064=CARTESIAN_POINT('Ctrl Pts',(37.3137483572184,-5.14654695197108,-8.03194619825229));
#63065=CARTESIAN_POINT('Ctrl Pts',(37.2782077345349,-5.15128300733771,-8.07825729478609));
#63066=CARTESIAN_POINT('Ctrl Pts',(37.2648808648161,-5.15308014992894,-8.0961319256744));
#63067=CARTESIAN_POINT('Ctrl Pts',(37.1901355122883,-5.16329997089006,-8.19934822840204));
#63068=CARTESIAN_POINT('Ctrl Pts',(37.1341120226287,-5.17152014443217,-8.28846522314088));
#63069=CARTESIAN_POINT('Ctrl Pts',(37.0364096980596,-5.18761099129585,-8.46916717581044));
#63070=CARTESIAN_POINT('Ctrl Pts',(36.9943077805397,-5.19546105951395,-8.56021608581399));
#63071=CARTESIAN_POINT('Ctrl Pts',(36.9580195978366,-5.20345233470371,-8.65357770242256));
#63072=CARTESIAN_POINT('Origin',(39.2,8.05522481984854,-9.525));
#63073=CARTESIAN_POINT('',(36.9580196851476,-6.73822005631196,-8.65357747779021));
#63074=CARTESIAN_POINT('',(36.9596139210734,-6.47468182945015,-8.65421859155223));
#63075=CARTESIAN_POINT('',(36.958019684865,8.05522481984854,-8.65357747851728));
#63076=CARTESIAN_POINT('Ctrl Pts',(36.9580196851476,-6.73822005631196,-8.65357747779021));
#63077=CARTESIAN_POINT('Ctrl Pts',(36.9617632876953,-6.73732493420928,-8.64394600395906));
#63078=CARTESIAN_POINT('Ctrl Pts',(36.9655691048304,-6.7364326449218,-8.63433826822591));
#63079=CARTESIAN_POINT('Ctrl Pts',(36.9751700656461,-6.73422539355429,-8.61054969304967));
#63080=CARTESIAN_POINT('Ctrl Pts',(36.9810390153733,-6.73291421589457,-8.59639901597012));
#63081=CARTESIAN_POINT('Ctrl Pts',(36.9913409806347,-6.73067762730601,-8.57221537059667));
#63082=CARTESIAN_POINT('Ctrl Pts',(36.995708044588,-6.72974852321965,-8.56215514665832));
#63083=CARTESIAN_POINT('Ctrl Pts',(37.0052308720689,-6.72776294903167,-8.5406222281924));
#63084=CARTESIAN_POINT('Ctrl Pts',(37.0104080080805,-6.72670774970838,-8.52915962448612));
#63085=CARTESIAN_POINT('Ctrl Pts',(37.02515821817,-6.72376667044422,-8.49717266876666));
#63086=CARTESIAN_POINT('Ctrl Pts',(37.0349319176222,-6.72189216412974,-8.47674139129352));
#63087=CARTESIAN_POINT('Ctrl Pts',(37.1161897070929,-6.70686484166701,-8.31286408263086));
#63088=CARTESIAN_POINT('Ctrl Pts',(37.2015708021965,-6.69441356220162,-8.1767281771791));
#63089=CARTESIAN_POINT('Ctrl Pts',(37.3755072074582,-6.67218516050087,-7.95264745657533));
#63090=CARTESIAN_POINT('Ctrl Pts',(37.458511783565,-6.66248933493119,-7.86118509309098));
#63091=CARTESIAN_POINT('Ctrl Pts',(37.5708004800093,-6.65000379136199,-7.75510388194618));
#63092=CARTESIAN_POINT('Ctrl Pts',(37.5938571623798,-6.64747059549469,-7.73415428826679));
#63093=CARTESIAN_POINT('Ctrl Pts',(37.6333013925827,-6.64318109659655,-7.69968928695764));
#63094=CARTESIAN_POINT('Ctrl Pts',(37.6494733214651,-6.6414344333673,-7.68593211455313));
#63095=CARTESIAN_POINT('Ctrl Pts',(37.6671808776097,-6.63953370052731,-7.67126820095321));
#63096=CARTESIAN_POINT('Ctrl Pts',(37.6685382520381,-6.63938807380186,-7.67014664750604));
#63097=CARTESIAN_POINT('Ctrl Pts',(37.6712600756542,-6.63909620868146,-7.66790271941159));
#63098=CARTESIAN_POINT('Ctrl Pts',(37.6726245323447,-6.63894996998278,-7.66678035565537));
#63099=CARTESIAN_POINT('Ctrl Pts',(37.6754466796612,-6.63864765171348,-7.66446414493327));
#63100=CARTESIAN_POINT('Ctrl Pts',(37.6769045384281,-6.63849156420354,-7.66327050583539));
#63101=CARTESIAN_POINT('Ctrl Pts',(37.6800493630152,-6.63815503779881,-7.66070180974682));
#63102=CARTESIAN_POINT('Ctrl Pts',(37.6817367941519,-6.63797457672905,-7.65932732807841));
#63103=CARTESIAN_POINT('Ctrl Pts',(37.6976120293693,-6.63627783768494,-7.64643210085669));
#63104=CARTESIAN_POINT('Ctrl Pts',(37.7119284223306,-6.63475539226718,-7.63507145452685));
#63105=CARTESIAN_POINT('Ctrl Pts',(37.7425622002386,-6.63151278937312,-7.61132615255223));
#63106=CARTESIAN_POINT('Ctrl Pts',(37.7589110164648,-6.62979110882047,-7.59898467800878));
#63107=CARTESIAN_POINT('Ctrl Pts',(37.8009451972879,-6.62538535777805,-7.56808852067323));
#63108=CARTESIAN_POINT('Ctrl Pts',(37.8268423927752,-6.62269033423657,-7.54983042274668));
#63109=CARTESIAN_POINT('Ctrl Pts',(37.9458759828876,-6.61038255860204,-7.46938154361071));
#63110=CARTESIAN_POINT('Ctrl Pts',(38.0429106479893,-6.60055645517692,-7.41323989339178));
#63111=CARTESIAN_POINT('Ctrl Pts',(38.2701190271191,-6.57802028181283,-7.30215426009766));
#63112=CARTESIAN_POINT('Ctrl Pts',(38.4019433277125,-6.56525751550808,-7.25149479849223));
#63113=CARTESIAN_POINT('Ctrl Pts',(38.5969246568206,-6.54721870987632,-7.19562633303788));
#63114=CARTESIAN_POINT('Ctrl Pts',(38.6570490389488,-6.54176914670581,-7.18088236616085));
#63115=CARTESIAN_POINT('Ctrl Pts',(38.7352459054524,-6.53487509170483,-7.16487754279157));
#63116=CARTESIAN_POINT('Ctrl Pts',(38.7528509064137,-6.53333551884981,-7.16147887068167));
#63117=CARTESIAN_POINT('Ctrl Pts',(38.7817487065672,-6.53083055211108,-7.15623457009995));
#63118=CARTESIAN_POINT('Ctrl Pts',(38.7930192020985,-6.52985908382715,-7.15427216741645));
#63119=CARTESIAN_POINT('Ctrl Pts',(38.8157844488211,-6.52790844759465,-7.15047545210971));
#63120=CARTESIAN_POINT('Ctrl Pts',(38.8272793278231,-6.52692945011543,-7.14864402147418));
#63121=CARTESIAN_POINT('Ctrl Pts',(38.8574383659131,-6.52437529971452,-7.14406313519393));
#63122=CARTESIAN_POINT('Ctrl Pts',(38.8761228817015,-6.52280737414565,-7.14144960032692));
#63123=CARTESIAN_POINT('Ctrl Pts',(38.9611921081414,-6.51572612648478,-7.13056922250495));
#63124=CARTESIAN_POINT('Ctrl Pts',(39.0278803730816,-6.51033316904641,-7.12485314492138));
#63125=CARTESIAN_POINT('Ctrl Pts',(39.2443969461397,-6.49307836567454,-7.11536813755116));
#63126=CARTESIAN_POINT('Ctrl Pts',(39.3943568228586,-6.48150273421907,-7.12280796894516));
#63127=CARTESIAN_POINT('Ctrl Pts',(39.6410462369733,-6.46183336385126,-7.1583119504988));
#63128=CARTESIAN_POINT('Ctrl Pts',(39.7384518990124,-6.45390307346302,-7.17855598356188));
#63129=CARTESIAN_POINT('Ctrl Pts',(39.8634263135476,-6.44332082728093,-7.21272208856444));
#63130=CARTESIAN_POINT('Ctrl Pts',(39.8923816996738,-6.44084021023864,-7.22122678394347));
#63131=CARTESIAN_POINT('Ctrl Pts',(39.940422740592,-6.43667142025576,-7.23632473577453));
#63132=CARTESIAN_POINT('Ctrl Pts',(39.9595997632192,-6.43499301680374,-7.24261781295982));
#63133=CARTESIAN_POINT('Ctrl Pts',(39.9973266423046,-6.43166134067247,-7.2555262814895));
#63134=CARTESIAN_POINT('Ctrl Pts',(40.0158789603609,-6.43000857575912,-7.26212965322686));
#63135=CARTESIAN_POINT('Ctrl Pts',(40.0569160058768,-6.42631939660508,-7.27730631477722));
#63136=CARTESIAN_POINT('Ctrl Pts',(40.0793570539079,-6.42427947064588,-7.28599061523573));
#63137=CARTESIAN_POINT('Ctrl Pts',(40.1594038099944,-6.41691922974186,-7.31835632365124));
#63138=CARTESIAN_POINT('Ctrl Pts',(40.21620989349,-6.41153757785529,-7.34393421720117));
#63139=CARTESIAN_POINT('Ctrl Pts',(40.4384415418904,-6.38982333259559,-7.45456465709944));
#63140=CARTESIAN_POINT('Ctrl Pts',(40.5947397533889,-6.37298054649957,-7.55646688203441));
#63141=CARTESIAN_POINT('Ctrl Pts',(40.7771573655121,-6.35179173635574,-7.70811837674365));
#63142=CARTESIAN_POINT('Ctrl Pts',(40.815546189843,-6.34723783469156,-7.74216645793597));
#63143=CARTESIAN_POINT('Ctrl Pts',(40.8775942195695,-6.33974907837542,-7.80084994513031));
#63144=CARTESIAN_POINT('Ctrl Pts',(40.9018699802078,-6.33678419194224,-7.82480745270185));
#63145=CARTESIAN_POINT('Ctrl Pts',(40.9357801864565,-6.33260135466889,-7.85972753655362));
#63146=CARTESIAN_POINT('Ctrl Pts',(40.9458357920986,-6.33135560774718,-7.87027263471603));
#63147=CARTESIAN_POINT('Ctrl Pts',(40.9632327349762,-6.32919185155013,-7.88885157513314));
#63148=CARTESIAN_POINT('Ctrl Pts',(40.9706162556708,-6.32827082573229,-7.89684477377029));
#63149=CARTESIAN_POINT('Ctrl Pts',(40.9867227172739,-6.32625584533185,-7.9145203552941));
#63150=CARTESIAN_POINT('Ctrl Pts',(40.9954215500755,-6.32516362084392,-7.92422386441594));
#63151=CARTESIAN_POINT('Ctrl Pts',(41.0209337916485,-6.32194669716284,-7.95315226187664));
#63152=CARTESIAN_POINT('Ctrl Pts',(41.0375210865199,-6.31983732708361,-7.97257557323292));
#63153=CARTESIAN_POINT('Ctrl Pts',(41.1329344721321,-6.30757115000303,-8.08797485831539));
#63154=CARTESIAN_POINT('Ctrl Pts',(41.2045525960589,-6.29781322727732,-8.1896891916301));
#63155=CARTESIAN_POINT('Ctrl Pts',(41.3311472018903,-6.27838567107459,-8.40279187484914));
#63156=CARTESIAN_POINT('Ctrl Pts',(41.3859998902747,-6.26874217145774,-8.51379226876584));
#63157=CARTESIAN_POINT('Ctrl Pts',(41.4486825380718,-6.2553053979647,-8.66985955813001));
#63158=CARTESIAN_POINT('Ctrl Pts',(41.4641361821291,-6.25171931273061,-8.71165797551311));
#63159=CARTESIAN_POINT('Ctrl Pts',(41.4900234305108,-6.2451573368809,-8.78814466990518));
#63160=CARTESIAN_POINT('Ctrl Pts',(41.5008514781816,-6.24219408799807,-8.82268576157862));
#63161=CARTESIAN_POINT('Ctrl Pts',(41.516836877065,-6.2374385119812,-8.87802383753787));
#63162=CARTESIAN_POINT('Ctrl Pts',(41.5225031421398,-6.23566256111774,-8.89866912647387));
#63163=CARTESIAN_POINT('Ctrl Pts',(41.5327626263355,-6.23226518490991,-8.93810514483334));
#63164=CARTESIAN_POINT('Ctrl Pts',(41.5374062426974,-6.23064551324529,-8.95688112868409));
#63165=CARTESIAN_POINT('Ctrl Pts',(41.5474859403931,-6.22693241201079,-8.99985458000316));
#63166=CARTESIAN_POINT('Ctrl Pts',(41.5527751291091,-6.22483451716637,-9.02408379408837));
#63167=CARTESIAN_POINT('Ctrl Pts',(41.5687678124529,-6.21796751208791,-9.10319612269222));
#63168=CARTESIAN_POINT('Ctrl Pts',(41.5779316196392,-6.21315158159198,-9.15836724187236));
#63169=CARTESIAN_POINT('Ctrl Pts',(41.6109195015664,-6.19093840323978,-9.41120223122716));
#63170=CARTESIAN_POINT('Ctrl Pts',(41.6120653831861,-6.17289934019233,-9.61101541992265));
#63171=CARTESIAN_POINT('Ctrl Pts',(41.5827176011395,-6.15068148692619,-9.85816223897083));
#63172=CARTESIAN_POINT('Ctrl Pts',(41.575297428387,-6.14625685843701,-9.90749584153287));
#63173=CARTESIAN_POINT('Ctrl Pts',(41.560349006788,-6.13895450013743,-9.98946046965122));
#63174=CARTESIAN_POINT('Ctrl Pts',(41.5536641906323,-6.13604844213904,-10.0222284901388));
#63175=CARTESIAN_POINT('Ctrl Pts',(41.5431122892356,-6.13193280231949,-10.0689548436887));
#63176=CARTESIAN_POINT('Ctrl Pts',(41.5397995474366,-6.13069657537435,-10.0830324204316));
#63177=CARTESIAN_POINT('Ctrl Pts',(41.5337741617397,-6.12854314511448,-10.1076399481452));
#63178=CARTESIAN_POINT('Ctrl Pts',(41.5311168162326,-6.12762302436337,-10.1181825649661));
#63179=CARTESIAN_POINT('Ctrl Pts',(41.5250978360649,-6.12560254477502,-10.1413966543453));
#63180=CARTESIAN_POINT('Ctrl Pts',(41.5217039906145,-6.1245039919606,-10.1540591287194));
#63181=CARTESIAN_POINT('Ctrl Pts',(41.5114994861476,-6.1213143061097,-10.1909243046892));
#63182=CARTESIAN_POINT('Ctrl Pts',(41.5044124112449,-6.11923777688948,-10.2150497405517));
#63183=CARTESIAN_POINT('Ctrl Pts',(41.4609714704746,-6.1072489642283,-10.3547879043515));
#63184=CARTESIAN_POINT('Ctrl Pts',(41.4162949157245,-6.09771662276638,-10.4676480982827));
#63185=CARTESIAN_POINT('Ctrl Pts',(41.3098505940253,-6.07862994592636,-10.6866042205433));
#63186=CARTESIAN_POINT('Ctrl Pts',(41.2481098308799,-6.06910124965959,-10.792295354218));
#63187=CARTESIAN_POINT('Ctrl Pts',(41.1396377229013,-6.05388472510908,-10.9492031649496));
#63188=CARTESIAN_POINT('Ctrl Pts',(41.0982809803045,-6.04835819458522,-11.003876891567));
#63189=CARTESIAN_POINT('Ctrl Pts',(41.0375021287759,-6.04053690080271,-11.0774703120498));
#63190=CARTESIAN_POINT('Ctrl Pts',(41.0200071030013,-6.0383173326261,-11.0979437909876));
#63191=CARTESIAN_POINT('Ctrl Pts',(40.9891986898125,-6.03445912854515,-11.1327949870413));
#63192=CARTESIAN_POINT('Ctrl Pts',(40.9760462450375,-6.03282717824222,-11.1473120414329));
#63193=CARTESIAN_POINT('Ctrl Pts',(40.9486326795084,-6.02945519070382,-11.1768369314884));
#63194=CARTESIAN_POINT('Ctrl Pts',(40.9343522206689,-6.02771442745515,-11.1918244698666));
#63195=CARTESIAN_POINT('Ctrl Pts',(40.8969815866578,-6.02319769938935,-11.2300452471005));
#63196=CARTESIAN_POINT('Ctrl Pts',(40.8736078931447,-6.02040965430334,-11.252993690112));
#63197=CARTESIAN_POINT('Ctrl Pts',(40.7504643489673,-6.00589956425235,-11.3690542873462));
#63198=CARTESIAN_POINT('Ctrl Pts',(40.6433889578231,-5.99385045387143,-11.4540129472089));
#63199=CARTESIAN_POINT('Ctrl Pts',(40.4271535582749,-5.9706093319988,-11.5974608473102));
#63200=CARTESIAN_POINT('Ctrl Pts',(40.3195244837418,-5.95948640846034,-11.6575257418319));
#63201=CARTESIAN_POINT('Ctrl Pts',(40.158227233283,-5.94373343670977,-11.7319504980944));
#63202=CARTESIAN_POINT('Ctrl Pts',(40.1079163080143,-5.93894207212785,-11.7531200883342));
#63203=CARTESIAN_POINT('Ctrl Pts',(40.0408195983243,-5.93274567540705,-11.7787019317493));
#63204=CARTESIAN_POINT('Ctrl Pts',(40.0246490200211,-5.93126682506256,-11.7846690113618));
#63205=CARTESIAN_POINT('Ctrl Pts',(39.9977743403617,-5.92883448782804,-11.794259061274));
#63206=CARTESIAN_POINT('Ctrl Pts',(39.987106631958,-5.92787556985234,-11.7979812488116));
#63207=CARTESIAN_POINT('Ctrl Pts',(39.9652223638526,-5.92592234557862,-11.8054445759096));
#63208=CARTESIAN_POINT('Ctrl Pts',(39.9540037628862,-5.92492845178307,-11.8091784243139));
#63209=CARTESIAN_POINT('Ctrl Pts',(39.9240024159592,-5.92228902496824,-11.8189185433317));
#63210=CARTESIAN_POINT('Ctrl Pts',(39.9051720203854,-5.92065161827214,-11.8247770067141));
#63211=CARTESIAN_POINT('Ctrl Pts',(39.807573326011,-5.9122531806656,-11.8538301123938));
#63212=CARTESIAN_POINT('Ctrl Pts',(39.7277170384287,-5.90567613948618,-11.8732149368493));
#63213=CARTESIAN_POINT('Ctrl Pts',(39.4941296177812,-5.88685949958672,-11.9173943922438));
#63214=CARTESIAN_POINT('Ctrl Pts',(39.3387995799375,-5.87484286204838,-11.9314079673804));
#63215=CARTESIAN_POINT('Ctrl Pts',(39.1025025399608,-5.85608414372925,-11.9297577765034));
#63216=CARTESIAN_POINT('Ctrl Pts',(39.0218909637995,-5.84960492601225,-11.9251334172715));
#63217=CARTESIAN_POINT('Ctrl Pts',(38.9134250808235,-5.84067886678781,-11.9134168210842));
#63218=CARTESIAN_POINT('Ctrl Pts',(38.8852365266294,-5.83834022655684,-11.9098655964751));
#63219=CARTESIAN_POINT('Ctrl Pts',(38.8374746602102,-5.83434157424136,-11.9029870085379));
#63220=CARTESIAN_POINT('Ctrl Pts',(38.8178670655835,-5.83268961730645,-11.8999149891599));
#63221=CARTESIAN_POINT('Ctrl Pts',(38.7806416173982,-5.82953228057051,-11.8936097753284));
#63222=CARTESIAN_POINT('Ctrl Pts',(38.7630173824434,-5.82802841888467,-11.8904217120192));
#63223=CARTESIAN_POINT('Ctrl Pts',(38.7217743692136,-5.82448702663994,-11.8824845806877));
#63224=CARTESIAN_POINT('Ctrl Pts',(38.6981885315037,-5.82244465002882,-11.8775769831172));
#63225=CARTESIAN_POINT('Ctrl Pts',(38.6135077247214,-5.81504723860042,-11.8586258023767));
#63226=CARTESIAN_POINT('Ctrl Pts',(38.5528991174626,-5.80962995434926,-11.8425507557642));
#63227=CARTESIAN_POINT('Ctrl Pts',(38.2869390602945,-5.78528680433578,-11.7607651565887));
#63228=CARTESIAN_POINT('Ctrl Pts',(38.0903467014128,-5.7656346295313,-11.6699875869335));
#63229=CARTESIAN_POINT('Ctrl Pts',(37.8661221209814,-5.74211087553907,-11.5272859424611));
#63230=CARTESIAN_POINT('Ctrl Pts',(37.8245713105267,-5.73770523398101,-11.49897469517));
#63231=CARTESIAN_POINT('Ctrl Pts',(37.7703770435447,-5.7319237744806,-11.4595057354295));
#63232=CARTESIAN_POINT('Ctrl Pts',(37.7569226576988,-5.73048547387496,-11.4494900808571));
#63233=CARTESIAN_POINT('Ctrl Pts',(37.7346535900901,-5.72810125882929,-11.4325477617431));
#63234=CARTESIAN_POINT('Ctrl Pts',(37.7257807868404,-5.72715033748417,-11.4256988975437));
#63235=CARTESIAN_POINT('Ctrl Pts',(37.7075338508162,-5.72519323776088,-11.4114095393946));
#63236=CARTESIAN_POINT('Ctrl Pts',(37.6981668410966,-5.72418764997645,-11.4039607071011));
#63237=CARTESIAN_POINT('Ctrl Pts',(37.6729915944048,-5.7214812436611,-11.3836322999105));
#63238=CARTESIAN_POINT('Ctrl Pts',(37.6572903968992,-5.71978928554687,-11.3706207254715));
#63239=CARTESIAN_POINT('Ctrl Pts',(37.5601887042316,-5.70928587629362,-11.2880474370306));
#63240=CARTESIAN_POINT('Ctrl Pts',(37.4833310081189,-5.70079253976512,-11.2133044670983));
#63241=CARTESIAN_POINT('Ctrl Pts',(37.3209233792285,-5.68169521221423,-11.0327626464593));
#63242=CARTESIAN_POINT('Ctrl Pts',(37.238853538038,-5.67116022287281,-10.9243499671334));
#63243=CARTESIAN_POINT('Ctrl Pts',(37.1389832251379,-5.65628667485469,-10.7662460920522));
#63244=CARTESIAN_POINT('Ctrl Pts',(37.1129949173773,-5.65217738587393,-10.7220343251728));
#63245=CARTESIAN_POINT('Ctrl Pts',(37.0691780535898,-5.64476468373186,-10.6417221478682));
#63246=CARTESIAN_POINT('Ctrl Pts',(37.0508052825954,-5.64147977256848,-10.6059404322621));
#63247=CARTESIAN_POINT('Ctrl Pts',(37.0236868419793,-5.63633210306697,-10.5496989172435));
#63248=CARTESIAN_POINT('Ctrl Pts',(37.0143128058653,-5.63449085519254,-10.5295487812455));
#63249=CARTESIAN_POINT('Ctrl Pts',(36.9973571311387,-5.63103982064296,-10.4917401578452));
#63250=CARTESIAN_POINT('Ctrl Pts',(36.9897052451479,-5.62943256572078,-10.4741149517957));
#63251=CARTESIAN_POINT('Ctrl Pts',(36.9730109495247,-5.62580986630952,-10.4343645820266));
#63252=CARTESIAN_POINT('Ctrl Pts',(36.9640856554668,-5.62379069445494,-10.4121928365886));
#63253=CARTESIAN_POINT('Ctrl Pts',(36.9418351655035,-5.61853378096758,-10.3544499571195));
#63254=CARTESIAN_POINT('Ctrl Pts',(36.9290200698861,-5.61527986165507,-10.3186910347625));
#63255=CARTESIAN_POINT('Ctrl Pts',(36.8586020307597,-5.59596973608905,-10.1065070297757));
#63256=CARTESIAN_POINT('Ctrl Pts',(36.8207380237783,-5.57930051890073,-9.92422533382003));
#63257=CARTESIAN_POINT('Ctrl Pts',(36.7977867859462,-5.55618743923678,-9.66781775090883));
#63258=CARTESIAN_POINT('Ctrl Pts',(36.7945903213438,-5.54975260958905,-9.59592895843203));
#63259=CARTESIAN_POINT('Ctrl Pts',(36.7946376502955,-5.53970999683671,-9.48202068814434));
#63260=CARTESIAN_POINT('Ctrl Pts',(36.7957540752139,-5.53604252743491,-9.44004474681283));
#63261=CARTESIAN_POINT('Ctrl Pts',(36.7988223204285,-5.53103101498072,-9.3819599937646));
#63262=CARTESIAN_POINT('Ctrl Pts',(36.799838757767,-5.52964461290738,-9.3658122241438));
#63263=CARTESIAN_POINT('Ctrl Pts',(36.8018192412762,-5.52733069010559,-9.33871311521891));
#63264=CARTESIAN_POINT('Ctrl Pts',(36.8026955466722,-5.52639861951119,-9.32775615125956));
#63265=CARTESIAN_POINT('Ctrl Pts',(36.8046979925372,-5.52444578697903,-9.30470772694864));
#63266=CARTESIAN_POINT('Ctrl Pts',(36.8058406255734,-5.5234259203755,-9.29261819697242));
#63267=CARTESIAN_POINT('Ctrl Pts',(36.8092307565423,-5.52063741178237,-9.25943385384409));
#63268=CARTESIAN_POINT('Ctrl Pts',(36.8116659024057,-5.51887856483244,-9.23835861012314));
#63269=CARTESIAN_POINT('Ctrl Pts',(36.8307047768568,-5.50662621036752,-9.09074056940703));
#63270=CARTESIAN_POINT('Ctrl Pts',(36.8570807199413,-5.49658439037482,-8.96564233949315));
#63271=CARTESIAN_POINT('Ctrl Pts',(36.9122212614242,-5.48133196633905,-8.77908232341413));
#63272=CARTESIAN_POINT('Ctrl Pts',(36.9338279612903,-5.4761097739669,-8.71581746937143));
#63273=CARTESIAN_POINT('Ctrl Pts',(36.9580198925264,-5.47085833376936,-8.65357694424991));
#63274=CARTESIAN_POINT('',(36.7953937665934,-5.27977575808644,-9.52712105355602));
#63275=CARTESIAN_POINT('Ctrl Pts',(36.9580195978366,-5.20345233470371,-8.65357770242256));
#63276=CARTESIAN_POINT('Ctrl Pts',(36.9423609402093,-5.20690063750865,-8.69386402929538));
#63277=CARTESIAN_POINT('Ctrl Pts',(36.9277847806697,-5.21037444878413,-8.73458104174594));
#63278=CARTESIAN_POINT('Ctrl Pts',(36.9022171597942,-5.21702892112913,-8.81257191891362));
#63279=CARTESIAN_POINT('Ctrl Pts',(36.8910202278685,-5.22020074035216,-8.84974313907366));
#63280=CARTESIAN_POINT('Ctrl Pts',(36.8748524133117,-5.22522801618809,-8.90853212764523));
#63281=CARTESIAN_POINT('Ctrl Pts',(36.8692724073146,-5.2270640211245,-8.9299766739618));
#63282=CARTESIAN_POINT('Ctrl Pts',(36.8594082182302,-5.23050993985417,-8.97015562393998));
#63283=CARTESIAN_POINT('Ctrl Pts',(36.8550507176876,-5.23211737822682,-8.98887036230359));
#63284=CARTESIAN_POINT('Ctrl Pts',(36.8469379765276,-5.23528696707361,-9.02570602778406));
#63285=CARTESIAN_POINT('Ctrl Pts',(36.8431667138616,-5.23684848821396,-9.04382209399185));
#63286=CARTESIAN_POINT('Ctrl Pts',(36.8350760192108,-5.2404105884101,-9.08506698208142));
#63287=CARTESIAN_POINT('Ctrl Pts',(36.830886252031,-5.24241506382615,-9.10821893009701));
#63288=CARTESIAN_POINT('Ctrl Pts',(36.8195276657382,-5.24836071037824,-9.17670319407919));
#63289=CARTESIAN_POINT('Ctrl Pts',(36.8133162770967,-5.2523302120571,-9.22218089056959));
#63290=CARTESIAN_POINT('Ctrl Pts',(36.7991452241016,-5.26389805224255,-9.35395403251787));
#63291=CARTESIAN_POINT('Ctrl Pts',(36.7945433759335,-5.27158206251985,-9.44052960809255));
#63292=CARTESIAN_POINT('Ctrl Pts',(36.794620964868,-5.27933234931437,-9.52715447146443));
#63293=CARTESIAN_POINT('Ctrl Pts',(36.7953937665934,-5.27977575808644,-9.52712105355602));
#63294=CARTESIAN_POINT('Ctrl Pts',(36.7935531956842,-5.2976235321573,-9.73963463083655));
#63295=CARTESIAN_POINT('Ctrl Pts',(36.9163459897307,-5.3823399067148,-10.7462609175526));
#63296=CARTESIAN_POINT('Ctrl Pts',(38.3249527608304,-5.53392488175899,-12.2249208567151));
#63297=CARTESIAN_POINT('Ctrl Pts',(40.9825464123629,-5.73453068321897,-11.733576145637));
#63298=CARTESIAN_POINT('Ctrl Pts',(42.0237943679678,-5.93513648467895,-9.23957808294332));
#63299=CARTESIAN_POINT('Ctrl Pts',(40.504532346838,-6.13574228613894,-7.00438982399976));
#63300=CARTESIAN_POINT('Ctrl Pts',(38.0819715177778,-6.31559073439599,-7.04957992665282));
#63301=CARTESIAN_POINT('Ctrl Pts',(37.1630963681982,-6.42857058216639,-8.14366218756688));
#63302=CARTESIAN_POINT('Ctrl Pts',(36.9596139210735,-6.47468182945012,-8.65421859155197));
#63303=CARTESIAN_POINT('Origin',(39.2,8.05522481984854,-9.525));
#63304=CARTESIAN_POINT('',(36.960685369651,-8.0104155729454,-8.65458630036363));
#63305=CARTESIAN_POINT('',(36.9580196848652,-7.74707540691375,-8.65357747851679));
#63306=CARTESIAN_POINT('',(36.958019684865,8.05522481984854,-8.65357747851728));
#63307=CARTESIAN_POINT('',(36.7979795612525,-6.81524146755324,-9.52396154577679));
#63308=CARTESIAN_POINT('Ctrl Pts',(36.7980085683911,-6.81522481984856,-9.52396299273671));
#63309=CARTESIAN_POINT('Ctrl Pts',(36.7998408421343,-6.85429379911921,-9.99043766253926));
#63310=CARTESIAN_POINT('Ctrl Pts',(37.155387877586,-6.96023137887653,-11.2578897609434));
#63311=CARTESIAN_POINT('Ctrl Pts',(39.2043913575984,-7.13303755912051,-12.363179688143));
#63312=CARTESIAN_POINT('Ctrl Pts',(41.5790395607839,-7.33364336058048,-11.0727254258319));
#63313=CARTESIAN_POINT('Ctrl Pts',(41.7964646321477,-7.53424916204047,-8.3788522608558));
#63314=CARTESIAN_POINT('Ctrl Pts',(39.6595137365683,-7.73485496350045,-6.72426253398319));
#63315=CARTESIAN_POINT('Ctrl Pts',(37.6390531498371,-7.89357710046876,-7.42449738893203));
#63316=CARTESIAN_POINT('Ctrl Pts',(37.0669560907077,-7.98543063695042,-8.37601688395995));
#63317=CARTESIAN_POINT('Ctrl Pts',(36.960685369651,-8.0104155729454,-8.65458630036363));
#63318=CARTESIAN_POINT('Ctrl Pts',(36.7946203023417,-6.81716940505584,-9.52379397623225));
#63319=CARTESIAN_POINT('Ctrl Pts',(36.7947236645737,-6.7994075675383,-9.31764097916309));
#63320=CARTESIAN_POINT('Ctrl Pts',(36.8213300094935,-6.78083055974931,-9.11238328777849));
#63321=CARTESIAN_POINT('Ctrl Pts',(36.8896249052172,-6.75676977471914,-8.85275714142221));
#63322=CARTESIAN_POINT('Ctrl Pts',(36.9078343242278,-6.75120685609406,-8.79307025277999));
#63323=CARTESIAN_POINT('Ctrl Pts',(36.9377559246244,-6.74320114444374,-8.70712224457528));
#63324=CARTESIAN_POINT('Ctrl Pts',(36.9476490838554,-6.7406997411387,-8.68025877573441));
#63325=CARTESIAN_POINT('Ctrl Pts',(36.9580196851476,-6.73822005631196,-8.65357747779021));
#63326=CARTESIAN_POINT('',(36.7912413910993,-6.54982113404641,-9.52410385179467));
#63327=CARTESIAN_POINT('Ctrl Pts',(36.9596139210735,-6.47468182945012,-8.65421859155197));
#63328=CARTESIAN_POINT('Ctrl Pts',(36.8680146416272,-6.49543918265305,-8.88404971154581));
#63329=CARTESIAN_POINT('Ctrl Pts',(36.7994752463598,-6.5204702995535,-9.17684559940756));
#63330=CARTESIAN_POINT('Ctrl Pts',(36.7909182968623,-6.54550141645394,-9.47345140065415));
#63331=CARTESIAN_POINT('Ctrl Pts',(36.7911611527837,-6.54977518015146,-9.52410755556446));
#63332=CARTESIAN_POINT('Ctrl Pts',(36.7946202300976,-6.55175625458268,-9.52394788588594));
#63333=CARTESIAN_POINT('Ctrl Pts',(36.7945192429906,-6.57057638584763,-9.7548281115921));
#63334=CARTESIAN_POINT('Ctrl Pts',(36.8276582622447,-6.58807846590248,-9.98456139645675));
#63335=CARTESIAN_POINT('Ctrl Pts',(36.913485047566,-6.61222119073305,-10.2752709658564));
#63336=CARTESIAN_POINT('Ctrl Pts',(36.9370116534691,-6.6180310435769,-10.3434980442765));
#63337=CARTESIAN_POINT('Ctrl Pts',(36.9736516944288,-6.62618226114725,-10.4360305520619));
#63338=CARTESIAN_POINT('Ctrl Pts',(36.9841714418198,-6.62843927809972,-10.4613263965217));
#63339=CARTESIAN_POINT('Ctrl Pts',(37.0029798955398,-6.63234105742448,-10.5044601804163));
#63340=CARTESIAN_POINT('Ctrl Pts',(37.0110597725077,-6.63397870689111,-10.5223866936633));
#63341=CARTESIAN_POINT('Ctrl Pts',(37.0280301087171,-6.63734300289247,-10.5588384282946));
#63342=CARTESIAN_POINT('Ctrl Pts',(37.0369399624873,-6.63907019712561,-10.5773527557263));
#63343=CARTESIAN_POINT('Ctrl Pts',(37.0603350133932,-6.64350943445977,-10.6244140992691));
#63344=CARTESIAN_POINT('Ctrl Pts',(37.0751544165008,-6.64623277238769,-10.6527892758816));
#63345=CARTESIAN_POINT('Ctrl Pts',(37.1489780264201,-6.65939761601173,-10.7875188140521));
#63346=CARTESIAN_POINT('Ctrl Pts',(37.2154157112662,-6.67009447107294,-10.8895733192653));
#63347=CARTESIAN_POINT('Ctrl Pts',(37.3698533729294,-6.69279948136676,-11.0915292819344));
#63348=CARTESIAN_POINT('Ctrl Pts',(37.4590132488357,-6.70480223993357,-11.1900572313959));
#63349=CARTESIAN_POINT('Ctrl Pts',(37.5856563622757,-6.72022330687607,-11.3086524542241));
#63350=CARTESIAN_POINT('Ctrl Pts',(37.6161800852135,-6.72382997238577,-11.3358109725625));
#63351=CARTESIAN_POINT('Ctrl Pts',(37.6630318637157,-6.7291881757941,-11.3754058195997));
#63352=CARTESIAN_POINT('Ctrl Pts',(37.6788501177488,-6.73096807486855,-11.3884312065346));
#63353=CARTESIAN_POINT('Ctrl Pts',(37.7072945431781,-6.73411471909965,-11.4112498687287));
#63354=CARTESIAN_POINT('Ctrl Pts',(37.7198552916762,-6.73548599752059,-11.4211223147714));
#63355=CARTESIAN_POINT('Ctrl Pts',(37.7326816424699,-6.73686719019395,-11.4309983805954));
#63356=CARTESIAN_POINT('Ctrl Pts',(37.7328493229138,-6.73688524341524,-11.4311274563635));
#63357=CARTESIAN_POINT('Ctrl Pts',(37.7331836619575,-6.7369212333024,-11.4313847510581));
#63358=CARTESIAN_POINT('Ctrl Pts',(37.7333503203456,-6.73693916998665,-11.431512970264));
#63359=CARTESIAN_POINT('Ctrl Pts',(37.7336830354551,-6.73697497213335,-11.4317688763368));
#63360=CARTESIAN_POINT('Ctrl Pts',(37.7338490920594,-6.73699283760785,-11.4318965633782));
#63361=CARTESIAN_POINT('Ctrl Pts',(37.7341810275632,-6.73702854301002,-11.4321517318273));
#63362=CARTESIAN_POINT('Ctrl Pts',(37.7343469064506,-6.73704638294455,-11.4322792133131));
#63363=CARTESIAN_POINT('Ctrl Pts',(37.7346789187009,-6.73708208375974,-11.432534302964));
#63364=CARTESIAN_POINT('Ctrl Pts',(37.7348450520678,-6.73709994463227,-11.4326619110403));
#63365=CARTESIAN_POINT('Ctrl Pts',(37.7351780183152,-6.73713573513146,-11.4329175953405));
#63366=CARTESIAN_POINT('Ctrl Pts',(37.7353448513137,-6.73715366474497,-11.4330456713778));
#63367=CARTESIAN_POINT('Ctrl Pts',(37.7356796799401,-6.73718964240742,-11.4333026462008));
#63368=CARTESIAN_POINT('Ctrl Pts',(37.7358476757828,-6.73720769043537,-11.4334315446793));
#63369=CARTESIAN_POINT('Ctrl Pts',(37.7361853171221,-6.73724395710308,-11.4336905365446));
#63370=CARTESIAN_POINT('Ctrl Pts',(37.7363549629734,-6.73726217571738,-11.4338206295227));
#63371=CARTESIAN_POINT('Ctrl Pts',(37.7366964219543,-6.73729883894172,-11.4340824051724));
#63372=CARTESIAN_POINT('Ctrl Pts',(37.736868235519,-6.73731728351362,-11.4342140872691));
#63373=CARTESIAN_POINT('Ctrl Pts',(37.7372145857926,-6.7373544580567,-11.4344794643356));
#63374=CARTESIAN_POINT('Ctrl Pts',(37.7373891230734,-6.73737318798078,-11.4346131585831));
#63375=CARTESIAN_POINT('Ctrl Pts',(37.7377415239058,-6.7374109976085,-11.43488301832));
#63376=CARTESIAN_POINT('Ctrl Pts',(37.7379193881638,-6.73743007725286,-11.4350191829061));
#63377=CARTESIAN_POINT('Ctrl Pts',(37.7382791040823,-6.73746865681699,-11.4352944849595));
#63378=CARTESIAN_POINT('Ctrl Pts',(37.7384609565821,-6.73748815666127,-11.4354336213003));
#63379=CARTESIAN_POINT('Ctrl Pts',(37.7388293809965,-6.73752765459989,-11.4357154214385));
#63380=CARTESIAN_POINT('Ctrl Pts',(37.7390159539487,-6.73754765260462,-11.4358580838842));
#63381=CARTESIAN_POINT('Ctrl Pts',(37.739394637933,-6.73758823398598,-11.4361475555698));
#63382=CARTESIAN_POINT('Ctrl Pts',(37.7395867502073,-6.73760881725327,-11.4362943631711));
#63383=CARTESIAN_POINT('Ctrl Pts',(37.7399774375662,-6.7376506674804,-11.4365928238029));
#63384=CARTESIAN_POINT('Ctrl Pts',(37.7401760141838,-6.73767193431238,-11.4367444748885));
#63385=CARTESIAN_POINT('Ctrl Pts',(37.7405806853476,-6.7377152637571,-11.4370534186145));
#63386=CARTESIAN_POINT('Ctrl Pts',(37.7407867817177,-6.73773732621305,-11.4372107088933));
#63387=CARTESIAN_POINT('Ctrl Pts',(37.7412077086163,-6.73778237600391,-11.4375318475774));
#63388=CARTESIAN_POINT('Ctrl Pts',(37.7414225413037,-6.73780536314421,-11.4376956930943));
#63389=CARTESIAN_POINT('Ctrl Pts',(37.7418623574362,-6.73785241255197,-11.438031008572));
#63390=CARTESIAN_POINT('Ctrl Pts',(37.7420873435587,-6.73787647458877,-11.4382024750684));
#63391=CARTESIAN_POINT('Ctrl Pts',(37.7425491346872,-6.73792585057906,-11.4385542867136));
#63392=CARTESIAN_POINT('Ctrl Pts',(37.7427859429672,-6.73795116425038,-11.4387346276292));
#63393=CARTESIAN_POINT('Ctrl Pts',(37.7432733654522,-6.73800325393794,-11.4391056804099));
#63394=CARTESIAN_POINT('Ctrl Pts',(37.7435239836945,-6.73803002960599,-11.4392963870586));
#63395=CARTESIAN_POINT('Ctrl Pts',(37.7524331798043,-6.73898161442979,-11.4460730311482));
#63396=CARTESIAN_POINT('Ctrl Pts',(37.761136422089,-6.73990242395748,-11.4526002992707));
#63397=CARTESIAN_POINT('Ctrl Pts',(37.7803585487991,-6.74191682629841,-11.4668137890099));
#63398=CARTESIAN_POINT('Ctrl Pts',(37.7908959667028,-6.74300869093637,-11.4744739005115));
#63399=CARTESIAN_POINT('Ctrl Pts',(37.8222640585244,-6.74622421569818,-11.4968895038783));
#63400=CARTESIAN_POINT('Ctrl Pts',(37.8432688417769,-6.74833256294983,-11.5114000762294));
#63401=CARTESIAN_POINT('Ctrl Pts',(37.9641873841679,-6.76024257099755,-11.592120135349));
#63402=CARTESIAN_POINT('Ctrl Pts',(38.0687224461405,-6.76967388898407,-11.6511321611206));
#63403=CARTESIAN_POINT('Ctrl Pts',(38.2873834282866,-6.7886158749594,-11.7538548467886));
#63404=CARTESIAN_POINT('Ctrl Pts',(38.401292479853,-6.79810090833219,-11.7971634779365));
#63405=CARTESIAN_POINT('Ctrl Pts',(38.5849579538793,-6.81337050174021,-11.8514680719438));
#63406=CARTESIAN_POINT('Ctrl Pts',(38.6527548206729,-6.81899987655743,-11.8683419358709));
#63407=CARTESIAN_POINT('Ctrl Pts',(38.7477409148245,-6.82694091070454,-11.8876360336061));
#63408=CARTESIAN_POINT('Ctrl Pts',(38.7743858473484,-6.82917411420624,-11.8925809975287));
#63409=CARTESIAN_POINT('Ctrl Pts',(38.8204492586569,-6.83304795322695,-11.9003271057356));
#63410=CARTESIAN_POINT('Ctrl Pts',(38.8398293911233,-6.83468174645656,-11.9033428493689));
#63411=CARTESIAN_POINT('Ctrl Pts',(38.8796740548795,-6.83805014577164,-11.9090449205769));
#63412=CARTESIAN_POINT('Ctrl Pts',(38.9001405480022,-6.83978540982395,-11.9117055006084));
#63413=CARTESIAN_POINT('Ctrl Pts',(38.9528809944916,-6.84427156090478,-11.9178725336195));
#63414=CARTESIAN_POINT('Ctrl Pts',(38.9851951655634,-6.84703421948019,-11.9209894463542));
#63415=CARTESIAN_POINT('Ctrl Pts',(39.154662731107,-6.8616040651487,-11.9338800625799));
#63416=CARTESIAN_POINT('Ctrl Pts',(39.2923794695661,-6.87374447884458,-11.9325321528038));
#63417=CARTESIAN_POINT('Ctrl Pts',(39.5509855063054,-6.89701388041658,-11.9077776026887));
#63418=CARTESIAN_POINT('Ctrl Pts',(39.6717031521427,-6.90806971246242,-11.8868461744628));
#63419=CARTESIAN_POINT('Ctrl Pts',(39.8434288012692,-6.92378020262187,-11.8433733816551));
#63420=CARTESIAN_POINT('Ctrl Pts',(39.8960815563142,-6.9285927737816,-11.8281125587806));
#63421=CARTESIAN_POINT('Ctrl Pts',(39.9645728675133,-6.93481162982387,-11.8056970587235));
#63422=CARTESIAN_POINT('Ctrl Pts',(39.9809162230095,-6.93629238467935,-11.8001528848118));
#63423=CARTESIAN_POINT('Ctrl Pts',(40.0078608141697,-6.93872683237865,-11.7906878746723));
#63424=CARTESIAN_POINT('Ctrl Pts',(40.0184963349342,-6.93968597757649,-11.7868674612639));
#63425=CARTESIAN_POINT('Ctrl Pts',(40.0401935171523,-6.94163854392647,-11.7789004704902));
#63426=CARTESIAN_POINT('Ctrl Pts',(40.0512522462144,-6.94263156257877,-11.7747471211273));
#63427=CARTESIAN_POINT('Ctrl Pts',(40.0806500064579,-6.94526669973878,-11.7634583345894));
#63428=CARTESIAN_POINT('Ctrl Pts',(40.0989333776727,-6.9469007351729,-11.7561788383743));
#63429=CARTESIAN_POINT('Ctrl Pts',(40.1919966226582,-6.95520366280167,-11.7177961031288));
#63430=CARTESIAN_POINT('Ctrl Pts',(40.2652699604614,-6.96169375148389,-11.6831509350186));
#63431=CARTESIAN_POINT('Ctrl Pts',(40.4746208673889,-6.98050300226922,-11.5708979512558));
#63432=CARTESIAN_POINT('Ctrl Pts',(40.6050269756479,-6.9925895708988,-11.4836366796581));
#63433=CARTESIAN_POINT('Ctrl Pts',(40.7885758196115,-7.01143830824701,-11.3329896599929));
#63434=CARTESIAN_POINT('Ctrl Pts',(40.8484831470591,-7.01793395749599,-11.2785394417222));
#63435=CARTESIAN_POINT('Ctrl Pts',(40.9255759232657,-7.02687861515469,-11.2010217535354));
#63436=CARTESIAN_POINT('Ctrl Pts',(40.9452635025684,-7.02921879139036,-11.1805109040702));
#63437=CARTESIAN_POINT('Ctrl Pts',(40.9780695963466,-7.03321897771903,-11.1450973258889));
#63438=CARTESIAN_POINT('Ctrl Pts',(40.9913759229167,-7.03487091201093,-11.1303719469763));
#63439=CARTESIAN_POINT('Ctrl Pts',(41.016334868724,-7.03802746795102,-11.1020545487435));
#63440=CARTESIAN_POINT('Ctrl Pts',(41.0280209943483,-7.03953056551109,-11.0884937199208));
#63441=CARTESIAN_POINT('Ctrl Pts',(41.0550597121541,-7.04306900646214,-11.0563998633379));
#63442=CARTESIAN_POINT('Ctrl Pts',(41.0702873893966,-7.04510917880011,-11.0377647099678));
#63443=CARTESIAN_POINT('Ctrl Pts',(41.1239757211677,-7.0524782179523,-10.9700127558453));
#63444=CARTESIAN_POINT('Ctrl Pts',(41.1607984526013,-7.05786865066967,-10.9196370040375));
#63445=CARTESIAN_POINT('Ctrl Pts',(41.3161643070524,-7.08221193381776,-10.6887539425036));
#63446=CARTESIAN_POINT('Ctrl Pts',(41.4120335234907,-7.1018957366992,-10.4942048998635));
#63447=CARTESIAN_POINT('Ctrl Pts',(41.4966273510425,-7.12545217856426,-10.2418572465852));
#63448=CARTESIAN_POINT('Ctrl Pts',(41.5111126641656,-7.12985987359822,-10.1936858318763));
#63449=CARTESIAN_POINT('Ctrl Pts',(41.528401992268,-7.13564334628572,-10.1288860881664));
#63450=CARTESIAN_POINT('Ctrl Pts',(41.5325562912574,-7.13708166834152,-10.1126354672255));
#63451=CARTESIAN_POINT('Ctrl Pts',(41.5392022018627,-7.13946574671488,-10.0854565825735));
#63452=CARTESIAN_POINT('Ctrl Pts',(41.5417879716383,-7.1404165114773,-10.0745522188296));
#63453=CARTESIAN_POINT('Ctrl Pts',(41.5469762837167,-7.14237306633793,-10.051970937339));
#63454=CARTESIAN_POINT('Ctrl Pts',(41.5495680853971,-7.14337826812535,-10.0402920302354));
#63455=CARTESIAN_POINT('Ctrl Pts',(41.5563388034762,-7.14608318061396,-10.0086688871477));
#63456=CARTESIAN_POINT('Ctrl Pts',(41.5603517338086,-7.14777404456037,-9.98868947203034));
#63457=CARTESIAN_POINT('Ctrl Pts',(41.5834156080898,-7.15807825410333,-9.86579020240314));
#63458=CARTESIAN_POINT('Ctrl Pts',(41.5959888290629,-7.16638815582971,-9.76175328351839));
#63459=CARTESIAN_POINT('Ctrl Pts',(41.609303289201,-7.1854464791118,-9.51988788413041));
#63460=CARTESIAN_POINT('Ctrl Pts',(41.6050711605563,-7.19611602353937,-9.38217148976502));
#63461=CARTESIAN_POINT('Ctrl Pts',(41.5802468024443,-7.21310905505812,-9.16992358403679));
#63462=CARTESIAN_POINT('Ctrl Pts',(41.5678117207838,-7.21923401000237,-9.09474469183967));
#63463=CARTESIAN_POINT('Ctrl Pts',(41.5459815571247,-7.2277507799812,-8.99302141375947));
#63464=CARTESIAN_POINT('Ctrl Pts',(41.5396564342281,-7.23004741377237,-8.96585930089216));
#63465=CARTESIAN_POINT('Ctrl Pts',(41.5280479998318,-7.23399592570049,-8.91966085858103));
#63466=CARTESIAN_POINT('Ctrl Pts',(41.5229996769323,-7.23564023579455,-8.90056792375326));
#63467=CARTESIAN_POINT('Ctrl Pts',(41.5122581110401,-7.23899905865904,-8.86187724229014));
#63468=CARTESIAN_POINT('Ctrl Pts',(41.5065494230994,-7.24071394413184,-8.84228551521467));
#63469=CARTESIAN_POINT('Ctrl Pts',(41.491449594579,-7.24508129875793,-8.79281664961974));
#63470=CARTESIAN_POINT('Ctrl Pts',(41.4817232373491,-7.24774434467291,-8.76304686987602));
#63471=CARTESIAN_POINT('Ctrl Pts',(41.4368783200271,-7.2594152058107,-8.63435625015533));
#63472=CARTESIAN_POINT('Ctrl Pts',(41.3958923154472,-7.26860837135119,-8.53761894578032));
#63473=CARTESIAN_POINT('Ctrl Pts',(41.2825107275651,-7.29104467985914,-8.31227283041029));
#63474=CARTESIAN_POINT('Ctrl Pts',(41.2043462575023,-7.30439011615891,-8.18703455269513));
#63475=CARTESIAN_POINT('Ctrl Pts',(41.0770538417761,-7.32311044022609,-8.01950967201676));
#63476=CARTESIAN_POINT('Ctrl Pts',(41.036923703605,-7.32866877645552,-7.9707975292015));
#63477=CARTESIAN_POINT('Ctrl Pts',(40.9829175125755,-7.33567673440827,-7.91026064983037));
#63478=CARTESIAN_POINT('Ctrl Pts',(40.9707633029699,-7.3372251856827,-7.89694121401002));
#63479=CARTESIAN_POINT('Ctrl Pts',(40.9506412288704,-7.33974066313203,-7.87538200183495));
#63480=CARTESIAN_POINT('Ctrl Pts',(40.9427624964945,-7.34071385987671,-7.86706057043653));
#63481=CARTESIAN_POINT('Ctrl Pts',(40.9277557464838,-7.34254499472489,-7.85143579324031));
#63482=CARTESIAN_POINT('Ctrl Pts',(40.9206402192662,-7.34340387044973,-7.84412096759225));
#63483=CARTESIAN_POINT('Ctrl Pts',(40.901282556124,-7.34571604528823,-7.82447285515044));
#63484=CARTESIAN_POINT('Ctrl Pts',(40.8889526347475,-7.34716280630934,-7.81222623854819));
#63485=CARTESIAN_POINT('Ctrl Pts',(40.839475904814,-7.35287180796252,-7.76413769347751));
#63486=CARTESIAN_POINT('Ctrl Pts',(40.8013090479579,-7.35706377639324,-7.72935868942916));
#63487=CARTESIAN_POINT('Ctrl Pts',(40.6607940735945,-7.37189143919899,-7.60936359430232));
#63488=CARTESIAN_POINT('Ctrl Pts',(40.5525263257329,-7.38223228760084,-7.53144522605973));
#63489=CARTESIAN_POINT('Ctrl Pts',(40.3636713449649,-7.39951503978045,-7.41803260097788));
#63490=CARTESIAN_POINT('Ctrl Pts',(40.2866090963879,-7.40637994508828,-7.37727530010874));
#63491=CARTESIAN_POINT('Ctrl Pts',(40.1544738549429,-7.41804344883372,-7.31632528217816));
#63492=CARTESIAN_POINT('Ctrl Pts',(40.1005680473364,-7.42277280644113,-7.29380290118905));
#63493=CARTESIAN_POINT('Ctrl Pts',(40.0220655853351,-7.42965597334912,-7.26431219118926));
#63494=CARTESIAN_POINT('Ctrl Pts',(39.9980914436809,-7.43175739982458,-7.25573775377028));
#63495=CARTESIAN_POINT('Ctrl Pts',(39.9556489513511,-7.43547934972116,-7.24131378795487));
#63496=CARTESIAN_POINT('Ctrl Pts',(39.9372372553629,-7.43709449387007,-7.23530368043308));
#63497=CARTESIAN_POINT('Ctrl Pts',(39.8984453192548,-7.44049985045436,-7.22315725364914));
#63498=CARTESIAN_POINT('Ctrl Pts',(39.8780523027481,-7.44229142140527,-7.21706782915396));
#63499=CARTESIAN_POINT('Ctrl Pts',(39.8233393019105,-7.44710339623546,-7.20151806061534));
#63500=CARTESIAN_POINT('Ctrl Pts',(39.788886984732,-7.45013907017388,-7.19254806340412));
#63501=CARTESIAN_POINT('Ctrl Pts',(39.5724500673931,-7.46925690701238,-7.14129733218012));
#63502=CARTESIAN_POINT('Ctrl Pts',(39.386289774908,-7.48598117123899,-7.11958440573875));
#63503=CARTESIAN_POINT('Ctrl Pts',(39.084101005368,-7.5131316433615,-7.1196420736939));
#63504=CARTESIAN_POINT('Ctrl Pts',(38.9687974283207,-7.52347149521631,-7.12797446899214));
#63505=CARTESIAN_POINT('Ctrl Pts',(38.8342146259304,-7.53525485945145,-7.14750652346068));
#63506=CARTESIAN_POINT('Ctrl Pts',(38.8139411176832,-7.53702193602859,-7.15071425548855));
#63507=CARTESIAN_POINT('Ctrl Pts',(38.7818884797256,-7.53980063131737,-7.15620715199266));
#63508=CARTESIAN_POINT('Ctrl Pts',(38.7700817420961,-7.54082092028483,-7.15832150238878));
#63509=CARTESIAN_POINT('Ctrl Pts',(38.7474207796818,-7.54277231434138,-7.16255480967862));
#63510=CARTESIAN_POINT('Ctrl Pts',(38.7365646370478,-7.54370405939397,-7.16466042679972));
#63511=CARTESIAN_POINT('Ctrl Pts',(38.7121176425693,-7.54579599692027,-7.16957724655369));
#63512=CARTESIAN_POINT('Ctrl Pts',(38.6985355659258,-7.54695385491767,-7.17243140553701));
#63513=CARTESIAN_POINT('Ctrl Pts',(38.6495097132471,-7.55112004207163,-7.18317766153988));
#63514=CARTESIAN_POINT('Ctrl Pts',(38.6142187403869,-7.55409399807666,-7.19175501664385));
#63515=CARTESIAN_POINT('Ctrl Pts',(38.3306292569215,-7.57789191888648,-7.26752144154939));
#63516=CARTESIAN_POINT('Ctrl Pts',(38.0943662873774,-7.59726436997668,-7.37334475882706));
#63517=CARTESIAN_POINT('Ctrl Pts',(37.8399552926992,-7.62181673862617,-7.54047206003717));
#63518=CARTESIAN_POINT('Ctrl Pts',(37.8013484148333,-7.62565114144592,-7.56748986856382));
#63519=CARTESIAN_POINT('Ctrl Pts',(37.7446781114511,-7.63146445660931,-7.60968138054314));
#63520=CARTESIAN_POINT('Ctrl Pts',(37.7260022544897,-7.63341165048591,-7.6240166284239));
#63521=CARTESIAN_POINT('Ctrl Pts',(37.693946787916,-7.6368110863648,-7.64937820288367));
#63522=CARTESIAN_POINT('Ctrl Pts',(37.6804701345545,-7.6382583443645,-7.66027954958062));
#63523=CARTESIAN_POINT('Ctrl Pts',(37.650317950409,-7.64153847116682,-7.68521374962079));
#63524=CARTESIAN_POINT('Ctrl Pts',(37.6337131969188,-7.64337457300378,-7.69932930534523));
#63525=CARTESIAN_POINT('Ctrl Pts',(37.5893616877527,-7.64836189819676,-7.73808255289733));
#63526=CARTESIAN_POINT('Ctrl Pts',(37.5619906890326,-7.65153001601184,-7.76313879533985));
#63527=CARTESIAN_POINT('Ctrl Pts',(37.4128868552171,-7.66931288530945,-7.90611119976877));
#63528=CARTESIAN_POINT('Ctrl Pts',(37.3033244738866,-7.684438800844,-8.03598223007141));
#63529=CARTESIAN_POINT('Ctrl Pts',(37.1360743121515,-7.71124531933222,-8.28295695108838));
#63530=CARTESIAN_POINT('Ctrl Pts',(37.072497836211,-7.72282786446461,-8.39530858016603));
#63531=CARTESIAN_POINT('Ctrl Pts',(37.0095099486189,-7.7357927206205,-8.53100064399404));
#63532=CARTESIAN_POINT('Ctrl Pts',(37.0010370610652,-7.73757515561057,-8.54988797231634));
#63533=CARTESIAN_POINT('Ctrl Pts',(36.9880262531494,-7.74037230706476,-8.57992336701947));
#63534=CARTESIAN_POINT('Ctrl Pts',(36.9833266177378,-7.7413958809209,-8.59099955306472));
#63535=CARTESIAN_POINT('Ctrl Pts',(36.9744746554689,-7.74334900692064,-8.61230522698373));
#63536=CARTESIAN_POINT('Ctrl Pts',(36.9703093571092,-7.74427924014572,-8.62252869679819));
#63537=CARTESIAN_POINT('Ctrl Pts',(36.9634507368028,-7.74583057432999,-8.63970013303504));
#63538=CARTESIAN_POINT('Ctrl Pts',(36.9607191031609,-7.74645386404971,-8.64663246328934));
#63539=CARTESIAN_POINT('Ctrl Pts',(36.9580196848653,-7.74707540691374,-8.65357747851663));
#63540=CARTESIAN_POINT('Origin',(39.2,8.05522481984854,-9.525));
#63541=CARTESIAN_POINT('',(36.958019684865,-9.28019056162069,-8.65357747851727));
#63542=CARTESIAN_POINT('',(36.9580196445751,-9.01353011641035,-8.65357758217454));
#63543=CARTESIAN_POINT('',(36.958019684865,8.05522481984854,-8.65357747851728));
#63544=CARTESIAN_POINT('',(36.7946209480143,-8.08522481984856,-9.52713557209757));
#63545=CARTESIAN_POINT('Ctrl Pts',(36.7946209480143,-8.08522481984856,-9.52713557209757));
#63546=CARTESIAN_POINT('Ctrl Pts',(36.7947125349209,-8.09388971051084,-9.63029351600966));
#63547=CARTESIAN_POINT('Ctrl Pts',(36.8014440163763,-8.10255460117313,-9.73316083263825));
#63548=CARTESIAN_POINT('Ctrl Pts',(36.8146812005732,-8.11121949183542,-9.83501156349611));
#63549=CARTESIAN_POINT('Ctrl Pts',(36.8273339973927,-8.11950185003041,-9.93236584853728));
#63550=CARTESIAN_POINT('Ctrl Pts',(36.8459303117105,-8.12778420822541,-10.0287917844142));
#63551=CARTESIAN_POINT('Ctrl Pts',(36.8703130343641,-8.1360665664204,-10.1236748587891));
#63552=CARTESIAN_POINT('Ctrl Pts',(36.890192917571,-8.14281939365521,-10.2010355565127));
#63553=CARTESIAN_POINT('Ctrl Pts',(36.9139671233725,-8.14957222089002,-10.2775483060069));
#63554=CARTESIAN_POINT('Ctrl Pts',(36.9415464626432,-8.15632504812483,-10.3527925851326));
#63555=CARTESIAN_POINT('Ctrl Pts',(36.969086513572,-8.16306825557206,-10.4279296744907));
#63556=CARTESIAN_POINT('Ctrl Pts',(37.0004207730383,-8.16981146301929,-10.5018014480561));
#63557=CARTESIAN_POINT('Ctrl Pts',(37.0354096749355,-8.17655467046653,-10.5740003188927));
#63558=CARTESIAN_POINT('Ctrl Pts',(37.0703585153005,-8.1832901570878,-10.6461165235915));
#63559=CARTESIAN_POINT('Ctrl Pts',(37.1089534794919,-8.19002564370908,-10.7165632147592));
#63560=CARTESIAN_POINT('Ctrl Pts',(37.1510066430008,-8.19676113033035,-10.7849520496325));
#63561=CARTESIAN_POINT('Ctrl Pts',(37.1930334705739,-8.20349239883036,-10.8532980557668));
#63562=CARTESIAN_POINT('Ctrl Pts',(37.2385139547638,-8.21022366733036,-10.9195883676319));
#63563=CARTESIAN_POINT('Ctrl Pts',(37.2872144678815,-8.21695493583037,-10.983459616348));
#63564=CARTESIAN_POINT('Ctrl Pts',(37.3358994818713,-8.22368406207796,-11.0473105377906));
#63565=CARTESIAN_POINT('Ctrl Pts',(37.3878022070609,-8.23041318832557,-11.1087435544642));
#63566=CARTESIAN_POINT('Ctrl Pts',(37.44264680587,-8.23714231457317,-11.1674258569205));
#63567=CARTESIAN_POINT('Ctrl Pts',(37.4974908418339,-8.2438713717628,-11.2261075571471));
#63568=CARTESIAN_POINT('Ctrl Pts',(37.555276371965,-8.25060042895244,-11.2820382595347));
#63569=CARTESIAN_POINT('Ctrl Pts',(37.6156895375635,-8.25732948614207,-11.3349208002048));
#63570=CARTESIAN_POINT('Ctrl Pts',(37.676162183044,-8.26406516843609,-11.3878554064679));
#63571=CARTESIAN_POINT('Ctrl Pts',(37.7392672801181,-8.27080085073012,-11.4377355482707));
#63572=CARTESIAN_POINT('Ctrl Pts',(37.8046570358675,-8.27753653302414,-11.484303691837));
#63573=CARTESIAN_POINT('Ctrl Pts',(37.8700780195631,-8.28427543205327,-11.530894074781));
#63574=CARTESIAN_POINT('Ctrl Pts',(37.9377854422335,-8.29101433108241,-11.5741690568134));
#63575=CARTESIAN_POINT('Ctrl Pts',(38.007403729675,-8.29775323011155,-11.6139152879921));
#63576=CARTESIAN_POINT('Ctrl Pts',(38.0771462831552,-8.30450415782335,-11.6537324647064));
#63577=CARTESIAN_POINT('Ctrl Pts',(38.1488060997928,-8.31125508553515,-11.6900080934659));
#63578=CARTESIAN_POINT('Ctrl Pts',(38.2219844649816,-8.31800601324695,-11.722575609089));
#63579=CARTESIAN_POINT('Ctrl Pts',(38.2894306676579,-8.3242281314581,-11.7525920661895));
#63580=CARTESIAN_POINT('Ctrl Pts',(38.3581663381352,-8.33045024966925,-11.7794590313155));
#63581=CARTESIAN_POINT('Ctrl Pts',(38.427868318026,-8.3366723678804,-11.8030837583575));
#63582=CARTESIAN_POINT('Ctrl Pts',(38.5035154551363,-8.34342519513398,-11.8287235316973));
#63583=CARTESIAN_POINT('Ctrl Pts',(38.5805812464378,-8.35017802238755,-11.8506387668023));
#63584=CARTESIAN_POINT('Ctrl Pts',(38.6586648020085,-8.35693084964113,-11.8686742836443));
#63585=CARTESIAN_POINT('Ctrl Pts',(38.7366371230947,-8.36367405710662,-11.8866841078624));
#63586=CARTESIAN_POINT('Ctrl Pts',(38.8156238782593,-8.3704172645721,-11.9008250865046));
#63587=CARTESIAN_POINT('Ctrl Pts',(38.8952074722694,-8.37716047203758,-11.9109912949212));
#63588=CARTESIAN_POINT('Ctrl Pts',(38.9746999447843,-8.38389595867624,-11.9211458632488));
#63589=CARTESIAN_POINT('Ctrl Pts',(39.0547874377658,-8.39063144531491,-11.9273346472732));
#63590=CARTESIAN_POINT('Ctrl Pts',(39.1350420370788,-8.39736693195357,-11.9295027360045));
#63591=CARTESIAN_POINT('Ctrl Pts',(39.2152463766714,-8.40409820047043,-11.9316694669628));
#63592=CARTESIAN_POINT('Ctrl Pts',(39.2956171499091,-8.41082946898729,-11.9298204884061));
#63593=CARTESIAN_POINT('Ctrl Pts',(39.3757223731024,-8.41756073750415,-11.9239528115391));
#63594=CARTESIAN_POINT('Ctrl Pts',(39.45580210249,-8.42428986376805,-11.9180870020835));
#63595=CARTESIAN_POINT('Ctrl Pts',(39.535615984925,-8.43101899003195,-11.908205068333));
#63596=CARTESIAN_POINT('Ctrl Pts',(39.6147345538958,-8.43774811629586,-11.8943560716374));
#63597=CARTESIAN_POINT('Ctrl Pts',(39.6938523109022,-8.44447717350124,-11.8805072170688));
#63598=CARTESIAN_POINT('Ctrl Pts',(39.7722743095289,-8.45120623070661,-11.862691462269));
#63599=CARTESIAN_POINT('Ctrl Pts',(39.849580149142,-8.45793528791199,-11.8410091913118));
#63600=CARTESIAN_POINT('Ctrl Pts',(39.9269621003357,-8.46467097022075,-11.8193055730421));
#63601=CARTESIAN_POINT('Ctrl Pts',(40.0032252473015,-8.47140665252953,-11.793727960483));
#63602=CARTESIAN_POINT('Ctrl Pts',(40.0779638258342,-8.47814233483829,-11.7644268161578));
#63603=CARTESIAN_POINT('Ctrl Pts',(40.1527380969901,-8.48488123388166,-11.7351116785947));
#63604=CARTESIAN_POINT('Ctrl Pts',(40.2259859235215,-8.49162013292502,-11.7020696585099));
#63605=CARTESIAN_POINT('Ctrl Pts',(40.2973233541722,-8.49835903196838,-11.6654986336806));
#63606=CARTESIAN_POINT('Ctrl Pts',(40.3687881194565,-8.50510995969337,-11.6288623309458));
#63607=CARTESIAN_POINT('Ctrl Pts',(40.438335270284,-8.51186088741837,-11.5886846704396));
#63608=CARTESIAN_POINT('Ctrl Pts',(40.5056073831098,-8.51861181514336,-11.5452084807191));
#63609=CARTESIAN_POINT('Ctrl Pts',(40.5676099767651,-8.52483393320903,-11.5051378420593));
#63610=CARTESIAN_POINT('Ctrl Pts',(40.6276800916756,-8.5310560512747,-11.4622658551984));
#63611=CARTESIAN_POINT('Ctrl Pts',(40.6855634194983,-8.53727816934038,-11.4168124301972));
#63612=CARTESIAN_POINT('Ctrl Pts',(40.7483838482196,-8.54403099678038,-11.3674821005007));
#63613=CARTESIAN_POINT('Ctrl Pts',(40.808860880547,-8.55078382422039,-11.3149279128816));
#63614=CARTESIAN_POINT('Ctrl Pts',(40.8666454375787,-8.5575366516604,-11.2594007408318));
#63615=CARTESIAN_POINT('Ctrl Pts',(40.9243476772194,-8.56427985931329,-11.2039526703997));
#63616=CARTESIAN_POINT('Ctrl Pts',(40.9793647258058,-8.57102306696619,-11.1455403473925));
#63617=CARTESIAN_POINT('Ctrl Pts',(41.0313796185417,-8.57776627461908,-11.08445555794));
#63618=CARTESIAN_POINT('Ctrl Pts',(41.0833349553559,-8.58450176144576,-11.0234407092439));
#63619=CARTESIAN_POINT('Ctrl Pts',(41.1322946670043,-8.59123724827243,-10.959759828654));
#63620=CARTESIAN_POINT('Ctrl Pts',(41.1779788660801,-8.59797273509911,-10.8937412281876));
#63621=CARTESIAN_POINT('Ctrl Pts',(41.2236344552709,-8.60470400380426,-10.8277639720941));
#63622=CARTESIAN_POINT('Ctrl Pts',(41.2660183391843,-8.61143527250941,-10.7594522847394));
#63623=CARTESIAN_POINT('Ctrl Pts',(41.3048918846036,-8.61816654121456,-10.6891662675623));
#63624=CARTESIAN_POINT('Ctrl Pts',(41.3437530583631,-8.62489566766676,-10.6189026191887));
#63625=CARTESIAN_POINT('Ctrl Pts',(41.379105886766,-8.63162479411896,-10.5466662966233));
#63626=CARTESIAN_POINT('Ctrl Pts',(41.410756698362,-8.63835392057116,-10.4728437450591));
#63627=CARTESIAN_POINT('Ctrl Pts',(41.4424071851363,-8.64508297796458,-10.399021951111));
#63628=CARTESIAN_POINT('Ctrl Pts',(41.4703555481585,-8.651812035358,-10.3236143896706));
#63629=CARTESIAN_POINT('Ctrl Pts',(41.4944560482581,-8.65854109275142,-10.2470279683032));
#63630=CARTESIAN_POINT('Ctrl Pts',(41.5185802765345,-8.66527677524652,-10.170366143681));
#63631=CARTESIAN_POINT('Ctrl Pts',(41.5388489339166,-8.67201245774162,-10.0925235864974));
#63632=CARTESIAN_POINT('Ctrl Pts',(41.5551662165498,-8.67874814023672,-10.0139223218698));
#63633=CARTESIAN_POINT('Ctrl Pts',(41.5714912917648,-8.68548703946577,-9.93528351993889));
#63634=CARTESIAN_POINT('Ctrl Pts',(41.5838611608091,-8.69222593869483,-9.85588575006578));
#63635=CARTESIAN_POINT('Ctrl Pts',(41.5922316478546,-8.69896483792388,-9.77615868968205));
#63636=CARTESIAN_POINT('Ctrl Pts',(41.6006170759006,-8.7057157658313,-9.69628931953318));
#63637=CARTESIAN_POINT('Ctrl Pts',(41.6049888319449,-8.71246669373873,-9.61608995117826));
#63638=CARTESIAN_POINT('Ctrl Pts',(41.6053548816596,-8.71921762164615,-9.53599261918044));
#63639=CARTESIAN_POINT('Ctrl Pts',(41.6056922580852,-8.72543973803089,-9.46216944573941));
#63640=CARTESIAN_POINT('Ctrl Pts',(41.6026275097846,-8.73166185441563,-9.38843322435266));
#63641=CARTESIAN_POINT('Ctrl Pts',(41.5962057755786,-8.73788397080037,-9.3151171148383));
#63642=CARTESIAN_POINT('Ctrl Pts',(41.589236304541,-8.7446367977696,-9.23554756470546));
#63643=CARTESIAN_POINT('Ctrl Pts',(41.5782862902815,-8.75138962473884,-9.15617810952552));
#63644=CARTESIAN_POINT('Ctrl Pts',(41.5633749964623,-8.75814245170807,-9.07743819365742));
#63645=CARTESIAN_POINT('Ctrl Pts',(41.5484849446318,-8.76488565889009,-8.99881044729108));
#63646=CARTESIAN_POINT('Ctrl Pts',(41.5296449068395,-8.7716288660721,-8.92081091354556));
#63647=CARTESIAN_POINT('Ctrl Pts',(41.5069259604112,-8.77837207325411,-8.84386450864681));
#63648=CARTESIAN_POINT('Ctrl Pts',(41.4842330266779,-8.78510755961192,-8.7670062056926));
#63649=CARTESIAN_POINT('Ctrl Pts',(41.4576701422759,-8.79184304596973,-8.69119908015933));
#63650=CARTESIAN_POINT('Ctrl Pts',(41.4273592378361,-8.79857853232755,-8.61685696609709));
#63651=CARTESIAN_POINT('Ctrl Pts',(41.397067315698,-8.80530980056528,-8.54256140902384));
#63652=CARTESIAN_POINT('Ctrl Pts',(41.3630322084855,-8.812041068803,-8.46972947288336));
#63653=CARTESIAN_POINT('Ctrl Pts',(41.3254250170237,-8.81877233704073,-8.39875782293064));
#63654=CARTESIAN_POINT('Ctrl Pts',(41.2878297941888,-8.8255014630276,-8.32780875996649));
#63655=CARTESIAN_POINT('Ctrl Pts',(41.2466649629836,-8.83223058901446,-8.25871921917403));
#63656=CARTESIAN_POINT('Ctrl Pts',(41.2021482609573,-8.83895971500133,-8.19186261565221));
#63657=CARTESIAN_POINT('Ctrl Pts',(41.1576320157731,-8.84568877193213,-8.12500669823043));
#63658=CARTESIAN_POINT('Ctrl Pts',(41.109764227764,-8.85241782886293,-8.06038405990319));
#63659=CARTESIAN_POINT('Ctrl Pts',(41.0588059699817,-8.85914688579374,-7.99833916328465));
#63660=CARTESIAN_POINT('Ctrl Pts',(41.0077975411245,-8.86588256783368,-7.93623318021433));
#63661=CARTESIAN_POINT('Ctrl Pts',(40.9536928610552,-8.87261824987363,-7.87671036975368));
#63662=CARTESIAN_POINT('Ctrl Pts',(40.8967929575717,-8.87935393191357,-7.82008164314675));
#63663=CARTESIAN_POINT('Ctrl Pts',(40.83986588059,-8.88609283069084,-7.76342587254676));
#63664=CARTESIAN_POINT('Ctrl Pts',(40.7801412677275,-8.8928317294681,-7.70966725177175));
#63665=CARTESIAN_POINT('Ctrl Pts',(40.7179547755422,-8.89957062824536,-7.65907764260981));
#63666=CARTESIAN_POINT('Ctrl Pts',(40.6556572827293,-8.90632155571193,-7.60839773283484));
#63667=CARTESIAN_POINT('Ctrl Pts',(40.5908895067894,-8.9130724831785,-7.5608984140266));
#63668=CARTESIAN_POINT('Ctrl Pts',(40.5240175796269,-8.91982341064507,-7.51680917409751));
#63669=CARTESIAN_POINT('Ctrl Pts',(40.4623837976759,-8.9260455311835,-7.47617348860916));
#63670=CARTESIAN_POINT('Ctrl Pts',(40.3989631596466,-8.93226765172192,-7.43843421289083));
#63671=CARTESIAN_POINT('Ctrl Pts',(40.3340593217838,-8.93848977226034,-7.40373566025466));
#63672=CARTESIAN_POINT('Ctrl Pts',(40.2636196054445,-8.94524259952276,-7.36607754502513));
#63673=CARTESIAN_POINT('Ctrl Pts',(40.191171604636,-8.95199542678518,-7.33186203898538));
#63674=CARTESIAN_POINT('Ctrl Pts',(40.1170854580263,-8.9587482540476,-7.30130775351517));
#63675=CARTESIAN_POINT('Ctrl Pts',(40.0431048513928,-8.96549146151925,-7.27079699438167));
#63676=CARTESIAN_POINT('Ctrl Pts',(39.9674911613073,-8.97223466899091,-7.24393727356921));
#63677=CARTESIAN_POINT('Ctrl Pts',(39.8906390569906,-8.97897787646257,-7.22090133949106));
#63678=CARTESIAN_POINT('Ctrl Pts',(39.8138749467179,-8.98571336310341,-7.19789178107321));
#63679=CARTESIAN_POINT('Ctrl Pts',(39.7358756847227,-8.99244884974427,-7.1786974414596));
#63680=CARTESIAN_POINT('Ctrl Pts',(39.6570544575941,-8.99918433638512,-7.16344242771993));
#63681=CARTESIAN_POINT('Ctrl Pts',(39.5782825925599,-9.00591560490174,-7.14819696749085));
#63682=CARTESIAN_POINT('Ctrl Pts',(39.4986902408647,-9.01264687341836,-7.13688602432732));
#63683=CARTESIAN_POINT('Ctrl Pts',(39.4187030896245,-9.01937814193498,-7.12958314630028));
#63684=CARTESIAN_POINT('Ctrl Pts',(39.3387413946417,-9.02610726819624,-7.1222825924458));
#63685=CARTESIAN_POINT('Ctrl Pts',(39.2583856137036,-9.03283639445751,-7.11898761284158));
#63686=CARTESIAN_POINT('Ctrl Pts',(39.1780674571923,-9.03956552071877,-7.11971999385394));
#63687=CARTESIAN_POINT('Ctrl Pts',(39.0977501249847,-9.04629457791913,-7.1204523673499));
#63688=CARTESIAN_POINT('Ctrl Pts',(39.0174708827296,-9.05302363511949,-7.12521201364624));
#63689=CARTESIAN_POINT('Ctrl Pts',(38.9376608845403,-9.05975269231985,-7.13396860478583));
#63690=CARTESIAN_POINT('Ctrl Pts',(38.8577723093407,-9.06648837461994,-7.14273381723563));
#63691=CARTESIAN_POINT('Ctrl Pts',(38.7783543656978,-9.07322405692002,-7.15550378442089));
#63692=CARTESIAN_POINT('Ctrl Pts',(38.6998319524494,-9.07995973922011,-7.17219638120615));
#63693=CARTESIAN_POINT('Ctrl Pts',(38.6212720395694,-9.08669863825278,-7.1888969498074));
#63694=CARTESIAN_POINT('Ctrl Pts',(38.5436089604323,-9.09343753728544,-7.2095237603379));
#63695=CARTESIAN_POINT('Ctrl Pts',(38.4672538433217,-9.10017643631811,-7.23394434500747));
#63696=CARTESIAN_POINT('Ctrl Pts',(38.3907624352322,-9.10692736402916,-7.25840851949158));
#63697=CARTESIAN_POINT('Ctrl Pts',(38.3155840918235,-9.11367829174021,-7.28667983478684));
#63698=CARTESIAN_POINT('Ctrl Pts',(38.2421111166827,-9.12042921945127,-7.31857714124942));
#63699=CARTESIAN_POINT('Ctrl Pts',(38.1743933825736,-9.12665133754095,-7.34797588702892));
#63700=CARTESIAN_POINT('Ctrl Pts',(38.1081243179802,-9.13287345563064,-7.38045414295515));
#63701=CARTESIAN_POINT('Ctrl Pts',(38.043590752109,-9.13909557372032,-7.41583651752828));
#63702=CARTESIAN_POINT('Ctrl Pts',(37.9735684441467,-9.14584689860331,-7.45422825205204));
#63703=CARTESIAN_POINT('Ctrl Pts',(37.9053303526129,-9.15259822348629,-7.49618189473797));
#63704=CARTESIAN_POINT('Ctrl Pts',(37.8392616084537,-9.15934954836928,-7.54150712777384));
#63705=CARTESIAN_POINT('Ctrl Pts',(37.7732801318622,-9.16609195569664,-7.58677249251809));
#63706=CARTESIAN_POINT('Ctrl Pts',(37.7094626957699,-9.17283436302401,-7.63540034608263));
#63707=CARTESIAN_POINT('Ctrl Pts',(37.6481695692668,-9.17957677035136,-7.68715472396333));
#63708=CARTESIAN_POINT('Ctrl Pts',(37.5869385168687,-9.18631234936168,-7.73885668802749));
#63709=CARTESIAN_POINT('Ctrl Pts',(37.5282270519293,-9.19304792837199,-7.79367858954149));
#63710=CARTESIAN_POINT('Ctrl Pts',(37.4723649792722,-9.1997835073823,-7.85134227526805));
#63711=CARTESIAN_POINT('Ctrl Pts',(37.4165349163425,-9.20651522681425,-7.90897291891853));
#63712=CARTESIAN_POINT('Ctrl Pts',(37.3635513307144,-9.21324694624619,-7.96944178262451));
#63713=CARTESIAN_POINT('Ctrl Pts',(37.3137085688905,-9.21997866567814,-8.03243255384461));
#63714=CARTESIAN_POINT('Ctrl Pts',(37.2638848573161,-9.22670781220019,-8.09539924955469));
#63715=CARTESIAN_POINT('Ctrl Pts',(37.2171998715998,-9.23343695872224,-8.16088557055856));
#63716=CARTESIAN_POINT('Ctrl Pts',(37.1739078494426,-9.24016610524428,-8.22854192437635));
#63717=CARTESIAN_POINT('Ctrl Pts',(37.1305984247999,-9.24689795674221,-8.29622547463044));
#63718=CARTESIAN_POINT('Ctrl Pts',(37.0906849460329,-9.25362980824013,-8.36608041073893));
#63719=CARTESIAN_POINT('Ctrl Pts',(37.0543779583574,-9.26036165973806,-8.4377286452695));
#63720=CARTESIAN_POINT('Ctrl Pts',(37.0187301282128,-9.26697129369893,-8.50807609787391));
#63721=CARTESIAN_POINT('Ctrl Pts',(36.9865590682883,-9.27358092765981,-8.58015186205256));
#63722=CARTESIAN_POINT('Ctrl Pts',(36.958019684865,-9.28019056162069,-8.65357747851727));
#63723=CARTESIAN_POINT('Ctrl Pts',(36.960685369651,-8.0104155729454,-8.65458630036363));
#63724=CARTESIAN_POINT('Ctrl Pts',(36.8546210246965,-8.03535198857979,-8.93261473925435));
#63725=CARTESIAN_POINT('Ctrl Pts',(36.7977097135442,-8.06028840421417,-9.23031464669973));
#63726=CARTESIAN_POINT('Ctrl Pts',(36.7950831462415,-8.08522481984856,-9.52713516174327));
#63727=CARTESIAN_POINT('Ctrl Pts',(36.9580196848653,-7.74707540691374,-8.65357747851663));
#63728=CARTESIAN_POINT('Ctrl Pts',(36.9557192832498,-7.74760507592088,-8.65949591074869));
#63729=CARTESIAN_POINT('Ctrl Pts',(36.9534422769949,-7.74813347633361,-8.66542355503469));
#63730=CARTESIAN_POINT('Ctrl Pts',(36.9385689284089,-7.75161289183026,-8.70460560453435));
#63731=CARTESIAN_POINT('Ctrl Pts',(36.9266869243085,-7.75452656133757,-8.73812929403557));
#63732=CARTESIAN_POINT('Ctrl Pts',(36.863934925878,-7.77078488506504,-8.92848245261727));
#63733=CARTESIAN_POINT('Ctrl Pts',(36.828545827178,-7.78351852163012,-9.08996910296661));
#63734=CARTESIAN_POINT('Ctrl Pts',(36.8008855876117,-7.80279450956416,-9.33375563665433));
#63735=CARTESIAN_POINT('Ctrl Pts',(36.7958325908309,-7.80915024552102,-9.41408664139223));
#63736=CARTESIAN_POINT('Ctrl Pts',(36.7941109414962,-7.82005563610156,-9.54992027288729));
#63737=CARTESIAN_POINT('Ctrl Pts',(36.7953233986568,-7.82454801430526,-9.6053288116448));
#63738=CARTESIAN_POINT('Ctrl Pts',(36.7998563183302,-7.83114971608571,-9.6855844017261));
#63739=CARTESIAN_POINT('Ctrl Pts',(36.8016535078935,-7.8332126283415,-9.71050215909714));
#63740=CARTESIAN_POINT('Ctrl Pts',(36.8055272614556,-7.83689135166922,-9.75462162839259));
#63741=CARTESIAN_POINT('Ctrl Pts',(36.807447635962,-7.83850220249299,-9.77383514087833));
#63742=CARTESIAN_POINT('Ctrl Pts',(36.8119976958038,-7.84192430919047,-9.81441551111349));
#63743=CARTESIAN_POINT('Ctrl Pts',(36.814683320022,-7.84373716682399,-9.83577421790203));
#63744=CARTESIAN_POINT('Ctrl Pts',(36.8227343084892,-7.84867274740736,-9.89352977171098));
#63745=CARTESIAN_POINT('Ctrl Pts',(36.8286483929567,-7.85181215800447,-9.92984268068579));
#63746=CARTESIAN_POINT('Ctrl Pts',(36.8731323127851,-7.87268663518829,-10.1683600252124));
#63747=CARTESIAN_POINT('Ctrl Pts',(36.936685525334,-7.89121409677273,-10.3649976786444));
#63748=CARTESIAN_POINT('Ctrl Pts',(37.0651256510204,-7.91821393823356,-10.6373188243089));
#63749=CARTESIAN_POINT('Ctrl Pts',(37.110889416959,-7.92670498690201,-10.7210615521798));
#63750=CARTESIAN_POINT('Ctrl Pts',(37.1721034926394,-7.93669016016827,-10.8187878313208));
#63751=CARTESIAN_POINT('Ctrl Pts',(37.1829077053943,-7.93840744430387,-10.8355685605592));
#63752=CARTESIAN_POINT('Ctrl Pts',(37.2004708255962,-7.94112625358973,-10.862115169617));
#63753=CARTESIAN_POINT('Ctrl Pts',(37.2070950324872,-7.94213585262632,-10.8719683386859));
#63754=CARTESIAN_POINT('Ctrl Pts',(37.2200682466042,-7.94408216118704,-10.8909601018931));
#63755=CARTESIAN_POINT('Ctrl Pts',(37.2264081277018,-7.94501937406278,-10.9001043158043));
#63756=CARTESIAN_POINT('Ctrl Pts',(37.2425585166079,-7.94737296096718,-10.923056750464));
#63757=CARTESIAN_POINT('Ctrl Pts',(37.2524521310074,-7.94878393405045,-10.9368063560044));
#63758=CARTESIAN_POINT('Ctrl Pts',(37.2909028501468,-7.95415624462862,-10.9890695589739));
#63759=CARTESIAN_POINT('Ctrl Pts',(37.3204661500628,-7.95805740334165,-11.026833876662));
#63760=CARTESIAN_POINT('Ctrl Pts',(37.4485437095088,-7.97415993082891,-11.1807289991672));
#63761=CARTESIAN_POINT('Ctrl Pts',(37.5568471653784,-7.98593576459318,-11.2882625770026));
#63762=CARTESIAN_POINT('Ctrl Pts',(37.7653106740694,-8.00712926902897,-11.4592396438754));
#63763=CARTESIAN_POINT('Ctrl Pts',(37.8613299674977,-8.01643513006614,-11.5268923508703));
#63764=CARTESIAN_POINT('Ctrl Pts',(37.9887949419618,-8.02856506107532,-11.6034176554755));
#63765=CARTESIAN_POINT('Ctrl Pts',(38.0160108610134,-8.0311422410835,-11.619040873149));
#63766=CARTESIAN_POINT('Ctrl Pts',(38.0614275172243,-8.03542747858772,-11.6439437420481));
#63767=CARTESIAN_POINT('Ctrl Pts',(38.0794553534316,-8.03712454192942,-11.6535322459264));
#63768=CARTESIAN_POINT('Ctrl Pts',(38.1149484540488,-8.04045950887018,-11.6718341741303));
#63769=CARTESIAN_POINT('Ctrl Pts',(38.1324020566718,-8.04209658794781,-11.6805668424024));
#63770=CARTESIAN_POINT('Ctrl Pts',(38.1709689274312,-8.04570888633528,-11.699279952791));
#63771=CARTESIAN_POINT('Ctrl Pts',(38.1921249206493,-8.04768711216782,-11.7091671188801));
#63772=CARTESIAN_POINT('Ctrl Pts',(38.266274625906,-8.05461157351053,-11.7425140140712));
#63773=CARTESIAN_POINT('Ctrl Pts',(38.3199651512337,-8.05961020241652,-11.7643635105122));
#63774=CARTESIAN_POINT('Ctrl Pts',(38.5572104028629,-8.08165218037708,-11.8510615377907));
#63775=CARTESIAN_POINT('Ctrl Pts',(38.7474500407185,-8.09928992575252,-11.8954255131623));
#63776=CARTESIAN_POINT('Ctrl Pts',(38.9905235047393,-8.12111639917068,-11.9217609499181));
#63777=CARTESIAN_POINT('Ctrl Pts',(39.0402970256571,-8.12554394431615,-11.9255914087887));
#63778=CARTESIAN_POINT('Ctrl Pts',(39.1235724894052,-8.13285038807015,-11.9293982014905));
#63779=CARTESIAN_POINT('Ctrl Pts',(39.1570187879001,-8.13575765596819,-11.9302286426536));
#63780=CARTESIAN_POINT('Ctrl Pts',(39.2049352860259,-8.13987450483956,-11.9304184088523));
#63781=CARTESIAN_POINT('Ctrl Pts',(39.2193974376962,-8.14111075633384,-11.9303452664022));
#63782=CARTESIAN_POINT('Ctrl Pts',(39.2447272762823,-8.14326401399199,-11.9299886832563));
#63783=CARTESIAN_POINT('Ctrl Pts',(39.2555949139665,-8.14418393966456,-11.9297620091198));
#63784=CARTESIAN_POINT('Ctrl Pts',(39.2795586873442,-8.14620369170012,-11.9290996297714));
#63785=CARTESIAN_POINT('Ctrl Pts',(39.2926532760722,-8.14730171598736,-11.9286305892746));
#63786=CARTESIAN_POINT('Ctrl Pts',(39.3308393035071,-8.15048906115418,-11.9269502539552));
#63787=CARTESIAN_POINT('Ctrl Pts',(39.3559174288441,-8.15256380683637,-11.92545284318));
#63788=CARTESIAN_POINT('Ctrl Pts',(39.5022309677506,-8.16458522608844,-11.9144136441816));
#63789=CARTESIAN_POINT('Ctrl Pts',(39.6226431555327,-8.17414908542271,-11.8960804694966));
#63790=CARTESIAN_POINT('Ctrl Pts',(39.8603920576504,-8.1932779224102,-11.8411838736332));
#63791=CARTESIAN_POINT('Ctrl Pts',(39.9773354920761,-8.2028172729783,-11.8045991748579));
#63792=CARTESIAN_POINT('Ctrl Pts',(40.1542850305467,-8.21801628721203,-11.7340353721403));
#63793=CARTESIAN_POINT('Ctrl Pts',(40.2164787761007,-8.22351296900573,-11.7061158854337));
#63794=CARTESIAN_POINT('Ctrl Pts',(40.3014267406593,-8.23129907624866,-11.6635589380572));
#63795=CARTESIAN_POINT('Ctrl Pts',(40.3252504086465,-8.23351423423578,-11.651120080486));
#63796=CARTESIAN_POINT('Ctrl Pts',(40.3660588760584,-8.23736698471357,-11.6289350933298));
#63797=CARTESIAN_POINT('Ctrl Pts',(40.3831426909002,-8.238997938578,-11.6193756837645));
#63798=CARTESIAN_POINT('Ctrl Pts',(40.4180578303322,-8.24236989645333,-11.599275072546));
#63799=CARTESIAN_POINT('Ctrl Pts',(40.4358734093178,-8.24411164480865,-11.5887099634585));
#63800=CARTESIAN_POINT('Ctrl Pts',(40.4815647228206,-8.2486354051167,-11.5608099803201));
#63801=CARTESIAN_POINT('Ctrl Pts',(40.5092250447636,-8.25142957551763,-11.5431327925609));
#63802=CARTESIAN_POINT('Ctrl Pts',(40.6496393209387,-8.26591198361009,-11.4492951232816));
#63803=CARTESIAN_POINT('Ctrl Pts',(40.7561246750734,-8.27792499418585,-11.3642467793816));
#63804=CARTESIAN_POINT('Ctrl Pts',(40.944369117659,-8.30115569241861,-11.1857978445688));
#63805=CARTESIAN_POINT('Ctrl Pts',(41.0272419579355,-8.31230587164552,-11.0941593955072));
#63806=CARTESIAN_POINT('Ctrl Pts',(41.1360829728037,-8.32808246806383,-10.9534290454211));
#63807=CARTESIAN_POINT('Ctrl Pts',(41.1679722742019,-8.33287126147658,-10.9091651492865));
#63808=CARTESIAN_POINT('Ctrl Pts',(41.207922230718,-8.33906469165564,-10.8495369468115));
#63809=CARTESIAN_POINT('Ctrl Pts',(41.2173587760633,-8.34054307246339,-10.8351196241973));
#63810=CARTESIAN_POINT('Ctrl Pts',(41.2327237174883,-8.34297469220922,-10.8110850699198));
#63811=CARTESIAN_POINT('Ctrl Pts',(41.2387405876956,-8.34393335855134,-10.801525501894));
#63812=CARTESIAN_POINT('Ctrl Pts',(41.2509159434523,-8.34588609388394,-10.7818756723839));
#63813=CARTESIAN_POINT('Ctrl Pts',(41.2570677811711,-8.34687975039062,-10.7717817873244));
#63814=CARTESIAN_POINT('Ctrl Pts',(41.273280475595,-8.34951853759041,-10.7447334377515));
#63815=CARTESIAN_POINT('Ctrl Pts',(41.2832080326043,-8.35115554593282,-10.7276994469445));
#63816=CARTESIAN_POINT('Ctrl Pts',(41.3333662098905,-8.35954874560748,-10.6391516692073));
#63817=CARTESIAN_POINT('Ctrl Pts',(41.3701330254643,-8.36612121499884,-10.5657264751803));
#63818=CARTESIAN_POINT('Ctrl Pts',(41.4655602476742,-8.38493811013668,-10.3479932160128));
#63819=CARTESIAN_POINT('Ctrl Pts',(41.5140566899546,-8.39695903170728,-10.1997030342007));
#63820=CARTESIAN_POINT('Ctrl Pts',(41.5654275823018,-8.41572311895518,-9.9689817522342));
#63821=CARTESIAN_POINT('Ctrl Pts',(41.5789906495108,-8.42220318112985,-9.88937407040343));
#63822=CARTESIAN_POINT('Ctrl Pts',(41.5918834934816,-8.43112989149296,-9.78103376744624));
#63823=CARTESIAN_POINT('Ctrl Pts',(41.5947402755858,-8.43346830152467,-9.75276920527259));
#63824=CARTESIAN_POINT('Ctrl Pts',(41.5987411404646,-8.4374663861597,-9.70468755128886));
#63825=CARTESIAN_POINT('Ctrl Pts',(41.6001417552086,-8.43911800571743,-9.6848942791888));
#63826=CARTESIAN_POINT('Ctrl Pts',(41.6023400688019,-8.44227457039063,-9.64721183001717));
#63827=CARTESIAN_POINT('Ctrl Pts',(41.6031831955961,-8.44377799702457,-9.62932654936618));
#63828=CARTESIAN_POINT('Ctrl Pts',(41.6046918816193,-8.44731815310019,-9.58736831309691));
#63829=CARTESIAN_POINT('Ctrl Pts',(41.6051957278988,-8.44935972361859,-9.56329192985939));
#63830=CARTESIAN_POINT('Ctrl Pts',(41.6057079777021,-8.45674998483878,-9.4766010606857));
#63831=CARTESIAN_POINT('Ctrl Pts',(41.6036330747786,-8.46216076257928,-9.41400512831191));
#63832=CARTESIAN_POINT('Ctrl Pts',(41.5835736399115,-8.48649938844244,-9.13652034207096));
#63833=CARTESIAN_POINT('Ctrl Pts',(41.5391821044146,-8.50615426264701,-8.92454779612619));
#63834=CARTESIAN_POINT('Ctrl Pts',(41.450358402793,-8.52968592411832,-8.67395861545585));
#63835=CARTESIAN_POINT('Ctrl Pts',(41.4320636291046,-8.53409618206888,-8.62707053562132));
#63836=CARTESIAN_POINT('Ctrl Pts',(41.4057246551034,-8.53988242761902,-8.56535782749339));
#63837=CARTESIAN_POINT('Ctrl Pts',(41.3989781481434,-8.54132103218477,-8.54999768895353));
#63838=CARTESIAN_POINT('Ctrl Pts',(41.3874573953104,-8.54370544457166,-8.52449578735511));
#63839=CARTESIAN_POINT('Ctrl Pts',(41.3827720796763,-8.54465626377964,-8.51431478333761));
#63840=CARTESIAN_POINT('Ctrl Pts',(41.3729391671339,-8.54661278486869,-8.49333561878766));
#63841=CARTESIAN_POINT('Ctrl Pts',(41.367781908375,-8.54761789973075,-8.48254250136713));
#63842=CARTESIAN_POINT('Ctrl Pts',(41.3536243409231,-8.55032231375158,-8.45347298504391));
#63843=CARTESIAN_POINT('Ctrl Pts',(41.3444717424969,-8.55201277170828,-8.43527114575487));
#63844=CARTESIAN_POINT('Ctrl Pts',(41.287386356406,-8.56222673593459,-8.32525046657764));
#63845=CARTESIAN_POINT('Ctrl Pts',(41.2337882994846,-8.57045334566809,-8.23647666372327));
#63846=CARTESIAN_POINT('Ctrl Pts',(41.0956213723443,-8.58949412233432,-8.03785072479634));
#63847=CARTESIAN_POINT('Ctrl Pts',(41.0069699058512,-8.60022463820565,-7.93130868984514));
#63848=CARTESIAN_POINT('Ctrl Pts',(40.8559193820491,-8.61729879914516,-7.77868410864893));
#63849=CARTESIAN_POINT('Ctrl Pts',(40.7996347986024,-8.62344122677296,-7.7269859398101));
#63850=CARTESIAN_POINT('Ctrl Pts',(40.7195575774502,-8.63197821629589,-7.66017375429541));
#63851=CARTESIAN_POINT('Ctrl Pts',(40.6978150984942,-8.63427697566421,-7.64266582210873));
#63852=CARTESIAN_POINT('Ctrl Pts',(40.6601748804735,-8.63822800299212,-7.61342147181324));
#63853=CARTESIAN_POINT('Ctrl Pts',(40.6444277975249,-8.63987267830823,-7.60149501172627));
#63854=CARTESIAN_POINT('Ctrl Pts',(40.6121239817596,-8.64323125161284,-7.57764925235708));
#63855=CARTESIAN_POINT('Ctrl Pts',(40.5955589716999,-8.64494551318919,-7.56574397389094));
#63856=CARTESIAN_POINT('Ctrl Pts',(40.5532130630552,-8.64930921117664,-7.53611943567535));
#63857=CARTESIAN_POINT('Ctrl Pts',(40.5272350341944,-8.65196918821372,-7.51869033817353));
#63858=CARTESIAN_POINT('Ctrl Pts',(40.4130721215735,-8.66359223010618,-7.44528407932634));
#63859=CARTESIAN_POINT('Ctrl Pts',(40.3216467031703,-8.67273866870194,-7.39458582807992));
#63860=CARTESIAN_POINT('Ctrl Pts',(40.0935723953588,-8.6951689036031,-7.28686897864534));
#63861=CARTESIAN_POINT('Ctrl Pts',(39.9543881480952,-8.70855893992475,-7.23620165720945));
#63862=CARTESIAN_POINT('Ctrl Pts',(39.7700044030205,-8.72552222665956,-7.1877402259859));
#63863=CARTESIAN_POINT('Ctrl Pts',(39.7282844788106,-8.72930920436744,-7.17795839934688));
#63864=CARTESIAN_POINT('Ctrl Pts',(39.6569324128432,-8.73567840210739,-7.16322813821743));
#63865=CARTESIAN_POINT('Ctrl Pts',(39.6274289405675,-8.73828112534517,-7.15771076865525));
#63866=CARTESIAN_POINT('Ctrl Pts',(39.5841491430127,-8.74204732005984,-7.15045272676392));
#63867=CARTESIAN_POINT('Ctrl Pts',(39.5704502120145,-8.74323184566089,-7.1482770489051));
#63868=CARTESIAN_POINT('Ctrl Pts',(39.5470574558826,-8.74524089813474,-7.14476896443429));
#63869=CARTESIAN_POINT('Ctrl Pts',(39.5373733805641,-8.74606857085188,-7.14337705008226));
#63870=CARTESIAN_POINT('Ctrl Pts',(39.5147458032615,-8.74799306535275,-7.14026552989884));
#63871=CARTESIAN_POINT('Ctrl Pts',(39.5017964072842,-8.74908734502324,-7.13859216257249));
#63872=CARTESIAN_POINT('Ctrl Pts',(39.4633426112578,-8.7523176555313,-7.13394104873244));
#63873=CARTESIAN_POINT('Ctrl Pts',(39.4378023597089,-8.7544381621786,-7.13126600511164));
#63874=CARTESIAN_POINT('Ctrl Pts',(39.2956381081665,-8.76612802966791,-7.11867398730389));
#63875=CARTESIAN_POINT('Ctrl Pts',(39.1784378413477,-8.7753459442424,-7.11686908431961));
#63876=CARTESIAN_POINT('Ctrl Pts',(38.9410866157831,-8.79399130468109,-7.13055263126393));
#63877=CARTESIAN_POINT('Ctrl Pts',(38.8213157290546,-8.80339273515776,-7.14655292626023));
#63878=CARTESIAN_POINT('Ctrl Pts',(38.6322370600079,-8.81878162505628,-7.18646063030293));
#63879=CARTESIAN_POINT('Ctrl Pts',(38.5619412705909,-8.82462612617245,-7.20465512849876));
#63880=CARTESIAN_POINT('Ctrl Pts',(38.4663443113245,-8.83281762599381,-7.23407096825798));
#63881=CARTESIAN_POINT('Ctrl Pts',(38.440248653903,-8.83507911984349,-7.24259244109609));
#63882=CARTESIAN_POINT('Ctrl Pts',(38.3957119791689,-8.83898616508868,-7.2579841776568));
#63883=CARTESIAN_POINT('Ctrl Pts',(38.3771984890805,-8.84062455245881,-7.26463773156211));
#63884=CARTESIAN_POINT('Ctrl Pts',(38.3395357914404,-8.84398814799495,-7.27869731171502));
#63885=CARTESIAN_POINT('Ctrl Pts',(38.3203956915924,-8.84571388357338,-7.28612290951717));
#63886=CARTESIAN_POINT('Ctrl Pts',(38.2717369420788,-8.85014462547898,-7.30572082084604));
#63887=CARTESIAN_POINT('Ctrl Pts',(38.2423623175846,-8.85286084099711,-7.31823715853267));
#63888=CARTESIAN_POINT('Ctrl Pts',(38.1053165669283,-8.86573706334251,-7.37988295872333));
#63889=CARTESIAN_POINT('Ctrl Pts',(38.001135476713,-8.87613765481072,-7.4363224881149));
#63890=CARTESIAN_POINT('Ctrl Pts',(37.801439105181,-8.89730863221659,-7.56438209788894));
#63891=CARTESIAN_POINT('Ctrl Pts',(37.7062347971764,-8.90805171406802,-7.63591037150568));
#63892=CARTESIAN_POINT('Ctrl Pts',(37.5784457791295,-8.92321088883573,-7.74764279939344));
#63893=CARTESIAN_POINT('Ctrl Pts',(37.5412468273952,-8.92772253753241,-7.78230801646997));
#63894=CARTESIAN_POINT('Ctrl Pts',(37.4811283027383,-8.93515033605419,-7.8420023476698));
#63895=CARTESIAN_POINT('Ctrl Pts',(37.457589942948,-8.93809595991985,-7.86638354444659));
#63896=CARTESIAN_POINT('Ctrl Pts',(37.4247023173413,-8.94225663751462,-7.90192197359008));
#63897=CARTESIAN_POINT('Ctrl Pts',(37.4149281686698,-8.94349911007786,-7.91267784490645));
#63898=CARTESIAN_POINT('Ctrl Pts',(37.3980108438776,-8.94565910848903,-7.93163679438678));
#63899=CARTESIAN_POINT('Ctrl Pts',(37.3908249745688,-8.94657961861338,-7.93980065271793));
#63900=CARTESIAN_POINT('Ctrl Pts',(37.3751377002543,-8.94859574575634,-7.9578685863311));
#63901=CARTESIAN_POINT('Ctrl Pts',(37.366661209268,-8.94968961053923,-7.96779346792477));
#63902=CARTESIAN_POINT('Ctrl Pts',(37.3417662135749,-8.95291737751067,-7.99742738102724));
#63903=CARTESIAN_POINT('Ctrl Pts',(37.3255810132762,-8.95503579196878,-8.01733142427825));
#63904=CARTESIAN_POINT('Ctrl Pts',(37.2450264833285,-8.9657053935844,-8.11969785772744));
#63905=CARTESIAN_POINT('Ctrl Pts',(37.1857588452718,-8.97397947296573,-8.20604808724587));
#63906=CARTESIAN_POINT('Ctrl Pts',(37.087028361216,-8.98915842577011,-8.37215427388057));
#63907=CARTESIAN_POINT('Ctrl Pts',(37.0460031090574,-8.99606679494006,-8.45075620351427));
#63908=CARTESIAN_POINT('Ctrl Pts',(36.9911539509655,-9.00652134797575,-8.57168736622732));
#63909=CARTESIAN_POINT('Ctrl Pts',(36.9740189001327,-9.01001361398599,-8.61241497730244));
#63910=CARTESIAN_POINT('Ctrl Pts',(36.9580196445751,-9.01353011641035,-8.65357758217454));
#63911=CARTESIAN_POINT('Origin',(39.2,8.05522481984854,-9.525));
#63912=CARTESIAN_POINT('',(36.958019684939,-10.5481760837449,-8.65357747832709));
#63913=CARTESIAN_POINT('',(36.9580196499262,-10.2836033739986,-8.65357756840738));
#63914=CARTESIAN_POINT('',(36.958019684865,8.05522481984854,-8.65357747851728));
#63915=CARTESIAN_POINT('',(36.794620234193,-9.35522481984856,-9.52393856416118));
#63916=CARTESIAN_POINT('Ctrl Pts',(36.958019684939,-10.5481760837449,-8.65357747832709));
#63917=CARTESIAN_POINT('Ctrl Pts',(36.9617940800382,-10.5472770356811,-8.64386678196179));
#63918=CARTESIAN_POINT('Ctrl Pts',(36.9656316767484,-10.5463810343756,-8.63418032043723));
#63919=CARTESIAN_POINT('Ctrl Pts',(36.9744232493849,-10.5443689686419,-8.61240383311359));
#63920=CARTESIAN_POINT('Ctrl Pts',(36.9794130521616,-10.5432548445178,-8.60032856197506));
#63921=CARTESIAN_POINT('Ctrl Pts',(36.9887368682618,-10.5412238092281,-8.57827585147578));
#63922=CARTESIAN_POINT('Ctrl Pts',(36.993040355656,-10.540305287641,-8.56828667307018));
#63923=CARTESIAN_POINT('Ctrl Pts',(37.0032471680292,-10.5381698972795,-8.54503021541096));
#63924=CARTESIAN_POINT('Ctrl Pts',(37.0092030852763,-10.5369561511453,-8.53178668216365));
#63925=CARTESIAN_POINT('Ctrl Pts',(37.0294181743284,-10.5329391486733,-8.48790331687982));
#63926=CARTESIAN_POINT('Ctrl Pts',(37.0442039027969,-10.5301647308001,-8.45750830262123));
#63927=CARTESIAN_POINT('Ctrl Pts',(37.0827314884524,-10.5233007687884,-8.38237538734461));
#63928=CARTESIAN_POINT('Ctrl Pts',(37.107255376584,-10.5192463126082,-8.33805531683175));
#63929=CARTESIAN_POINT('Ctrl Pts',(37.2308012985563,-10.5000738513962,-8.13053189905721));
#63930=CARTESIAN_POINT('Ctrl Pts',(37.3476119881842,-10.4854240899873,-7.97873157066489));
#63931=CARTESIAN_POINT('Ctrl Pts',(37.522672845037,-10.4653892921338,-7.79990533755317));
#63932=CARTESIAN_POINT('Ctrl Pts',(37.5657592104529,-10.4605876239119,-7.75903455987815));
#63933=CARTESIAN_POINT('Ctrl Pts',(37.6281276227031,-10.4537734694143,-7.70411180169745));
#63934=CARTESIAN_POINT('Ctrl Pts',(37.6461758521252,-10.4518167501323,-7.68868656337561));
#63935=CARTESIAN_POINT('Ctrl Pts',(37.6795458159023,-10.4482238036903,-7.66101053822831));
#63936=CARTESIAN_POINT('Ctrl Pts',(37.6947949256035,-10.4465911263317,-7.64867506124427));
#63937=CARTESIAN_POINT('Ctrl Pts',(37.726121059886,-10.4432543619239,-7.62396201354268));
#63938=CARTESIAN_POINT('Ctrl Pts',(37.742207212201,-10.4415498898669,-7.61159865946782));
#63939=CARTESIAN_POINT('Ctrl Pts',(37.7830280507703,-10.4372454530019,-7.58103850562135));
#63940=CARTESIAN_POINT('Ctrl Pts',(37.807957632509,-10.4346355351603,-7.56310967272344));
#63941=CARTESIAN_POINT('Ctrl Pts',(37.9208329336029,-10.422895043784,-7.48516665422902));
#63942=CARTESIAN_POINT('Ctrl Pts',(38.0123488530201,-10.4135720331113,-7.43056298306245));
#63943=CARTESIAN_POINT('Ctrl Pts',(38.1882442185085,-10.3960098730176,-7.34085561649105));
#63944=CARTESIAN_POINT('Ctrl Pts',(38.2716003716131,-10.3878248635031,-7.30414227070433));
#63945=CARTESIAN_POINT('Ctrl Pts',(38.45558357101,-10.370175925564,-7.23528053283743));
#63946=CARTESIAN_POINT('Ctrl Pts',(38.5566702979195,-10.3607320609294,-7.20484853907379));
#63947=CARTESIAN_POINT('Ctrl Pts',(38.6844766904349,-10.3493076526327,-7.17537259514505));
#63948=CARTESIAN_POINT('Ctrl Pts',(38.7096078057195,-10.3470857526408,-7.1699991759541));
#63949=CARTESIAN_POINT('Ctrl Pts',(38.7476376875347,-10.3437647909215,-7.16250303413089));
#63950=CARTESIAN_POINT('Ctrl Pts',(38.7604745014706,-10.3426508774321,-7.16008119883126));
#63951=CARTESIAN_POINT('Ctrl Pts',(38.7840365716084,-10.3406199457246,-7.15583438609));
#63952=CARTESIAN_POINT('Ctrl Pts',(38.7947549822719,-10.3397013202964,-7.15397748512991));
#63953=CARTESIAN_POINT('Ctrl Pts',(38.8198168862019,-10.3375652530155,-7.14981057904506));
#63954=CARTESIAN_POINT('Ctrl Pts',(38.8341692606762,-10.3363509393952,-7.14755770028923));
#63955=CARTESIAN_POINT('Ctrl Pts',(38.8820156119236,-10.332329850656,-7.14049086430308));
#63956=CARTESIAN_POINT('Ctrl Pts',(38.9155926427797,-10.3295519945498,-7.13625332229212));
#63957=CARTESIAN_POINT('Ctrl Pts',(38.9997022074193,-10.3226773067431,-7.12743726084013));
#63958=CARTESIAN_POINT('Ctrl Pts',(39.0503126204247,-10.3186157049019,-7.12374600052062));
#63959=CARTESIAN_POINT('Ctrl Pts',(39.2826908550674,-10.300153916378,-7.11417426852147));
#63960=CARTESIAN_POINT('Ctrl Pts',(39.4646370330087,-10.286177500558,-7.12731600651833));
#63961=CARTESIAN_POINT('Ctrl Pts',(39.7082488838147,-10.2663941915519,-7.17300221878139));
#63962=CARTESIAN_POINT('Ctrl Pts',(39.7725951872106,-10.2610690557433,-7.18783423850404));
#63963=CARTESIAN_POINT('Ctrl Pts',(39.8625284554224,-10.2534300364104,-7.21250096916805));
#63964=CARTESIAN_POINT('Ctrl Pts',(39.888686152377,-10.2511843767762,-7.22015575737469));
#63965=CARTESIAN_POINT('Ctrl Pts',(39.9332770612134,-10.2473117631226,-7.23403166053559));
#63966=CARTESIAN_POINT('Ctrl Pts',(39.9517756756488,-10.2456919317577,-7.24003512766715));
#63967=CARTESIAN_POINT('Ctrl Pts',(39.9896661285934,-10.2423454071276,-7.25284185926933));
#63968=CARTESIAN_POINT('Ctrl Pts',(40.0090475747856,-10.2406180004534,-7.25967062510547));
#63969=CARTESIAN_POINT('Ctrl Pts',(40.0583877829925,-10.2361788523927,-7.27776885795176));
#63970=CARTESIAN_POINT('Ctrl Pts',(40.0882124252737,-10.233455822443,-7.28938915117906));
#63971=CARTESIAN_POINT('Ctrl Pts',(40.2383347973881,-10.2195386369256,-7.35135801289239));
#63972=CARTESIAN_POINT('Ctrl Pts',(40.3546059034522,-10.2080467966561,-7.41082592155569));
#63973=CARTESIAN_POINT('Ctrl Pts',(40.5785310510507,-10.1844926843788,-7.54935309821659));
#63974=CARTESIAN_POINT('Ctrl Pts',(40.6856013191408,-10.1724637933771,-7.62855112747738));
#63975=CARTESIAN_POINT('Ctrl Pts',(40.824604694199,-10.1560849996368,-7.75039986586704));
#63976=CARTESIAN_POINT('Ctrl Pts',(40.8625157233103,-10.151530729951,-7.78586556626632));
#63977=CARTESIAN_POINT('Ctrl Pts',(40.9115761107257,-10.145547882651,-7.83483334931611));
#63978=CARTESIAN_POINT('Ctrl Pts',(40.9237658741182,-10.1440536291517,-7.84726719777123));
#63979=CARTESIAN_POINT('Ctrl Pts',(40.9428896340482,-10.1416984848065,-7.86720237781049));
#63980=CARTESIAN_POINT('Ctrl Pts',(40.9499123870889,-10.1408312233466,-7.87461704981788));
#63981=CARTESIAN_POINT('Ctrl Pts',(40.9647118087771,-10.1389989050201,-7.89044305997697));
#63982=CARTESIAN_POINT('Ctrl Pts',(40.9724760659392,-10.1380348279483,-7.89886569781726));
#63983=CARTESIAN_POINT('Ctrl Pts',(40.992286676239,-10.1355667239808,-7.92066665406841));
#63984=CARTESIAN_POINT('Ctrl Pts',(41.004243889023,-10.1340690510318,-7.9341256921298));
#63985=CARTESIAN_POINT('Ctrl Pts',(41.0571795100254,-10.12739543117,-7.99507466851855));
#63986=CARTESIAN_POINT('Ctrl Pts',(41.0964463891134,-10.1223261527214,-8.04402729016236));
#63987=CARTESIAN_POINT('Ctrl Pts',(41.2202168738326,-10.1057176448463,-8.21133685118462));
#63988=CARTESIAN_POINT('Ctrl Pts',(41.2959066539736,-10.0944725374643,-8.33581226783064));
#63989=CARTESIAN_POINT('Ctrl Pts',(41.4070036138665,-10.0745939711146,-8.56247997881646));
#63990=CARTESIAN_POINT('Ctrl Pts',(41.4476377485976,-10.0660805265843,-8.66161744501087));
#63991=CARTESIAN_POINT('Ctrl Pts',(41.491495524814,-10.0547839971975,-8.79295459457397));
#63992=CARTESIAN_POINT('Ctrl Pts',(41.5008712378666,-10.0522009732421,-8.82297893348488));
#63993=CARTESIAN_POINT('Ctrl Pts',(41.515363171757,-10.0479083883193,-8.87280064987866));
#63994=CARTESIAN_POINT('Ctrl Pts',(41.5208206752382,-10.0462098947368,-8.89249549481313));
#63995=CARTESIAN_POINT('Ctrl Pts',(41.5310541170087,-10.0428551107256,-8.93134253255975));
#63996=CARTESIAN_POINT('Ctrl Pts',(41.5358465787012,-10.0411994950142,-8.95048873268257));
#63997=CARTESIAN_POINT('Ctrl Pts',(41.5468206884597,-10.0371934950487,-8.99674017662814));
#63998=CARTESIAN_POINT('Ctrl Pts',(41.552768922648,-10.0348359477567,-9.02389717416046));
#63999=CARTESIAN_POINT('Ctrl Pts',(41.5730979672251,-10.02602881308,-9.12507025077084));
#64000=CARTESIAN_POINT('Ctrl Pts',(41.5844654080335,-10.019488163995,-9.19963881468357));
#64001=CARTESIAN_POINT('Ctrl Pts',(41.6063421594812,-10.0010026183094,-9.4086567564682));
#64002=CARTESIAN_POINT('Ctrl Pts',(41.6090794607252,-9.98887829976523,-9.54363325619523));
#64003=CARTESIAN_POINT('Ctrl Pts',(41.5936031465559,-9.96704373995819,-9.78627214944001));
#64004=CARTESIAN_POINT('Ctrl Pts',(41.5794011660872,-9.95735461240898,-9.89385662884896));
#64005=CARTESIAN_POINT('Ctrl Pts',(41.5539589993196,-9.94619583057232,-10.0201221711368));
#64006=CARTESIAN_POINT('Ctrl Pts',(41.5496759170829,-9.94443998410839,-10.0400651457396));
#64007=CARTESIAN_POINT('Ctrl Pts',(41.5424777267598,-9.9416746446538,-10.071620786504));
#64008=CARTESIAN_POINT('Ctrl Pts',(41.5397288573405,-9.94065661836519,-10.083269717966));
#64009=CARTESIAN_POINT('Ctrl Pts',(41.5342376778165,-9.93869488463575,-10.105786551795));
#64010=CARTESIAN_POINT('Ctrl Pts',(41.5315061910978,-9.93775067214095,-10.1166565264216));
#64011=CARTESIAN_POINT('Ctrl Pts',(41.5244986800392,-9.93540418742908,-10.1437406522502));
#64012=CARTESIAN_POINT('Ctrl Pts',(41.5201287793553,-9.93400707040984,-10.1599303934326));
#64013=CARTESIAN_POINT('Ctrl Pts',(41.5019945811145,-9.92845835596267,-10.2244259429448));
#64014=CARTESIAN_POINT('Ctrl Pts',(41.4868869044157,-9.92437400293287,-10.272345300723));
#64015=CARTESIAN_POINT('Ctrl Pts',(41.3989475470494,-9.90298886321175,-10.5235499768259));
#64016=CARTESIAN_POINT('Ctrl Pts',(41.3004915580736,-9.88654338108804,-10.7168146022263));
#64017=CARTESIAN_POINT('Ctrl Pts',(41.142025084017,-9.86428891187898,-10.9456641222148));
#64018=CARTESIAN_POINT('Ctrl Pts',(41.1045153843572,-9.85924720532869,-10.9955671974628));
#64019=CARTESIAN_POINT('Ctrl Pts',(41.0499101822128,-9.85215982858639,-11.0626165633304));
#64020=CARTESIAN_POINT('Ctrl Pts',(41.0344307861134,-9.85017659942571,-11.0810514080777));
#64021=CARTESIAN_POINT('Ctrl Pts',(41.0069590010383,-9.84669877990423,-11.1127886303995));
#64022=CARTESIAN_POINT('Ctrl Pts',(40.995089640264,-9.84520923072148,-11.1261954013841));
#64023=CARTESIAN_POINT('Ctrl Pts',(40.9697477932711,-9.84205511770859,-11.1541837775884));
#64024=CARTESIAN_POINT('Ctrl Pts',(40.9562423224549,-9.84038925692244,-11.1687335207685));
#64025=CARTESIAN_POINT('Ctrl Pts',(40.9229560450303,-9.83631829915349,-11.2037150083473));
#64026=CARTESIAN_POINT('Ctrl Pts',(40.9029905055498,-9.83390544839181,-11.2239658034489));
#64027=CARTESIAN_POINT('Ctrl Pts',(40.824829431575,-9.82456438149032,-11.300481428066));
#64028=CARTESIAN_POINT('Ctrl Pts',(40.7641736385596,-9.81752979043384,-11.3541426000984));
#64029=CARTESIAN_POINT('Ctrl Pts',(40.5785047596695,-9.79658175681074,-11.5024035769155));
#64030=CARTESIAN_POINT('Ctrl Pts',(40.4468215228621,-9.78241488299629,-11.58796574652));
#64031=CARTESIAN_POINT('Ctrl Pts',(40.2360295279814,-9.7611736992508,-11.6973325575484));
#64032=CARTESIAN_POINT('Ctrl Pts',(40.1624447608922,-9.7540050842331,-11.7309213887749));
#64033=CARTESIAN_POINT('Ctrl Pts',(40.069012631137,-9.74530382552355,-11.7680018031981));
#64034=CARTESIAN_POINT('Ctrl Pts',(40.0506360904107,-9.74361122996381,-11.7750351909826));
#64035=CARTESIAN_POINT('Ctrl Pts',(40.0210902668807,-9.74092198060536,-11.7859297381599));
#64036=CARTESIAN_POINT('Ctrl Pts',(40.0099757828261,-9.73991754412972,-11.7899352655416));
#64037=CARTESIAN_POINT('Ctrl Pts',(39.9881688247258,-9.73796145018396,-11.7976131750646));
#64038=CARTESIAN_POINT('Ctrl Pts',(39.9774792388317,-9.73700946800847,-11.8012923326884));
#64039=CARTESIAN_POINT('Ctrl Pts',(39.9503965567882,-9.73461396267094,-11.810400652182));
#64040=CARTESIAN_POINT('Ctrl Pts',(39.9339697189982,-9.73317607279061,-11.8157290626079));
#64041=CARTESIAN_POINT('Ctrl Pts',(39.8651005550662,-9.72720479884732,-11.8372513838694));
#64042=CARTESIAN_POINT('Ctrl Pts',(39.8121642880277,-9.72275231909575,-11.8518264601564));
#64043=CARTESIAN_POINT('Ctrl Pts',(39.640287380292,-9.7085921309835,-11.8928764562191));
#64044=CARTESIAN_POINT('Ctrl Pts',(39.5198168892167,-9.69910990610688,-11.9121350400517));
#64045=CARTESIAN_POINT('Ctrl Pts',(39.2720406308413,-9.67961969546622,-11.9326417025696));
#64046=CARTESIAN_POINT('Ctrl Pts',(39.1450701988678,-9.66963364297617,-11.9330915589169));
#64047=CARTESIAN_POINT('Ctrl Pts',(38.9808679185907,-9.65627350106521,-11.9206775558384));
#64048=CARTESIAN_POINT('Ctrl Pts',(38.9431446465176,-9.65317450966836,-11.9169270128237));
#64049=CARTESIAN_POINT('Ctrl Pts',(38.883725001822,-9.64823647720225,-11.909597588981));
#64050=CARTESIAN_POINT('Ctrl Pts',(38.8619609144421,-9.64641572807348,-11.9066097594778));
#64051=CARTESIAN_POINT('Ctrl Pts',(38.8213975626643,-9.64299790976286,-11.9004739230374));
#64052=CARTESIAN_POINT('Ctrl Pts',(38.802588728532,-9.64140326751076,-11.8973997136829));
#64053=CARTESIAN_POINT('Ctrl Pts',(38.7600151002384,-9.6377702863768,-11.8899207899825));
#64054=CARTESIAN_POINT('Ctrl Pts',(38.7362765673883,-9.63572785811218,-11.8853808043069));
#64055=CARTESIAN_POINT('Ctrl Pts',(38.6630789974455,-9.62937562810909,-11.8702350163411));
#64056=CARTESIAN_POINT('Ctrl Pts',(38.6138864504958,-9.62502895838328,-11.8584269938047));
#64057=CARTESIAN_POINT('Ctrl Pts',(38.4971933890948,-9.6145217455718,-11.8264937261181));
#64058=CARTESIAN_POINT('Ctrl Pts',(38.4301358487702,-9.60832272945565,-11.8049381294784));
#64059=CARTESIAN_POINT('Ctrl Pts',(38.2778280882835,-9.59388048457267,-11.7484932153076));
#64060=CARTESIAN_POINT('Ctrl Pts',(38.1934407173553,-9.58560423990945,-11.7115863592595));
#64061=CARTESIAN_POINT('Ctrl Pts',(38.0169567869119,-9.56782316210305,-11.6220154993521));
#64062=CARTESIAN_POINT('Ctrl Pts',(37.9257905002492,-9.55833839139738,-11.5679048657617));
#64063=CARTESIAN_POINT('Ctrl Pts',(37.8173108084081,-9.54687690179493,-11.4934214189966));
#64064=CARTESIAN_POINT('Ctrl Pts',(37.7963753985365,-9.54465661025689,-11.4785481622657));
#64065=CARTESIAN_POINT('Ctrl Pts',(37.7651580285667,-9.54133759851847,-11.4556092258415));
#64066=CARTESIAN_POINT('Ctrl Pts',(37.754697871366,-9.54022404905476,-11.447791004591));
#64067=CARTESIAN_POINT('Ctrl Pts',(37.735957291353,-9.5382271269469,-11.4335444075183));
#64068=CARTESIAN_POINT('Ctrl Pts',(37.7276547833192,-9.53734184818155,-11.427146782176));
#64069=CARTESIAN_POINT('Ctrl Pts',(37.7191393668961,-9.53643311376151,-11.4204959335104));
#64070=CARTESIAN_POINT('Ctrl Pts',(37.7188849673564,-9.53640596442008,-11.4202971557803));
#64071=CARTESIAN_POINT('Ctrl Pts',(37.718393885222,-9.53635355502442,-11.4199132843828));
#64072=CARTESIAN_POINT('Ctrl Pts',(37.7181571973048,-9.53632829450292,-11.4197281975995));
#64073=CARTESIAN_POINT('Ctrl Pts',(37.7176990352709,-9.53627939587673,-11.4193697826603));
#64074=CARTESIAN_POINT('Ctrl Pts',(37.7174775568987,-9.53625575739953,-11.4191964600311));
#64075=CARTESIAN_POINT('Ctrl Pts',(37.7170477493988,-9.53620988273649,-11.4188599834352));
#64076=CARTESIAN_POINT('Ctrl Pts',(37.7168394168242,-9.5361876462497,-11.4186968339557));
#64077=CARTESIAN_POINT('Ctrl Pts',(37.7164341791138,-9.5361443919746,-11.4183793761634));
#64078=CARTESIAN_POINT('Ctrl Pts',(37.7162372711094,-9.53612337393552,-11.4182250714952));
#64079=CARTESIAN_POINT('Ctrl Pts',(37.7158534316952,-9.53608240184531,-11.4179241835369));
#64080=CARTESIAN_POINT('Ctrl Pts',(37.715666497948,-9.53606244759097,-11.41777760329));
#64081=CARTESIAN_POINT('Ctrl Pts',(37.715301373173,-9.53602347148798,-11.417491210864));
#64082=CARTESIAN_POINT('Ctrl Pts',(37.7151231801841,-9.53600444946892,-11.417351401213));
#64083=CARTESIAN_POINT('Ctrl Pts',(37.7147744782518,-9.53596722493105,-11.4170777312097));
#64084=CARTESIAN_POINT('Ctrl Pts',(37.7146039676735,-9.53594902227067,-11.416943872989));
#64085=CARTESIAN_POINT('Ctrl Pts',(37.714269714768,-9.53591333877643,-11.4166813968791));
#64086=CARTESIAN_POINT('Ctrl Pts',(37.7141059710487,-9.535895857822,-11.4165527807812));
#64087=CARTESIAN_POINT('Ctrl Pts',(37.7137844534175,-9.53586153257664,-11.4163001701908));
#64088=CARTESIAN_POINT('Ctrl Pts',(37.7136266783115,-9.53584468818219,-11.4161761772082));
#64089=CARTESIAN_POINT('Ctrl Pts',(37.7133163964864,-9.53581156123753,-11.4159322687716));
#64090=CARTESIAN_POINT('Ctrl Pts',(37.7131638887586,-9.5357952786002,-11.4158123546102));
#64091=CARTESIAN_POINT('Ctrl Pts',(37.7128635209995,-9.53576320895746,-11.4155761218789));
#64092=CARTESIAN_POINT('Ctrl Pts',(37.7127156601183,-9.535747421879,-11.415459804422));
#64093=CARTESIAN_POINT('Ctrl Pts',(37.7124240329479,-9.53571628434737,-11.4152303352028));
#64094=CARTESIAN_POINT('Ctrl Pts',(37.7122802659038,-9.53570093382884,-11.4151171843706));
#64095=CARTESIAN_POINT('Ctrl Pts',(37.7119963299236,-9.53567061644701,-11.414893662106));
#64096=CARTESIAN_POINT('Ctrl Pts',(37.7118561603564,-9.53565564952944,-11.4147832914808));
#64097=CARTESIAN_POINT('Ctrl Pts',(37.7115789705714,-9.5356260514677,-11.4145649800894));
#64098=CARTESIAN_POINT('Ctrl Pts',(37.7114419498324,-9.53561142027915,-11.4144570400269));
#64099=CARTESIAN_POINT('Ctrl Pts',(37.7111706492607,-9.53558245009166,-11.4142432712618));
#64100=CARTESIAN_POINT('Ctrl Pts',(37.7110363689745,-9.53556811105396,-11.4141374431508));
#64101=CARTESIAN_POINT('Ctrl Pts',(37.7107701749681,-9.53553968522004,-11.4139276060386));
#64102=CARTESIAN_POINT('Ctrl Pts',(37.7106382608219,-9.53552559838653,-11.4138235975049));
#64103=CARTESIAN_POINT('Ctrl Pts',(37.7103764532939,-9.53549764005506,-11.4136171292427));
#64104=CARTESIAN_POINT('Ctrl Pts',(37.7102465596171,-9.53548376853252,-11.4135146699557));
#64105=CARTESIAN_POINT('Ctrl Pts',(37.7099884715763,-9.53545620651247,-11.4133110485913));
#64106=CARTESIAN_POINT('Ctrl Pts',(37.7098602769393,-9.53544251599159,-11.4132098868569));
#64107=CARTESIAN_POINT('Ctrl Pts',(37.7096052856644,-9.53541528381059,-11.4130086244448));
#64108=CARTESIAN_POINT('Ctrl Pts',(37.7094784888461,-9.53540174213591,-11.4129085240776));
#64109=CARTESIAN_POINT('Ctrl Pts',(37.7092260089581,-9.53537477730123,-11.412709161307));
#64110=CARTESIAN_POINT('Ctrl Pts',(37.7091003256796,-9.53536135412265,-11.4126098990948));
#64111=CARTESIAN_POINT('Ctrl Pts',(37.7088498023637,-9.53533459739803,-11.4124120000158));
#64112=CARTESIAN_POINT('Ctrl Pts',(37.7087249621897,-9.53532126384019,-11.4123133633073));
#64113=CARTESIAN_POINT('Ctrl Pts',(37.7084758657394,-9.53529465866364,-11.4121165110835));
#64114=CARTESIAN_POINT('Ctrl Pts',(37.7083516094116,-9.53528138704137,-11.4120182957091));
#64115=CARTESIAN_POINT('Ctrl Pts',(37.7081034302298,-9.53525487899175,-11.4118220887161));
#64116=CARTESIAN_POINT('Ctrl Pts',(37.7079795073268,-9.53524164256025,-11.4117240971595));
#64117=CARTESIAN_POINT('Ctrl Pts',(37.707731751225,-9.5352151788554,-11.4115281453052));
#64118=CARTESIAN_POINT('Ctrl Pts',(37.7076079179756,-9.53520195157689,-11.4114301849901));
#64119=CARTESIAN_POINT('Ctrl Pts',(37.707360101928,-9.53517548062033,-11.411234106383));
#64120=CARTESIAN_POINT('Ctrl Pts',(37.7072361191475,-9.5351622369436,-11.411135988051));
#64121=CARTESIAN_POINT('Ctrl Pts',(37.7069877674696,-9.53513570791645,-11.410939405993));
#64122=CARTESIAN_POINT('Ctrl Pts',(37.7068633986696,-9.53512242257502,-11.4108409422139));
#64123=CARTESIAN_POINT('Ctrl Pts',(37.7066140393411,-9.53509578504317,-11.4106434822971));
#64124=CARTESIAN_POINT('Ctrl Pts',(37.7064890489464,-9.53508243286479,-11.4105444860586));
#64125=CARTESIAN_POINT('Ctrl Pts',(37.7062382100754,-9.53505563640113,-11.4103457733642));
#64126=CARTESIAN_POINT('Ctrl Pts',(37.7061123617213,-9.5350421921258,-11.4102460567203));
#64127=CARTESIAN_POINT('Ctrl Pts',(37.7058595679992,-9.53501518593132,-11.4100457130005));
#64128=CARTESIAN_POINT('Ctrl Pts',(37.7057326227893,-9.53500162402505,-11.4099450856842));
#64129=CARTESIAN_POINT('Ctrl Pts',(37.7054773921606,-9.53497435657274,-11.4097427267039));
#64130=CARTESIAN_POINT('Ctrl Pts',(37.7053491069636,-9.53496065104545,-11.4096409947659));
#64131=CARTESIAN_POINT('Ctrl Pts',(37.705090947254,-9.53493306971971,-11.4094362276027));
#64132=CARTESIAN_POINT('Ctrl Pts',(37.7049610730091,-9.53491919394393,-11.4093331920511));
#64133=CARTESIAN_POINT('Ctrl Pts',(37.704699478435,-9.53489124466718,-11.40912561229));
#64134=CARTESIAN_POINT('Ctrl Pts',(37.7045677584072,-9.53487717119138,-11.409021067686));
#64135=CARTESIAN_POINT('Ctrl Pts',(37.7043022059747,-9.53484879803863,-11.4088102565151));
#64136=CARTESIAN_POINT('Ctrl Pts',(37.7041683739216,-9.53483449839102,-11.4087039894918));
#64137=CARTESIAN_POINT('Ctrl Pts',(37.7038983197439,-9.53480564319569,-11.4084895107224));
#64138=CARTESIAN_POINT('Ctrl Pts',(37.703762098019,-9.53479108768116,-11.4083812984475));
#64139=CARTESIAN_POINT('Ctrl Pts',(37.7034869733554,-9.53476168961095,-11.4081626952983));
#64140=CARTESIAN_POINT('Ctrl Pts',(37.7033480708792,-9.53474684709377,-11.4080523038246));
#64141=CARTESIAN_POINT('Ctrl Pts',(37.7030672779629,-9.53471684220376,-11.4078290955249));
#64142=CARTESIAN_POINT('Ctrl Pts',(37.7029253880609,-9.53470167987597,-11.4077162780271));
#64143=CARTESIAN_POINT('Ctrl Pts',(37.7026382955425,-9.5346710006205,-11.4074879560967));
#64144=CARTESIAN_POINT('Ctrl Pts',(37.702493093567,-9.5346554837471,-11.4073724509274));
#64145=CARTESIAN_POINT('Ctrl Pts',(37.7021990317842,-9.53462405847275,-11.4071384753005));
#64146=CARTESIAN_POINT('Ctrl Pts',(37.7020501726482,-9.53460815012737,-11.4070200039668));
#64147=CARTESIAN_POINT('Ctrl Pts',(37.7017484280631,-9.53457590247677,-11.4067797984307));
#64148=CARTESIAN_POINT('Ctrl Pts',(37.7015955433796,-9.534559563235,-11.4066580632445));
#64149=CARTESIAN_POINT('Ctrl Pts',(37.701285352924,-9.53452641154047,-11.4064110107814));
#64150=CARTESIAN_POINT('Ctrl Pts',(37.7011280479947,-9.53450959915693,-11.4062856923767));
#64151=CARTESIAN_POINT('Ctrl Pts',(37.6908226299531,-9.5334081555033,-11.3980736742179));
#64152=CARTESIAN_POINT('Ctrl Pts',(37.6807397676496,-9.53232893322692,-11.3899047407382));
#64153=CARTESIAN_POINT('Ctrl Pts',(37.6551096457665,-9.52958006986955,-11.3687938906684));
#64154=CARTESIAN_POINT('Ctrl Pts',(37.6396582496571,-9.52791759593007,-11.3557364131491));
#64155=CARTESIAN_POINT('Ctrl Pts',(37.5941074697056,-9.52299406482568,-11.3162472001429));
#64156=CARTESIAN_POINT('Ctrl Pts',(37.5645001959115,-9.51976382532131,-11.289255702678));
#64157=CARTESIAN_POINT('Ctrl Pts',(37.4437735190235,-9.50639330777485,-11.1735425343538));
#64158=CARTESIAN_POINT('Ctrl Pts',(37.35908429678,-9.49651381648505,-11.0784020242759));
#64159=CARTESIAN_POINT('Ctrl Pts',(37.2049198972074,-9.47647317360568,-10.8747943171741));
#64160=CARTESIAN_POINT('Ctrl Pts',(37.1358353763201,-9.46634017822809,-10.7665742172343));
#64161=CARTESIAN_POINT('Ctrl Pts',(37.060618810308,-9.45326726000504,-10.6249707271652));
#64162=CARTESIAN_POINT('Ctrl Pts',(37.0461024678045,-9.45062713929764,-10.5962668665065));
#64163=CARTESIAN_POINT('Ctrl Pts',(37.0232486224848,-9.44626525756486,-10.5487333469737));
#64164=CARTESIAN_POINT('Ctrl Pts',(37.0145693018241,-9.44455531067995,-10.5300717058368));
#64165=CARTESIAN_POINT('Ctrl Pts',(36.9980729350458,-9.44119654996351,-10.4933781916159));
#64166=CARTESIAN_POINT('Ctrl Pts',(36.9902352938204,-9.43954858926488,-10.4753573095408));
#64167=CARTESIAN_POINT('Ctrl Pts',(36.9720371232814,-9.43559276228321,-10.4320721704194));
#64168=CARTESIAN_POINT('Ctrl Pts',(36.9618845221947,-9.43327818522174,-10.4067241509388));
#64169=CARTESIAN_POINT('Ctrl Pts',(36.9267506914632,-9.42485891476378,-10.3144862336465));
#64170=CARTESIAN_POINT('Ctrl Pts',(36.9043218158565,-9.41867346592441,-10.2466719443444));
#64171=CARTESIAN_POINT('Ctrl Pts',(36.8249215104112,-9.39299183020817,-9.96516313493678));
#64172=CARTESIAN_POINT('Ctrl Pts',(36.7945377921274,-9.37278413225306,-9.74514521522786));
#64173=CARTESIAN_POINT('Ctrl Pts',(36.7946201670303,-9.35334798476491,-9.52410359447376));
#64174=CARTESIAN_POINT('Ctrl Pts',(36.958019684865,-9.28019056162069,-8.65357747851727));
#64175=CARTESIAN_POINT('Ctrl Pts',(36.9289224805849,-9.28692938518685,-8.72843824652977));
#64176=CARTESIAN_POINT('Ctrl Pts',(36.9036005899486,-9.29366820875302,-8.80470176169028));
#64177=CARTESIAN_POINT('Ctrl Pts',(36.8821687559105,-9.30040703231919,-8.88195158166545));
#64178=CARTESIAN_POINT('Ctrl Pts',(36.8606985388854,-9.30715792466944,-8.95933975092211));
#64179=CARTESIAN_POINT('Ctrl Pts',(36.8431324023123,-9.3139088170197,-9.03771729852912));
#64180=CARTESIAN_POINT('Ctrl Pts',(36.8295340594686,-9.32065970936996,-9.11665679976179));
#64181=CARTESIAN_POINT('Ctrl Pts',(36.8167488311576,-9.32700693130675,-9.19087610410068));
#64182=CARTESIAN_POINT('Ctrl Pts',(36.8074706247743,-9.33335415324353,-9.26559177363659));
#64183=CARTESIAN_POINT('Ctrl Pts',(36.8017103682723,-9.33970137518032,-9.34044706247925));
#64184=CARTESIAN_POINT('Ctrl Pts',(36.7970144018598,-9.3448758567364,-9.40147176200123));
#64185=CARTESIAN_POINT('Ctrl Pts',(36.7946472670224,-9.35005033829248,-9.46267794094415));
#64186=CARTESIAN_POINT('Ctrl Pts',(36.794620234193,-9.35522481984856,-9.52393856416118));
#64187=CARTESIAN_POINT('Ctrl Pts',(36.9580196445751,-9.01353011641035,-8.65357758217454));
#64188=CARTESIAN_POINT('Ctrl Pts',(36.9344154253712,-9.01871812617473,-8.71430610450518));
#64189=CARTESIAN_POINT('Ctrl Pts',(36.9132833758058,-9.02395946760844,-8.77598138396043));
#64190=CARTESIAN_POINT('Ctrl Pts',(36.8858593972149,-9.03180206969371,-8.86806699597638));
#64191=CARTESIAN_POINT('Ctrl Pts',(36.8776119862505,-9.03434065224797,-8.89784655849278));
#64192=CARTESIAN_POINT('Ctrl Pts',(36.8648949952305,-9.0385791582975,-8.94746162913789));
#64193=CARTESIAN_POINT('Ctrl Pts',(36.860099010553,-9.04026858181975,-8.96721038032214));
#64194=CARTESIAN_POINT('Ctrl Pts',(36.8511749069007,-9.04360142395969,-9.00610022573707));
#64195=CARTESIAN_POINT('Ctrl Pts',(36.8470291397489,-9.0452441409354,-9.02523567943694));
#64196=CARTESIAN_POINT('Ctrl Pts',(36.8375154918164,-9.04925763275802,-9.07189285179437));
#64197=CARTESIAN_POINT('Ctrl Pts',(36.8323945090578,-9.0516359449842,-9.09946124091152));
#64198=CARTESIAN_POINT('Ctrl Pts',(36.8159434184982,-9.06012583016564,-9.19754399402646));
#64199=CARTESIAN_POINT('Ctrl Pts',(36.8072739715262,-9.06631723385933,-9.26845922591632));
#64200=CARTESIAN_POINT('Ctrl Pts',(36.7862056400851,-9.0903382419935,-9.5410572169643));
#64201=CARTESIAN_POINT('Ctrl Pts',(36.7960737208553,-9.10873208830279,-9.74359297967492));
#64202=CARTESIAN_POINT('Ctrl Pts',(36.8400888654692,-9.13119095692045,-9.99333444517529));
#64203=CARTESIAN_POINT('Ctrl Pts',(36.8506838196181,-9.13571845453083,-10.0438759546695));
#64204=CARTESIAN_POINT('Ctrl Pts',(36.8669012853634,-9.14163130888702,-10.1104824013506));
#64205=CARTESIAN_POINT('Ctrl Pts',(36.871077766535,-9.14308264206995,-10.1268808315412));
#64206=CARTESIAN_POINT('Ctrl Pts',(36.8783146378802,-9.14548212313217,-10.1540915968782));
#64207=CARTESIAN_POINT('Ctrl Pts',(36.8812782900394,-9.14643541513576,-10.1649287558959));
#64208=CARTESIAN_POINT('Ctrl Pts',(36.887541153998,-9.14839051940489,-10.1872152055491));
#64209=CARTESIAN_POINT('Ctrl Pts',(36.8908496765499,-9.14939180205943,-10.1986614102247));
#64210=CARTESIAN_POINT('Ctrl Pts',(36.8999826216678,-9.1520742513772,-10.2293998053138));
#64211=CARTESIAN_POINT('Ctrl Pts',(36.905964828167,-9.15374682011653,-10.2486447600623));
#64212=CARTESIAN_POINT('Ctrl Pts',(36.9408847256793,-9.16306757444108,-10.3561955425281));
#64213=CARTESIAN_POINT('Ctrl Pts',(36.974682692969,-9.17047846023004,-10.4428538484939));
#64214=CARTESIAN_POINT('Ctrl Pts',(37.0745286436771,-9.18938183345089,-10.6606635654465));
#64215=CARTESIAN_POINT('Ctrl Pts',(37.1477032239511,-9.20073257884713,-10.7881065149531));
#64216=CARTESIAN_POINT('Ctrl Pts',(37.2772019709056,-9.21862531889779,-10.9723675120115));
#64217=CARTESIAN_POINT('Ctrl Pts',(37.3254922330012,-9.22493757626348,-11.0343850744063));
#64218=CARTESIAN_POINT('Ctrl Pts',(37.395097264099,-9.23367082741551,-11.1152743215673));
#64219=CARTESIAN_POINT('Ctrl Pts',(37.4138419100591,-9.23598986623126,-11.1362993039434));
#64220=CARTESIAN_POINT('Ctrl Pts',(37.4463836399599,-9.23996493004659,-11.1715341173834));
#64221=CARTESIAN_POINT('Ctrl Pts',(37.4599952739039,-9.24161312674279,-11.1859119308212));
#64222=CARTESIAN_POINT('Ctrl Pts',(37.4862807812569,-9.24476992453289,-11.2129992527201));
#64223=CARTESIAN_POINT('Ctrl Pts',(37.4989225254221,-9.24627706924369,-11.2257382003176));
#64224=CARTESIAN_POINT('Ctrl Pts',(37.5289868941784,-9.24983650513509,-11.2553631954002));
#64225=CARTESIAN_POINT('Ctrl Pts',(37.5465244697505,-9.25189377398882,-11.272129121169));
#64226=CARTESIAN_POINT('Ctrl Pts',(37.611572031719,-9.25945832746464,-11.3324579566349));
#64227=CARTESIAN_POINT('Ctrl Pts',(37.6605697484187,-9.26503186677864,-11.3743676032643));
#64228=CARTESIAN_POINT('Ctrl Pts',(37.8563925814175,-9.28686185112621,-11.528684318001));
#64229=CARTESIAN_POINT('Ctrl Pts',(38.0142958621842,-9.30361025247569,-11.6259807459587));
#64230=CARTESIAN_POINT('Ctrl Pts',(38.2273307069811,-9.32460528217157,-11.7255224397344));
#64231=CARTESIAN_POINT('Ctrl Pts',(38.273575581874,-9.32907008738731,-11.7453880449763));
#64232=CARTESIAN_POINT('Ctrl Pts',(38.3517252761918,-9.33643034117287,-11.7760919049392));
#64233=CARTESIAN_POINT('Ctrl Pts',(38.3832949506832,-9.339354646512,-11.7877368321361));
#64234=CARTESIAN_POINT('Ctrl Pts',(38.4288006870547,-9.34349097261239,-11.8034456579335));
#64235=CARTESIAN_POINT('Ctrl Pts',(38.4425435453908,-9.34472999517254,-11.808051192705));
#64236=CARTESIAN_POINT('Ctrl Pts',(38.4666673642307,-9.34688625079088,-11.8158937986996));
#64237=CARTESIAN_POINT('Ctrl Pts',(38.4770298073106,-9.34780643222435,-11.8191850996326));
#64238=CARTESIAN_POINT('Ctrl Pts',(38.4999072029813,-9.34982454929236,-11.826280967285));
#64239=CARTESIAN_POINT('Ctrl Pts',(38.5124313225082,-9.35092070520118,-11.8300538720609));
#64240=CARTESIAN_POINT('Ctrl Pts',(38.5497434597968,-9.354162529741,-11.8409630181109));
#64241=CARTESIAN_POINT('Ctrl Pts',(38.5746172301577,-9.35629250864609,-11.8478032253696));
#64242=CARTESIAN_POINT('Ctrl Pts',(38.7032275648562,-9.36716964162247,-11.8809547502022));
#64243=CARTESIAN_POINT('Ctrl Pts',(38.8085395211198,-9.37562660110951,-11.9007252948594));
#64244=CARTESIAN_POINT('Ctrl Pts',(39.0086154395789,-9.39144839220423,-11.9246136583454));
#64245=CARTESIAN_POINT('Ctrl Pts',(39.102976178276,-9.39881074545997,-11.9302775006137));
#64246=CARTESIAN_POINT('Ctrl Pts',(39.2994307137867,-9.41430456385499,-11.9304878335481));
#64247=CARTESIAN_POINT('Ctrl Pts',(39.401327521681,-9.42243554854533,-11.9241083793512));
#64248=CARTESIAN_POINT('Ctrl Pts',(39.5326370092824,-9.43324446802153,-11.9074626451227));
#64249=CARTESIAN_POINT('Ctrl Pts',(39.5626951781424,-9.4357410269147,-11.9030722604324));
#64250=CARTESIAN_POINT('Ctrl Pts',(39.6126083336388,-9.43992875992945,-11.8948135167427));
#64251=CARTESIAN_POINT('Ctrl Pts',(39.6325127778823,-9.44160996348719,-11.8912616900869));
#64252=CARTESIAN_POINT('Ctrl Pts',(39.6716740346309,-9.44494122061502,-11.8837629978567));
#64253=CARTESIAN_POINT('Ctrl Pts',(39.690931945976,-9.44659071079216,-11.8798301532031));
#64254=CARTESIAN_POINT('Ctrl Pts',(39.7335216176593,-9.45026495468826,-11.8705873741876));
#64255=CARTESIAN_POINT('Ctrl Pts',(39.7568263786638,-9.45229312518751,-11.865164468919));
#64256=CARTESIAN_POINT('Ctrl Pts',(39.8390167320672,-9.45951127684508,-11.844741985784));
#64257=CARTESIAN_POINT('Ctrl Pts',(39.897405579748,-9.4647592603458,-11.82786111959));
#64258=CARTESIAN_POINT('Ctrl Pts',(40.1350838547624,-9.48664071325854,-11.7492777377663));
#64259=CARTESIAN_POINT('Ctrl Pts',(40.3073969641814,-9.5038163855517,-11.6686990442503));
#64260=CARTESIAN_POINT('Ctrl Pts',(40.5111444269179,-9.52522670498369,-11.5422457551159));
#64261=CARTESIAN_POINT('Ctrl Pts',(40.5530194624337,-9.52968752121862,-11.5144017163747));
#64262=CARTESIAN_POINT('Ctrl Pts',(40.6213940994178,-9.5370420179428,-11.4657787623434));
#64263=CARTESIAN_POINT('Ctrl Pts',(40.6483849584916,-9.53996450285203,-11.4457198492305));
#64264=CARTESIAN_POINT('Ctrl Pts',(40.686394315102,-9.54409874875633,-11.416215175119));
#64265=CARTESIAN_POINT('Ctrl Pts',(40.6977602814479,-9.54533747605842,-11.4072266257179));
#64266=CARTESIAN_POINT('Ctrl Pts',(40.7175111228534,-9.5474934127188,-11.391314854948));
#64267=CARTESIAN_POINT('Ctrl Pts',(40.7259312508121,-9.54841356736591,-11.3844367380608));
#64268=CARTESIAN_POINT('Ctrl Pts',(40.7443800029017,-9.55043186052524,-11.3691568495542));
#64269=CARTESIAN_POINT('Ctrl Pts',(40.7543870965754,-9.55152821692362,-11.3607300612231));
#64270=CARTESIAN_POINT('Ctrl Pts',(40.7833327016928,-9.55470582553626,-11.335949082968));
#64271=CARTESIAN_POINT('Ctrl Pts',(40.8020861754531,-9.55677263608426,-11.3193798542235));
#64272=CARTESIAN_POINT('Ctrl Pts',(40.9131619938549,-9.56908871980126,-11.2181111696449));
#64273=CARTESIAN_POINT('Ctrl Pts',(40.9990233367886,-9.57892995906961,-11.1265847931235));
#64274=CARTESIAN_POINT('Ctrl Pts',(41.154860317439,-9.5984664254528,-10.9320313635483));
#64275=CARTESIAN_POINT('Ctrl Pts',(41.2247506456372,-9.6081353811315,-10.8294531332533));
#64276=CARTESIAN_POINT('Ctrl Pts',(41.3083526330411,-9.62156262916336,-10.6837252597242));
#64277=CARTESIAN_POINT('Ctrl Pts',(41.3292262521221,-9.62511057235681,-10.6449063352985));
#64278=CARTESIAN_POINT('Ctrl Pts',(41.3651448517381,-9.63160982123405,-10.5734698693304));
#64279=CARTESIAN_POINT('Ctrl Pts',(41.3805481817686,-9.63454886559171,-10.5410465804955));
#64280=CARTESIAN_POINT('Ctrl Pts',(41.4039444249854,-9.63927464161083,-10.4888140115401));
#64281=CARTESIAN_POINT('Ctrl Pts',(41.4124093548565,-9.64104535649277,-10.4692209820813));
#64282=CARTESIAN_POINT('Ctrl Pts',(41.4280501107404,-9.64443843451144,-10.4316532632785));
#64283=CARTESIAN_POINT('Ctrl Pts',(41.4352719504081,-9.64605910535436,-10.4136994412727));
#64284=CARTESIAN_POINT('Ctrl Pts',(41.4514469436813,-9.64981856816897,-10.3720428121556));
#64285=CARTESIAN_POINT('Ctrl Pts',(41.4602436023868,-9.65196232957961,-10.3482822226648));
#64286=CARTESIAN_POINT('Ctrl Pts',(41.4878101753346,-9.65902191197186,-10.2700483023016));
#64287=CARTESIAN_POINT('Ctrl Pts',(41.5049970219363,-9.66398760806054,-10.2150434099349));
#64288=CARTESIAN_POINT('Ctrl Pts',(41.5426964490361,-9.67645043885916,-10.0771825211629));
#64289=CARTESIAN_POINT('Ctrl Pts',(41.5608044380972,-9.68400917891454,-9.99375545354374));
#64290=CARTESIAN_POINT('Ctrl Pts',(41.6021819969037,-9.70714973416176,-9.73826647628879));
#64291=CARTESIAN_POINT('Ctrl Pts',(41.6113085376177,-9.72291560244844,-9.56447720947855));
#64292=CARTESIAN_POINT('Ctrl Pts',(41.6002690151893,-9.74019628992671,-9.36630602395826));
#64293=CARTESIAN_POINT('Ctrl Pts',(41.5984942461151,-9.74235258560614,-9.34142270700628));
#64294=CARTESIAN_POINT('Ctrl Pts',(41.5952004462384,-9.74560936749034,-9.30355367512303));
#64295=CARTESIAN_POINT('Ctrl Pts',(41.5939622219895,-9.74672354689406,-9.29054625901079));
#64296=CARTESIAN_POINT('Ctrl Pts',(41.5914993518288,-9.74875441272202,-9.26673261381967));
#64297=CARTESIAN_POINT('Ctrl Pts',(41.5903073766744,-9.74967271215101,-9.25592408483536));
#64298=CARTESIAN_POINT('Ctrl Pts',(41.5873534570663,-9.75180723904353,-9.23070927653705));
#64299=CARTESIAN_POINT('Ctrl Pts',(41.5855343767785,-9.75302034946539,-9.21631030329359));
#64300=CARTESIAN_POINT('Ctrl Pts',(41.579050542142,-9.75703396569632,-9.1684733605748));
#64301=CARTESIAN_POINT('Ctrl Pts',(41.5738119010657,-9.75980569281046,-9.13511523659956));
#64302=CARTESIAN_POINT('Ctrl Pts',(41.5589770417625,-9.76666155625317,-9.05209689660818));
#64303=CARTESIAN_POINT('Ctrl Pts',(41.5485136017834,-9.7707107051752,-9.00260678332336));
#64304=CARTESIAN_POINT('Ctrl Pts',(41.5097811595432,-9.78365199973941,-8.84426028245814));
#64305=CARTESIAN_POINT('Ctrl Pts',(41.4754391271478,-9.79239790701268,-8.73704407953041));
#64306=CARTESIAN_POINT('Ctrl Pts',(41.3873680148016,-9.81103431007076,-8.51659284458178));
#64307=CARTESIAN_POINT('Ctrl Pts',(41.3320517945614,-9.82091914870271,-8.40436975377723));
#64308=CARTESIAN_POINT('Ctrl Pts',(41.2518987335009,-9.83372037203025,-8.2693751724872));
#64309=CARTESIAN_POINT('Ctrl Pts',(41.2349708596009,-9.83635380046167,-8.24212217063219));
#64310=CARTESIAN_POINT('Ctrl Pts',(41.206308016301,-9.84070727654865,-8.19797180341846));
#64311=CARTESIAN_POINT('Ctrl Pts',(41.1948919232908,-9.84241559597815,-8.18087134152878));
#64312=CARTESIAN_POINT('Ctrl Pts',(41.1721365950787,-9.84577306863913,-8.14771407594685));
#64313=CARTESIAN_POINT('Ctrl Pts',(41.1608169535158,-9.8474213876668,-8.13164574062517));
#64314=CARTESIAN_POINT('Ctrl Pts',(41.1332792310059,-9.85138126940241,-8.09355588032824));
#64315=CARTESIAN_POINT('Ctrl Pts',(41.116880376171,-9.85369958468706,-8.07166922431114));
#64316=CARTESIAN_POINT('Ctrl Pts',(41.0561061641709,-9.86215427564569,-7.99337555530586));
#64317=CARTESIAN_POINT('Ctrl Pts',(41.009589760205,-9.868372332876,-7.93868786556885));
#64318=CARTESIAN_POINT('Ctrl Pts',(40.8782804376939,-9.88529719817478,-7.79761386017638));
#64319=CARTESIAN_POINT('Ctrl Pts',(40.7893026268582,-9.89614207952887,-7.71541463097446));
#64320=CARTESIAN_POINT('Ctrl Pts',(40.6022005687849,-9.91760229513573,-7.5670490247789));
#64321=CARTESIAN_POINT('Ctrl Pts',(40.5046042990956,-9.9281867129792,-7.50070951495733));
#64322=CARTESIAN_POINT('Ctrl Pts',(40.3803034851884,-9.94068756863581,-7.4289572605237));
#64323=CARTESIAN_POINT('Ctrl Pts',(40.3578732834571,-9.94290648671804,-7.41648367261546));
#64324=CARTESIAN_POINT('Ctrl Pts',(40.3237382186541,-9.94622371919711,-7.39820998840165));
#64325=CARTESIAN_POINT('Ctrl Pts',(40.3121796531136,-9.94733684359566,-7.3921428127624));
#64326=CARTESIAN_POINT('Ctrl Pts',(40.2918721734471,-9.94927415600868,-7.38169324980225));
#64327=CARTESIAN_POINT('Ctrl Pts',(40.2831454158522,-9.95010075030636,-7.37726987603079));
#64328=CARTESIAN_POINT('Ctrl Pts',(40.2619787855003,-9.95209156764051,-7.36670287614843));
#64329=CARTESIAN_POINT('Ctrl Pts',(40.2495123686742,-9.95325250933276,-7.36061342810938));
#64330=CARTESIAN_POINT('Ctrl Pts',(40.2098973011235,-9.95690745735638,-7.34168550134192));
#64331=CARTESIAN_POINT('Ctrl Pts',(40.1825591575719,-9.95937926365402,-7.32924671021298));
#64332=CARTESIAN_POINT('Ctrl Pts',(40.115637547872,-9.96532623098157,-7.30029787650304));
#64333=CARTESIAN_POINT('Ctrl Pts',(40.0758306760907,-9.96877725176993,-7.28432759902196));
#64334=CARTESIAN_POINT('Ctrl Pts',(39.896715422316,-9.98401715607191,-7.21797124708811));
#64335=CARTESIAN_POINT('Ctrl Pts',(39.753352482418,-9.99546803917869,-7.17945097993236));
#64336=CARTESIAN_POINT('Ctrl Pts',(39.5047537849347,-10.0153450547201,-7.13673394022701));
#64337=CARTESIAN_POINT('Ctrl Pts',(39.4011346862367,-10.0236325808985,-7.12578556124515));
#64338=CARTESIAN_POINT('Ctrl Pts',(39.2659092406184,-10.0346756155144,-7.12031998038202));
#64339=CARTESIAN_POINT('Ctrl Pts',(39.2346563370499,-10.0372430319197,-7.11966659659776));
#64340=CARTESIAN_POINT('Ctrl Pts',(39.1830064712796,-10.0415164391197,-7.11959356833189));
#64341=CARTESIAN_POINT('Ctrl Pts',(39.162613087625,-10.0432115614634,-7.11982411310598));
#64342=CARTESIAN_POINT('Ctrl Pts',(39.1224746869288,-10.0465647348121,-7.120788466116));
#64343=CARTESIAN_POINT('Ctrl Pts',(39.1027308734574,-10.0482221595811,-7.12150630516188));
#64344=CARTESIAN_POINT('Ctrl Pts',(39.0550998320814,-10.052241306479,-7.12382589514023));
#64345=CARTESIAN_POINT('Ctrl Pts',(39.0272280011592,-10.0546103157471,-7.12567033619452));
#64346=CARTESIAN_POINT('Ctrl Pts',(38.9231233594639,-10.0635273776686,-7.13438281886791));
#64347=CARTESIAN_POINT('Ctrl Pts',(38.8472086339259,-10.0701695500691,-7.14440202120306));
#64348=CARTESIAN_POINT('Ctrl Pts',(38.635221156407,-10.089127689256,-7.1827420198866));
#64349=CARTESIAN_POINT('Ctrl Pts',(38.5009438561124,-10.1016359384576,-7.21925489642919));
#64350=CARTESIAN_POINT('Ctrl Pts',(38.2740423966006,-10.1233335438638,-7.30260639305684));
#64351=CARTESIAN_POINT('Ctrl Pts',(38.179862504395,-10.1325146704086,-7.34423048354423));
#64352=CARTESIAN_POINT('Ctrl Pts',(38.0705633385727,-10.1431913812666,-7.40117311910755));
#64353=CARTESIAN_POINT('Ctrl Pts',(38.0526192474599,-10.1449447697072,-7.41081332768427));
#64354=CARTESIAN_POINT('Ctrl Pts',(38.0243352861874,-10.1477070103589,-7.42647468893905));
#64355=CARTESIAN_POINT('Ctrl Pts',(38.0139146940803,-10.1487243672929,-7.43234673995433));
#64356=CARTESIAN_POINT('Ctrl Pts',(37.9938151877964,-10.1506854280061,-7.4438712787138));
#64357=CARTESIAN_POINT('Ctrl Pts',(37.9841313322134,-10.1516296311222,-7.4495140454382));
#64358=CARTESIAN_POINT('Ctrl Pts',(37.9600500222372,-10.153976928477,-7.46377257541043));
#64359=CARTESIAN_POINT('Ctrl Pts',(37.9457021943752,-10.1553748567722,-7.47247192292882));
#64360=CARTESIAN_POINT('Ctrl Pts',(37.8886789585346,-10.1609333343494,-7.50786743237705));
#64361=CARTESIAN_POINT('Ctrl Pts',(37.8467514365339,-10.1650263304812,-7.53575240065824));
#64362=CARTESIAN_POINT('Ctrl Pts',(37.630315254609,-10.1863664489294,-7.68971230660831));
#64363=CARTESIAN_POINT('Ctrl Pts',(37.472439723281,-10.2027647859929,-7.83747490581266));
#64364=CARTESIAN_POINT('Ctrl Pts',(37.2965956220547,-10.2249978555818,-8.05297620016607));
#64365=CARTESIAN_POINT('Ctrl Pts',(37.2587918025823,-10.2300738902301,-8.10320122378667));
#64366=CARTESIAN_POINT('Ctrl Pts',(37.2092736239237,-10.2371987324867,-8.17465109891706));
#64367=CARTESIAN_POINT('Ctrl Pts',(37.1958458164185,-10.2391840930391,-8.19466185397618));
#64368=CARTESIAN_POINT('Ctrl Pts',(37.1729669221607,-10.2426642930727,-8.22988974196906));
#64369=CARTESIAN_POINT('Ctrl Pts',(37.1633807808665,-10.2441540693138,-8.2450172660976));
#64370=CARTESIAN_POINT('Ctrl Pts',(37.1435335308567,-10.2473072885702,-8.27712493463417));
#64371=CARTESIAN_POINT('Ctrl Pts',(37.133311854702,-10.2489720165361,-8.29412771694485));
#64372=CARTESIAN_POINT('Ctrl Pts',(37.1089788465773,-10.2530373991254,-8.33576108067051));
#64373=CARTESIAN_POINT('Ctrl Pts',(37.095091320872,-10.2554457618124,-8.36051815146242));
#64374=CARTESIAN_POINT('Ctrl Pts',(37.0435060037021,-10.2647448590642,-8.45641751422547));
#64375=CARTESIAN_POINT('Ctrl Pts',(37.0089550976382,-10.2717407321173,-8.52918173924758));
#64376=CARTESIAN_POINT('Ctrl Pts',(36.9712314234316,-10.2804210444538,-8.62014259324087));
#64377=CARTESIAN_POINT('Ctrl Pts',(36.9645309575376,-10.2820103420603,-8.63682539037184));
#64378=CARTESIAN_POINT('Ctrl Pts',(36.9580196499262,-10.2836033739986,-8.65357756840738));
#64379=CARTESIAN_POINT('Origin',(39.2,8.05522481984854,-9.525));
#64380=CARTESIAN_POINT('',(36.9580196917093,-11.8220201063326,-8.65357746090844));
#64381=CARTESIAN_POINT('',(36.9580196848654,-11.5570870138823,-8.65357747851634));
#64382=CARTESIAN_POINT('',(36.958019684865,8.05522481984854,-8.65357747851728));
#64383=CARTESIAN_POINT('Ctrl Pts',(36.9580196917093,-11.8220201063326,-8.65357746090844));
#64384=CARTESIAN_POINT('Ctrl Pts',(37.0195222368154,-11.8071546836758,-8.49534481388361));
#64385=CARTESIAN_POINT('Ctrl Pts',(37.0976042895335,-11.7918150351386,-8.34406686960644));
#64386=CARTESIAN_POINT('Ctrl Pts',(37.2243281706615,-11.7711587714622,-8.15158924554521));
#64387=CARTESIAN_POINT('Ctrl Pts',(37.2596109124396,-11.7657471775599,-8.10217621399113));
#64388=CARTESIAN_POINT('Ctrl Pts',(37.3045735023623,-11.7592799084008,-8.04399494539265));
#64389=CARTESIAN_POINT('Ctrl Pts',(37.3125007825056,-11.7581547439394,-8.03390499971234));
#64390=CARTESIAN_POINT('Ctrl Pts',(37.3362178562845,-11.7548336594147,-8.00420984006869));
#64391=CARTESIAN_POINT('Ctrl Pts',(37.3522358010931,-11.7526488305522,-7.9847876118182));
#64392=CARTESIAN_POINT('Ctrl Pts',(37.3688690972522,-11.7504410356872,-7.96525233010145));
#64393=CARTESIAN_POINT('Ctrl Pts',(37.3691817017606,-11.7503995641396,-7.96488540946997));
#64394=CARTESIAN_POINT('Ctrl Pts',(37.3697839232714,-11.7503197121562,-7.96417898014284));
#64395=CARTESIAN_POINT('Ctrl Pts',(37.3700735244568,-11.75028133074,-7.96383945807921));
#64396=CARTESIAN_POINT('Ctrl Pts',(37.3706319534729,-11.7502073566368,-7.96318513705621));
#64397=CARTESIAN_POINT('Ctrl Pts',(37.3709007680591,-11.7501717631295,-7.96287032693173));
#64398=CARTESIAN_POINT('Ctrl Pts',(37.3714195888865,-11.750103097176,-7.96226305075639));
#64399=CARTESIAN_POINT('Ctrl Pts',(37.3716695840387,-11.7500700240347,-7.96197057528958));
#64400=CARTESIAN_POINT('Ctrl Pts',(37.3721525125285,-11.7500061614658,-7.96140585978445));
#64401=CARTESIAN_POINT('Ctrl Pts',(37.3723854364694,-11.749975371457,-7.96113361186337));
#64402=CARTESIAN_POINT('Ctrl Pts',(37.3819792837052,-11.7487076597144,-7.94992512951868));
#64403=CARTESIAN_POINT('Ctrl Pts',(37.3914385004635,-11.747476956279,-7.93907266648057));
#64404=CARTESIAN_POINT('Ctrl Pts',(37.4081823772785,-11.7453327514335,-7.92020724389243));
#64405=CARTESIAN_POINT('Ctrl Pts',(37.4154244249836,-11.7444163577425,-7.91215772084796));
#64406=CARTESIAN_POINT('Ctrl Pts',(37.431526990034,-11.7424029053641,-7.89450101638728));
#64407=CARTESIAN_POINT('Ctrl Pts',(37.4404117415958,-11.7413076556525,-7.88491679848045));
#64408=CARTESIAN_POINT('Ctrl Pts',(37.4670098820244,-11.7380732117081,-7.85668963548916));
#64409=CARTESIAN_POINT('Ctrl Pts',(37.4849453534326,-11.7359495871312,-7.83825700165438));
#64410=CARTESIAN_POINT('Ctrl Pts',(37.5847524841808,-11.7244162263516,-7.73892169664024));
#64411=CARTESIAN_POINT('Ctrl Pts',(37.6720654790745,-11.7153454391813,-7.66367683318644));
#64412=CARTESIAN_POINT('Ctrl Pts',(37.8616071265024,-11.6968157202338,-7.5226960349588));
#64413=CARTESIAN_POINT('Ctrl Pts',(37.9640843881882,-11.6873845172794,-7.45786979289354));
#64414=CARTESIAN_POINT('Ctrl Pts',(38.1362960797734,-11.6718615008937,-7.36633037895077));
#64415=CARTESIAN_POINT('Ctrl Pts',(38.2031474330634,-11.6659101500289,-7.33465674946773));
#64416=CARTESIAN_POINT('Ctrl Pts',(38.296862276295,-11.6575912792807,-7.29543494156573));
#64417=CARTESIAN_POINT('Ctrl Pts',(38.3225602408113,-11.6553127294249,-7.2851970088896));
#64418=CARTESIAN_POINT('Ctrl Pts',(38.3668955358238,-11.651382461485,-7.26841412360326));
#64419=CARTESIAN_POINT('Ctrl Pts',(38.3854478718677,-11.649738062565,-7.26165123155069));
#64420=CARTESIAN_POINT('Ctrl Pts',(38.4234660880219,-11.64636748542,-7.24832039560665));
#64421=CARTESIAN_POINT('Ctrl Pts',(38.4429369975882,-11.6446408279038,-7.24177191415941));
#64422=CARTESIAN_POINT('Ctrl Pts',(38.4927768647658,-11.6402185146263,-7.22571729865245));
#64423=CARTESIAN_POINT('Ctrl Pts',(38.523253968771,-11.6375118177066,-7.21656327676573));
#64424=CARTESIAN_POINT('Ctrl Pts',(38.664175965299,-11.6249782284927,-7.17726674543057));
#64425=CARTESIAN_POINT('Ctrl Pts',(38.7764852118321,-11.6149282994709,-7.15443343461381));
#64426=CARTESIAN_POINT('Ctrl Pts',(39.026615993977,-11.5924443976172,-7.12192345211543));
#64427=CARTESIAN_POINT('Ctrl Pts',(39.1645252726663,-11.5799772490267,-7.11593805667749));
#64428=CARTESIAN_POINT('Ctrl Pts',(39.3633490766828,-11.5622878086934,-7.12439224120074));
#64429=CARTESIAN_POINT('Ctrl Pts',(39.4243966546015,-11.5568986809718,-7.12932717255241));
#64430=CARTESIAN_POINT('Ctrl Pts',(39.5029757819074,-11.5500646614959,-7.13871014658836));
#64431=CARTESIAN_POINT('Ctrl Pts',(39.5207325836487,-11.548527223667,-7.14103182541052));
#64432=CARTESIAN_POINT('Ctrl Pts',(39.5498109836354,-11.5460224885509,-7.14516458398484));
#64433=CARTESIAN_POINT('Ctrl Pts',(39.5611481033032,-11.5450491832041,-7.14685862529736));
#64434=CARTESIAN_POINT('Ctrl Pts',(39.5826078660378,-11.5432135096309,-7.15022224146873));
#64435=CARTESIAN_POINT('Ctrl Pts',(39.5927326732926,-11.5423502429387,-7.15187563723592));
#64436=CARTESIAN_POINT('Ctrl Pts',(39.620206445833,-11.5400146197291,-7.15654279369386));
#64437=CARTESIAN_POINT('Ctrl Pts',(39.637533886892,-11.5385490123967,-7.15968244220655));
#64438=CARTESIAN_POINT('Ctrl Pts',(39.7074110032163,-11.5326628278137,-7.17313803008069));
#64439=CARTESIAN_POINT('Ctrl Pts',(39.7596486613197,-11.5283180062888,-7.18501811655564));
#64440=CARTESIAN_POINT('Ctrl Pts',(39.9533989118675,-11.5122595782045,-7.23594252906467));
#64441=CARTESIAN_POINT('Ctrl Pts',(40.0916442762226,-11.5009005542583,-7.28616743490815));
#64442=CARTESIAN_POINT('Ctrl Pts',(40.329224786239,-11.4802516527406,-7.39800380030746));
#64443=CARTESIAN_POINT('Ctrl Pts',(40.4302806875294,-11.4710616282955,-7.45481521743878));
#64444=CARTESIAN_POINT('Ctrl Pts',(40.5529540547388,-11.4590608071579,-7.53594289813821));
#64445=CARTESIAN_POINT('Ctrl Pts',(40.5787231066101,-11.4564896875235,-7.55371736125102));
#64446=CARTESIAN_POINT('Ctrl Pts',(40.620710760708,-11.4522109894795,-7.58390480255449));
#64447=CARTESIAN_POINT('Ctrl Pts',(40.6371318001931,-11.4505143131566,-7.59603090577427));
#64448=CARTESIAN_POINT('Ctrl Pts',(40.6689673515638,-11.4471774759012,-7.62017198771938));
#64449=CARTESIAN_POINT('Ctrl Pts',(40.6843937191474,-11.4455381153245,-7.63216876748468));
#64450=CARTESIAN_POINT('Ctrl Pts',(40.7179837501729,-11.4419175238457,-7.65895422361889));
#64451=CARTESIAN_POINT('Ctrl Pts',(40.7360807990141,-11.4399332453863,-7.67382275271356));
#64452=CARTESIAN_POINT('Ctrl Pts',(40.7985070376105,-11.4329671290314,-7.72665782777859));
#64453=CARTESIAN_POINT('Ctrl Pts',(40.841665473089,-11.4279320845181,-7.76596828980467));
#64454=CARTESIAN_POINT('Ctrl Pts',(41.0421755785805,-11.403430760465,-7.96241191243846));
#64455=CARTESIAN_POINT('Ctrl Pts',(41.1786505420858,-11.3831518322833,-8.13928504758494));
#64456=CARTESIAN_POINT('Ctrl Pts',(41.3137051728022,-11.3590453381884,-8.37582095550486));
#64457=CARTESIAN_POINT('Ctrl Pts',(41.3371797435689,-11.3546548590138,-8.42009015976991));
#64458=CARTESIAN_POINT('Ctrl Pts',(41.3666384748711,-11.3488898535286,-8.4801022567753));
#64459=CARTESIAN_POINT('Ctrl Pts',(41.3738633161429,-11.347453247059,-8.49521754417655));
#64460=CARTESIAN_POINT('Ctrl Pts',(41.3856551655224,-11.3450711785047,-8.52056486679085));
#64461=CARTESIAN_POINT('Ctrl Pts',(41.3903095596056,-11.3441207238461,-8.53075531402184));
#64462=CARTESIAN_POINT('Ctrl Pts',(41.3997866770966,-11.3421644541308,-8.55189433930267));
#64463=CARTESIAN_POINT('Ctrl Pts',(41.4045992022457,-11.3411592316009,-8.56284698290802));
#64464=CARTESIAN_POINT('Ctrl Pts',(41.4173950150876,-11.3384527280887,-8.59256862531486));
#64465=CARTESIAN_POINT('Ctrl Pts',(41.4252218816092,-11.3367603257791,-8.61140458410712));
#64466=CARTESIAN_POINT('Ctrl Pts',(41.4735975747839,-11.3260429539613,-8.73213594129483));
#64467=CARTESIAN_POINT('Ctrl Pts',(41.5073837384875,-11.3173526131309,-8.83661993110928));
#64468=CARTESIAN_POINT('Ctrl Pts',(41.5553543782027,-11.3017676870822,-9.02901063007428));
#64469=CARTESIAN_POINT('Ctrl Pts',(41.5720209596351,-11.2948618796711,-9.11607906777508));
#64470=CARTESIAN_POINT('Ctrl Pts',(41.5989223045068,-11.2790101483759,-9.31577503321823));
#64471=CARTESIAN_POINT('Ctrl Pts',(41.606096997276,-11.2700413059539,-9.42858939908781));
#64472=CARTESIAN_POINT('Ctrl Pts',(41.6051103870479,-11.2582897474402,-9.5725917650785));
#64473=CARTESIAN_POINT('Ctrl Pts',(41.6042936235563,-11.2557340979116,-9.60369525065076));
#64474=CARTESIAN_POINT('Ctrl Pts',(41.6019448565877,-11.2514756369124,-9.65510865733092));
#64475=CARTESIAN_POINT('Ctrl Pts',(41.6007577412977,-11.2497835576421,-9.67543128407569));
#64476=CARTESIAN_POINT('Ctrl Pts',(41.5979261762536,-11.2464518162339,-9.71522265886003));
#64477=CARTESIAN_POINT('Ctrl Pts',(41.5963021745664,-11.2448129153817,-9.73469131303294));
#64478=CARTESIAN_POINT('Ctrl Pts',(41.5917890010068,-11.2408201578185,-9.78185309414413));
#64479=CARTESIAN_POINT('Ctrl Pts',(41.588655846342,-11.2384589336017,-9.80951932264566));
#64480=CARTESIAN_POINT('Ctrl Pts',(41.5759554407952,-11.2301053614676,-9.90656743512703));
#64481=CARTESIAN_POINT('Ctrl Pts',(41.5638400520901,-11.2240364975671,-9.97557306420601));
#64482=CARTESIAN_POINT('Ctrl Pts',(41.5047640422709,-11.1999937477026,-10.2429497519612));
#64483=CARTESIAN_POINT('Ctrl Pts',(41.4356905819047,-11.1814334847706,-10.4355268394577));
#64484=CARTESIAN_POINT('Ctrl Pts',(41.3196780700855,-11.1588007556919,-10.663199214008));
#64485=CARTESIAN_POINT('Ctrl Pts',(41.2946908038853,-11.1542602388255,-10.7085556906512));
#64486=CARTESIAN_POINT('Ctrl Pts',(41.259613007265,-11.1483339703858,-10.7676318165868));
#64487=CARTESIAN_POINT('Ctrl Pts',(41.2508154771883,-11.1468817937277,-10.7820980472147));
#64488=CARTESIAN_POINT('Ctrl Pts',(41.2359282272724,-11.1444816548536,-10.8060056057672));
#64489=CARTESIAN_POINT('Ctrl Pts',(41.2299239398314,-11.143528533282,-10.8154991012039));
#64490=CARTESIAN_POINT('Ctrl Pts',(41.217415886543,-11.1415738445939,-10.8349725034995));
#64491=CARTESIAN_POINT('Ctrl Pts',(41.2109041376472,-11.1405728049616,-10.84494673657));
#64492=CARTESIAN_POINT('Ctrl Pts',(41.1931917250614,-11.1378927764832,-10.871642012258));
#64493=CARTESIAN_POINT('Ctrl Pts',(41.1818545231596,-11.1362223535868,-10.8882720538359));
#64494=CARTESIAN_POINT('Ctrl Pts',(41.1174879701893,-11.1269725938104,-10.9801881435499));
#64495=CARTESIAN_POINT('Ctrl Pts',(41.0603708219234,-11.1196261435177,-11.0525332709065));
#64496=CARTESIAN_POINT('Ctrl Pts',(40.9014456362142,-11.1007300890364,-11.2316476080352));
#64497=CARTESIAN_POINT('Ctrl Pts',(40.7937363377978,-11.089327744614,-11.3326415028221));
#64498=CARTESIAN_POINT('Ctrl Pts',(40.6153230183019,-11.071366618117,-11.4715134424039));
#64499=CARTESIAN_POINT('Ctrl Pts',(40.5508517925976,-11.0650399920595,-11.5167959093007));
#64500=CARTESIAN_POINT('Ctrl Pts',(40.4604401461102,-11.0562893734585,-11.5738871800599));
#64501=CARTESIAN_POINT('Ctrl Pts',(40.4363364277138,-11.053967832134,-11.58852129645));
#64502=CARTESIAN_POINT('Ctrl Pts',(40.3948678220516,-11.0499890690345,-11.6127108014208));
#64503=CARTESIAN_POINT('Ctrl Pts',(40.3776314688782,-11.0483396961033,-11.6224817226459));
#64504=CARTESIAN_POINT('Ctrl Pts',(40.3445484759961,-11.0451810084547,-11.6406994421413));
#64505=CARTESIAN_POINT('Ctrl Pts',(40.3287240207539,-11.0436731548696,-11.649183935298));
#64506=CARTESIAN_POINT('Ctrl Pts',(40.2871589904224,-11.0397193906007,-11.6708739931416));
#64507=CARTESIAN_POINT('Ctrl Pts',(40.2612733555155,-11.0372637940236,-11.6837933140816));
#64508=CARTESIAN_POINT('Ctrl Pts',(40.163583322238,-11.02801680778,-11.7303680519948));
#64509=CARTESIAN_POINT('Ctrl Pts',(40.0903699814951,-11.0211247214396,-11.7609292011787));
#64510=CARTESIAN_POINT('Ctrl Pts',(39.8361762735025,-10.9973065390112,-11.8525710098921));
#64511=CARTESIAN_POINT('Ctrl Pts',(39.649515633545,-10.9799374337163,-11.895702646915));
#64512=CARTESIAN_POINT('Ctrl Pts',(39.4076359026872,-10.9583827891825,-11.9219744241546));
#64513=CARTESIAN_POINT('Ctrl Pts',(39.3553625440727,-10.9537852750119,-11.9259295356887));
#64514=CARTESIAN_POINT('Ctrl Pts',(39.2859992675856,-10.9477963348357,-11.9289023516445));
#64515=CARTESIAN_POINT('Ctrl Pts',(39.2689937542405,-10.946336942828,-11.9294505200274));
#64516=CARTESIAN_POINT('Ctrl Pts',(39.2407277277163,-10.943927423039,-11.9300615251131));
#64517=CARTESIAN_POINT('Ctrl Pts',(39.229470296981,-10.9429720734464,-11.9302258130321));
#64518=CARTESIAN_POINT('Ctrl Pts',(39.2078022050263,-10.9411419438774,-11.9303898710122));
#64519=CARTESIAN_POINT('Ctrl Pts',(39.1973921092614,-10.9402665093473,-11.930401113665));
#64520=CARTESIAN_POINT('Ctrl Pts',(39.1685312025315,-10.9378492171314,-11.9302449147077));
#64521=CARTESIAN_POINT('Ctrl Pts',(39.1500813325842,-10.9363149756565,-11.9299327590745));
#64522=CARTESIAN_POINT('Ctrl Pts',(39.0692034001497,-10.9296304803071,-11.9276331756873));
#64523=CARTESIAN_POINT('Ctrl Pts',(39.006856311245,-10.9245847574778,-11.9234268236468));
#64524=CARTESIAN_POINT('Ctrl Pts',(38.7915986559681,-10.9073130463647,-11.9004535848222));
#64525=CARTESIAN_POINT('Ctrl Pts',(38.6403769544948,-10.8954217297262,-11.8694399865349));
#64526=CARTESIAN_POINT('Ctrl Pts',(38.3972836927085,-10.8753551150544,-11.7947045784404));
#64527=CARTESIAN_POINT('Ctrl Pts',(38.3033645998504,-10.8673559082107,-11.759267906401));
#64528=CARTESIAN_POINT('Ctrl Pts',(38.1843612714501,-10.8566956605179,-11.7056526227532));
#64529=CARTESIAN_POINT('Ctrl Pts',(38.1570210968949,-10.8542093514122,-11.6927090972907));
#64530=CARTESIAN_POINT('Ctrl Pts',(38.1118448482176,-10.8500336717585,-11.6702690363627));
#64531=CARTESIAN_POINT('Ctrl Pts',(38.0938707171895,-10.8483541407158,-11.6610568415827));
#64532=CARTESIAN_POINT('Ctrl Pts',(38.0586145450799,-10.8450222671022,-11.6424228569449));
#64533=CARTESIAN_POINT('Ctrl Pts',(38.0413279078921,-10.8433704514099,-11.6330131037533));
#64534=CARTESIAN_POINT('Ctrl Pts',(38.0032061280026,-10.8396860013776,-11.6116514463966));
#64535=CARTESIAN_POINT('Ctrl Pts',(37.9824309105439,-10.8376498872258,-11.5995976123797));
#64536=CARTESIAN_POINT('Ctrl Pts',(37.9089609177217,-10.8303452151844,-11.555486458818));
#64537=CARTESIAN_POINT('Ctrl Pts',(37.8573275130777,-10.8250166660665,-11.52171888788));
#64538=CARTESIAN_POINT('Ctrl Pts',(37.6302323351314,-10.8006576014357,-11.3604082176992));
#64539=CARTESIAN_POINT('Ctrl Pts',(37.4712198005621,-10.7808839185243,-11.2114720860351));
#64540=CARTESIAN_POINT('Ctrl Pts',(37.3026515652698,-10.7572476118606,-11.0043391704961));
#64541=CARTESIAN_POINT('Ctrl Pts',(37.2721740260759,-10.752845264629,-10.9643969091811));
#64542=CARTESIAN_POINT('Ctrl Pts',(37.2332182424327,-10.7470674178816,-10.9098839657391));
#64543=CARTESIAN_POINT('Ctrl Pts',(37.2236120549459,-10.745629521514,-10.8961399710529));
#64544=CARTESIAN_POINT('Ctrl Pts',(37.2078263716079,-10.7432458307098,-10.8730440519958));
#64545=CARTESIAN_POINT('Ctrl Pts',(37.2015672474306,-10.7422950327158,-10.8637475820482));
#64546=CARTESIAN_POINT('Ctrl Pts',(37.1887591683886,-10.7403380799546,-10.8444341465707));
#64547=CARTESIAN_POINT('Ctrl Pts',(37.1822196160994,-10.7393325167499,-10.8344115057756));
#64548=CARTESIAN_POINT('Ctrl Pts',(37.1647394034661,-10.7366259473597,-10.8071790411262));
#64549=CARTESIAN_POINT('Ctrl Pts',(37.1539420023191,-10.7349338057897,-10.7898776795524));
#64550=CARTESIAN_POINT('Ctrl Pts',(37.0874577471661,-10.7243699231704,-10.6802661583647));
#64551=CARTESIAN_POINT('Ctrl Pts',(37.0378009606188,-10.7158208738665,-10.5844230280174));
#64552=CARTESIAN_POINT('Ctrl Pts',(36.9407480131908,-10.6967109946233,-10.3616073506474));
#64553=CARTESIAN_POINT('Ctrl Pts',(36.8973065566811,-10.6862163689718,-10.2333310587889));
#64554=CARTESIAN_POINT('Ctrl Pts',(36.8525937228548,-10.6713925919154,-10.0524047612069));
#64555=CARTESIAN_POINT('Ctrl Pts',(36.8419050820114,-10.6672909083432,-10.0023465784628));
#64556=CARTESIAN_POINT('Ctrl Pts',(36.8256923288185,-10.6598905226161,-9.91246479852545));
#64557=CARTESIAN_POINT('Ctrl Pts',(36.8195545181075,-10.6566102317367,-9.87277122553581));
#64558=CARTESIAN_POINT('Ctrl Pts',(36.8115700151325,-10.6514683029081,-9.81091688774761));
#64559=CARTESIAN_POINT('Ctrl Pts',(36.8090318658065,-10.649628100642,-9.78885142111596));
#64560=CARTESIAN_POINT('Ctrl Pts',(36.8048686574815,-10.6461781952384,-9.74763861086654));
#64561=CARTESIAN_POINT('Ctrl Pts',(36.8031667693101,-10.6445710138068,-9.72850065783374));
#64562=CARTESIAN_POINT('Ctrl Pts',(36.7998617855699,-10.6409473874819,-9.68550321698142));
#64563=CARTESIAN_POINT('Ctrl Pts',(36.7983848922809,-10.6389272034291,-9.66163643975376));
#64564=CARTESIAN_POINT('Ctrl Pts',(36.7954814940953,-10.6336653214152,-9.59976554608665));
#64565=CARTESIAN_POINT('Ctrl Pts',(36.7946001050408,-10.6304073900687,-9.56174407021846));
#64566=CARTESIAN_POINT('Ctrl Pts',(36.7947067641619,-10.6130956163816,-9.36132361716306));
#64567=CARTESIAN_POINT('Ctrl Pts',(36.8112388358979,-10.5985869402844,-9.19938264598348));
#64568=CARTESIAN_POINT('Ctrl Pts',(36.8679872736717,-10.5732732082353,-8.92349507448723));
#64569=CARTESIAN_POINT('Ctrl Pts',(36.9006948735118,-10.5625511509026,-8.80855498415655));
#64570=CARTESIAN_POINT('Ctrl Pts',(36.9470719552065,-10.5508228197936,-8.68214641616852));
#64571=CARTESIAN_POINT('Ctrl Pts',(36.9524776905052,-10.5494961679529,-8.66783582272116));
#64572=CARTESIAN_POINT('Ctrl Pts',(36.958019684939,-10.5481760837449,-8.65357747832709));
#64573=CARTESIAN_POINT('Ctrl Pts',(36.9580196499262,-10.2836033739986,-8.65357756840738));
#64574=CARTESIAN_POINT('Ctrl Pts',(36.9084867414416,-10.2957219083884,-8.78101496670975));
#64575=CARTESIAN_POINT('Ctrl Pts',(36.8699012361887,-10.3080770742071,-8.91246580418143));
#64576=CARTESIAN_POINT('Ctrl Pts',(36.8261576094698,-10.3277553664387,-9.12796664229451));
#64577=CARTESIAN_POINT('Ctrl Pts',(36.8138532195428,-10.335133254408,-9.2102459589881));
#64578=CARTESIAN_POINT('Ctrl Pts',(36.8039287097411,-10.3440412841354,-9.31266661688286));
#64579=CARTESIAN_POINT('Ctrl Pts',(36.8022657951861,-10.3457406691889,-9.33235043669171));
#64580=CARTESIAN_POINT('Ctrl Pts',(36.7999950071111,-10.3484379371115,-9.36385133724607));
#64581=CARTESIAN_POINT('Ctrl Pts',(36.7992315479296,-10.349443683289,-9.37565571453295));
#64582=CARTESIAN_POINT('Ctrl Pts',(36.797909668938,-10.3513998356577,-9.39873663268032));
#64583=CARTESIAN_POINT('Ctrl Pts',(36.7973435069549,-10.3523505877009,-9.41001224593019));
#64584=CARTESIAN_POINT('Ctrl Pts',(36.7961150936825,-10.3547393658493,-9.43847720714928));
#64585=CARTESIAN_POINT('Ctrl Pts',(36.7955577835264,-10.3561718214584,-9.45567095255194));
#64586=CARTESIAN_POINT('Ctrl Pts',(36.794009009724,-10.3620865381518,-9.52711755760656));
#64587=CARTESIAN_POINT('Ctrl Pts',(36.7946688482976,-10.3664897904078,-9.58139523367149));
#64588=CARTESIAN_POINT('Ctrl Pts',(36.8028873106598,-10.3808162537491,-9.75992956150876));
#64589=CARTESIAN_POINT('Ctrl Pts',(36.8182501684603,-10.3904986983501,-9.88362769426369));
#64590=CARTESIAN_POINT('Ctrl Pts',(36.8701406366574,-10.4108615187152,-10.1381061228902));
#64591=CARTESIAN_POINT('Ctrl Pts',(36.9082857402076,-10.4215245235867,-10.2680892633524));
#64592=CARTESIAN_POINT('Ctrl Pts',(36.969015255277,-10.4352192103108,-10.4247995537014));
#64593=CARTESIAN_POINT('Ctrl Pts',(36.9815116166847,-10.4379144720478,-10.4551834506818));
#64594=CARTESIAN_POINT('Ctrl Pts',(37.0028968720256,-10.4423430987306,-10.5042956751161));
#64595=CARTESIAN_POINT('Ctrl Pts',(37.0114128592375,-10.4440639088899,-10.5231825713195));
#64596=CARTESIAN_POINT('Ctrl Pts',(37.0284468290345,-10.4474267113169,-10.5596945883188));
#64597=CARTESIAN_POINT('Ctrl Pts',(37.0369381201021,-10.4490676831488,-10.5773304238024));
#64598=CARTESIAN_POINT('Ctrl Pts',(37.0575892724685,-10.4529781452075,-10.6189152486571));
#64599=CARTESIAN_POINT('Ctrl Pts',(37.0699366337988,-10.455253946288,-10.6427675191933));
#64600=CARTESIAN_POINT('Ctrl Pts',(37.1149603467756,-10.4633433974374,-10.7262868891846));
#64601=CARTESIAN_POINT('Ctrl Pts',(37.1497624147167,-10.469229585653,-10.7847636541255));
#64602=CARTESIAN_POINT('Ctrl Pts',(37.2540020574395,-10.4859235625733,-10.9441303991183));
#64603=CARTESIAN_POINT('Ctrl Pts',(37.3287281318592,-10.4968876624622,-11.0413027638943));
#64604=CARTESIAN_POINT('Ctrl Pts',(37.4918609597442,-10.5188273743655,-11.222920277095));
#64605=CARTESIAN_POINT('Ctrl Pts',(37.5799744628514,-10.5297706570977,-11.3071884702292));
#64606=CARTESIAN_POINT('Ctrl Pts',(37.6935144391638,-10.5425606736771,-11.4003626414968));
#64607=CARTESIAN_POINT('Ctrl Pts',(37.7131797625734,-10.5447322115027,-11.4159916748559));
#64608=CARTESIAN_POINT('Ctrl Pts',(37.7434706469762,-10.5480071633345,-11.4393006132146));
#64609=CARTESIAN_POINT('Ctrl Pts',(37.7539193318076,-10.5491244918161,-11.447205847394));
#64610=CARTESIAN_POINT('Ctrl Pts',(37.7731542373874,-10.5511581700227,-11.4615129147173));
#64611=CARTESIAN_POINT('Ctrl Pts',(37.7819196790074,-10.5520761678913,-11.4679408928559));
#64612=CARTESIAN_POINT('Ctrl Pts',(37.802448949461,-10.5542062207974,-11.4827827139772));
#64613=CARTESIAN_POINT('Ctrl Pts',(37.814245527631,-10.5554152046499,-11.4911502152087));
#64614=CARTESIAN_POINT('Ctrl Pts',(37.8535776650137,-10.5593995323423,-11.5185192578973));
#64615=CARTESIAN_POINT('Ctrl Pts',(37.8814357331471,-10.5621466670681,-11.5370538623808));
#64616=CARTESIAN_POINT('Ctrl Pts',(37.9517972183045,-10.5689261483888,-11.5817775940225));
#64617=CARTESIAN_POINT('Ctrl Pts',(37.994747418289,-10.5729245033001,-11.6072370728988));
#64618=CARTESIAN_POINT('Ctrl Pts',(38.2080392924415,-10.5922685059288,-11.7248563759732));
#64619=CARTESIAN_POINT('Ctrl Pts',(38.3882851470639,-10.6071229143317,-11.797548351));
#64620=CARTESIAN_POINT('Ctrl Pts',(38.6315881828157,-10.6273047431252,-11.8629817157395));
#64621=CARTESIAN_POINT('Ctrl Pts',(38.6884036098759,-10.6320209547872,-11.8760675443641));
#64622=CARTESIAN_POINT('Ctrl Pts',(38.7687798267058,-10.6387336432129,-11.891528608507));
#64623=CARTESIAN_POINT('Ctrl Pts',(38.7919889046969,-10.640676582182,-11.8956402846765));
#64624=CARTESIAN_POINT('Ctrl Pts',(38.8345699440263,-10.6442520436382,-11.9025400579212));
#64625=CARTESIAN_POINT('Ctrl Pts',(38.8539229053777,-10.6458811369632,-11.9054340885575));
#64626=CARTESIAN_POINT('Ctrl Pts',(38.8934589456214,-10.6492187323971,-11.9108539771598));
#64627=CARTESIAN_POINT('Ctrl Pts',(38.9136430033449,-10.6509276935298,-11.9133605746287));
#64628=CARTESIAN_POINT('Ctrl Pts',(38.9646467842253,-10.6552602751684,-11.9190387727834));
#64629=CARTESIAN_POINT('Ctrl Pts',(38.9954995406788,-10.6578941303377,-11.921871325597));
#64630=CARTESIAN_POINT('Ctrl Pts',(39.1367650399096,-10.6700198009259,-11.9320935161316));
#64631=CARTESIAN_POINT('Ctrl Pts',(39.2475338716148,-10.6797207201588,-11.9324531828017));
#64632=CARTESIAN_POINT('Ctrl Pts',(39.445286252741,-10.6973684454969,-11.9194422924778));
#64633=CARTESIAN_POINT('Ctrl Pts',(39.5322723603936,-10.7052441766121,-11.9089280761907));
#64634=CARTESIAN_POINT('Ctrl Pts',(39.7211448505958,-10.7224742174449,-11.8755591855773));
#64635=CARTESIAN_POINT('Ctrl Pts',(39.8225262277717,-10.731808167891,-11.8507657428578));
#64636=CARTESIAN_POINT('Ctrl Pts',(39.9464372578176,-10.743122127395,-11.8117753046892));
#64637=CARTESIAN_POINT('Ctrl Pts',(39.9707630614893,-10.7453382799188,-11.8036913650251));
#64638=CARTESIAN_POINT('Ctrl Pts',(40.0072707178494,-10.7486522588533,-11.7909075814864));
#64639=CARTESIAN_POINT('Ctrl Pts',(40.0195501544948,-10.7497648534031,-11.7864952461642));
#64640=CARTESIAN_POINT('Ctrl Pts',(40.0419994857473,-10.7517943590197,-11.7782217200871));
#64641=CARTESIAN_POINT('Ctrl Pts',(40.0521795753056,-10.7527128648811,-11.7743913033801));
#64642=CARTESIAN_POINT('Ctrl Pts',(40.0759072994248,-10.7548498428737,-11.7652791681621));
#64643=CARTESIAN_POINT('Ctrl Pts',(40.0894335555238,-10.756065173785,-11.7599434739442));
#64644=CARTESIAN_POINT('Ctrl Pts',(40.1343532266901,-10.7600943241237,-11.7417516196986));
#64645=CARTESIAN_POINT('Ctrl Pts',(40.1655248383629,-10.7628790641116,-11.7283533149218));
#64646=CARTESIAN_POINT('Ctrl Pts',(40.2427461466651,-10.7697754406884,-11.6932079616155));
#64647=CARTESIAN_POINT('Ctrl Pts',(40.2884097048502,-10.7738515595481,-11.6706491791863));
#64648=CARTESIAN_POINT('Ctrl Pts',(40.4360521967061,-10.7871373044353,-11.5917829224825));
#64649=CARTESIAN_POINT('Ctrl Pts',(40.5346613037689,-10.7961893457013,-11.5295194305981));
#64650=CARTESIAN_POINT('Ctrl Pts',(40.7253424041157,-10.8148061066151,-11.3887885875116));
#64651=CARTESIAN_POINT('Ctrl Pts',(40.8167812176551,-10.8243531609113,-11.3100460841137));
#64652=CARTESIAN_POINT('Ctrl Pts',(40.92452973377,-10.8367867671987,-11.2021622242884));
#64653=CARTESIAN_POINT('Ctrl Pts',(40.9466769911781,-10.8394124476964,-11.1790844065265));
#64654=CARTESIAN_POINT('Ctrl Pts',(40.9822815989904,-10.8437565776157,-11.1404712057185));
#64655=CARTESIAN_POINT('Ctrl Pts',(40.9960121827993,-10.8454634022954,-11.1251922069943));
#64656=CARTESIAN_POINT('Ctrl Pts',(41.022502515718,-10.8488204646873,-11.0949440545143));
#64657=CARTESIAN_POINT('Ctrl Pts',(41.0352776930479,-10.8504698925187,-11.0799905126656));
#64658=CARTESIAN_POINT('Ctrl Pts',(41.0654188628578,-10.8544367223528,-11.0438209383249));
#64659=CARTESIAN_POINT('Ctrl Pts',(41.0826078785501,-10.8567609377225,-11.0224618588037));
#64660=CARTESIAN_POINT('Ctrl Pts',(41.1437855434125,-10.8652672820721,-10.9437239671596));
#64661=CARTESIAN_POINT('Ctrl Pts',(41.1855419730588,-10.8715324270427,-10.8846693403957));
#64662=CARTESIAN_POINT('Ctrl Pts',(41.2897916053692,-10.888491048448,-10.7221686343017));
#64663=CARTESIAN_POINT('Ctrl Pts',(41.3472545971897,-10.8993200646208,-10.6157490115158));
#64664=CARTESIAN_POINT('Ctrl Pts',(41.4443014108719,-10.9207168285928,-10.3983435042842));
#64665=CARTESIAN_POINT('Ctrl Pts',(41.4842273844128,-10.9312539053336,-10.2878425800484));
#64666=CARTESIAN_POINT('Ctrl Pts',(41.5228670610808,-10.9437110362452,-10.1501404901966));
#64667=CARTESIAN_POINT('Ctrl Pts',(41.5294072050516,-10.9459308670538,-10.1253117937378));
#64668=CARTESIAN_POINT('Ctrl Pts',(41.5386719509606,-10.9492491928116,-10.0877049862597));
#64669=CARTESIAN_POINT('Ctrl Pts',(41.5416918082754,-10.9503625111018,-10.0750026320766));
#64670=CARTESIAN_POINT('Ctrl Pts',(41.5467934001117,-10.9522999563364,-10.0527398900864));
#64671=CARTESIAN_POINT('Ctrl Pts',(41.5489203725474,-10.9531264921375,-10.0431908399045));
#64672=CARTESIAN_POINT('Ctrl Pts',(41.5539219056732,-10.9551169174535,-10.0200726883061));
#64673=CARTESIAN_POINT('Ctrl Pts',(41.5567374648022,-10.9562775286216,-10.0064912829887));
#64674=CARTESIAN_POINT('Ctrl Pts',(41.5652734111053,-10.9599306815867,-9.96344655767705));
#64675=CARTESIAN_POINT('Ctrl Pts',(41.5705602424409,-10.9624010495705,-9.9338986166187));
#64676=CARTESIAN_POINT('Ctrl Pts',(41.5820485305772,-10.9683438481892,-9.86194736065849));
#64677=CARTESIAN_POINT('Ctrl Pts',(41.5876728879078,-10.9717921789487,-9.81946125311835));
#64678=CARTESIAN_POINT('Ctrl Pts',(41.6076393388287,-10.9870075235218,-9.62980887855387));
#64679=CARTESIAN_POINT('Ctrl Pts',(41.6095306903536,-10.9984375474365,-9.48165181689282));
#64680=CARTESIAN_POINT('Ctrl Pts',(41.5895254900321,-11.0183151823196,-9.23017599949378));
#64681=CARTESIAN_POINT('Ctrl Pts',(41.5744801152151,-11.0266261326242,-9.12676281801236));
#64682=CARTESIAN_POINT('Ctrl Pts',(41.5462617575271,-11.0376953917936,-8.99406967398162));
#64683=CARTESIAN_POINT('Ctrl Pts',(41.5391599541552,-11.0402643627764,-8.96360729170602));
#64684=CARTESIAN_POINT('Ctrl Pts',(41.5264490211558,-11.0445395322422,-8.91352315235615));
#64685=CARTESIAN_POINT('Ctrl Pts',(41.5211803938592,-11.0462348399066,-8.89381816489547));
#64686=CARTESIAN_POINT('Ctrl Pts',(41.5103178428527,-11.0495877526568,-8.85516827798776));
#64687=CARTESIAN_POINT('Ctrl Pts',(41.5047398724836,-11.0512447256363,-8.83622054232609));
#64688=CARTESIAN_POINT('Ctrl Pts',(41.4907178594649,-11.0552616691938,-8.79066786067397));
#64689=CARTESIAN_POINT('Ctrl Pts',(41.482043032499,-11.0576289101027,-8.76413768701433));
#64690=CARTESIAN_POINT('Ctrl Pts',(41.4479111557556,-11.0665304887987,-8.6655918782574));
#64691=CARTESIAN_POINT('Ctrl Pts',(41.419493070404,-11.0731585308123,-8.5946588186566));
#64692=CARTESIAN_POINT('Ctrl Pts',(41.3302585507642,-11.0920503395271,-8.39939569306689));
#64693=CARTESIAN_POINT('Ctrl Pts',(41.2620240332296,-11.1045045809736,-8.27879140406469));
#64694=CARTESIAN_POINT('Ctrl Pts',(41.1252113916338,-11.1262220760604,-8.07926372538336));
#64695=CARTESIAN_POINT('Ctrl Pts',(41.0611372446436,-11.1354750028157,-7.9976605204486));
#64696=CARTESIAN_POINT('Ctrl Pts',(40.978401595812,-11.1462198305567,-7.90526061308855));
#64697=CARTESIAN_POINT('Ctrl Pts',(40.9646197924781,-11.1479734971254,-7.89025690395843));
#64698=CARTESIAN_POINT('Ctrl Pts',(40.9424460428653,-11.1507360063675,-7.86672445441237));
#64699=CARTESIAN_POINT('Ctrl Pts',(40.9341786524732,-11.1517533583101,-7.85808056045626));
#64700=CARTESIAN_POINT('Ctrl Pts',(40.9180411779184,-11.1537142768979,-7.84145818909626));
#64701=CARTESIAN_POINT('Ctrl Pts',(40.9101793057365,-11.1546583440911,-7.83347250408296));
#64702=CARTESIAN_POINT('Ctrl Pts',(40.8904116176671,-11.1570050538713,-7.81367220510285));
#64703=CARTESIAN_POINT('Ctrl Pts',(40.8784371573212,-11.1584025348881,-7.80192628807131));
#64704=CARTESIAN_POINT('Ctrl Pts',(40.8300705285717,-11.1639570157993,-7.75546549099086));
#64705=CARTESIAN_POINT('Ctrl Pts',(40.7927133037988,-11.168046577823,-7.7217674433887));
#64706=CARTESIAN_POINT('Ctrl Pts',(40.5889342179779,-11.1895000061557,-7.54922722663526));
#64707=CARTESIAN_POINT('Ctrl Pts',(40.405373956332,-11.206003068983,-7.43217787512118));
#64708=CARTESIAN_POINT('Ctrl Pts',(40.1525624862095,-11.2282730897704,-7.31540989973278));
#64709=CARTESIAN_POINT('Ctrl Pts',(40.0955493997673,-11.2332610788826,-7.29169443044493));
#64710=CARTESIAN_POINT('Ctrl Pts',(40.0151766737935,-11.2402889462241,-7.26183477666319));
#64711=CARTESIAN_POINT('Ctrl Pts',(39.9925384884744,-11.2422679293991,-7.25380813272534));
#64712=CARTESIAN_POINT('Ctrl Pts',(39.9511412189918,-11.2458883806525,-7.23982450275232));
#64713=CARTESIAN_POINT('Ctrl Pts',(39.9324217437083,-11.2475260948706,-7.23375611834104));
#64714=CARTESIAN_POINT('Ctrl Pts',(39.894349171778,-11.2508594217414,-7.22192817682606));
#64715=CARTESIAN_POINT('Ctrl Pts',(39.874993841179,-11.2525552946411,-7.21618128553747));
#64716=CARTESIAN_POINT('Ctrl Pts',(39.8264830836253,-11.2568102955336,-7.20243982466638));
#64717=CARTESIAN_POINT('Ctrl Pts',(39.7972458360909,-11.2593789056762,-7.19475021628325));
#64718=CARTESIAN_POINT('Ctrl Pts',(39.6705748379916,-11.2705311119887,-7.16397523146468));
#64719=CARTESIAN_POINT('Ctrl Pts',(39.571911203467,-11.2792833309542,-7.1464384690286));
#64720=CARTESIAN_POINT('Ctrl Pts',(39.3201977297819,-11.3017738485723,-7.11774238386917));
#64721=CARTESIAN_POINT('Ctrl Pts',(39.1666401786788,-11.3156599356947,-7.11497513495131));
#64722=CARTESIAN_POINT('Ctrl Pts',(38.9508263075888,-11.3349265170344,-7.13172532438285));
#64723=CARTESIAN_POINT('Ctrl Pts',(38.8879944091471,-11.3405009498216,-7.13910279687247));
#64724=CARTESIAN_POINT('Ctrl Pts',(38.8071905235519,-11.3475720191562,-7.15183798004175));
#64725=CARTESIAN_POINT('Ctrl Pts',(38.7888942573365,-11.3491665098539,-7.15493894777457));
#64726=CARTESIAN_POINT('Ctrl Pts',(38.7592486012549,-11.3517375014518,-7.16031713274855));
#64727=CARTESIAN_POINT('Ctrl Pts',(38.7478770216168,-11.352720670949,-7.16246498688973));
#64728=CARTESIAN_POINT('Ctrl Pts',(38.7252332551786,-11.3546718214504,-7.16691140775319));
#64729=CARTESIAN_POINT('Ctrl Pts',(38.7139611885625,-11.3556398252072,-7.16920893092704));
#64730=CARTESIAN_POINT('Ctrl Pts',(38.6848789464987,-11.3581298717878,-7.17535423369443));
#64731=CARTESIAN_POINT('Ctrl Pts',(38.6670947500283,-11.359645346537,-7.17932376844657));
#64732=CARTESIAN_POINT('Ctrl Pts',(38.5857779917595,-11.3665489807708,-7.19844674428742));
#64733=CARTESIAN_POINT('Ctrl Pts',(38.5228270631866,-11.3718212782781,-7.21598342055357));
#64734=CARTESIAN_POINT('Ctrl Pts',(38.3081413857634,-11.3898042757577,-7.28532805048672));
#64735=CARTESIAN_POINT('Ctrl Pts',(38.1609219435414,-11.4021644674764,-7.34971513679241));
#64736=CARTESIAN_POINT('Ctrl Pts',(37.941235538372,-11.4220918536305,-7.47322529008722));
#64737=CARTESIAN_POINT('Ctrl Pts',(37.8639219058059,-11.4294249864097,-7.52271146340682));
#64738=CARTESIAN_POINT('Ctrl Pts',(37.7652077726044,-11.4393786760974,-7.59416259753143));
#64739=CARTESIAN_POINT('Ctrl Pts',(37.7411220416127,-11.4418569256409,-7.61229595873185));
#64740=CARTESIAN_POINT('Ctrl Pts',(37.7030816107448,-11.4458561599467,-7.6420719097457));
#64741=CARTESIAN_POINT('Ctrl Pts',(37.6889063963383,-11.4473659777947,-7.65342875091646));
#64742=CARTESIAN_POINT('Ctrl Pts',(37.659685460767,-11.4505204633043,-7.67738823890888));
#64743=CARTESIAN_POINT('Ctrl Pts',(37.6446627183865,-11.4521660767446,-7.69001662371618));
#64744=CARTESIAN_POINT('Ctrl Pts',(37.6092371505462,-11.4561053771815,-7.72054355289071));
#64745=CARTESIAN_POINT('Ctrl Pts',(37.588979910956,-11.4584056218504,-7.73860596290142));
#64746=CARTESIAN_POINT('Ctrl Pts',(37.5175036837037,-11.4666989912739,-7.80454247878495));
#64747=CARTESIAN_POINT('Ctrl Pts',(37.4680827200657,-11.4727696434315,-7.85430302754183));
#64748=CARTESIAN_POINT('Ctrl Pts',(37.339063270394,-11.4895916436224,-7.99609291303347));
#64749=CARTESIAN_POINT('Ctrl Pts',(37.2641647155925,-11.5004891065534,-8.0921085710049));
#64750=CARTESIAN_POINT('Ctrl Pts',(37.1307908826643,-11.5221406781137,-8.29273923816963));
#64751=CARTESIAN_POINT('Ctrl Pts',(37.072207700021,-11.5328631560084,-8.39690475642306));
#64752=CARTESIAN_POINT('Ctrl Pts',(37.0106895824316,-11.5454994911493,-8.52828832563821));
#64753=CARTESIAN_POINT('Ctrl Pts',(37.0001581503638,-11.5477231729444,-8.55175272190109));
#64754=CARTESIAN_POINT('Ctrl Pts',(36.9848465490632,-11.5510460987544,-8.58738663269681));
#64755=CARTESIAN_POINT('Ctrl Pts',(36.979786344245,-11.5521602228075,-8.59943261452653));
#64756=CARTESIAN_POINT('Ctrl Pts',(36.9706968990618,-11.5541905416767,-8.62157388130927));
#64757=CARTESIAN_POINT('Ctrl Pts',(36.9666377179502,-11.5551083543723,-8.63165572388229));
#64758=CARTESIAN_POINT('Ctrl Pts',(36.9610940144708,-11.5563777321211,-8.64569867865025));
#64759=CARTESIAN_POINT('Ctrl Pts',(36.9595516596191,-11.556732665845,-8.64963604120397));
#64760=CARTESIAN_POINT('Ctrl Pts',(36.9580196848654,-11.5570870138823,-8.65357747851634));
#64761=CARTESIAN_POINT('Origin',(39.2,5.9,-9.525));
#64762=CARTESIAN_POINT('',(36.0897704597331,5.287170157044,-9.52330892006467));
#64763=CARTESIAN_POINT('',(40.6132835138381,5.69998730739364,-6.75441154943334));
#64764=CARTESIAN_POINT('Ctrl Pts',(36.0897704597335,5.28717015708686,-9.52330891940844));
#64765=CARTESIAN_POINT('Ctrl Pts',(36.0898186087208,5.29295414852404,-9.43475346949347));
#64766=CARTESIAN_POINT('Ctrl Pts',(36.093648521948,5.29873813996121,-9.34629745832044));
#64767=CARTESIAN_POINT('Ctrl Pts',(36.1012366733098,5.30452213139838,-9.25817328083612));
#64768=CARTESIAN_POINT('Ctrl Pts',(36.1095595677739,5.31086617331557,-9.16151624357196));
#64769=CARTESIAN_POINT('Ctrl Pts',(36.1224233930836,5.31721021523276,-9.0650837361024));
#64770=CARTESIAN_POINT('Ctrl Pts',(36.1398093077089,5.32355425714994,-8.96933501125699));
#64771=CARTESIAN_POINT('Ctrl Pts',(36.1571717859258,5.32988974722729,-8.87371535676938));
#64772=CARTESIAN_POINT('Ctrl Pts',(36.1790441594873,5.33622523730464,-8.77877807778213));
#64773=CARTESIAN_POINT('Ctrl Pts',(36.2053557432597,5.34256072738198,-8.68497831666542));
#64774=CARTESIAN_POINT('Ctrl Pts',(36.2316396524023,5.34888955376535,-8.59127721451519));
#64775=CARTESIAN_POINT('Ctrl Pts',(36.2623533713891,5.35521838014872,-8.4987116686923));
#64776=CARTESIAN_POINT('Ctrl Pts',(36.2973751696389,5.3615472065321,-8.40772664621805));
#64777=CARTESIAN_POINT('Ctrl Pts',(36.3323715300516,5.36787143601689,-8.31680771007555));
#64778=CARTESIAN_POINT('Ctrl Pts',(36.3716695917911,5.37419566550169,-8.22746742000405));
#64779=CARTESIAN_POINT('Ctrl Pts',(36.4150980812374,5.38051989498649,-8.14013467955456));
#64780=CARTESIAN_POINT('Ctrl Pts',(36.4585103955461,5.38684176898338,-8.05283446657974));
#64781=CARTESIAN_POINT('Ctrl Pts',(36.5060498866431,5.39316364298027,-7.96754070695239));
#64782=CARTESIAN_POINT('Ctrl Pts',(36.5574979048968,5.39948551697716,-7.88466060515663));
#64783=CARTESIAN_POINT('Ctrl Pts',(36.6089405603399,5.40580673199799,-7.80178914257183));
#64784=CARTESIAN_POINT('Ctrl Pts',(36.664290702917,5.41212794701881,-7.72133120751426));
#64785=CARTESIAN_POINT('Ctrl Pts',(36.7232851845049,5.41844916203964,-7.64366686214077));
#64786=CARTESIAN_POINT('Ctrl Pts',(36.7822893395842,5.4247714135679,-7.56598978192578));
#64787=CARTESIAN_POINT('Ctrl Pts',(36.84493875699,5.43109366509616,-7.49110754802284));
#64788=CARTESIAN_POINT('Ctrl Pts',(36.9109293061056,5.43741591662442,-7.41936802568588));
#64789=CARTESIAN_POINT('Ctrl Pts',(36.9769880025767,5.44374469703791,-7.34755441912344));
#64790=CARTESIAN_POINT('Ctrl Pts',(37.0463944240091,5.45007347745141,-7.2788903247904));
#64791=CARTESIAN_POINT('Ctrl Pts',(37.1188069345913,5.4564022578649,-7.21368736917858));
#64792=CARTESIAN_POINT('Ctrl Pts',(37.1912605533614,5.46273463109256,-7.14844739820395));
#64793=CARTESIAN_POINT('Ctrl Pts',(37.2667233231194,5.46906700432022,-7.08667275512045));
#64794=CARTESIAN_POINT('Ctrl Pts',(37.3448214302059,5.47539937754789,-7.02863401579883));
#64795=CARTESIAN_POINT('Ctrl Pts',(37.423041153471,5.4817416116936,-6.97050489721));
#64796=CARTESIAN_POINT('Ctrl Pts',(37.5039040477082,5.48808384583931,-6.91612354267705));
#64797=CARTESIAN_POINT('Ctrl Pts',(37.5870083665495,5.49442607998502,-6.86571651693195));
#64798=CARTESIAN_POINT('Ctrl Pts',(37.6337516315119,5.49799336427614,-6.83736433267458));
#64799=CARTESIAN_POINT('Ctrl Pts',(37.6812035684037,5.50156064856726,-6.81026865835675));
#64800=CARTESIAN_POINT('Ctrl Pts',(37.7292897654297,5.50512793285838,-6.78446318053741));
#64801=CARTESIAN_POINT('Ctrl Pts',(37.8143208444197,5.51143598072031,-6.7388312163036));
#64802=CARTESIAN_POINT('Ctrl Pts',(37.9016290082981,5.51774402858223,-6.6970792600513));
#64803=CARTESIAN_POINT('Ctrl Pts',(37.9908238206751,5.52405207644415,-6.6594418309423));
#64804=CARTESIAN_POINT('Ctrl Pts',(38.0799001524758,5.53035174510636,-6.62185439694147));
#64805=CARTESIAN_POINT('Ctrl Pts',(38.170857749694,5.53665141376857,-6.58837079902755));
#64806=CARTESIAN_POINT('Ctrl Pts',(38.2632811158576,5.54295108243077,-6.55917998101857));
#64807=CARTESIAN_POINT('Ctrl Pts',(38.3592770146033,5.54949425847089,-6.52886082119773));
#64808=CARTESIAN_POINT('Ctrl Pts',(38.4568538782844,5.55603743451101,-6.50317327731934));
#64809=CARTESIAN_POINT('Ctrl Pts',(38.5555224272059,5.56258061055113,-6.48227436151968));
#64810=CARTESIAN_POINT('Ctrl Pts',(38.6503563799917,5.56886949646706,-6.46218764882469));
#64811=CARTESIAN_POINT('Ctrl Pts',(38.7461982684,5.57515838238298,-6.44652438776735));
#64812=CARTESIAN_POINT('Ctrl Pts',(38.8425989931736,5.58144726829891,-6.43537297182663));
#64813=CARTESIAN_POINT('Ctrl Pts',(38.9389691045005,5.58773415708801,-6.42422509717958));
#64814=CARTESIAN_POINT('Ctrl Pts',(39.0358972618107,5.5940210458771,-6.41758627158632));
#64815=CARTESIAN_POINT('Ctrl Pts',(39.1329269213326,5.6003079346662,-6.41549331002198));
#64816=CARTESIAN_POINT('Ctrl Pts',(39.2299525855833,5.60659456458779,-6.41340043463695));
#64817=CARTESIAN_POINT('Ctrl Pts',(39.3270793027399,5.61288119450939,-6.41585305997413));
#64818=CARTESIAN_POINT('Ctrl Pts',(39.4238492929252,5.61916782443098,-6.42283589296813));
#64819=CARTESIAN_POINT('Ctrl Pts',(39.5206420447427,5.62545593305437,-6.42982036842044));
#64820=CARTESIAN_POINT('Ctrl Pts',(39.6170774631422,5.63174404167775,-6.44133713569765));
#64821=CARTESIAN_POINT('Ctrl Pts',(39.7127027584188,5.63803215030114,-6.45731902988435));
#64822=CARTESIAN_POINT('Ctrl Pts',(39.8084320099681,5.64432709485985,-6.47331829832484));
#64823=CARTESIAN_POINT('Ctrl Pts',(39.9033489454962,5.65062203941857,-6.49379230721495));
#64824=CARTESIAN_POINT('Ctrl Pts',(39.9970111559666,5.65691698397728,-6.51862279975302));
#64825=CARTESIAN_POINT('Ctrl Pts',(40.0907338317231,5.6632159923481,-6.54346932205198));
#64826=CARTESIAN_POINT('Ctrl Pts',(40.1831997504376,5.66951500071891,-6.57267779281377));
#64827=CARTESIAN_POINT('Ctrl Pts',(40.2739838418386,5.67581400908973,-6.60608078899577));
#64828=CARTESIAN_POINT('Ctrl Pts',(40.3649048763921,5.68212251919207,-6.63953417188681));
#64829=CARTESIAN_POINT('Ctrl Pts',(40.4541386166821,5.68843102929442,-6.6771945337928));
#64830=CARTESIAN_POINT('Ctrl Pts',(40.5412823371517,5.69473953939677,-6.71884741239094));
#64831=CARTESIAN_POINT('Ctrl Pts',(40.5654459943908,5.69648879539572,-6.73039713595159));
#64832=CARTESIAN_POINT('Ctrl Pts',(40.5894491185416,5.69823805139468,-6.74225356980704));
#64833=CARTESIAN_POINT('Ctrl Pts',(40.6132835138381,5.69998730739364,-6.75441154943334));
#64834=CARTESIAN_POINT('',(37.7868905613917,5.7,-6.75432276015119));
#64835=CARTESIAN_POINT('Origin',(39.2,5.7,-9.525));
#64836=CARTESIAN_POINT('',(36.0893719342297,5.47782984291316,-9.52215481026634));
#64837=CARTESIAN_POINT('Ctrl Pts',(37.7868905613917,5.7,-6.75432276015119));
#64838=CARTESIAN_POINT('Ctrl Pts',(36.8702811367888,5.63313139951334,-7.22181475481399));
#64839=CARTESIAN_POINT('Ctrl Pts',(36.1407178101623,5.55907468048439,-8.27832117013194));
#64840=CARTESIAN_POINT('Ctrl Pts',(36.0859047902816,5.48501796145545,-9.41200135228371));
#64841=CARTESIAN_POINT('Ctrl Pts',(36.0866947581083,5.47782984291316,-9.52215236154092));
#64842=CARTESIAN_POINT('',(36.090096854374,4.20782989897492,-9.52397950441223));
#64843=CARTESIAN_POINT('Ctrl Pts',(36.0897713010337,5.47782984291316,-9.52215517555409));
#64844=CARTESIAN_POINT('Ctrl Pts',(36.0896845820882,5.47163671312522,-9.61696445391203));
#64845=CARTESIAN_POINT('Ctrl Pts',(36.0939371013632,5.46544358333727,-9.71197140607672));
#64846=CARTESIAN_POINT('Ctrl Pts',(36.1025565077274,5.45925045354932,-9.8067347424057));
#64847=CARTESIAN_POINT('Ctrl Pts',(36.111164773093,5.45306532868048,-9.90137559254964));
#64848=CARTESIAN_POINT('Ctrl Pts',(36.1241286777308,5.44688020381164,-9.99577300073165));
#64849=CARTESIAN_POINT('Ctrl Pts',(36.1414238647493,5.44069507894279,-10.08948443537));
#64850=CARTESIAN_POINT('Ctrl Pts',(36.1587018744572,5.43451609704374,-10.1831027972695));
#64851=CARTESIAN_POINT('Ctrl Pts',(36.180302538393,5.42833711514468,-10.276036091567));
#64852=CARTESIAN_POINT('Ctrl Pts',(36.206149703286,5.42215813324563,-10.3678469930927));
#64853=CARTESIAN_POINT('Ctrl Pts',(36.2319831605192,5.41598242827781,-10.4596092040711));
#64854=CARTESIAN_POINT('Ctrl Pts',(36.2620585261269,5.40980672330998,-10.550249764139));
#64855=CARTESIAN_POINT('Ctrl Pts',(36.2962488119258,5.40363101834216,-10.6393427168774));
#64856=CARTESIAN_POINT('Ctrl Pts',(36.3304311027509,5.39745675748626,-10.728414836335));
#64857=CARTESIAN_POINT('Ctrl Pts',(36.368726239351,5.39128249663036,-10.8159396400812));
#64858=CARTESIAN_POINT('Ctrl Pts',(36.4109581736926,5.38510823577446,-10.901508751882));
#64859=CARTESIAN_POINT('Ctrl Pts',(36.4531927534159,5.37893358816677,-10.987083223678));
#64860=CARTESIAN_POINT('Ctrl Pts',(36.4993644161621,5.37275894055907,-11.070701350939));
#64861=CARTESIAN_POINT('Ctrl Pts',(36.5492506059328,5.36658429295137,-11.1519782735957));
#64862=CARTESIAN_POINT('Ctrl Pts',(36.5991859844777,5.36040355701846,-11.2333353369127));
#64863=CARTESIAN_POINT('Ctrl Pts',(36.6528429610527,5.35422282108556,-11.312346197209));
#64864=CARTESIAN_POINT('Ctrl Pts',(36.709955245206,5.34804208515265,-11.3886544132491));
#64865=CARTESIAN_POINT('Ctrl Pts',(36.7670975456727,5.34185810083089,-11.4650027343447));
#64866=CARTESIAN_POINT('Ctrl Pts',(36.8276984744866,5.33567411650914,-11.5386452336246));
#64867=CARTESIAN_POINT('Ctrl Pts',(36.8914525110087,5.32949013218739,-11.6092598551936));
#64868=CARTESIAN_POINT('Ctrl Pts',(36.9553103802596,5.32329607634698,-11.679989482953));
#64869=CARTESIAN_POINT('Ctrl Pts',(37.022331284959,5.31710202050658,-11.747681066423));
#64870=CARTESIAN_POINT('Ctrl Pts',(37.092174261948,5.31090796466618,-11.8120507888776));
#64871=CARTESIAN_POINT('Ctrl Pts',(37.1377268961641,5.30686810880413,-11.8540336846242));
#64872=CARTESIAN_POINT('Ctrl Pts',(37.1844793126437,5.30282825294209,-11.8946043393667));
#64873=CARTESIAN_POINT('Ctrl Pts',(37.2323302861203,5.29878839708004,-11.9336939510824));
#64874=CARTESIAN_POINT('Ctrl Pts',(37.3074239402655,5.2924485565949,-11.9950381948787));
#64875=CARTESIAN_POINT('Ctrl Pts',(37.3855179670266,5.28610871610976,-12.0529727414287));
#64876=CARTESIAN_POINT('Ctrl Pts',(37.4662702301628,5.27976887562462,-12.10719126675));
#64877=CARTESIAN_POINT('Ctrl Pts',(37.5469137842503,5.27343756986037,-12.1613368028563));
#64878=CARTESIAN_POINT('Ctrl Pts',(37.6302081027073,5.26710626409612,-12.2117760199869));
#64879=CARTESIAN_POINT('Ctrl Pts',(37.7157778598847,5.26077495833187,-12.2582426331542));
#64880=CARTESIAN_POINT('Ctrl Pts',(37.8012578484924,5.2544502945435,-12.3046604996434));
#64881=CARTESIAN_POINT('Ctrl Pts',(37.8890081486045,5.24812563075512,-12.3471138408602));
#64882=CARTESIAN_POINT('Ctrl Pts',(37.9786251560617,5.24180096696674,-12.3853800697626));
#64883=CARTESIAN_POINT('Ctrl Pts',(38.0681776933297,5.23548085312132,-12.4236187700619));
#64884=CARTESIAN_POINT('Ctrl Pts',(38.1595938679232,5.22916073927589,-12.4576761763042));
#64885=CARTESIAN_POINT('Ctrl Pts',(38.2524470688899,5.22284062543047,-12.4873764270674));
#64886=CARTESIAN_POINT('Ctrl Pts',(38.345266110195,5.21652283668475,-12.5170657514382));
#64887=CARTESIAN_POINT('Ctrl Pts',(38.4395207123484,5.21020504793904,-12.5424009729244));
#64888=CARTESIAN_POINT('Ctrl Pts',(38.5347668204555,5.20388725919333,-12.5632553332024));
#64889=CARTESIAN_POINT('Ctrl Pts',(38.6300035147641,5.19757009487617,-12.5841076323071));
#64890=CARTESIAN_POINT('Ctrl Pts',(38.7262310940903,5.19125293055902,-12.6004798577207));
#64891=CARTESIAN_POINT('Ctrl Pts',(38.8229939761624,5.18493576624186,-12.6122960840985));
#64892=CARTESIAN_POINT('Ctrl Pts',(38.9197733282269,5.17861752668133,-12.6241143217141));
#64893=CARTESIAN_POINT('Ctrl Pts',(39.0170877310747,5.17229928712079,-12.6313749672716));
#64894=CARTESIAN_POINT('Ctrl Pts',(39.1144761579347,5.16598104756026,-12.6340539276987));
#64895=CARTESIAN_POINT('Ctrl Pts',(39.2119664658373,5.15965619829409,-12.6367356906689));
#64896=CARTESIAN_POINT('Ctrl Pts',(39.3095305156666,5.15333134902793,-12.6348261872233));
#64897=CARTESIAN_POINT('Ctrl Pts',(39.4067071575398,5.14700649976176,-12.628353477115));
#64898=CARTESIAN_POINT('Ctrl Pts',(39.5039396160097,5.14067801761063,-12.621877049193));
#64899=CARTESIAN_POINT('Ctrl Pts',(39.6007837901789,5.1343495354595,-12.6108322441893));
#64900=CARTESIAN_POINT('Ctrl Pts',(39.6967855871465,5.12802105330837,-12.5952988019578));
#64901=CARTESIAN_POINT('Ctrl Pts',(39.7929384685036,5.12168261160552,-12.5797409137189));
#64902=CARTESIAN_POINT('Ctrl Pts',(39.8882458988043,5.11534416990267,-12.5596803719045));
#64903=CARTESIAN_POINT('Ctrl Pts',(39.9822659189178,5.10900572819981,-12.5352476119083));
#64904=CARTESIAN_POINT('Ctrl Pts',(40.0357801837033,5.10539801733989,-12.5213409866354));
#64905=CARTESIAN_POINT('Ctrl Pts',(40.0888776682847,5.10179030647997,-12.506018824456));
#64906=CARTESIAN_POINT('Ctrl Pts',(40.1414797165299,5.09818259562005,-12.4893121624186));
#64907=CARTESIAN_POINT('Ctrl Pts',(40.2339622594588,5.09183968150153,-12.4599392645826));
#64908=CARTESIAN_POINT('Ctrl Pts',(40.3252235287212,5.08549676738301,-12.4261851533917));
#64909=CARTESIAN_POINT('Ctrl Pts',(40.4148198060276,5.07915385326449,-12.3881701821203));
#64910=CARTESIAN_POINT('Ctrl Pts',(40.504298514821,5.07281926233756,-12.3502050942123));
#64911=CARTESIAN_POINT('Ctrl Pts',(40.5921161766902,5.06648467141063,-12.3079904287888));
#64912=CARTESIAN_POINT('Ctrl Pts',(40.6778446151691,5.06015008048369,-12.2616961735486));
#64913=CARTESIAN_POINT('Ctrl Pts',(40.7634859526157,5.05382192557051,-12.2154489537788));
#64914=CARTESIAN_POINT('Ctrl Pts',(40.8470419056743,5.04749377065732,-12.1651305912952));
#64915=CARTESIAN_POINT('Ctrl Pts',(40.9281055745149,5.04116561574414,-12.1109585797593));
#64916=CARTESIAN_POINT('Ctrl Pts',(41.0091147299018,5.03484171636965,-12.0568229976558));
#64917=CARTESIAN_POINT('Ctrl Pts',(41.0876345718574,5.02851781699517,-11.9988391599899));
#64918=CARTESIAN_POINT('Ctrl Pts',(41.1632848624888,5.02219391762068,-11.9372693053683));
#64919=CARTESIAN_POINT('Ctrl Pts',(41.238909503085,5.01587216243151,-11.8757203266605));
#64920=CARTESIAN_POINT('Ctrl Pts',(41.311666188255,5.00955040724233,-11.8105880219351));
#64921=CARTESIAN_POINT('Ctrl Pts',(41.3812063787698,5.00322865205315,-11.7421759934913));
#64922=CARTESIAN_POINT('Ctrl Pts',(41.4507416429264,4.99690734470903,-11.6737688114845));
#64923=CARTESIAN_POINT('Ctrl Pts',(41.5170605551517,4.99058603736491,-11.6020826734505));
#64924=CARTESIAN_POINT('Ctrl Pts',(41.5798509405664,4.9842647300208,-11.5274585273072));
#64925=CARTESIAN_POINT('Ctrl Pts',(41.6426537189718,4.97794217503499,-11.452819652534));
#64926=CARTESIAN_POINT('Ctrl Pts',(41.701926306672,4.97161962004918,-11.3752419510508));
#64927=CARTESIAN_POINT('Ctrl Pts',(41.7573970375836,4.96529706506337,-11.2950991624931));
#64928=CARTESIAN_POINT('Ctrl Pts',(41.8129278532602,4.95896766161487,-11.2148695649004));
#64929=CARTESIAN_POINT('Ctrl Pts',(41.8646483422961,4.95263825816637,-11.1320696919911));
#64930=CARTESIAN_POINT('Ctrl Pts',(41.9123305013042,4.94630885471787,-11.0471018049378));
#64931=CARTESIAN_POINT('Ctrl Pts',(41.9600410945071,4.93997567687043,-10.9620832491752));
#64932=CARTESIAN_POINT('Ctrl Pts',(42.0037083670312,4.93364249902299,-10.8748944939855));
#64933=CARTESIAN_POINT('Ctrl Pts',(42.0431514999804,4.92730932117555,-10.7859600315075));
#64934=CARTESIAN_POINT('Ctrl Pts',(42.0826577742244,4.9209660050602,-10.6968832011014));
#64935=CARTESIAN_POINT('Ctrl Pts',(42.117926248496,4.91462268894484,-10.6060554889158));
#64936=CARTESIAN_POINT('Ctrl Pts',(42.1488252210036,4.90827937282948,-10.5139188383651));
#64937=CARTESIAN_POINT('Ctrl Pts',(42.16620302351,4.90471184660635,-10.4621005289865));
#64938=CARTESIAN_POINT('Ctrl Pts',(42.1821996577844,4.90114432038321,-10.4098684426213));
#64939=CARTESIAN_POINT('Ctrl Pts',(42.196798807768,4.89757679416008,-10.3573025643722));
#64940=CARTESIAN_POINT('Ctrl Pts',(42.2226830905886,4.89125157263462,-10.2641032986035));
#64941=CARTESIAN_POINT('Ctrl Pts',(42.2442615259797,4.88492635110916,-10.169529793704));
#64942=CARTESIAN_POINT('Ctrl Pts',(42.261390504317,4.8786011295837,-10.0740162410875));
#64943=CARTESIAN_POINT('Ctrl Pts',(42.2784961340242,4.8722845300119,-9.97863288366201));
#64944=CARTESIAN_POINT('Ctrl Pts',(42.291164283726,4.8659679304401,-9.88231245299431));
#64945=CARTESIAN_POINT('Ctrl Pts',(42.2993012966942,4.8596513308683,-9.78550359922624));
#64946=CARTESIAN_POINT('Ctrl Pts',(42.3074296686005,4.85334143917913,-9.68879755115629));
#64947=CARTESIAN_POINT('Ctrl Pts',(42.3110364326971,4.84703154748996,-9.59160454565647));
#64948=CARTESIAN_POINT('Ctrl Pts',(42.310079287173,4.84072165580079,-9.49438169832463));
#64949=CARTESIAN_POINT('Ctrl Pts',(42.3091228371721,4.83441634928264,-9.39722949933418));
#64950=CARTESIAN_POINT('Ctrl Pts',(42.3036090748728,4.82811104276449,-9.30004793881186));
#64951=CARTESIAN_POINT('Ctrl Pts',(42.2935477251791,4.82180573624634,-9.20329652637949));
#64952=CARTESIAN_POINT('Ctrl Pts',(42.2834901108703,4.81550277064146,-9.10658103395573));
#64953=CARTESIAN_POINT('Ctrl Pts',(42.2688883089752,4.80919980503657,-9.0102958080121));
#64954=CARTESIAN_POINT('Ctrl Pts',(42.2498040233362,4.80289683943168,-8.91489667092989));
#64955=CARTESIAN_POINT('Ctrl Pts',(42.2307216194919,4.79659449532698,-8.81950694062298));
#64956=CARTESIAN_POINT('Ctrl Pts',(42.2071576968169,4.79029215122228,-8.72500355541852));
#64957=CARTESIAN_POINT('Ctrl Pts',(42.1792251473581,4.78398980711758,-8.63183250493014));
#64958=CARTESIAN_POINT('Ctrl Pts',(42.1512877362539,4.77768636609325,-8.53864523807026));
#64959=CARTESIAN_POINT('Ctrl Pts',(42.1189803143276,4.77138292506893,-8.44679118646755));
#64960=CARTESIAN_POINT('Ctrl Pts',(42.0824654273109,4.76507948404461,-8.3567005036133));
#64961=CARTESIAN_POINT('Ctrl Pts',(42.0459115304473,4.7587693088828,-8.26651357443237));
#64962=CARTESIAN_POINT('Ctrl Pts',(42.0051413596025,4.752459133721,-8.17809418206875));
#64963=CARTESIAN_POINT('Ctrl Pts',(41.9603652649566,4.7461489585592,-8.09185162773666));
#64964=CARTESIAN_POINT('Ctrl Pts',(41.9155630444213,4.73983510154573,-8.00555875272652));
#64965=CARTESIAN_POINT('Ctrl Pts',(41.8667504660697,4.73352124453225,-7.92144562385831));
#64966=CARTESIAN_POINT('Ctrl Pts',(41.8141823393613,4.72720738751878,-7.83989426163472));
#64967=CARTESIAN_POINT('Ctrl Pts',(41.7615294415422,4.72088334880958,-7.75821139007305));
#64968=CARTESIAN_POINT('Ctrl Pts',(41.7051091568404,4.71455931010037,-7.67909889090502));
#64969=CARTESIAN_POINT('Ctrl Pts',(41.6452178075563,4.70823527139117,-7.60290725340594));
#64970=CARTESIAN_POINT('Ctrl Pts',(41.6096586298144,4.70448051182747,-7.55767013631543));
#64971=CARTESIAN_POINT('Ctrl Pts',(41.5728766039077,4.70072575226378,-7.513461999658));
#64972=CARTESIAN_POINT('Ctrl Pts',(41.5349397866914,4.69697099270009,-7.47034994575101));
#64973=CARTESIAN_POINT('Ctrl Pts',(41.470942430499,4.69063691665347,-7.39762224552403));
#64974=CARTESIAN_POINT('Ctrl Pts',(41.4034330822141,4.68430284060685,-7.32776149494582));
#64975=CARTESIAN_POINT('Ctrl Pts',(41.3326984783807,4.67796876456024,-7.26112547759101));
#64976=CARTESIAN_POINT('Ctrl Pts',(41.2620589909275,4.67164320590614,-7.1945790652727));
#64977=CARTESIAN_POINT('Ctrl Pts',(41.188203183454,4.66531764725203,-7.13124906469978));
#64978=CARTESIAN_POINT('Ctrl Pts',(41.1114571080781,4.65899208859793,-7.07145921638181));
#64979=CARTESIAN_POINT('Ctrl Pts',(41.034791305441,4.65267314617684,-7.01173190539693));
#64980=CARTESIAN_POINT('Ctrl Pts',(40.9552415880006,4.64635420375576,-6.95553765238175));
#64981=CARTESIAN_POINT('Ctrl Pts',(40.8731690713976,4.64003526133468,-6.9031617304993));
#64982=CARTESIAN_POINT('Ctrl Pts',(40.7911548182755,4.63372080474631,-6.85082299041221));
#64983=CARTESIAN_POINT('Ctrl Pts',(40.7066216939506,4.62740634815794,-6.80229742691731));
#64984=CARTESIAN_POINT('Ctrl Pts',(40.6199611695792,4.62109189156957,-6.75782799056738));
#64985=CARTESIAN_POINT('Ctrl Pts',(40.5333319751213,4.61477971781275,-6.71337463101373));
#64986=CARTESIAN_POINT('Ctrl Pts',(40.4445772973412,4.60846754405593,-6.67297468417212));
#64987=CARTESIAN_POINT('Ctrl Pts',(40.3541138485031,4.60215537029911,-6.636825511228));
#64988=CARTESIAN_POINT('Ctrl Pts',(40.2636586344952,4.59584377113545,-6.60067962892009));
#64989=CARTESIAN_POINT('Ctrl Pts',(40.1714953646493,4.58953217197179,-6.56878391315326));
#64990=CARTESIAN_POINT('Ctrl Pts',(40.0780604265547,4.58322057280813,-6.54128745683861));
#64991=CARTESIAN_POINT('Ctrl Pts',(39.9846087204924,4.57690784095586,-6.51378606597057));
#64992=CARTESIAN_POINT('Ctrl Pts',(39.8898853122176,4.57059510910359,-6.49068562596634));
#64993=CARTESIAN_POINT('Ctrl Pts',(39.794340414305,4.56428237725131,-6.47208497910214));
#64994=CARTESIAN_POINT('Ctrl Pts',(39.6986936174699,4.55796291285144,-6.45346449459184));
#64995=CARTESIAN_POINT('Ctrl Pts',(39.6022240115942,4.55164344845157,-6.43935346793963));
#64996=CARTESIAN_POINT('Ctrl Pts',(39.5053904357368,4.5453239840517,-6.4297993062387));
#64997=CARTESIAN_POINT('Ctrl Pts',(39.4085002460812,4.53900082497383,-6.42023955869238));
#64998=CARTESIAN_POINT('Ctrl Pts',(39.3112460990197,4.53267766589596,-6.41524200372406));
#64999=CARTESIAN_POINT('Ctrl Pts',(39.2140882719303,4.52635450681809,-6.4148019076763));
#65000=CARTESIAN_POINT('Ctrl Pts',(39.1167750937143,4.52002123728473,-6.41436110793415));
#65001=CARTESIAN_POINT('Ctrl Pts',(39.019558979423,4.51368796775138,-6.41849229985226));
#65002=CARTESIAN_POINT('Ctrl Pts',(38.9228964794896,4.50735469821802,-6.42713875523439));
#65003=CARTESIAN_POINT('Ctrl Pts',(38.8669867995618,4.50369152922538,-6.4321398730749));
#65004=CARTESIAN_POINT('Ctrl Pts',(38.811262184866,4.50002836023275,-6.43865059954992));
#65005=CARTESIAN_POINT('Ctrl Pts',(38.7558092127628,4.49636519124011,-6.44665219680531));
#65006=CARTESIAN_POINT('Ctrl Pts',(38.6599291495522,4.4900314482279,-6.46048722893314));
#65007=CARTESIAN_POINT('Ctrl Pts',(38.5645302463999,4.48369770521569,-6.47882995958531));
#65008=CARTESIAN_POINT('Ctrl Pts',(38.4700688058746,4.47736396220348,-6.50163579687419));
#65009=CARTESIAN_POINT('Ctrl Pts',(38.3757341241126,4.47103871850515,-6.5244110307791));
#65010=CARTESIAN_POINT('Ctrl Pts',(38.2823348259906,4.46471347480681,-6.55163736586205));
#65011=CARTESIAN_POINT('Ctrl Pts',(38.1903201893549,4.45838823110848,-6.58321868031024));
#65012=CARTESIAN_POINT('Ctrl Pts',(38.0984015320586,4.4520695851943,-6.6147670526765));
#65013=CARTESIAN_POINT('Ctrl Pts',(38.0078650761294,4.44575093928013,-6.65066123217911));
#65014=CARTESIAN_POINT('Ctrl Pts',(37.9191470452254,4.43943229336595,-6.69075471048375));
#65015=CARTESIAN_POINT('Ctrl Pts',(37.8304915911859,4.43311810428028,-6.73081990903357));
#65016=CARTESIAN_POINT('Ctrl Pts',(37.7436524094708,4.42680391519462,-6.7750783383247));
#65017=CARTESIAN_POINT('Ctrl Pts',(37.6590468694962,4.42048972610895,-6.82333493887741));
#65018=CARTESIAN_POINT('Ctrl Pts',(37.5744716754993,4.41417780177145,-6.87157423094508));
#65019=CARTESIAN_POINT('Ctrl Pts',(37.4921289106524,4.40786587743394,-6.92380862841624));
#65020=CARTESIAN_POINT('Ctrl Pts',(37.4124115565431,4.40155395309643,-6.97979701993741));
#65021=CARTESIAN_POINT('Ctrl Pts',(37.3327012260753,4.39524258488242,-7.03578047850027));
#65022=CARTESIAN_POINT('Ctrl Pts',(37.2556162040234,4.3889312166684,-7.09551702208044));
#65023=CARTESIAN_POINT('Ctrl Pts',(37.1815197986723,4.38261984845438,-7.15872268536673));
#65024=CARTESIAN_POINT('Ctrl Pts',(37.1074098738343,4.37630732868032,-7.22193988103615));
#65025=CARTESIAN_POINT('Ctrl Pts',(37.0362899812941,4.36999480890626,-7.28862716988691));
#65026=CARTESIAN_POINT('Ctrl Pts',(36.9684888985377,4.3636822891322,-7.35846154962566));
#65027=CARTESIAN_POINT('Ctrl Pts',(36.9006151772389,4.35736300645382,-7.42837074627515));
#65028=CARTESIAN_POINT('Ctrl Pts',(36.8360676692771,4.35104372377543,-7.50143345093607));
#65029=CARTESIAN_POINT('Ctrl Pts',(36.7751367898097,4.34472444109705,-7.57729132959634));
#65030=CARTESIAN_POINT('Ctrl Pts',(36.7141701232154,4.33840144685282,-7.65319376260332));
#65031=CARTESIAN_POINT('Ctrl Pts',(36.6568245722978,4.3320784526086,-7.73189428560719));
#65032=CARTESIAN_POINT('Ctrl Pts',(36.6033476688481,4.32575545836437,-7.81300487032726));
#65033=CARTESIAN_POINT('Ctrl Pts',(36.5497850149696,4.31942232517357,-7.89424551619452));
#65034=CARTESIAN_POINT('Ctrl Pts',(36.5001036187132,4.31308919198277,-7.97790356498957));
#65035=CARTESIAN_POINT('Ctrl Pts',(36.4545054296171,4.30675605879197,-8.06356569874036));
#65036=CARTESIAN_POINT('Ctrl Pts',(36.4281136380704,4.30309050245469,-8.11314611459069));
#65037=CARTESIAN_POINT('Ctrl Pts',(36.4030888281374,4.29942494611741,-8.16339749101763));
#65038=CARTESIAN_POINT('Ctrl Pts',(36.3794626743309,4.29575938978012,-8.21423692171043));
#65039=CARTESIAN_POINT('Ctrl Pts',(36.3352160404628,4.288894602117,-8.30944808872224));
#65040=CARTESIAN_POINT('Ctrl Pts',(36.2957430807869,4.28202981445388,-8.40701169084998));
#65041=CARTESIAN_POINT('Ctrl Pts',(36.2612786271195,4.27516502679075,-8.50644840804449));
#65042=CARTESIAN_POINT('Ctrl Pts',(36.2269374637337,4.26832479665038,-8.60552940856349));
#65043=CARTESIAN_POINT('Ctrl Pts',(36.1975691938129,4.26148456651002,-8.70646986597188));
#65044=CARTESIAN_POINT('Ctrl Pts',(36.1733603994216,4.25464433636965,-8.80877141839319));
#65045=CARTESIAN_POINT('Ctrl Pts',(36.1492076389944,4.24781993870753,-8.91083618242152));
#65046=CARTESIAN_POINT('Ctrl Pts',(36.1301906402494,4.2409955410454,-9.01425545804629));
#65047=CARTESIAN_POINT('Ctrl Pts',(36.1164468242244,4.23417114338327,-9.11851449587413));
#65048=CARTESIAN_POINT('Ctrl Pts',(36.1027487584133,4.22736946267633,-9.22242647774091));
#65049=CARTESIAN_POINT('Ctrl Pts',(36.0942889360373,4.22056778196938,-9.3271723358877));
#65050=CARTESIAN_POINT('Ctrl Pts',(36.0911539354075,4.21376610126243,-9.43222716147583));
#65051=CARTESIAN_POINT('Ctrl Pts',(36.0902419066779,4.21178736857714,-9.46278952188274));
#65052=CARTESIAN_POINT('Ctrl Pts',(36.0897802097724,4.20980863589185,-9.493377948687));
#65053=CARTESIAN_POINT('Ctrl Pts',(36.0897701674737,4.20782990320657,-9.52397933185991));
#65054=CARTESIAN_POINT('',(36.0897712272353,2.93782984291316,-9.52776296339717));
#65055=CARTESIAN_POINT('Ctrl Pts',(36.0944248666917,4.20782984291316,-9.5239817904194));
#65056=CARTESIAN_POINT('Ctrl Pts',(36.0961127382952,4.17027109138215,-10.1039645708521));
#65057=CARTESIAN_POINT('Ctrl Pts',(36.529553577299,4.0658437393645,-11.7188971193403));
#65058=CARTESIAN_POINT('Ctrl Pts',(39.123431789966,3.89454778686015,-13.194039457166));
#65059=CARTESIAN_POINT('Ctrl Pts',(42.230539573114,3.69394198540018,-11.5947102098393));
#65060=CARTESIAN_POINT('Ctrl Pts',(42.5896834516285,3.49333618394021,-8.11861111471374));
#65061=CARTESIAN_POINT('Ctrl Pts',(39.8751829600439,3.29273038248021,-5.91779011158274));
#65062=CARTESIAN_POINT('Ctrl Pts',(36.8044545844578,3.10756161888526,-6.9054988491143));
#65063=CARTESIAN_POINT('Ctrl Pts',(36.0968354029096,2.98926145577694,-8.73662212930356));
#65064=CARTESIAN_POINT('Ctrl Pts',(36.0896823919881,2.9378298931553,-9.52776226947597));
#65065=CARTESIAN_POINT('',(36.0897704721981,1.66782984286977,-9.52328614782123));
#65066=CARTESIAN_POINT('Ctrl Pts',(36.0897712272353,2.93782984291316,-9.52776296339717));
#65067=CARTESIAN_POINT('Ctrl Pts',(36.0898865823914,2.92938781562177,-9.657616629196));
#65068=CARTESIAN_POINT('Ctrl Pts',(36.0981377832265,2.92094578833037,-9.78711742420437));
#65069=CARTESIAN_POINT('Ctrl Pts',(36.114371081634,2.91250376103898,-9.91541622794557));
#65070=CARTESIAN_POINT('Ctrl Pts',(36.1278218581146,2.90550876721274,-10.0217235530829));
#65071=CARTESIAN_POINT('Ctrl Pts',(36.1467519556812,2.8985137733865,-10.1272063727662));
#65072=CARTESIAN_POINT('Ctrl Pts',(36.1710500170942,2.89151877956026,-10.2313941208384));
#65073=CARTESIAN_POINT('Ctrl Pts',(36.19304725805,2.88518615235742,-10.3257161722989));
#65074=CARTESIAN_POINT('Ctrl Pts',(36.2194927104237,2.87885352515457,-10.4191735792048));
#65075=CARTESIAN_POINT('Ctrl Pts',(36.2503030538065,2.87252089795173,-10.5113156586593));
#65076=CARTESIAN_POINT('Ctrl Pts',(36.2810719318078,2.86619679336739,-10.603333730847));
#65077=CARTESIAN_POINT('Ctrl Pts',(36.3161938876909,2.85987268878306,-10.6940395827062));
#65078=CARTESIAN_POINT('Ctrl Pts',(36.3555348578463,2.85354858419872,-10.7829939220729));
#65079=CARTESIAN_POINT('Ctrl Pts',(36.394834650207,2.84723109899053,-10.8718551538345));
#65080=CARTESIAN_POINT('Ctrl Pts',(36.4383445016696,2.84091361378234,-10.9589681199301));
#65081=CARTESIAN_POINT('Ctrl Pts',(36.4858812591661,2.83459612857415,-11.0439108313374));
#65082=CARTESIAN_POINT('Ctrl Pts',(36.5333842740557,2.82828312765204,-11.128793248592));
#65083=CARTESIAN_POINT('Ctrl Pts',(36.584908299381,2.82197012672992,-11.2115080932165));
#65084=CARTESIAN_POINT('Ctrl Pts',(36.6402234176746,2.8156571258078,-11.2916563054195));
#65085=CARTESIAN_POINT('Ctrl Pts',(36.6955185471165,2.8093464061723,-11.3717755550029));
#65086=CARTESIAN_POINT('Ctrl Pts',(36.7546017992502,2.80303568653681,-11.4493296555402));
#65087=CARTESIAN_POINT('Ctrl Pts',(36.8171994548306,2.79672496690131,-11.5239477769167));
#65088=CARTESIAN_POINT('Ctrl Pts',(36.8797914444659,2.79041481847235,-11.5985591443314));
#65089=CARTESIAN_POINT('Ctrl Pts',(36.9458969238692,2.78410467004339,-11.6702347260536));
#65090=CARTESIAN_POINT('Ctrl Pts',(37.0152020108701,2.77779452161443,-11.7386369168394));
#65091=CARTESIAN_POINT('Ctrl Pts',(37.0845195957786,2.77148323526536,-11.8070514427118));
#65092=CARTESIAN_POINT('Ctrl Pts',(37.1570376229935,2.7651719489163,-11.8721910980819));
#65093=CARTESIAN_POINT('Ctrl Pts',(37.2324062670082,2.75886066256724,-11.9337560181121));
#65094=CARTESIAN_POINT('Ctrl Pts',(37.3078555124955,2.75254262674058,-11.9953867775014));
#65095=CARTESIAN_POINT('Ctrl Pts',(37.3861611217752,2.74622459091391,-12.0534348921755));
#65096=CARTESIAN_POINT('Ctrl Pts',(37.4669413473052,2.73990655508725,-12.1076417403929));
#65097=CARTESIAN_POINT('Ctrl Pts',(37.5477689074287,2.73358481709641,-12.1618803520661));
#65098=CARTESIAN_POINT('Ctrl Pts',(37.631073597226,2.72726307910557,-12.2122729889631));
#65099=CARTESIAN_POINT('Ctrl Pts',(37.7164477520338,2.72094134111473,-12.2586062958031));
#65100=CARTESIAN_POINT('Ctrl Pts',(37.8019587970218,2.71460946675586,-12.3050138941514));
#65101=CARTESIAN_POINT('Ctrl Pts',(37.889545539423,2.708277592397,-12.3473489753417));
#65102=CARTESIAN_POINT('Ctrl Pts',(37.9787790179551,2.70194571803814,-12.3854457634979));
#65103=CARTESIAN_POINT('Ctrl Pts',(38.0306062077465,2.69826813805885,-12.4075725426249));
#65104=CARTESIAN_POINT('Ctrl Pts',(38.0829885683538,2.69459055807955,-12.4282705229668));
#65105=CARTESIAN_POINT('Ctrl Pts',(38.1358399153893,2.69091297810026,-12.447515007185));
#65106=CARTESIAN_POINT('Ctrl Pts',(38.2268474624822,2.6845803574212,-12.4806531087094));
#65107=CARTESIAN_POINT('Ctrl Pts',(38.3195624478393,2.67824773674214,-12.5095937395124));
#65108=CARTESIAN_POINT('Ctrl Pts',(38.4135619344936,2.67191511606308,-12.5341603184315));
#65109=CARTESIAN_POINT('Ctrl Pts',(38.5074349132907,2.66559101805048,-12.5586938347737));
#65110=CARTESIAN_POINT('Ctrl Pts',(38.6025885379292,2.65926692003788,-12.5788648897886));
#65111=CARTESIAN_POINT('Ctrl Pts',(38.6985816725519,2.65294282202529,-12.5945456200876));
#65112=CARTESIAN_POINT('Ctrl Pts',(38.7944743314453,2.64662534342732,-12.6102099374127));
#65113=CARTESIAN_POINT('Ctrl Pts',(38.8912043240746,2.64030786482936,-12.6213932037357));
#65114=CARTESIAN_POINT('Ctrl Pts',(38.9883181706112,2.63399038623139,-12.6280181204767));
#65115=CARTESIAN_POINT('Ctrl Pts',(39.085363083138,2.62767739194897,-12.6346383346743));
#65116=CARTESIAN_POINT('Ctrl Pts',(39.1827908728243,2.62136439766654,-12.6367066022538));
#65117=CARTESIAN_POINT('Ctrl Pts',(39.2801416979861,2.61505140338411,-12.6341973178208));
#65118=CARTESIAN_POINT('Ctrl Pts',(39.3774573438581,2.60874069040392,-12.6316889401581));
#65119=CARTESIAN_POINT('Ctrl Pts',(39.4746956437448,2.60242997742373,-12.6246063085977));
#65120=CARTESIAN_POINT('Ctrl Pts',(39.5713964520392,2.59611926444353,-12.6129759274179));
#65121=CARTESIAN_POINT('Ctrl Pts',(39.6680885074651,2.58980912267719,-12.6013465989615));
#65122=CARTESIAN_POINT('Ctrl Pts',(39.7642427338712,2.58349898091085,-12.5851703917463));
#65123=CARTESIAN_POINT('Ctrl Pts',(39.8594048536913,2.57718883914451,-12.5645256030881));
#65124=CARTESIAN_POINT('Ctrl Pts',(39.9545841342963,2.57087755945706,-12.5438770915119));
#65125=CARTESIAN_POINT('Ctrl Pts',(40.0487705256217,2.5645662797696,-12.5187584907639));
#65126=CARTESIAN_POINT('Ctrl Pts',(40.1415217058894,2.55825500008215,-12.4892988260698));
#65127=CARTESIAN_POINT('Ctrl Pts',(40.2343720777595,2.55193697087471,-12.4598076561018));
#65128=CARTESIAN_POINT('Ctrl Pts',(40.3257837568097,2.54561894166727,-12.425966286297));
#65129=CARTESIAN_POINT('Ctrl Pts',(40.4153315082647,2.53930091245983,-12.3879530170645));
#65130=CARTESIAN_POINT('Ctrl Pts',(40.5049317320566,2.53297918107393,-12.3499174731793));
#65131=CARTESIAN_POINT('Ctrl Pts',(40.5926654594737,2.52665744968802,-12.3077053515008));
#65132=CARTESIAN_POINT('Ctrl Pts',(40.6781311942546,2.52033571830212,-12.2615413984574));
#65133=CARTESIAN_POINT('Ctrl Pts',(40.763733967387,2.51400385046037,-12.2153034247316));
#65134=CARTESIAN_POINT('Ctrl Pts',(40.8470611119474,2.50767198261862,-12.1651011923231));
#65135=CARTESIAN_POINT('Ctrl Pts',(40.9277393326589,2.50134011477686,-12.1112032888548));
#65136=CARTESIAN_POINT('Ctrl Pts',(40.9745984817717,2.49766246873134,-12.0798985591122));
#65137=CARTESIAN_POINT('Ctrl Pts',(41.0205646165812,2.49398482268582,-12.0473478859908));
#65138=CARTESIAN_POINT('Ctrl Pts',(41.0655699423,2.49030717664029,-12.013609941973));
#65139=CARTESIAN_POINT('Ctrl Pts',(41.1430655829285,2.48397455862786,-11.9555158488098));
#65140=CARTESIAN_POINT('Ctrl Pts',(41.2179796614594,2.47764194061542,-11.893697564131));
#65141=CARTESIAN_POINT('Ctrl Pts',(41.2899331267851,2.47130932260298,-11.8284127242999));
#65142=CARTESIAN_POINT('Ctrl Pts',(41.3617897538102,2.46498522732066,-11.7632157478247));
#65143=CARTESIAN_POINT('Ctrl Pts',(41.4306933659334,2.45866113203834,-11.6945617803698));
#65144=CARTESIAN_POINT('Ctrl Pts',(41.4962957594979,2.45233703675603,-11.6227503278064));
#65145=CARTESIAN_POINT('Ctrl Pts',(41.5618294865846,2.44601956094786,-11.5510140407858));
#65146=CARTESIAN_POINT('Ctrl Pts',(41.6240685712259,2.4397020851397,-11.4761271602531));
#65147=CARTESIAN_POINT('Ctrl Pts',(41.6827004043077,2.43338460933153,-11.3984271684137));
#65148=CARTESIAN_POINT('Ctrl Pts',(41.7412906182062,2.42707161791641,-11.3207823310873));
#65149=CARTESIAN_POINT('Ctrl Pts',(41.7962784084439,2.42075862650128,-11.2403287004153));
#65150=CARTESIAN_POINT('Ctrl Pts',(41.8473909752809,2.41444563508615,-11.157437342412));
#65151=CARTESIAN_POINT('Ctrl Pts',(41.8984850713801,2.40813492502014,-11.0745759391662));
#65152=CARTESIAN_POINT('Ctrl Pts',(41.9457064974003,2.40182421495412,-10.989278930866));
#65153=CARTESIAN_POINT('Ctrl Pts',(41.9888259231194,2.39551350488811,-10.9019461221984));
#65154=CARTESIAN_POINT('Ctrl Pts',(42.0319414455877,2.38920336607934,-10.8146212190596));
#65155=CARTESIAN_POINT('Ctrl Pts',(42.0709555126086,2.38289322727057,-10.7252612741663));
#65156=CARTESIAN_POINT('Ctrl Pts',(42.1056853720536,2.3765830884618,-10.6342894895083));
#65157=CARTESIAN_POINT('Ctrl Pts',(42.1404214941901,2.37027181177188,-10.5433013002859));
#65158=CARTESIAN_POINT('Ctrl Pts',(42.1708717184259,2.36396053508196,-10.4507011025792));
#65159=CARTESIAN_POINT('Ctrl Pts',(42.1969023064928,2.35764925839203,-10.3569298156925));
#65160=CARTESIAN_POINT('Ctrl Pts',(42.2229607324854,2.35133123222525,-10.2630582468561));
#65161=CARTESIAN_POINT('Ctrl Pts',(42.2445899689501,2.34501320605846,-10.1680135105659));
#65162=CARTESIAN_POINT('Ctrl Pts',(42.2617068798173,2.33869517989168,-10.0722491525615));
#65163=CARTESIAN_POINT('Ctrl Pts',(42.2788338206155,2.33237345157523,-9.97642867988201));
#65164=CARTESIAN_POINT('Ctrl Pts',(42.2914431141386,2.32605172325879,-9.87988817925913));
#65165=CARTESIAN_POINT('Ctrl Pts',(42.2995034932724,2.31972999494234,-9.78308670653901));
#65166=CARTESIAN_POINT('Ctrl Pts',(42.307576796649,2.31339813018564,-9.68613001956475));
#65167=CARTESIAN_POINT('Ctrl Pts',(42.3110866053107,2.30706626542893,-9.58891196167446));
#65168=CARTESIAN_POINT('Ctrl Pts',(42.3100537791399,2.30073440067222,-9.49189193818005));
#65169=CARTESIAN_POINT('Ctrl Pts',(42.3094538928027,2.29705672550825,-9.43554074551828));
#65170=CARTESIAN_POINT('Ctrl Pts',(42.3073225134909,2.29337905034427,-9.37925629083746));
#65171=CARTESIAN_POINT('Ctrl Pts',(42.3036717148399,2.2897013751803,-9.32312741790204));
#65172=CARTESIAN_POINT('Ctrl Pts',(42.2973853725387,2.28336875397506,-9.22647861801376));
#65173=CARTESIAN_POINT('Ctrl Pts',(42.2865693255086,2.27703613276983,-9.1299558590541));
#65174=CARTESIAN_POINT('Ctrl Pts',(42.2712321176497,2.27070351156459,-9.0340173807386));
#65175=CARTESIAN_POINT('Ctrl Pts',(42.2559155511875,2.26437941304139,-8.93820802006958));
#65176=CARTESIAN_POINT('Ctrl Pts',(42.2360899860721,2.25805531451819,-8.84298180532608));
#65177=CARTESIAN_POINT('Ctrl Pts',(42.2118158887524,2.25173121599499,-8.74879403174244));
#65178=CARTESIAN_POINT('Ctrl Pts',(42.1875671991186,2.24541373690265,-8.65470484445572));
#65179=CARTESIAN_POINT('Ctrl Pts',(42.1588793427473,2.23909625781031,-8.56165235869884));
#65180=CARTESIAN_POINT('Ctrl Pts',(42.1258640434083,2.23277877871797,-8.47008282202319));
#65181=CARTESIAN_POINT('Ctrl Pts',(42.0928721793498,2.22646578396769,-8.37857828423685));
#65182=CARTESIAN_POINT('Ctrl Pts',(42.0555591270576,2.2201527892174,-8.28855501303765));
#65183=CARTESIAN_POINT('Ctrl Pts',(42.0140864933062,2.21383979446712,-8.20044427784569));
#65184=CARTESIAN_POINT('Ctrl Pts',(41.9726288464674,2.20752908103568,-8.11236538311758));
#65185=CARTESIAN_POINT('Ctrl Pts',(41.92701479098,2.20121836760425,-8.02619804638502));
#65186=CARTESIAN_POINT('Ctrl Pts',(41.8774537600952,2.19490765417281,-7.9423528455615));
#65187=CARTESIAN_POINT('Ctrl Pts',(41.8278972153596,2.18859751197247,-7.85851523421045));
#65188=CARTESIAN_POINT('Ctrl Pts',(41.7743946282699,2.18228736977213,-7.77699971720841));
#65189=CARTESIAN_POINT('Ctrl Pts',(41.7172004849958,2.17597722757179,-7.69819065821384));
#65190=CARTESIAN_POINT('Ctrl Pts',(41.6599960279446,2.16966594746824,-7.61936738764078));
#65191=CARTESIAN_POINT('Ctrl Pts',(41.5990989494367,2.1633546673647,-7.54325189831572));
#65192=CARTESIAN_POINT('Ctrl Pts',(41.5348053636789,2.15704338726115,-7.47019719519463));
#65193=CARTESIAN_POINT('Ctrl Pts',(41.4704430202524,2.15072535766771,-7.39706436497859));
#65194=CARTESIAN_POINT('Ctrl Pts',(41.4026772072064,2.14440732807428,-7.32699918476624));
#65195=CARTESIAN_POINT('Ctrl Pts',(41.3318422719954,2.13808929848084,-7.26031918800166));
#65196=CARTESIAN_POINT('Ctrl Pts',(41.2609658297919,2.13176756672539,-7.19360011890483));
#65197=CARTESIAN_POINT('Ctrl Pts',(41.1870170163125,2.12544583496994,-7.13027046749327));
#65198=CARTESIAN_POINT('Ctrl Pts',(41.1103631456135,2.11912410321448,-7.07060734502775));
#65199=CARTESIAN_POINT('Ctrl Pts',(41.0335863661418,2.11279223503299,-7.01084855718895));
#65200=CARTESIAN_POINT('Ctrl Pts',(40.9540962256173,2.10646036685149,-6.95476828958038));
#65201=CARTESIAN_POINT('Ctrl Pts',(40.8722888243246,2.10012849867,-6.90260019429931));
#65202=CARTESIAN_POINT('Ctrl Pts',(40.8247738891365,2.09645085702011,-6.87230020154806));
#65203=CARTESIAN_POINT('Ctrl Pts',(40.7764777108262,2.09277321537021,-6.84331910900542));
#65204=CARTESIAN_POINT('Ctrl Pts',(40.7274812829116,2.08909557372032,-6.81569536905595));
#65205=CARTESIAN_POINT('Ctrl Pts',(40.6431131484773,2.08276295360239,-6.76812938302743));
#65206=CARTESIAN_POINT('Ctrl Pts',(40.5563745365518,2.07643033348445,-6.72442538258168));
#65207=CARTESIAN_POINT('Ctrl Pts',(40.4676538386611,2.07009771336651,-6.68482669574058));
#65208=CARTESIAN_POINT('Ctrl Pts',(40.3790525446178,2.06377361594085,-6.64528130238878));
#65209=CARTESIAN_POINT('Ctrl Pts',(40.2884748624991,2.05744951851519,-6.60983041799162));
#65210=CARTESIAN_POINT('Ctrl Pts',(40.1963351000381,2.05112542108953,-6.57867228208874));
#65211=CARTESIAN_POINT('Ctrl Pts',(40.1042917803644,2.04480794310337,-6.54754675943986));
#65212=CARTESIAN_POINT('Ctrl Pts',(40.0106900429605,2.03849046511721,-6.52070519189233));
#65213=CARTESIAN_POINT('Ctrl Pts',(39.9159646374313,2.03217298713105,-6.49829795142503));
#65214=CARTESIAN_POINT('Ctrl Pts',(39.82130647106,2.02585999349519,-6.47590661634208));
#65215=CARTESIAN_POINT('Ctrl Pts',(39.7255266466333,2.01954699985933,-6.45794345104749));
#65216=CARTESIAN_POINT('Ctrl Pts',(39.6290746383508,2.01323400622348,-6.44450886908854));
#65217=CARTESIAN_POINT('Ctrl Pts',(39.5326574848847,2.00692329391114,-6.43107914197811));
#65218=CARTESIAN_POINT('Ctrl Pts',(39.4355690629136,2.0006125815988,-6.42217480674485));
#65219=CARTESIAN_POINT('Ctrl Pts',(39.3382676628183,1.99430186928646,-6.41784491756225));
#65220=CARTESIAN_POINT('Ctrl Pts',(39.2409750702715,1.98799172820849,-6.41351542031346));
#65221=CARTESIAN_POINT('Ctrl Pts',(39.1434699748185,1.98168158713053,-6.41375956508012));
#65222=CARTESIAN_POINT('Ctrl Pts',(39.0462133422926,1.97537144605256,-6.41857435034875));
#65223=CARTESIAN_POINT('Ctrl Pts',(38.9489391715773,1.96906016707328,-6.4233900038627));
#65224=CARTESIAN_POINT('Ctrl Pts',(38.851913989548,1.962748888094,-6.43277791322323));
#65225=CARTESIAN_POINT('Ctrl Pts',(38.7555952575182,1.95643760911472,-6.44668307710858));
#65226=CARTESIAN_POINT('Ctrl Pts',(38.659173518999,1.95011958064156,-6.46060311164357));
#65227=CARTESIAN_POINT('Ctrl Pts',(38.5634601723352,1.94380155216841,-6.47904998274993));
#65228=CARTESIAN_POINT('Ctrl Pts',(38.468903874672,1.93748352369525,-6.50191728389209));
#65229=CARTESIAN_POINT('Ctrl Pts',(38.3742921700424,1.93116179305946,-6.5247979845414));
#65230=CARTESIAN_POINT('Ctrl Pts',(38.2808392840599,1.92484006242367,-6.5521041504863));
#65231=CARTESIAN_POINT('Ctrl Pts',(38.1889780452493,1.91851833178789,-6.58367967403887));
#65232=CARTESIAN_POINT('Ctrl Pts',(38.0969695135832,1.91218646471404,-6.61530582666079));
#65233=CARTESIAN_POINT('Ctrl Pts',(38.0065581313407,1.90585459764019,-6.65121484504372));
#65234=CARTESIAN_POINT('Ctrl Pts',(37.9181560702437,1.89952273056634,-6.69120276084421));
#65235=CARTESIAN_POINT('Ctrl Pts',(37.8668106959715,1.89584507779768,-6.71442840148728));
#65236=CARTESIAN_POINT('Ctrl Pts',(37.8161427060572,1.89216742502901,-6.73902918483806));
#65237=CARTESIAN_POINT('Ctrl Pts',(37.7662285731077,1.88848977226034,-6.76495830677739));
#65238=CARTESIAN_POINT('Ctrl Pts',(37.6802804830955,1.88215715236861,-6.80960615248134));
#65239=CARTESIAN_POINT('Ctrl Pts',(37.5962706002101,1.87582453247687,-6.85835002622903));
#65240=CARTESIAN_POINT('Ctrl Pts',(37.5146149849758,1.86949191258514,-6.91099770389696));
#65241=CARTESIAN_POINT('Ctrl Pts',(37.4330692652116,1.86316781539252,-6.96357452616485));
#65242=CARTESIAN_POINT('Ctrl Pts',(37.3538718800542,1.85684371819989,-7.02004447501155));
#65243=CARTESIAN_POINT('Ctrl Pts',(37.2774153000616,1.85051962100727,-7.08016897834167));
#65244=CARTESIAN_POINT('Ctrl Pts',(37.201038747334,1.84420214326063,-7.14023054922626));
#65245=CARTESIAN_POINT('Ctrl Pts',(37.1273976383947,1.83788466551399,-7.20393880094852));
#65246=CARTESIAN_POINT('Ctrl Pts',(37.0568555343101,1.83156718776735,-7.27101187845124));
#65247=CARTESIAN_POINT('Ctrl Pts',(36.9863635033928,1.82525419437972,-7.33803734521896));
#65248=CARTESIAN_POINT('Ctrl Pts',(36.9189664200622,1.81894120099208,-7.40842258887038));
#65249=CARTESIAN_POINT('Ctrl Pts',(36.8549940598641,1.81262820760444,-7.48184611601883));
#65250=CARTESIAN_POINT('Ctrl Pts',(36.7910448173821,1.80631749554562,-7.55524311007945));
#65251=CARTESIAN_POINT('Ctrl Pts',(36.7305181259069,1.80000678348679,-7.6316758766227));
#65252=CARTESIAN_POINT('Ctrl Pts',(36.67370557269,1.79369607142797,-7.71078746574647));
#65253=CARTESIAN_POINT('Ctrl Pts',(36.6168981620889,1.78738593060851,-7.789891893768));
#65254=CARTESIAN_POINT('Ctrl Pts',(36.5638044762192,1.78107578978905,-7.87167430692623));
#65255=CARTESIAN_POINT('Ctrl Pts',(36.5146739743187,1.7747656489696,-7.95574706031865));
#65256=CARTESIAN_POINT('Ctrl Pts',(36.465534612801,1.76845437025352,-8.03983497440311));
#65257=CARTESIAN_POINT('Ctrl Pts',(36.4203600752962,1.76214309153745,-8.12621367143539));
#65258=CARTESIAN_POINT('Ctrl Pts',(36.3793543617298,1.75583181282138,-8.2144700170514));
#65259=CARTESIAN_POINT('Ctrl Pts',(36.3383047953098,1.74951378461706,-8.3028207468951));
#65260=CARTESIAN_POINT('Ctrl Pts',(36.3014331381041,1.74319575641274,-8.39305273697286));
#65261=CARTESIAN_POINT('Ctrl Pts',(36.2688955317398,1.73687772820842,-8.48473212630355));
#65262=CARTESIAN_POINT('Ctrl Pts',(36.2363388593963,1.73055599784504,-8.5764652367749));
#65263=CARTESIAN_POINT('Ctrl Pts',(36.2081214216448,1.72423426748166,-8.66964701699669));
#65264=CARTESIAN_POINT('Ctrl Pts',(36.1843490890647,1.71791253711828,-8.76382969298902));
#65265=CARTESIAN_POINT('Ctrl Pts',(36.1605386392775,1.71158067031984,-8.85816338405539));
#65266=CARTESIAN_POINT('Ctrl Pts',(36.1411876137695,1.7052488035214,-8.95350074722008));
#65267=CARTESIAN_POINT('Ctrl Pts',(36.1263505140941,1.69891693672297,-9.04938514458597));
#65268=CARTESIAN_POINT('Ctrl Pts',(36.1177328757093,1.69523928141543,-9.10507642396817));
#65269=CARTESIAN_POINT('Ctrl Pts',(36.1106370296069,1.69156162610789,-9.16095215353144));
#65270=CARTESIAN_POINT('Ctrl Pts',(36.1050655842624,1.68788397080035,-9.21692271232171));
#65271=CARTESIAN_POINT('Ctrl Pts',(36.0949386176573,1.68119926150462,-9.3186578895869));
#65272=CARTESIAN_POINT('Ctrl Pts',(36.0898268905567,1.67451455220889,-9.42090043518689));
#65273=CARTESIAN_POINT('Ctrl Pts',(36.0897704721985,1.66782984291316,-9.52328614715663));
#65274=CARTESIAN_POINT('',(36.08977020096,0.397829842977112,-9.52388193753632));
#65275=CARTESIAN_POINT('Ctrl Pts',(36.0897704721981,1.66782984286977,-9.52328614782123));
#65276=CARTESIAN_POINT('Ctrl Pts',(36.0897177166195,1.66157911429467,-9.61902483550123));
#65277=CARTESIAN_POINT('Ctrl Pts',(36.094089700507,1.65532838571958,-9.71493781111452));
#65278=CARTESIAN_POINT('Ctrl Pts',(36.1029083362522,1.64907765714449,-9.8105763982615));
#65279=CARTESIAN_POINT('Ctrl Pts',(36.1117161895845,1.64283457124101,-9.90609804954951));
#65280=CARTESIAN_POINT('Ctrl Pts',(36.1249598533129,1.63659148533753,-10.0013455349007));
#65281=CARTESIAN_POINT('Ctrl Pts',(36.1426092124648,1.63034839943405,-10.0958697094739));
#65282=CARTESIAN_POINT('Ctrl Pts',(36.1602423302137,1.6241110585819,-10.1903069004235));
#65283=CARTESIAN_POINT('Ctrl Pts',(36.1822730039185,1.61787371772975,-10.2840216636972));
#65284=CARTESIAN_POINT('Ctrl Pts',(36.2086193831783,1.61163637687759,-10.3765707006487));
#65285=CARTESIAN_POINT('Ctrl Pts',(36.2349529388969,1.60540207191878,-10.4690746913199));
#65286=CARTESIAN_POINT('Ctrl Pts',(36.2655979066875,1.59916776695996,-10.5604136509191));
#65287=CARTESIAN_POINT('Ctrl Pts',(36.3004217192847,1.59293346200114,-10.650156187782));
#65288=CARTESIAN_POINT('Ctrl Pts',(36.3352385865237,1.58670040042946,-10.7398808261434));
#65289=CARTESIAN_POINT('Ctrl Pts',(36.374232480264,1.58046733885778,-10.8280092555743));
#65290=CARTESIAN_POINT('Ctrl Pts',(36.4172219193474,1.5742342772861,-10.9141280742752));
#65291=CARTESIAN_POINT('Ctrl Pts',(36.4602151348599,1.56800066816797,-11.0002544581274));
#65292=CARTESIAN_POINT('Ctrl Pts',(36.5072043906412,1.56176705904983,-11.0843704793567));
#65293=CARTESIAN_POINT('Ctrl Pts',(36.5579618411616,1.5555334499317,-11.1660865364574));
#65294=CARTESIAN_POINT('Ctrl Pts',(36.6087696800298,1.54929365253459,-11.2478837153848));
#65295=CARTESIAN_POINT('Ctrl Pts',(36.6633529439873,1.54305385513747,-11.327275791583));
#65296=CARTESIAN_POINT('Ctrl Pts',(36.7214401637571,1.53681405774035,-11.4039017513068));
#65297=CARTESIAN_POINT('Ctrl Pts',(36.7795583433284,1.53057093460498,-11.4805685517613));
#65298=CARTESIAN_POINT('Ctrl Pts',(36.8411839074336,1.52432781146962,-11.5544659570656));
#65299=CARTESIAN_POINT('Ctrl Pts',(36.906006215445,1.51808468833425,-11.6252674042424));
#65300=CARTESIAN_POINT('Ctrl Pts',(36.9709326194122,1.51183153957822,-11.6961825490727));
#65301=CARTESIAN_POINT('Ctrl Pts',(37.0390656975799,1.50557839082219,-11.7639914937854));
#65302=CARTESIAN_POINT('Ctrl Pts',(37.1100593558897,1.49932524206616,-11.8284059036557));
#65303=CARTESIAN_POINT('Ctrl Pts',(37.1556505611154,1.49530955115757,-11.8697720009918));
#65304=CARTESIAN_POINT('Ctrl Pts',(37.2024208073046,1.49129386024897,-11.9097389989716));
#65305=CARTESIAN_POINT('Ctrl Pts',(37.2502721211606,1.48727816934038,-11.9482399491954));
#65306=CARTESIAN_POINT('Ctrl Pts',(37.3257321603814,1.48094554920851,-12.0089547547003));
#65307=CARTESIAN_POINT('Ctrl Pts',(37.4041619730563,1.47461292907664,-12.0662469089251));
#65308=CARTESIAN_POINT('Ctrl Pts',(37.4852181569681,1.46828030894477,-12.1198128802879));
#65309=CARTESIAN_POINT('Ctrl Pts',(37.5661652522127,1.46195621150737,-12.1733067604155));
#65310=CARTESIAN_POINT('Ctrl Pts',(37.6497313315992,1.45563211406997,-12.2230841858521));
#65311=CARTESIAN_POINT('Ctrl Pts',(37.735540056303,1.44930801663257,-12.2688818717662));
#65312=CARTESIAN_POINT('Ctrl Pts',(37.8212589648937,1.44299053863687,-12.3146316211778));
#65313=CARTESIAN_POINT('Ctrl Pts',(37.9092154683211,1.43667306064118,-12.3564097076499));
#65314=CARTESIAN_POINT('Ctrl Pts',(37.9990052376984,1.43035558264549,-12.39399672949));
#65315=CARTESIAN_POINT('Ctrl Pts',(38.0887312713447,1.42404258900342,-12.4315570708259));
#65316=CARTESIAN_POINT('Ctrl Pts',(38.1802875816035,1.41772959536135,-12.4649320935326));
#65317=CARTESIAN_POINT('Ctrl Pts',(38.2732471482195,1.41141660171928,-12.4939492761947));
#65318=CARTESIAN_POINT('Ctrl Pts',(38.3661731220506,1.4051058894028,-12.5229559729216));
#65319=CARTESIAN_POINT('Ctrl Pts',(38.4605009276115,1.39879517708631,-12.5476078285589));
#65320=CARTESIAN_POINT('Ctrl Pts',(38.5557864532949,1.39248446476983,-12.5677815496913));
#65321=CARTESIAN_POINT('Ctrl Pts',(38.6510633538717,1.38617432368981,-12.5879534447279));
#65322=CARTESIAN_POINT('Ctrl Pts',(38.7472973743376,1.37986418260979,-12.603647920822));
#65323=CARTESIAN_POINT('Ctrl Pts',(38.8440332560997,1.37355404152977,-12.6147926030944));
#65324=CARTESIAN_POINT('Ctrl Pts',(38.9407865821129,1.36724276255051,-12.6259392950724));
#65325=CARTESIAN_POINT('Ctrl Pts',(39.038041514729,1.36093148357126,-12.6325345136804));
#65326=CARTESIAN_POINT('Ctrl Pts',(39.1353377543829,1.354620204592,-12.6345577574459));
#65327=CARTESIAN_POINT('Ctrl Pts',(39.2327380458558,1.34830217612211,-12.6365831649352));
#65328=CARTESIAN_POINT('Ctrl Pts',(39.3301792946209,1.34198414765222,-12.6340268270135));
#65329=CARTESIAN_POINT('Ctrl Pts',(39.4272014857098,1.33566611918233,-12.6269203951409));
#65330=CARTESIAN_POINT('Ctrl Pts',(39.524280528672,1.32934438855162,-12.6198097991286));
#65331=CARTESIAN_POINT('Ctrl Pts',(39.6209395910218,1.32302265792092,-12.6081438523935));
#65332=CARTESIAN_POINT('Ctrl Pts',(39.7167261508899,1.31670092729021,-12.5920058261905));
#65333=CARTESIAN_POINT('Ctrl Pts',(39.8126662975388,1.31036906022431,-12.5758419238365));
#65334=CARTESIAN_POINT('Ctrl Pts',(39.9077307210829,1.30403719315842,-12.5551917162477));
#65335=CARTESIAN_POINT('Ctrl Pts',(40.0014794568133,1.29770532609252,-12.5301890677969));
#65336=CARTESIAN_POINT('Ctrl Pts',(40.0559302674504,1.29402767335515,-12.5156671175476));
#65337=CARTESIAN_POINT('Ctrl Pts',(40.1099375420237,1.29035002061777,-12.4996778081882));
#65338=CARTESIAN_POINT('Ctrl Pts',(40.1634181868812,1.2866723678804,-12.4822548165633));
#65339=CARTESIAN_POINT('Ctrl Pts',(40.2555075253338,1.28033974776062,-12.4522538362669));
#65340=CARTESIAN_POINT('Ctrl Pts',(40.3463541332558,1.27400712764084,-12.4178951367548));
#65341=CARTESIAN_POINT('Ctrl Pts',(40.4355161287737,1.26767450752106,-12.3793003605858));
#65342=CARTESIAN_POINT('Ctrl Pts',(40.524558126488,1.26135041009641,-12.3407575268205));
#65343=CARTESIAN_POINT('Ctrl Pts',(40.6119196200631,1.25502631267176,-12.297990119818));
#65344=CARTESIAN_POINT('Ctrl Pts',(40.697174425737,1.24870221524711,-12.2511693622772));
#65345=CARTESIAN_POINT('Ctrl Pts',(40.7823399950771,1.24238473726479,-12.2043976120941));
#65346=CARTESIAN_POINT('Ctrl Pts',(40.8654028790095,1.23606725928246,-12.1535811553654));
#65347=CARTESIAN_POINT('Ctrl Pts',(40.9459583408031,1.22974978130014,-12.0989386405041));
#65348=CARTESIAN_POINT('Ctrl Pts',(41.0264566216689,1.22343678767238,-12.0443349127049));
#65349=CARTESIAN_POINT('Ctrl Pts',(41.1044506579647,1.21712379404462,-11.9859107708638));
#65350=CARTESIAN_POINT('Ctrl Pts',(41.1795625661053,1.21081080041686,-11.9239294903716));
#65351=CARTESIAN_POINT('Ctrl Pts',(41.2546473310598,1.20450008811525,-11.8619706080512));
#65352=CARTESIAN_POINT('Ctrl Pts',(41.3268517004008,1.19818937581364,-11.7964574193223));
#65353=CARTESIAN_POINT('Ctrl Pts',(41.3958296707027,1.19187866351202,-11.7276944205136));
#65354=CARTESIAN_POINT('Ctrl Pts',(41.4648013972136,1.18556852244741,-11.658937646037));
#65355=CARTESIAN_POINT('Ctrl Pts',(41.5305469957859,1.1792583813828,-11.5869319552453));
#65356=CARTESIAN_POINT('Ctrl Pts',(41.5927570080808,1.17294824031818,-11.5120190117812));
#65357=CARTESIAN_POINT('Ctrl Pts',(41.654978238618,1.16663696135488,-11.4370925593736));
#65358=CARTESIAN_POINT('Ctrl Pts',(41.7136623372357,1.16032568239159,-11.3592581494967));
#65359=CARTESIAN_POINT('Ctrl Pts',(41.7685405279353,1.15401440342829,-11.278890021995));
#65360=CARTESIAN_POINT('Ctrl Pts',(41.8234774071826,1.14769637497505,-11.1984359461663));
#65361=CARTESIAN_POINT('Ctrl Pts',(41.8746000056417,1.14137834652181,-11.1154431048064));
#65362=CARTESIAN_POINT('Ctrl Pts',(41.9216833747809,1.13506031806857,-11.0303140072228));
#65363=CARTESIAN_POINT('Ctrl Pts',(41.9687943332519,1.12873858745496,-10.9451350267408));
#65364=CARTESIAN_POINT('Ctrl Pts',(42.0118611559856,1.12241685684135,-10.8578176894343));
#65365=CARTESIAN_POINT('Ctrl Pts',(42.0507062157808,1.11609512622774,-10.7687864463841));
#65366=CARTESIAN_POINT('Ctrl Pts',(42.0896135608007,1.10976325917944,-10.6796124482188));
#65367=CARTESIAN_POINT('Ctrl Pts',(42.1242854700353,1.10343139213113,-10.5887194651272));
#65368=CARTESIAN_POINT('Ctrl Pts',(42.1545935460052,1.09709952508282,-10.4965490882113));
#65369=CARTESIAN_POINT('Ctrl Pts',(42.1721969767555,1.09342187219535,-10.4430150120506));
#65370=CARTESIAN_POINT('Ctrl Pts',(42.1883292228158,1.08974421930789,-10.3890502585163));
#65371=CARTESIAN_POINT('Ctrl Pts',(42.2029730639892,1.08606656642042,-10.3347428171064));
#65372=CARTESIAN_POINT('Ctrl Pts',(42.2281885714969,1.07973394624948,-10.2412298050229));
#65373=CARTESIAN_POINT('Ctrl Pts',(42.2490757054682,1.07340132607854,-10.1463754208036));
#65374=CARTESIAN_POINT('Ctrl Pts',(42.2654947861516,1.0670687059076,-10.0506161802851));
#65375=CARTESIAN_POINT('Ctrl Pts',(42.2818917693775,1.06074460843094,-9.95498581639423));
#65376=CARTESIAN_POINT('Ctrl Pts',(42.2938325777206,1.05442051095429,-9.85845344400553));
#65377=CARTESIAN_POINT('Ctrl Pts',(42.3012276298065,1.04809641347763,-9.76146953508838));
#65378=CARTESIAN_POINT('Ctrl Pts',(42.3086149414812,1.04177893544254,-9.66458713936265));
#65379=CARTESIAN_POINT('Ctrl Pts',(42.3114659230558,1.03546145740745,-9.56725458046418));
#65380=CARTESIAN_POINT('Ctrl Pts',(42.309742429924,1.02914397937235,-9.46993029480624));
#65381=CARTESIAN_POINT('Ctrl Pts',(42.3080201601844,1.02283098569086,-9.37267509312588));
#65382=CARTESIAN_POINT('Ctrl Pts',(42.3017298789135,1.01651799200937,-9.27542858901532));
#65383=CARTESIAN_POINT('Ctrl Pts',(42.2908854897475,1.01020499832788,-9.17865112650952));
#65384=CARTESIAN_POINT('Ctrl Pts',(42.2800450194169,1.00389428597198,-9.08190863646093));
#65385=CARTESIAN_POINT('Ctrl Pts',(42.2646537598981,0.997583573616074,-8.98563528537614));
#65386=CARTESIAN_POINT('Ctrl Pts',(42.2447775587764,0.99127286126017,-8.89028725357704));
#65387=CARTESIAN_POINT('Ctrl Pts',(42.2249031568195,0.984962720140777,-8.7949478525432));
#65388=CARTESIAN_POINT('Ctrl Pts',(42.2005447098696,0.978652579021385,-8.70053403232942));
#65389=CARTESIAN_POINT('Ctrl Pts',(42.1718191649682,0.972342437901991,-8.60749168743394));
#65390=CARTESIAN_POINT('Ctrl Pts',(42.1430884400284,0.966031158883453,-8.51443256433925));
#65391=CARTESIAN_POINT('Ctrl Pts',(42.1099891820753,0.959719879864914,-8.42274582559994));
#65392=CARTESIAN_POINT('Ctrl Pts',(42.0726878545949,0.953408600846376,-8.33286110584249));
#65393=CARTESIAN_POINT('Ctrl Pts',(42.0353466358428,0.947090572337603,-8.24288026039698));
#65394=CARTESIAN_POINT('Ctrl Pts',(41.9937945437706,0.940772543828831,-8.15470568593885));
#65395=CARTESIAN_POINT('Ctrl Pts',(41.9482456711112,0.934454515320058,-8.06874576940746));
#65396=CARTESIAN_POINT('Ctrl Pts',(41.9026701082835,0.928132784650637,-7.98273548314129));
#65397=CARTESIAN_POINT('Ctrl Pts',(41.8530933239235,0.921811053981216,-7.89894281511702));
#65398=CARTESIAN_POINT('Ctrl Pts',(41.799773651133,0.915489323311794,-7.81774852005495));
#65399=CARTESIAN_POINT('Ctrl Pts',(41.7463684841319,0.909157456207825,-7.73642403585629));
#65400=CARTESIAN_POINT('Ctrl Pts',(41.6892087016501,0.902825589103855,-7.65770659763154));
#65401=CARTESIAN_POINT('Ctrl Pts',(41.6285938994227,0.896493721999885,-7.58194510510211));
#65402=CARTESIAN_POINT('Ctrl Pts',(41.5933878273459,0.8928160696534,-7.53794158667712));
#65403=CARTESIAN_POINT('Ctrl Pts',(41.5570169369935,0.889138417306913,-7.49493459441095));
#65404=CARTESIAN_POINT('Ctrl Pts',(41.5195454962285,0.885460764960428,-7.45298664487264));
#65405=CARTESIAN_POINT('Ctrl Pts',(41.4550227033396,0.879128144814911,-7.38075566562761));
#65406=CARTESIAN_POINT('Ctrl Pts',(41.3870106994681,0.872795524669392,-7.31141596690157));
#65407=CARTESIAN_POINT('Ctrl Pts',(41.3157986633026,0.866462904523875,-7.24532312174136));
#65408=CARTESIAN_POINT('Ctrl Pts',(41.2446824671559,0.860138807072926,-7.17931922698708));
#65409=CARTESIAN_POINT('Ctrl Pts',(41.1703751163723,0.853814709621979,-7.1165537957038));
#65410=CARTESIAN_POINT('Ctrl Pts',(41.0932048609678,0.847490612171031,-7.05734807817065));
#65411=CARTESIAN_POINT('Ctrl Pts',(41.0161153797798,0.841173134161922,-6.99820433134664));
#65412=CARTESIAN_POINT('Ctrl Pts',(40.9361692965096,0.834855656152813,-6.94261315568515));
#65413=CARTESIAN_POINT('Ctrl Pts',(40.8537296467609,0.828538178143704,-6.89085708278307));
#65414=CARTESIAN_POINT('Ctrl Pts',(40.7713485153901,0.822225184488502,-6.8391377480457));
#65415=CARTESIAN_POINT('Ctrl Pts',(40.6864777057602,0.8159121908333,-6.79124833587066));
#65416=CARTESIAN_POINT('Ctrl Pts',(40.5995103014359,0.809599197178097,-6.74742883636173));
#65417=CARTESIAN_POINT('Ctrl Pts',(40.5125743245118,0.803288484848641,-6.70362517189999));
#65418=CARTESIAN_POINT('Ctrl Pts',(40.4235436484879,0.796977772519183,-6.66388869429876));
#65419=CARTESIAN_POINT('Ctrl Pts',(40.3328362638571,0.790667060189726,-6.62841362079596));
#65420=CARTESIAN_POINT('Ctrl Pts',(40.2421370899287,0.784356919096905,-6.59294175844597));
#65421=CARTESIAN_POINT('Ctrl Pts',(40.1497619165014,0.778046778004085,-6.56173069234922));
#65422=CARTESIAN_POINT('Ctrl Pts',(40.0561480528386,0.771736636911264,-6.53492622757887));
#65423=CARTESIAN_POINT('Ctrl Pts',(39.9625173079169,0.765425357919411,-6.50811692919638));
#65424=CARTESIAN_POINT('Ctrl Pts',(39.8676478495388,0.759114078927558,-6.48571593073111));
#65425=CARTESIAN_POINT('Ctrl Pts',(39.7719904378764,0.752802799935705,-6.46781868514836));
#65426=CARTESIAN_POINT('Ctrl Pts',(39.6762307270179,0.746484771453607,-6.44990229965995));
#65427=CARTESIAN_POINT('Ctrl Pts',(39.5796818111064,0.740166742971509,-6.4364993634139));
#65428=CARTESIAN_POINT('Ctrl Pts',(39.4828026929409,0.733848714489411,-6.4276538311378));
#65429=CARTESIAN_POINT('Ctrl Pts',(39.3858668067417,0.727526983846716,-6.41880311566552));
#65430=CARTESIAN_POINT('Ctrl Pts',(39.2886007696971,0.721205253204021,-6.41451514109264));
#65431=CARTESIAN_POINT('Ctrl Pts',(39.1914646285191,0.714883522561326,-6.41478171178715));
#65432=CARTESIAN_POINT('Ctrl Pts',(39.0941727366117,0.708551655483863,-6.41504870990836));
#65433=CARTESIAN_POINT('Ctrl Pts',(38.9970115929632,0.702219788406399,-6.41988481414417));
#65434=CARTESIAN_POINT('Ctrl Pts',(38.9004371244342,0.695887921328936,-6.42922986375236));
#65435=CARTESIAN_POINT('Ctrl Pts',(38.8443450836742,0.692210268719442,-6.43465762236715));
#65436=CARTESIAN_POINT('Ctrl Pts',(38.7884508038198,0.688532616109947,-6.44160549850996));
#65437=CARTESIAN_POINT('Ctrl Pts',(38.7328417651375,0.684854963500453,-6.45005384819504));
#65438=CARTESIAN_POINT('Ctrl Pts',(38.6370875011892,0.678522343354097,-6.4646012225939));
#65439=CARTESIAN_POINT('Ctrl Pts',(38.5418470733761,0.672189723207741,-6.48365082630189));
#65440=CARTESIAN_POINT('Ctrl Pts',(38.4475763025267,0.665857103061384,-6.50715486938435));
#65441=CARTESIAN_POINT('Ctrl Pts',(38.3534324050684,0.659533005609661,-6.53062727978125));
#65442=CARTESIAN_POINT('Ctrl Pts',(38.2602559915588,0.653208908157937,-6.55854210938224));
#65443=CARTESIAN_POINT('Ctrl Pts',(38.1684954987019,0.646884810706214,-6.59080008917221));
#65444=CARTESIAN_POINT('Ctrl Pts',(38.0768310516849,0.640567332696389,-6.62302430448834));
#65445=CARTESIAN_POINT('Ctrl Pts',(37.9865799893365,0.634249854686566,-6.65958248809077));
#65446=CARTESIAN_POINT('Ctrl Pts',(37.8981773405126,0.627932376676741,-6.70032507779298));
#65447=CARTESIAN_POINT('Ctrl Pts',(37.8098374428005,0.621619383020876,-6.74103874706314));
#65448=CARTESIAN_POINT('Ctrl Pts',(37.7233437461858,0.615306389365011,-6.7859307349164));
#65449=CARTESIAN_POINT('Ctrl Pts',(37.6391120808485,0.608993395709147,-6.83480306357564));
#65450=CARTESIAN_POINT('Ctrl Pts',(37.5549108542985,0.602682683379081,-6.88365773124704));
#65451=CARTESIAN_POINT('Ctrl Pts',(37.4729704126545,0.596371971049014,-6.93648966241158));
#65452=CARTESIAN_POINT('Ctrl Pts',(37.3936818713432,0.590061258718948,-6.99305500237745));
#65453=CARTESIAN_POINT('Ctrl Pts',(37.3144005071177,0.583751117625572,-7.04961522212933));
#65454=CARTESIAN_POINT('Ctrl Pts',(37.2377709218384,0.577440976532196,-7.10990792462877));
#65455=CARTESIAN_POINT('Ctrl Pts',(37.164154251486,0.57113083543882,-7.17364661499862));
#65456=CARTESIAN_POINT('Ctrl Pts',(37.0905243059421,0.564819556446501,-7.23739679927759));
#65457=CARTESIAN_POINT('Ctrl Pts',(37.0199086850006,0.558508277454183,-7.30459391935354));
#65458=CARTESIAN_POINT('Ctrl Pts',(36.9526337132396,0.552196998461865,-7.37491269339294));
#65459=CARTESIAN_POINT('Ctrl Pts',(36.8852867954021,0.545878969979356,-7.44530666865163));
#65460=CARTESIAN_POINT('Ctrl Pts',(36.8212879620569,0.539560941496847,-7.51882864629538));
#65461=CARTESIAN_POINT('Ctrl Pts',(36.7609249196866,0.533242913014338,-7.59511829235724));
#65462=CARTESIAN_POINT('Ctrl Pts',(36.7005265065239,0.526921182371293,-7.67145264168656));
#65463=CARTESIAN_POINT('Ctrl Pts',(36.643768381483,0.520599451728249,-7.75055753365188));
#65464=CARTESIAN_POINT('Ctrl Pts',(36.5908951519223,0.514277721085204,-7.83204325376056));
#65465=CARTESIAN_POINT('Ctrl Pts',(36.5379371439888,0.507945854007472,-7.91365963028698));
#65466=CARTESIAN_POINT('Ctrl Pts',(36.4888766904532,0.501613986929741,-7.99766408041352));
#65467=CARTESIAN_POINT('Ctrl Pts',(36.4439126320639,0.49528211985201,-8.08364193442328));
#65468=CARTESIAN_POINT('Ctrl Pts',(36.4177967669668,0.491604467248162,-8.13357928699093));
#65469=CARTESIAN_POINT('Ctrl Pts',(36.3930619200093,0.487926814644315,-8.1841819632088));
#65470=CARTESIAN_POINT('Ctrl Pts',(36.3697394600482,0.484249162040468,-8.23536597094681));
#65471=CARTESIAN_POINT('Ctrl Pts',(36.3240692249413,0.47704755211852,-8.33559492068105));
#65472=CARTESIAN_POINT('Ctrl Pts',(36.2836741068734,0.469845942196575,-8.43836987688406));
#65473=CARTESIAN_POINT('Ctrl Pts',(36.2488179398193,0.462644332274628,-8.54313692371715));
#65474=CARTESIAN_POINT('Ctrl Pts',(36.2155628225379,0.455773514201086,-8.6430917014258));
#65475=CARTESIAN_POINT('Ctrl Pts',(36.1873493158459,0.448902696127545,-8.74485929566455));
#65476=CARTESIAN_POINT('Ctrl Pts',(36.1643595640711,0.442031878054002,-8.84793442219139));
#65477=CARTESIAN_POINT('Ctrl Pts',(36.1414261472589,0.435177896494522,-8.95075696950586));
#65478=CARTESIAN_POINT('Ctrl Pts',(36.123691054362,0.428323914935042,-9.0548803662193));
#65479=CARTESIAN_POINT('Ctrl Pts',(36.1112870594205,0.421469933375563,-9.15978359347306));
#65480=CARTESIAN_POINT('Ctrl Pts',(36.0989262652497,0.414639822938852,-9.26432146260688));
#65481=CARTESIAN_POINT('Ctrl Pts',(36.0918596059849,0.407809712502143,-9.36963344301793));
#65482=CARTESIAN_POINT('Ctrl Pts',(36.0901688933401,0.400979602065433,-9.47518894750603));
#65483=CARTESIAN_POINT('Ctrl Pts',(36.0899089982004,0.399929682369326,-9.49141486423484));
#65484=CARTESIAN_POINT('Ctrl Pts',(36.0897760372556,0.398879762673219,-9.50764651150324));
#65485=CARTESIAN_POINT('Ctrl Pts',(36.08977020096,0.397829842977112,-9.52388193753633));
#65486=CARTESIAN_POINT('',(36.0897712321793,-0.872170157086845,-9.5277685231493));
#65487=CARTESIAN_POINT('Ctrl Pts',(36.0897702009597,0.39782984291316,-9.52388193852522));
#65488=CARTESIAN_POINT('Ctrl Pts',(36.0897343557348,0.391381464763058,-9.62359638990521));
#65489=CARTESIAN_POINT('Ctrl Pts',(36.0944981487142,0.384933086612956,-9.7232801458052));
#65490=CARTESIAN_POINT('Ctrl Pts',(36.1040264597517,0.378484708462853,-9.82245334253061));
#65491=CARTESIAN_POINT('Ctrl Pts',(36.1135603149128,0.372032578272663,-9.92168424396891));
#65492=CARTESIAN_POINT('Ctrl Pts',(36.1278641678259,0.365580448082471,-10.0204035870194));
#65493=CARTESIAN_POINT('Ctrl Pts',(36.1468512464212,0.359128317892281,-10.1181385516219));
#65494=CARTESIAN_POINT('Ctrl Pts',(36.1658692662952,0.352665673332668,-10.2160327847905));
#65495=CARTESIAN_POINT('Ctrl Pts',(36.1895856790021,0.346203028773054,-10.3129390317701));
#65496=CARTESIAN_POINT('Ctrl Pts',(36.217862847812,0.339740384213441,-10.4083960937427));
#65497=CARTESIAN_POINT('Ctrl Pts',(36.2461635676093,0.333272357160923,-10.503932658302));
#65498=CARTESIAN_POINT('Ctrl Pts',(36.2790324788456,0.326804330108407,-10.5980172454756));
#65499=CARTESIAN_POINT('Ctrl Pts',(36.3162831849237,0.320336303055889,-10.6902072705516));
#65500=CARTESIAN_POINT('Ctrl Pts',(36.3536114327368,0.313854812042757,-10.7825892000301));
#65501=CARTESIAN_POINT('Ctrl Pts',(36.3953395343823,0.307373321029622,-10.8730683119811));
#65502=CARTESIAN_POINT('Ctrl Pts',(36.4412340768188,0.300891830016489,-10.9612246460753));
#65503=CARTESIAN_POINT('Ctrl Pts',(36.4819454198771,0.295142340204486,-11.0394248539767));
#65504=CARTESIAN_POINT('Ctrl Pts',(36.5259344897854,0.289392850392485,-11.1157975248511));
#65505=CARTESIAN_POINT('Ctrl Pts',(36.5730104120667,0.283643360580482,-11.1900694753642));
#65506=CARTESIAN_POINT('Ctrl Pts',(36.624860914235,0.277310740431624,-11.2718743077396));
#65507=CARTESIAN_POINT('Ctrl Pts',(36.6806262385994,0.270978120282766,-11.3513969780834));
#65508=CARTESIAN_POINT('Ctrl Pts',(36.7400792061342,0.264645500133907,-11.4282394333889));
#65509=CARTESIAN_POINT('Ctrl Pts',(36.7994521594771,0.258321402679619,-11.5049784710314));
#65510=CARTESIAN_POINT('Ctrl Pts',(36.8625026264951,0.251997305225331,-11.579044120041));
#65511=CARTESIAN_POINT('Ctrl Pts',(36.9289592727588,0.245673207771043,-11.6500658032427));
#65512=CARTESIAN_POINT('Ctrl Pts',(36.9953463587561,0.239355729758577,-11.7210131479474));
#65513=CARTESIAN_POINT('Ctrl Pts',(37.0651322388804,0.23303825174611,-11.7889225433691));
#65514=CARTESIAN_POINT('Ctrl Pts',(37.1380049329877,0.226720773733644,-11.8534559253971));
#65515=CARTESIAN_POINT('Ctrl Pts',(37.2108258996572,0.220407780075086,-11.9179434995057));
#65516=CARTESIAN_POINT('Ctrl Pts',(37.2867289977642,0.214094786416527,-11.9790595353139));
#65517=CARTESIAN_POINT('Ctrl Pts',(37.3653656506136,0.20778179275797,-12.0365030274621));
#65518=CARTESIAN_POINT('Ctrl Pts',(37.4439738865452,0.20147108042517,-12.0939257612625));
#65519=CARTESIAN_POINT('Ctrl Pts',(37.5253133616304,0.195160368092372,-12.1476783307608));
#65520=CARTESIAN_POINT('Ctrl Pts',(37.6090034464273,0.188849655759572,-12.1975008174779));
#65521=CARTESIAN_POINT('Ctrl Pts',(37.6926859557175,0.182539514663424,-12.2473187943347));
#65522=CARTESIAN_POINT('Ctrl Pts',(37.7787182758046,0.176229373567277,-12.2932071721927));
#65523=CARTESIAN_POINT('Ctrl Pts',(37.8666928061809,0.169919232471129,-12.3349506365433));
#65524=CARTESIAN_POINT('Ctrl Pts',(37.9546832008825,0.163607953475969,-12.3767016284351));
#65525=CARTESIAN_POINT('Ctrl Pts',(38.0446161063843,0.157296674480808,-12.4143060348617));
#65526=CARTESIAN_POINT('Ctrl Pts',(38.136062423033,0.150985395485647,-12.4475960181348));
#65527=CARTESIAN_POINT('Ctrl Pts',(38.2276065353931,0.144667367000273,-12.4809216028156));
#65528=CARTESIAN_POINT('Ctrl Pts',(38.3206668785228,0.138349338514899,-12.5099234029303));
#65529=CARTESIAN_POINT('Ctrl Pts',(38.4147978045665,0.132031310029525,-12.5344830395246));
#65530=CARTESIAN_POINT('Ctrl Pts',(38.5089838882917,0.125709579383574,-12.5590570672726));
#65531=CARTESIAN_POINT('Ctrl Pts',(38.6042413764323,0.119387848737622,-12.5791836579252));
#65532=CARTESIAN_POINT('Ctrl Pts',(38.7001150682789,0.113066118091671,-12.5947957111082));
#65533=CARTESIAN_POINT('Ctrl Pts',(38.7961424866082,0.106734251011021,-12.6104327970814));
#65534=CARTESIAN_POINT('Ctrl Pts',(38.8927876474032,0.10040238393037,-12.6215408412043));
#65535=CARTESIAN_POINT('Ctrl Pts',(38.9895909217126,0.0940705168497189,
-12.6281046828417));
#65536=CARTESIAN_POINT('Ctrl Pts',(39.0458158561015,0.090392864273315,-12.6319170700573));
#65537=CARTESIAN_POINT('Ctrl Pts',(39.1020941225829,0.086715211696911,-12.6341974578348));
#65538=CARTESIAN_POINT('Ctrl Pts',(39.1583362066502,0.0830375591205073,
-12.6349509290701));
#65539=CARTESIAN_POINT('Ctrl Pts',(39.2551805244327,0.0767049389712069,
-12.636248345568));
#65540=CARTESIAN_POINT('Ctrl Pts',(39.3522537177662,0.0703723188219073,
-12.6330200894804));
#65541=CARTESIAN_POINT('Ctrl Pts',(39.4490982840774,0.0640396986726079,
-12.6252388130223));
#65542=CARTESIAN_POINT('Ctrl Pts',(39.5458125130811,0.0577156012178801,
-12.6174680089186));
#65543=CARTESIAN_POINT('Ctrl Pts',(39.6422982943944,0.0513915037631515,
-12.6051563981387));
#65544=CARTESIAN_POINT('Ctrl Pts',(39.7380969970189,0.0450674063084238,
-12.5883286266249));
#65545=CARTESIAN_POINT('Ctrl Pts',(39.8337954270048,0.0387499282955115,
-12.5715184687635));
#65546=CARTESIAN_POINT('Ctrl Pts',(39.9288077795831,0.0324324502826007,
-12.5502016230762));
#65547=CARTESIAN_POINT('Ctrl Pts',(40.0226804318778,0.0261149722696885,
-12.5244545437305));
#65548=CARTESIAN_POINT('Ctrl Pts',(40.1164864502727,0.0198019786107041,
-12.4987257405095));
#65549=CARTESIAN_POINT('Ctrl Pts',(40.2091539561765,0.0134889849517186,
-12.4685730708776));
#65550=CARTESIAN_POINT('Ctrl Pts',(40.3002403546591,0.00717599129273427,
-12.4341238912909));
#65551=CARTESIAN_POINT('Ctrl Pts',(40.3912938372609,0.000865278959509648,
-12.3996871606001));
#65552=CARTESIAN_POINT('Ctrl Pts',(40.4807669391273,-0.0054454333737152,
-12.3609571595875));
#65553=CARTESIAN_POINT('Ctrl Pts',(40.5682339500845,-0.0117561457069399,
-12.3181105439521));
#65554=CARTESIAN_POINT('Ctrl Pts',(40.6556930436529,-0.0180662868035042,
-12.275267806731));
#65555=CARTESIAN_POINT('Ctrl Pts',(40.7411460147206,-0.0243764279000681,
-12.2283093883281));
#65556=CARTESIAN_POINT('Ctrl Pts',(40.8241897607595,-0.0306865689966322,
-12.177458910887));
#65557=CARTESIAN_POINT('Ctrl Pts',(40.9072484819621,-0.0369978479921994,
-12.1265992636498));
#65558=CARTESIAN_POINT('Ctrl Pts',(40.987896742334,-0.043309126987767,-12.0718463918084));
#65559=CARTESIAN_POINT('Ctrl Pts',(41.0657594437187,-0.0496204059833341,
-12.0134678722207));
#65560=CARTESIAN_POINT('Ctrl Pts',(41.143705414048,-0.0559384344691134,
-11.9550269207159));
#65561=CARTESIAN_POINT('Ctrl Pts',(41.2188595275753,-0.0622564629548936,
-11.8929528432398));
#65562=CARTESIAN_POINT('Ctrl Pts',(41.2908790564124,-0.068574491440673,
-11.8275541088878));
#65563=CARTESIAN_POINT('Ctrl Pts',(41.3629407863668,-0.0748962220870305,
-11.7621170529902));
#65564=CARTESIAN_POINT('Ctrl Pts',(41.431863964685,-0.0812179527333876,
-11.6933517696709));
#65565=CARTESIAN_POINT('Ctrl Pts',(41.4973435814427,-0.0875396833797453,
-11.621602757249));
#65566=CARTESIAN_POINT('Ctrl Pts',(41.562928189997,-0.0938715504607866,
-11.5497387005111));
#65567=CARTESIAN_POINT('Ctrl Pts',(41.6250579324058,-0.100203417541828,
-11.4748816977733));
#65568=CARTESIAN_POINT('Ctrl Pts',(41.6834688715607,-0.106535284622869,
-11.3974083467259));
#65569=CARTESIAN_POINT('Ctrl Pts',(41.7173949059955,-0.110212937195073,
-11.3524105498503));
#65570=CARTESIAN_POINT('Ctrl Pts',(41.750067224777,-0.113890589767275,-11.3065306738168));
#65571=CARTESIAN_POINT('Ctrl Pts',(41.781441153907,-0.117568242339479,-11.259846454824));
#65572=CARTESIAN_POINT('Ctrl Pts',(41.8354645212297,-0.12390086248949,-11.1794600071983));
#65573=CARTESIAN_POINT('Ctrl Pts',(41.8858232817599,-0.130233482639502,
-11.0964080852364));
#65574=CARTESIAN_POINT('Ctrl Pts',(41.9322444554138,-0.136566102789513,
-11.0110588443129));
#65575=CARTESIAN_POINT('Ctrl Pts',(41.9786031535875,-0.142890200244962,
-10.9258244698262));
#65576=CARTESIAN_POINT('Ctrl Pts',(42.0210345904329,-0.149214297700411,
-10.8382993024448));
#65577=CARTESIAN_POINT('Ctrl Pts',(42.0593087076327,-0.155538395155859,
-10.7488808632199));
#65578=CARTESIAN_POINT('Ctrl Pts',(42.0975427632596,-0.161855873169507,
-10.6595560184025));
#65579=CARTESIAN_POINT('Ctrl Pts',(42.1316279789981,-0.168173351183154,
-10.5683422413577));
#65580=CARTESIAN_POINT('Ctrl Pts',(42.1613804173148,-0.174490829196802,
-10.4756611787828));
#65581=CARTESIAN_POINT('Ctrl Pts',(42.1911117363711,-0.180803822856548,
-10.3830459042777));
#65582=CARTESIAN_POINT('Ctrl Pts',(42.2165162590907,-0.187116816516293,
-10.2889658300647));
#65583=CARTESIAN_POINT('Ctrl Pts',(42.2374587006585,-0.193429810176038,
-10.1938611923964));
#65584=CARTESIAN_POINT('Ctrl Pts',(42.2583935742588,-0.199740522510024,
-10.0987909226795));
#65585=CARTESIAN_POINT('Ctrl Pts',(42.2748694767364,-0.20605123484401,-10.0026972518387));
#65586=CARTESIAN_POINT('Ctrl Pts',(42.286801635077,-0.212361947177996,-9.90603322504187));
#65587=CARTESIAN_POINT('Ctrl Pts',(42.2987327133358,-0.218672088275344,
-9.80937794813424));
#65588=CARTESIAN_POINT('Ctrl Pts',(42.3061208118354,-0.224982229372693,
-9.71215285196113));
#65589=CARTESIAN_POINT('Ctrl Pts',(42.30893284416,-0.231292370470041,-9.61481772321296));
#65590=CARTESIAN_POINT('Ctrl Pts',(42.3117453835745,-0.237603649466402,
-9.51746504215571));
#65591=CARTESIAN_POINT('Ctrl Pts',(42.3099802052781,-0.243914928462761,
-9.42000272624048));
#65592=CARTESIAN_POINT('Ctrl Pts',(42.303656337438,-0.250226207459121,-9.3228911382925));
#65593=CARTESIAN_POINT('Ctrl Pts',(42.2973257066449,-0.256544235945681,
-9.22567569600509));
#65594=CARTESIAN_POINT('Ctrl Pts',(42.2864266816765,-0.26286226443224,-9.12881216761935));
#65595=CARTESIAN_POINT('Ctrl Pts',(42.271030227304,-0.2691802929188,-9.0327561621666));
#65596=CARTESIAN_POINT('Ctrl Pts',(42.2556247511067,-0.275502023565946,
-8.93664387099778));
#65597=CARTESIAN_POINT('Ctrl Pts',(42.2357166871887,-0.281823754213095,
-8.84134047288126));
#65598=CARTESIAN_POINT('Ctrl Pts',(42.2114277878788,-0.288145484860242,
-8.74728968677825));
#65599=CARTESIAN_POINT('Ctrl Pts',(42.1870999430878,-0.294477351942071,
-8.65308809708942));
#65600=CARTESIAN_POINT('Ctrl Pts',(42.1583773655456,-0.3008092190239,-8.56014354753402));
#65601=CARTESIAN_POINT('Ctrl Pts',(42.1254311381782,-0.307141086105729,
-8.46888290957993));
#65602=CARTESIAN_POINT('Ctrl Pts',(42.1062954273358,-0.310818738670307,
-8.41587722975762));
#65603=CARTESIAN_POINT('Ctrl Pts',(42.0857357750569,-0.314496391234885,
-8.36343922708463));
#65604=CARTESIAN_POINT('Ctrl Pts',(42.0637928565438,-0.318174043799464,
-8.3116488028156));
#65605=CARTESIAN_POINT('Ctrl Pts',(42.0260089263125,-0.324506663948962,
-8.2224698826979));
#65606=CARTESIAN_POINT('Ctrl Pts',(41.983989833842,-0.330839284098463,-8.13490263785141));
#65607=CARTESIAN_POINT('Ctrl Pts',(41.9378946495576,-0.337171904247962,
-8.0493768974349));
#65608=CARTESIAN_POINT('Ctrl Pts',(41.8918615020238,-0.343496001702896,
-7.96396626099521));
#65609=CARTESIAN_POINT('Ctrl Pts',(41.8417633716234,-0.34982009915783,-7.88059204983426));
#65610=CARTESIAN_POINT('Ctrl Pts',(41.7878073809052,-0.356144196612765,
-7.7996642030513));
#65611=CARTESIAN_POINT('Ctrl Pts',(41.7339078659995,-0.362461674625868,
-7.71882106356106));
#65612=CARTESIAN_POINT('Ctrl Pts',(41.6761587598858,-0.36877915263897,-7.64041955977328));
#65613=CARTESIAN_POINT('Ctrl Pts',(41.6148125979747,-0.375096630652074,
-7.56484419763051));
#65614=CARTESIAN_POINT('Ctrl Pts',(41.5535099815891,-0.381409624311284,
-7.48932248136806));
#65615=CARTESIAN_POINT('Ctrl Pts',(41.4886156603618,-0.387722617970494,
-7.41662325709803));
#65616=CARTESIAN_POINT('Ctrl Pts',(41.4204243307487,-0.394035611629704,
-7.34710045127899));
#65617=CARTESIAN_POINT('Ctrl Pts',(41.3522576434282,-0.400346323963149,
-7.277602768908));
#65618=CARTESIAN_POINT('Ctrl Pts',(41.2807966210374,-0.406657036296594,
-7.21127953605949));
#65619=CARTESIAN_POINT('Ctrl Pts',(41.206374296686,-0.412967748630038,-7.14844938313994));
#65620=CARTESIAN_POINT('Ctrl Pts',(41.1319587089367,-0.419277889726845,
-7.0856249175158));
#65621=CARTESIAN_POINT('Ctrl Pts',(41.0545826864648,-0.425588030823653,
-7.02629318510998));
#65622=CARTESIAN_POINT('Ctrl Pts',(40.974613160478,-0.43189817192046,-6.97073321997129));
#65623=CARTESIAN_POINT('Ctrl Pts',(40.8946292136973,-0.438209450916274,
-6.91516323578102));
#65624=CARTESIAN_POINT('Ctrl Pts',(40.8120511936819,-0.444520729912088,
-6.86336661922318));
#65625=CARTESIAN_POINT('Ctrl Pts',(40.7272750009004,-0.450832008907901,
-6.81557907948492));
#65626=CARTESIAN_POINT('Ctrl Pts',(40.6424081456583,-0.457150037393917,
-6.76774043417337));
#65627=CARTESIAN_POINT('Ctrl Pts',(40.5553388059945,-0.463468065879932,
-6.72391964041467));
#65628=CARTESIAN_POINT('Ctrl Pts',(40.466487291168,-0.469786094365948,-6.68430631813108));
#65629=CARTESIAN_POINT('Ctrl Pts',(40.3775837122242,-0.476107825012546,
-6.64466978372038));
#65630=CARTESIAN_POINT('Ctrl Pts',(40.2868962857968,-0.482429555659144,
-6.60924578919691));
#65631=CARTESIAN_POINT('Ctrl Pts',(40.194863126059,-0.488751286305741,-6.57817492658485));
#65632=CARTESIAN_POINT('Ctrl Pts',(40.1026823978522,-0.495083153387022,
-6.54705424410747));
#65633=CARTESIAN_POINT('Ctrl Pts',(40.0091520478015,-0.501415020468303,
-6.52030075142709));
#65634=CARTESIAN_POINT('Ctrl Pts',(39.9147230473378,-0.507746887549584,
-6.49800452288013));
#65635=CARTESIAN_POINT('Ctrl Pts',(39.8598771303633,-0.511424540119536,
-6.48505450653212));
#65636=CARTESIAN_POINT('Ctrl Pts',(39.8047282224243,-0.515102192689488,
-6.4736071754637));
#65637=CARTESIAN_POINT('Ctrl Pts',(39.7493654651879,-0.51877984525944,-6.46367214454922));
#65638=CARTESIAN_POINT('Ctrl Pts',(39.6540352768832,-0.525112465409043,
-6.44656482520372));
#65639=CARTESIAN_POINT('Ctrl Pts',(39.557739655896,-0.531445085558645,-6.43388492453164));
#65640=CARTESIAN_POINT('Ctrl Pts',(39.460925484113,-0.537777705708248,-6.42573419264491));
#65641=CARTESIAN_POINT('Ctrl Pts',(39.3642416087312,-0.544101803163289,
-6.41759443034054));
#65642=CARTESIAN_POINT('Ctrl Pts',(39.2670410017269,-0.550425900618329,
-6.41397175803448));
#65643=CARTESIAN_POINT('Ctrl Pts',(39.169780155618,-0.556749998073369,-6.41491681559713));
#65644=CARTESIAN_POINT('Ctrl Pts',(39.0726211125755,-0.56306747608658,-6.41586088396667));
#65645=CARTESIAN_POINT('Ctrl Pts',(38.9754023907747,-0.569384954099792,
-6.42136317302188));
#65646=CARTESIAN_POINT('Ctrl Pts',(38.8785840090073,-0.575702432113004,
-6.43142239249859));
#65647=CARTESIAN_POINT('Ctrl Pts',(38.781834352115,-0.582015425772317,-6.44147447161011));
#65648=CARTESIAN_POINT('Ctrl Pts',(38.6854849040381,-0.588328419431632,
-6.45607700538267));
#65649=CARTESIAN_POINT('Ctrl Pts',(38.5899931228984,-0.594641413090945,
-6.47517668334889));
#65650=CARTESIAN_POINT('Ctrl Pts',(38.4945358496122,-0.600952125424498,
-6.49426945926678));
#65651=CARTESIAN_POINT('Ctrl Pts',(38.3999360558037,-0.607262837758047,
-6.5178560645398));
#65652=CARTESIAN_POINT('Ctrl Pts',(38.3066425988733,-0.6135735500916,-6.54583179280656));
#65653=CARTESIAN_POINT('Ctrl Pts',(38.2133575867334,-0.619883691188486,
-6.57380498875036));
#65654=CARTESIAN_POINT('Ctrl Pts',(38.1213790951914,-0.626193832285376,
-6.60616639196017));
#65655=CARTESIAN_POINT('Ctrl Pts',(38.0311413537314,-0.632503973382262,
-6.6427612663169));
#65656=CARTESIAN_POINT('Ctrl Pts',(37.9408873398241,-0.638815252378183,
-6.67936273977682));
#65657=CARTESIAN_POINT('Ctrl Pts',(37.8523751046955,-0.645126531374105,
-6.7201990362465));
#65658=CARTESIAN_POINT('Ctrl Pts',(37.766018433538,-0.651437810370027,-6.76506747909534));
#65659=CARTESIAN_POINT('Ctrl Pts',(37.6795694097043,-0.657755838856146,
-6.8099839057388));
#65660=CARTESIAN_POINT('Ctrl Pts',(37.5952809408086,-0.664073867342263,
-6.85894088569714));
#65661=CARTESIAN_POINT('Ctrl Pts',(37.5135415600515,-0.670391895828382,
-6.91169010960686));
#65662=CARTESIAN_POINT('Ctrl Pts',(37.4317542826579,-0.676713626475093,
-6.96447024285776));
#65663=CARTESIAN_POINT('Ctrl Pts',(37.3525194234754,-0.683035357121804,
-7.02104679092049));
#65664=CARTESIAN_POINT('Ctrl Pts',(37.2761941931527,-0.689357087768515,
-7.08112973534995));
#65665=CARTESIAN_POINT('Ctrl Pts',(37.1997465808821,-0.695688954849898,
-7.14130901840487));
#65666=CARTESIAN_POINT('Ctrl Pts',(37.1262182437386,-0.702020821931283,
-7.20500563831858));
#65667=CARTESIAN_POINT('Ctrl Pts',(37.0559311178139,-0.708352689012665,
-7.27189119629315));
#65668=CARTESIAN_POINT('Ctrl Pts',(37.0151071987555,-0.712030341581586,
-7.31073942872559));
#65669=CARTESIAN_POINT('Ctrl Pts',(36.9753759799599,-0.715707994150504,
-7.35066277636454));
#65670=CARTESIAN_POINT('Ctrl Pts',(36.9367942392651,-0.719385646719425,
-7.39159184929921));
#65671=CARTESIAN_POINT('Ctrl Pts',(36.8700091971459,-0.725751667984734,
-7.46244012650557));
#65672=CARTESIAN_POINT('Ctrl Pts',(36.8064215504707,-0.732117689250043,
-7.53656840224095));
#65673=CARTESIAN_POINT('Ctrl Pts',(36.7463748568544,-0.738483710515352,
-7.61365118049482));
#65674=CARTESIAN_POINT('Ctrl Pts',(36.6874698523395,-0.744728692358501,
-7.68926835652253));
#65675=CARTESIAN_POINT('Ctrl Pts',(36.6319726606026,-0.750973674201652,
-7.76772832768793));
#65676=CARTESIAN_POINT('Ctrl Pts',(36.5801714436936,-0.757218656044802,
-7.84868589206516));
#65677=CARTESIAN_POINT('Ctrl Pts',(36.5284184462394,-0.76345782471139,-7.92956809663711));
#65678=CARTESIAN_POINT('Ctrl Pts',(36.4803548329806,-0.769696993377978,
-8.01294290208393));
#65679=CARTESIAN_POINT('Ctrl Pts',(36.4362275009105,-0.775936162044567,
-8.09843341333937));
#65680=CARTESIAN_POINT('Ctrl Pts',(36.3921285670166,-0.782171315489688,
-8.18386890711501));
#65681=CARTESIAN_POINT('Ctrl Pts',(36.3519610877662,-0.788406468934808,
-8.27141700411107));
#65682=CARTESIAN_POINT('Ctrl Pts',(36.3159271122552,-0.794641622379929,
-8.36067434492102));
#65683=CARTESIAN_POINT('Ctrl Pts',(36.2785896012964,-0.801102333605506,
-8.45316058584701));
#65684=CARTESIAN_POINT('Ctrl Pts',(36.2456905899654,-0.807563044831082,
-8.54748164869504));
#65685=CARTESIAN_POINT('Ctrl Pts',(36.2174009197196,-0.814023756056659,
-8.64316476640455));
#65686=CARTESIAN_POINT('Ctrl Pts',(36.1901025329634,-0.820258080890536,
-8.73549510219756));
#65687=CARTESIAN_POINT('Ctrl Pts',(36.1670959464817,-0.826492405724413,
-8.82909316493853));
#65688=CARTESIAN_POINT('Ctrl Pts',(36.1484837600194,-0.83272673055829,-8.92351908589345));
#65689=CARTESIAN_POINT('Ctrl Pts',(36.1298684664969,-0.838962096130854,
-9.01796077001624));
#65690=CARTESIAN_POINT('Ctrl Pts',(36.1156491071054,-0.845197461703417,
-9.1132301443313));
#65691=CARTESIAN_POINT('Ctrl Pts',(36.1058768389215,-0.851432827275981,
-9.20887895201744));
#65692=CARTESIAN_POINT('Ctrl Pts',(36.0960970467662,-0.857672993649282,
-9.30460140267786));
#65693=CARTESIAN_POINT('Ctrl Pts',(36.0907712056005,-0.863913160022584,
-9.40070342170071));
#65694=CARTESIAN_POINT('Ctrl Pts',(36.089898442095,-0.870153326395885,-9.49673425364528));
#65695=CARTESIAN_POINT('Ctrl Pts',(36.0898044159576,-0.870825603292871,
-9.50708002102593));
#65696=CARTESIAN_POINT('Ctrl Pts',(36.0897620250169,-0.871497880189858,
-9.51742496460401));
#65697=CARTESIAN_POINT('Ctrl Pts',(36.0897712321793,-0.872170157086845,
-9.5277685231493));
#65698=CARTESIAN_POINT('',(36.0897704137311,-2.14217015708684,-9.52339575640588));
#65699=CARTESIAN_POINT('Ctrl Pts',(36.0899125803325,-0.872170241694712,
-9.5277696990371));
#65700=CARTESIAN_POINT('Ctrl Pts',(36.0877068998987,-0.888110643856278,
-9.77301751196299));
#65701=CARTESIAN_POINT('Ctrl Pts',(36.2258738429507,-0.970919646504489,
-11.0446027236326));
#65702=CARTESIAN_POINT('Ctrl Pts',(37.9701641530118,-1.12059724963941,-12.9826522251454));
#65703=CARTESIAN_POINT('Ctrl Pts',(41.4231224819371,-1.32120305109937,-12.4448598512402));
#65704=CARTESIAN_POINT('Ctrl Pts',(42.8602373914268,-1.52180885255935,-9.25944895221449));
#65705=CARTESIAN_POINT('Ctrl Pts',(40.9783874130057,-1.72241465401934,-6.31482970391815));
#65706=CARTESIAN_POINT('Ctrl Pts',(37.483962962039,-1.92302045547933,-6.28107151667509));
#65707=CARTESIAN_POINT('Ctrl Pts',(36.1319771607599,-2.06293895650182,-8.30914305999039));
#65708=CARTESIAN_POINT('Ctrl Pts',(36.0852272677007,-2.13598885703766,-9.42861603492319));
#65709=CARTESIAN_POINT('Ctrl Pts',(36.0858265164569,-2.14217015708684,-9.52339372215993));
#65710=CARTESIAN_POINT('',(36.0897702438652,-3.41217015705251,-9.52376835315985));
#65711=CARTESIAN_POINT('Ctrl Pts',(36.0897704137311,-2.14217015708684,-9.52339575640588));
#65712=CARTESIAN_POINT('Ctrl Pts',(36.0897210100065,-2.14842487072775,-9.61917729887397));
#65713=CARTESIAN_POINT('Ctrl Pts',(36.0941003085369,-2.15467958436866,-9.7151342087082));
#65714=CARTESIAN_POINT('Ctrl Pts',(36.1029305733703,-2.16093429800956,-9.81081745841623));
#65715=CARTESIAN_POINT('Ctrl Pts',(36.1117498912511,-2.16718125763004,-9.90638208880517));
#65716=CARTESIAN_POINT('Ctrl Pts',(36.1250091728486,-2.17342821725052,-10.0016732896905));
#65717=CARTESIAN_POINT('Ctrl Pts',(36.1426786579585,-2.17967517687099,-10.0962415114449));
#65718=CARTESIAN_POINT('Ctrl Pts',(36.1603314513654,-2.18591623522185,-10.1907203981295));
#65719=CARTESIAN_POINT('Ctrl Pts',(36.1823860860398,-2.19215729357271,-10.2844772239474));
#65720=CARTESIAN_POINT('Ctrl Pts',(36.2087610630663,-2.19839835192357,-10.377068233812));
#65721=CARTESIAN_POINT('Ctrl Pts',(36.235122762356,-2.20463626838999,-10.4696126313497));
#65722=CARTESIAN_POINT('Ctrl Pts',(36.2658003628854,-2.21087418485642,-10.5609919475004));
#65723=CARTESIAN_POINT('Ctrl Pts',(36.3006616346398,-2.21711210132285,-10.6507742651395));
#65724=CARTESIAN_POINT('Ctrl Pts',(36.3355153493107,-2.22334866555934,-10.7405371201361));
#65725=CARTESIAN_POINT('Ctrl Pts',(36.374550771124,-2.22958522979582,-10.8287032461613));
#65726=CARTESIAN_POINT('Ctrl Pts',(36.4175867298321,-2.2358217940323,-10.9148586427739));
#65727=CARTESIAN_POINT('Ctrl Pts',(36.4606256955022,-2.24205879402327,-11.0010200591434));
#65728=CARTESIAN_POINT('Ctrl Pts',(36.5076655512623,-2.24829579401424,-11.0851700662614));
#65729=CARTESIAN_POINT('Ctrl Pts',(36.5584787228057,-2.2545327940052,-11.166918388663));
#65730=CARTESIAN_POINT('Ctrl Pts',(36.6093418550827,-2.26077592636473,-11.2487470879834));
#65731=CARTESIAN_POINT('Ctrl Pts',(36.6639854731947,-2.26701905872425,-11.3281690059682));
#65732=CARTESIAN_POINT('Ctrl Pts',(36.7221383179323,-2.27326219108377,-11.4048223685872));
#65733=CARTESIAN_POINT('Ctrl Pts',(36.7803211527836,-2.27950854310091,-11.481515262257));
#65734=CARTESIAN_POINT('Ctrl Pts',(36.8420165285394,-2.28575489511805,-11.5554364144923));
#65735=CARTESIAN_POINT('Ctrl Pts',(36.906913942458,-2.29200124713519,-11.6262584290388));
#65736=CARTESIAN_POINT('Ctrl Pts',(36.9719170676987,-2.29825777382787,-11.6971958054824));
#65737=CARTESIAN_POINT('Ctrl Pts',(37.0401323275585,-2.30451430052054,-11.7650236480001));
#65738=CARTESIAN_POINT('Ctrl Pts',(37.1112136356493,-2.31077082721321,-11.829452684913));
#65739=CARTESIAN_POINT('Ctrl Pts',(37.1621919695941,-2.31525790427523,-11.8756601204217));
#65740=CARTESIAN_POINT('Ctrl Pts',(37.2146437318066,-2.31974498133725,-11.9201201988837));
#65741=CARTESIAN_POINT('Ctrl Pts',(37.2684320627391,-2.32423205839928,-11.9627399280164));
#65742=CARTESIAN_POINT('Ctrl Pts',(37.3443436335834,-2.3305646785489,-12.0228892305014));
#65743=CARTESIAN_POINT('Ctrl Pts',(37.4231993222627,-2.33689729869852,-12.0795937882138));
#65744=CARTESIAN_POINT('Ctrl Pts',(37.5046534682714,-2.34322991884815,-12.132552643813));
#65745=CARTESIAN_POINT('Ctrl Pts',(37.5859979900185,-2.3495540163032,-12.1854402252569));
#65746=CARTESIAN_POINT('Ctrl Pts',(37.6699336548913,-2.35587811375825,-12.2345918876808));
#65747=CARTESIAN_POINT('Ctrl Pts',(37.7560821674047,-2.3622022112133,-12.2797471654606));
#65748=CARTESIAN_POINT('Ctrl Pts',(37.8421405081474,-2.36851968922653,-12.3248551791469));
#65749=CARTESIAN_POINT('Ctrl Pts',(37.9304067065361,-2.37483716723977,-12.3659749222822));
#65750=CARTESIAN_POINT('Ctrl Pts',(38.0204748056826,-2.38115464525301,-12.4028900202875));
#65751=CARTESIAN_POINT('Ctrl Pts',(38.110478971527,-2.38746763891236,-12.439778914741));
#65752=CARTESIAN_POINT('Ctrl Pts',(38.202282091807,-2.3937806325717,-12.4724689322425));
#65753=CARTESIAN_POINT('Ctrl Pts',(38.295455869171,-2.40009362623105,-12.5007907467231));
#65754=CARTESIAN_POINT('Ctrl Pts',(38.3885959763382,-2.40640433856464,-12.529102326553));
#65755=CARTESIAN_POINT('Ctrl Pts',(38.4831053384089,-2.41271505089823,-12.5530487128777));
#65756=CARTESIAN_POINT('Ctrl Pts',(38.5785389349689,-2.41902576323182,-12.5725099339544));
#65757=CARTESIAN_POINT('Ctrl Pts',(38.6739638930162,-2.42533590432875,-12.5919693934291));
#65758=CARTESIAN_POINT('Ctrl Pts',(38.7703124906826,-2.43164604542568,-12.6069444076832));
#65759=CARTESIAN_POINT('Ctrl Pts',(38.8671289413233,-2.43795618652261,-12.6173660053744));
#65760=CARTESIAN_POINT('Ctrl Pts',(38.9639628507405,-2.44426746551855,-12.627789482378));
#65761=CARTESIAN_POINT('Ctrl Pts',(39.0612643458969,-2.4505787445145,-12.6336578652206));
#65762=CARTESIAN_POINT('Ctrl Pts',(39.1585729868944,-2.45689002351044,-12.6349540921829));
#65763=CARTESIAN_POINT('Ctrl Pts',(39.2559856929666,-2.46320805199659,-12.6362517053732));
#65764=CARTESIAN_POINT('Ctrl Pts',(39.3534051221422,-2.46952608048274,-12.6329673950012));
#65765=CARTESIAN_POINT('Ctrl Pts',(39.4503715087784,-2.4758441089689,-12.6251362486981));
#65766=CARTESIAN_POINT('Ctrl Pts',(39.5473947145845,-2.48216583961563,-12.6173005135963));
#65767=CARTESIAN_POINT('Ctrl Pts',(39.6439639156643,-2.48848757026237,-12.6049126928345));
#65768=CARTESIAN_POINT('Ctrl Pts',(39.7396272249482,-2.4948093009091,-12.5880594364123));
#65769=CARTESIAN_POINT('Ctrl Pts',(39.8354439233815,-2.50114116799052,-12.5711791570209));
#65770=CARTESIAN_POINT('Ctrl Pts',(39.9303514031963,-2.50747303507194,-12.5498192406631));
#65771=CARTESIAN_POINT('Ctrl Pts',(40.0239107121449,-2.51380490215336,-12.5241168352221));
#65772=CARTESIAN_POINT('Ctrl Pts',(40.078251497959,-2.51748255472199,-12.5091884553028));
#65773=CARTESIAN_POINT('Ctrl Pts',(40.1321377965864,-2.52116020729063,-12.4927960712961));
#65774=CARTESIAN_POINT('Ctrl Pts',(40.1854867683263,-2.52483785985926,-12.4749739799452));
#65775=CARTESIAN_POINT('Ctrl Pts',(40.2773493809841,-2.53117048000889,-12.4442857806955));
#65776=CARTESIAN_POINT('Ctrl Pts',(40.3679367385615,-2.53750310015852,-12.4092492690312));
#65777=CARTESIAN_POINT('Ctrl Pts',(40.4568078803832,-2.54383572030815,-12.3699893856932));
#65778=CARTESIAN_POINT('Ctrl Pts',(40.5455594158526,-2.55015981776323,-12.3307823398831));
#65779=CARTESIAN_POINT('Ctrl Pts',(40.6325989296655,-2.5564839152183,-12.2873633948018));
#65780=CARTESIAN_POINT('Ctrl Pts',(40.7175015292641,-2.56280801267338,-12.2399069526562));
#65781=CARTESIAN_POINT('Ctrl Pts',(40.8023152611905,-2.56912549068661,-12.1925001832364));
#65782=CARTESIAN_POINT('Ctrl Pts',(40.8849961458686,-2.57544296869985,-12.141064530598));
#65783=CARTESIAN_POINT('Ctrl Pts',(40.9651410915204,-2.58176044671308,-12.0858216610936));
#65784=CARTESIAN_POINT('Ctrl Pts',(41.0452291476511,-2.58807344037242,-12.0306180047969));
#65785=CARTESIAN_POINT('Ctrl Pts',(41.1227844844056,-2.59438643403177,-11.971612751825));
#65786=CARTESIAN_POINT('Ctrl Pts',(41.197431195838,-2.60069942769111,-11.9090719936263));
#65787=CARTESIAN_POINT('Ctrl Pts',(41.2720509321971,-2.60701014002469,-11.8465538357739));
#65788=CARTESIAN_POINT('Ctrl Pts',(41.3437637968885,-2.61332085235827,-11.7805029919129));
#65789=CARTESIAN_POINT('Ctrl Pts',(41.4122260712237,-2.61963156469185,-11.7112265350824));
#65790=CARTESIAN_POINT('Ctrl Pts',(41.4806821484518,-2.62594170578879,-11.6419563490574));
#65791=CARTESIAN_POINT('Ctrl Pts',(41.5458879130941,-2.63225184688573,-11.5694614417768));
#65792=CARTESIAN_POINT('Ctrl Pts',(41.6075364682288,-2.63856198798267,-11.4940857795049));
#65793=CARTESIAN_POINT('Ctrl Pts',(41.6691961403618,-2.64487326697859,-11.4186965248445));
#65794=CARTESIAN_POINT('Ctrl Pts',(41.7272970521219,-2.65118454597451,-11.3404258219638));
#65795=CARTESIAN_POINT('Ctrl Pts',(41.781573231189,-2.65749582497043,-11.2596499084565));
#65796=CARTESIAN_POINT('Ctrl Pts',(41.8359074549949,-2.66381385345658,-11.1787876105192));
#65797=CARTESIAN_POINT('Ctrl Pts',(41.8864085357551,-2.67013188194273,-11.0954151167484));
#65798=CARTESIAN_POINT('Ctrl Pts',(41.9328545386116,-2.67644991042888,-11.0099366059498));
#65799=CARTESIAN_POINT('Ctrl Pts',(41.9793277573254,-2.68277164107561,-10.9244080075054));
#65800=CARTESIAN_POINT('Ctrl Pts',(42.0217409761598,-2.68909337172234,-10.8367713281497));
#65801=CARTESIAN_POINT('Ctrl Pts',(42.0599197442076,-2.69541510236907,-10.7474523342821));
#65802=CARTESIAN_POINT('Ctrl Pts',(42.0981597291293,-2.70174696945048,-10.6579901239129));
#65803=CARTESIAN_POINT('Ctrl Pts',(42.1321515528492,-2.70807883653189,-10.5668406221492));
#65804=CARTESIAN_POINT('Ctrl Pts',(42.1617701208713,-2.7144107036133,-10.4744463671076));
#65805=CARTESIAN_POINT('Ctrl Pts',(42.178973072444,-2.71808835618195,-10.4207822637692));
#65806=CARTESIAN_POINT('Ctrl Pts',(42.194701662792,-2.72176600875059,-10.3666984872842));
#65807=CARTESIAN_POINT('Ctrl Pts',(42.2089393296271,-2.72544366131924,-10.3122831533337));
#65808=CARTESIAN_POINT('Ctrl Pts',(42.2334554398906,-2.73177628146887,-10.2185843512333));
#65809=CARTESIAN_POINT('Ctrl Pts',(42.2536332752531,-2.7381089016185,-10.123576554382));
#65810=CARTESIAN_POINT('Ctrl Pts',(42.2693364213388,-2.74444152176813,-10.0276973100617));
#65811=CARTESIAN_POINT('Ctrl Pts',(42.2850184334997,-2.7507656192232,-9.93194710387979));
#65812=CARTESIAN_POINT('Ctrl Pts',(42.2962376557355,-2.75708971667826,-9.83532820920002));
#65813=CARTESIAN_POINT('Ctrl Pts',(42.3029078749237,-2.76341381413333,-9.73829175473226));
#65814=CARTESIAN_POINT('Ctrl Pts',(42.3095711123839,-2.76973129214659,-9.64135686845946));
#65815=CARTESIAN_POINT('Ctrl Pts',(42.3116947829521,-2.77604877015985,-9.54400572528747));
#65816=CARTESIAN_POINT('Ctrl Pts',(42.3092441683453,-2.78236624817311,-9.4466970338322));
#65817=CARTESIAN_POINT('Ctrl Pts',(42.3067952932655,-2.78867924183245,-9.34945741529036));
#65818=CARTESIAN_POINT('Ctrl Pts',(42.2997785991763,-2.79499223549179,-9.25226062449232));
#65819=CARTESIAN_POINT('Ctrl Pts',(42.2882114288376,-2.80130522915113,-9.15556688873823));
#65820=CARTESIAN_POINT('Ctrl Pts',(42.2766484385259,-2.80761594148472,-9.05890809518778));
#65821=CARTESIAN_POINT('Ctrl Pts',(42.2605382913067,-2.8139266538183,-8.96275242924147));
#65822=CARTESIAN_POINT('Ctrl Pts',(42.2399502413291,-2.82023736615188,-8.86755556649762));
#65823=CARTESIAN_POINT('Ctrl Pts',(42.2193640549523,-2.82654750724881,-8.7723673208376));
#65824=CARTESIAN_POINT('Ctrl Pts',(42.1943008643566,-2.83285764834574,-8.67813813320795));
#65825=CARTESIAN_POINT('Ctrl Pts',(42.1648809448693,-2.83916778944267,-8.58531301187511));
#65826=CARTESIAN_POINT('Ctrl Pts',(42.1354557201285,-2.84547906843863,-8.49247115151641));
#65827=CARTESIAN_POINT('Ctrl Pts',(42.1016723382666,-2.85179034743458,-8.40103427718842));
#65828=CARTESIAN_POINT('Ctrl Pts',(42.0637004681861,-2.85810162643054,-8.31143076777195));
#65829=CARTESIAN_POINT('Ctrl Pts',(42.0256879897337,-2.86441965491668,-8.22173143340328));
#65830=CARTESIAN_POINT('Ctrl Pts',(41.9834782512849,-2.87073768340283,-8.13386978161148));
#65831=CARTESIAN_POINT('Ctrl Pts',(41.9372883909053,-2.87705571188898,-8.04825258831602));
#65832=CARTESIAN_POINT('Ctrl Pts',(41.8910714647597,-2.8833774425357,-7.96258522611139));
#65833=CARTESIAN_POINT('Ctrl Pts',(41.8408699979806,-2.88969917318242,-7.87916531581658));
#65834=CARTESIAN_POINT('Ctrl Pts',(41.78694516131,-2.89602090382914,-7.79837167135629));
#65835=CARTESIAN_POINT('Ctrl Pts',(41.732933860091,-2.90235277091055,-7.71744848017113));
#65836=CARTESIAN_POINT('Ctrl Pts',(41.675187527059,-2.90868463799196,-7.63916031521021));
#65837=CARTESIAN_POINT('Ctrl Pts',(41.6140083564293,-2.91501650507338,-7.56385382798998));
#65838=CARTESIAN_POINT('Ctrl Pts',(41.5784744876479,-2.91869415764199,-7.52011458131945));
#65839=CARTESIAN_POINT('Ctrl Pts',(41.5417832786228,-2.92237181021061,-7.47738053618639));
#65840=CARTESIAN_POINT('Ctrl Pts',(41.5039994625352,-2.92604946277923,-7.43571372724143));
#65841=CARTESIAN_POINT('Ctrl Pts',(41.4389387884715,-2.93238208292886,-7.36396685366578));
#65842=CARTESIAN_POINT('Ctrl Pts',(41.3704106033539,-2.93871470307849,-7.2951372499552));
#65843=CARTESIAN_POINT('Ctrl Pts',(41.2987067345049,-2.94504732322812,-7.22957831859948));
#65844=CARTESIAN_POINT('Ctrl Pts',(41.2270993676031,-2.95137142068317,-7.16410761908714));
#65845=CARTESIAN_POINT('Ctrl Pts',(41.1523251316917,-2.95769551813822,-7.10189913573855));
#65846=CARTESIAN_POINT('Ctrl Pts',(41.0747146678837,-2.96401961559327,-7.04327165730782));
#65847=CARTESIAN_POINT('Ctrl Pts',(40.9971854390586,-2.97033709360651,-6.9847055443422));
#65848=CARTESIAN_POINT('Ctrl Pts',(40.9168262313329,-2.97665457161975,-6.92971324681606));
#65849=CARTESIAN_POINT('Ctrl Pts',(40.8340021811452,-2.98297204963299,-6.87857457597748));
#65850=CARTESIAN_POINT('Ctrl Pts',(40.7512369221952,-2.98928504329234,-6.82747220505116));
#65851=CARTESIAN_POINT('Ctrl Pts',(40.6660106701898,-2.99559803695169,-6.78021825170862));
#65852=CARTESIAN_POINT('Ctrl Pts',(40.5787182908357,-3.00191103061104,-6.73704976238542));
#65853=CARTESIAN_POINT('Ctrl Pts',(40.4914574563183,-3.00822174294462,-6.69389687285405));
#65854=CARTESIAN_POINT('Ctrl Pts',(40.4021323696278,-3.01453245527821,-6.65482670744933));
#65855=CARTESIAN_POINT('Ctrl Pts',(40.311162460707,-3.02084316761179,-6.62003035492356));
#65856=CARTESIAN_POINT('Ctrl Pts',(40.2202007862522,-3.02715330870873,-6.58523715211385));
#65857=CARTESIAN_POINT('Ctrl Pts',(40.1275949941139,-3.03346344980566,-6.55471714905668));
#65858=CARTESIAN_POINT('Ctrl Pts',(40.0337834707486,-3.03977359090259,-6.52861287934847));
#65859=CARTESIAN_POINT('Ctrl Pts',(39.9399550304815,-3.04608486989852,-6.50250390229351));
#65860=CARTESIAN_POINT('Ctrl Pts',(39.8449208484584,-3.05239614889445,-6.48081235730437));
#65861=CARTESIAN_POINT('Ctrl Pts',(39.749132385458,-3.05870742789038,-6.46363032677509));
#65862=CARTESIAN_POINT('Ctrl Pts',(39.6532414831113,-3.06502545637653,-6.44642992121483));
#65863=CARTESIAN_POINT('Ctrl Pts',(39.5565951205009,-3.07134348486269,-6.43374873555632));
#65864=CARTESIAN_POINT('Ctrl Pts',(39.4596526160273,-3.07766151334884,-6.42562729380763));
#65865=CARTESIAN_POINT('Ctrl Pts',(39.3626533063777,-3.08398324399558,-6.41750109315645));
#65866=CARTESIAN_POINT('Ctrl Pts',(39.2653579461476,-3.09030497464232,-6.41393997281143));
#65867=CARTESIAN_POINT('Ctrl Pts',(39.1682265079734,-3.09662670528906,-6.41493230007699));
#65868=CARTESIAN_POINT('Ctrl Pts',(39.0709393266122,-3.10295857237048,-6.41592621846704));
#65869=CARTESIAN_POINT('Ctrl Pts',(38.9738170284686,-3.10929043945189,-6.42148813853957));
#65870=CARTESIAN_POINT('Ctrl Pts',(38.8773150781794,-3.1156223065333,-6.43155449472119));
#65871=CARTESIAN_POINT('Ctrl Pts',(38.8212651578643,-3.11929995910194,-6.43740119999661));
#65872=CARTESIAN_POINT('Ctrl Pts',(38.7654243506651,-3.12297761167057,-6.44476650274189));
#65873=CARTESIAN_POINT('Ctrl Pts',(38.709879987631,-3.12665526423921,-6.45363010590137));
#65874=CARTESIAN_POINT('Ctrl Pts',(38.6142370888026,-3.13298788438884,-6.46889251335247));
#65875=CARTESIAN_POINT('Ctrl Pts',(38.5191416506987,-3.13932050453847,-6.4886531852611));
#65876=CARTESIAN_POINT('Ctrl Pts',(38.4250491243567,-3.1456531246881,-6.51286092730768));
#65877=CARTESIAN_POINT('Ctrl Pts',(38.3310832315159,-3.15197722214318,-6.53703608960273));
#65878=CARTESIAN_POINT('Ctrl Pts',(38.2381179876727,-3.15830131959827,-6.56564631843693));
#65879=CARTESIAN_POINT('Ctrl Pts',(38.1466010753143,-3.16462541705335,-6.59858899701855));
#65880=CARTESIAN_POINT('Ctrl Pts',(38.0551799538386,-3.17094289506661,-6.63149719445149));
#65881=CARTESIAN_POINT('Ctrl Pts',(37.9652045593308,-3.17726037307986,-6.66872867893345));
#65882=CARTESIAN_POINT('Ctrl Pts',(37.8771087910329,-3.18357785109312,-6.71013064208345));
#65883=CARTESIAN_POINT('Ctrl Pts',(37.7890755560121,-3.18989084475246,-6.75150321675674));
#65884=CARTESIAN_POINT('Ctrl Pts',(37.7029196893523,-3.1962038384118,-6.79704019928177));
#65885=CARTESIAN_POINT('Ctrl Pts',(37.6190555304126,-3.20251683207115,-6.8465405104835));
#65886=CARTESIAN_POINT('Ctrl Pts',(37.5352216774539,-3.20882754440473,-6.89602293376374));
#65887=CARTESIAN_POINT('Ctrl Pts',(37.4536782628863,-3.21513825673832,-6.94946561780621));
#65888=CARTESIAN_POINT('Ctrl Pts',(37.3748145692308,-3.2214489690719,-7.00662179246092));
#65889=CARTESIAN_POINT('Ctrl Pts',(37.295958014204,-3.22775911016883,-7.06377279342048));
#65890=CARTESIAN_POINT('Ctrl Pts',(37.2197810517871,-3.23406925126577,-7.12463635987137));
#65891=CARTESIAN_POINT('Ctrl Pts',(37.1466426673008,-3.2403793923627,-7.1889233066634));
#65892=CARTESIAN_POINT('Ctrl Pts',(37.073491093871,-3.24669067135863,-7.25322184623148));
#65893=CARTESIAN_POINT('Ctrl Pts',(37.0033795150905,-3.25300195035456,-7.32094470350832));
#65894=CARTESIAN_POINT('Ctrl Pts',(36.936631816048,-3.25931322935049,-7.39176416756751));
#65895=CARTESIAN_POINT('Ctrl Pts',(36.8698127348115,-3.26563125783664,-7.46265936830071));
#65896=CARTESIAN_POINT('Ctrl Pts',(36.8063650158503,-3.2719492863228,-7.53665746850689));
#65897=CARTESIAN_POINT('Ctrl Pts',(36.7465736653391,-3.27826731480895,-7.61339599464424));
#65898=CARTESIAN_POINT('Ctrl Pts',(36.6867472790282,-3.28458904545566,-7.69017948707857));
#65899=CARTESIAN_POINT('Ctrl Pts',(36.6305817796637,-3.29091077610238,-7.7697062459808));
#65900=CARTESIAN_POINT('Ctrl Pts',(36.5783188559795,-3.29723250674909,-7.85158474012361));
#65901=CARTESIAN_POINT('Ctrl Pts',(36.5259721325032,-3.30356437383051,-7.93359452046888));
#65902=CARTESIAN_POINT('Ctrl Pts',(36.477540697407,-3.30989624091193,-8.01796318672667));
#65903=CARTESIAN_POINT('Ctrl Pts',(36.4332202876357,-3.31622810799334,-8.10427459509259));
#65904=CARTESIAN_POINT('Ctrl Pts',(36.4074782645102,-3.31990576056196,-8.15440568101024));
#65905=CARTESIAN_POINT('Ctrl Pts',(36.3831221919925,-3.32358341313057,-8.2051917535564));
#65906=CARTESIAN_POINT('Ctrl Pts',(36.3601828105059,-3.32726106569919,-8.25654858857189));
#65907=CARTESIAN_POINT('Ctrl Pts',(36.3160477270097,-3.33433682331197,-8.35535849775967));
#65908=CARTESIAN_POINT('Ctrl Pts',(36.2770243650611,-3.34141258092474,-8.45658489155548));
#65909=CARTESIAN_POINT('Ctrl Pts',(36.243357954337,-3.34848833853752,-8.55970291271675));
#65910=CARTESIAN_POINT('Ctrl Pts',(36.2105182027539,-3.3553903550361,-8.66028893082336));
#65911=CARTESIAN_POINT('Ctrl Pts',(36.1827755450531,-3.36229237153469,-8.76267446198814));
#65912=CARTESIAN_POINT('Ctrl Pts',(36.1603110343668,-3.36919438803328,-8.86634861640778));
#65913=CARTESIAN_POINT('Ctrl Pts',(36.1369982913306,-3.37635701620315,-8.97393737964616));
#65914=CARTESIAN_POINT('Ctrl Pts',(36.1193703286723,-3.38351964437303,-9.08291374571453));
#65915=CARTESIAN_POINT('Ctrl Pts',(36.1075742388077,-3.3906822725429,-9.19268454081396));
#65916=CARTESIAN_POINT('Ctrl Pts',(36.0957781489431,-3.39784490071277,-9.30245533591338));
#65917=CARTESIAN_POINT('Ctrl Pts',(36.0898140999805,-3.40500752888264,-9.41302021472769));
#65918=CARTESIAN_POINT('Ctrl Pts',(36.0897702438652,-3.41217015705251,-9.52376835315984));
#65919=CARTESIAN_POINT('',(36.0897712316907,-4.68217015708684,-9.52776797424251));
#65920=CARTESIAN_POINT('Ctrl Pts',(36.089770243865,-3.41217015708684,-9.52376835369061));
#65921=CARTESIAN_POINT('Ctrl Pts',(36.0897308469584,-3.41860450524517,-9.6232558691197));
#65922=CARTESIAN_POINT('Ctrl Pts',(36.0944692869388,-3.4250388534035,-9.72271952248611));
#65923=CARTESIAN_POINT('Ctrl Pts',(36.1039523828961,-3.43147320156183,-9.82168131981128));
#65924=CARTESIAN_POINT('Ctrl Pts',(36.1134403070674,-3.43791082569778,-9.92069350244754));
#65925=CARTESIAN_POINT('Ctrl Pts',(36.1276776560797,-3.44434844983373,-10.0192029096662));
#65926=CARTESIAN_POINT('Ctrl Pts',(36.1465795645642,-3.45078607396968,-10.1167383690139));
#65927=CARTESIAN_POINT('Ctrl Pts',(36.165510976694,-3.45723374647609,-10.2144260696866));
#65928=CARTESIAN_POINT('Ctrl Pts',(36.1891214144015,-3.4636814189825,-10.3111363793427));
#65929=CARTESIAN_POINT('Ctrl Pts',(36.2172751014949,-3.4701290914889,-10.4064095715034));
#65930=CARTESIAN_POINT('Ctrl Pts',(36.2454507957173,-3.47658180400162,-10.5017572366603));
#65931=CARTESIAN_POINT('Ctrl Pts',(36.2781766812073,-3.48303451651434,-10.5956651556457));
#65932=CARTESIAN_POINT('Ctrl Pts',(36.3152681542323,-3.48948722902706,-10.6876920619465));
#65933=CARTESIAN_POINT('Ctrl Pts',(36.3524368379709,-3.49595337369811,-10.7799105341933));
#65934=CARTESIAN_POINT('Ctrl Pts',(36.393989101499,-3.50241951836916,-10.8702397909493));
#65935=CARTESIAN_POINT('Ctrl Pts',(36.4396932262027,-3.50888566304022,-10.9582610255738));
#65936=CARTESIAN_POINT('Ctrl Pts',(36.4844143268592,-3.51521273107987,-11.0443890614801));
#65937=CARTESIAN_POINT('Ctrl Pts',(36.5331102241574,-3.52153979911952,-11.1283070947645));
#65938=CARTESIAN_POINT('Ctrl Pts',(36.5855244989187,-3.52786686715917,-11.2096508561555));
#65939=CARTESIAN_POINT('Ctrl Pts',(36.6379847680988,-3.5341994873088,-11.2910659980827));
#65940=CARTESIAN_POINT('Ctrl Pts',(36.6943426987631,-3.54053210745842,-11.3701697916308));
#65941=CARTESIAN_POINT('Ctrl Pts',(36.7543681441278,-3.54686472760805,-11.4465658922981));
#65942=CARTESIAN_POINT('Ctrl Pts',(36.814312804837,-3.55318882506311,-11.5228591760244));
#65943=CARTESIAN_POINT('Ctrl Pts',(36.8779149020383,-3.55951292251816,-11.5964516687685));
#65944=CARTESIAN_POINT('Ctrl Pts',(36.9449003400655,-3.56583701997322,-11.666974831006));
#65945=CARTESIAN_POINT('Ctrl Pts',(37.0118156643394,-3.57215449798647,-11.7374241765492));
#65946=CARTESIAN_POINT('Ctrl Pts',(37.0821069894798,-3.57847197599972,-11.8048102631216));
#65947=CARTESIAN_POINT('Ctrl Pts',(37.1554598181657,-3.58478945401297,-11.8687973670445));
#65948=CARTESIAN_POINT('Ctrl Pts',(37.2287605785984,-3.59110244767231,-11.9327390508142));
#65949=CARTESIAN_POINT('Ctrl Pts',(37.305118193598,-3.59741544133165,-11.9932862618891));
#65950=CARTESIAN_POINT('Ctrl Pts',(37.3841818472024,-3.60372843499099,-12.0501406077426));
#65951=CARTESIAN_POINT('Ctrl Pts',(37.4632169295839,-3.61003914732457,-12.1069744081481));
#65952=CARTESIAN_POINT('Ctrl Pts',(37.5449557528238,-3.61634985965815,-12.1601177399249));
#65953=CARTESIAN_POINT('Ctrl Pts',(37.6290157560935,-3.62266057199173,-12.2093135357661));
#65954=CARTESIAN_POINT('Ctrl Pts',(37.7130681503719,-3.62897071308866,-12.2585048784743));
#65955=CARTESIAN_POINT('Ctrl Pts',(37.7994409294023,-3.63528085418559,-12.3037491749849));
#65956=CARTESIAN_POINT('Ctrl Pts',(37.8877248953068,-3.64159099528252,-12.3448341622341));
#65957=CARTESIAN_POINT('Ctrl Pts',(37.9760247813366,-3.64790227427845,-12.3859265582821));
#65958=CARTESIAN_POINT('Ctrl Pts',(38.0662361422508,-3.65421355327439,-12.4228579709121));
#65959=CARTESIAN_POINT('Ctrl Pts',(38.1579286363547,-3.66052483227032,-12.4554637731885));
#65960=CARTESIAN_POINT('Ctrl Pts',(38.2497191894404,-3.66684286075647,-12.4881044451869));
#65961=CARTESIAN_POINT('Ctrl Pts',(38.3429936253149,-3.67316088924262,-12.5164101246133));
#65962=CARTESIAN_POINT('Ctrl Pts',(38.4373054240797,-3.67947891772876,-12.5402657655275));
#65963=CARTESIAN_POINT('Ctrl Pts',(38.5316724865116,-3.68580064837548,-12.5641353850765));
#65964=CARTESIAN_POINT('Ctrl Pts',(38.6270776939102,-3.6921223790222,-12.5835496865475));
#65965=CARTESIAN_POINT('Ctrl Pts',(38.7230653569237,-3.69844410966892,-12.5984449725241));
#65966=CARTESIAN_POINT('Ctrl Pts',(38.8192069291644,-3.70477597675033,-12.613364142007));
#65967=CARTESIAN_POINT('Ctrl Pts',(38.9159323873655,-3.71110784383175,-12.6237497805225));
#65968=CARTESIAN_POINT('Ctrl Pts',(39.012782002131,-3.71743971091316,-12.6295901620301));
#65969=CARTESIAN_POINT('Ctrl Pts',(39.069033851694,-3.72111736348183,-12.6329823516918));
#65970=CARTESIAN_POINT('Ctrl Pts',(39.1253275853489,-3.72479501605049,-12.6348421862075));
#65971=CARTESIAN_POINT('Ctrl Pts',(39.1815737290658,-3.72847266861915,-12.6351754171492));
#65972=CARTESIAN_POINT('Ctrl Pts',(39.2784250374454,-3.73480528876879,-12.6357492138678));
#65973=CARTESIAN_POINT('Ctrl Pts',(39.375471400899,-3.74113790891842,-12.6317957542547));
#65974=CARTESIAN_POINT('Ctrl Pts',(39.4722551252913,-3.74747052906806,-12.623291109572));
#65975=CARTESIAN_POINT('Ctrl Pts',(39.5689085942595,-3.75379462652311,-12.6147979107817));
#65976=CARTESIAN_POINT('Ctrl Pts',(39.6652996947494,-3.76011872397817,-12.6017657389353));
#65977=CARTESIAN_POINT('Ctrl Pts',(39.7609699927092,-3.76644282143322,-12.5842226660019));
#65978=CARTESIAN_POINT('Ctrl Pts',(39.8565401524318,-3.77276029944646,-12.566697955428));
#65979=CARTESIAN_POINT('Ctrl Pts',(39.9513905816555,-3.77907777745969,-12.5446718089296));
#65980=CARTESIAN_POINT('Ctrl Pts',(40.0450682414024,-3.78539525547293,-12.5182240678361));
#65981=CARTESIAN_POINT('Ctrl Pts',(40.1386794056622,-3.79170824913227,-12.4917951002199));
#65982=CARTESIAN_POINT('Ctrl Pts',(40.2311190357782,-3.79802124279162,-12.4609508962037));
#65983=CARTESIAN_POINT('Ctrl Pts',(40.321945500733,-3.80433423645096,-12.4258221155881));
#65984=CARTESIAN_POINT('Ctrl Pts',(40.412739143739,-3.81064494878454,-12.3907060294557));
#65985=CARTESIAN_POINT('Ctrl Pts',(40.5019203724547,-3.81695566111812,-12.3513086008371));
#65986=CARTESIAN_POINT('Ctrl Pts',(40.5890648084925,-3.8232663734517,-12.307809661243));
#65987=CARTESIAN_POINT('Ctrl Pts',(40.6762013563408,-3.82957651454865,-12.2643146591107));
#65988=CARTESIAN_POINT('Ctrl Pts',(40.761301086895,-3.83588665564559,-12.216719079654));
#65989=CARTESIAN_POINT('Ctrl Pts',(40.8439625796973,-3.84219679674253,-12.1652495506022));
#65990=CARTESIAN_POINT('Ctrl Pts',(40.9266389787322,-3.84850807573848,-12.1137707401214));
#65991=CARTESIAN_POINT('Ctrl Pts',(41.0068758955392,-3.85481935473442,-12.0584168237454));
#65992=CARTESIAN_POINT('Ctrl Pts',(41.0843002416636,-3.86113063373037,-11.9994581734526));
#65993=CARTESIAN_POINT('Ctrl Pts',(41.1618073879408,-3.86744866221652,-11.9404364708319));
#65994=CARTESIAN_POINT('Ctrl Pts',(41.236495610022,-3.87376669070267,-11.8778026033331));
#65995=CARTESIAN_POINT('Ctrl Pts',(41.3080244943481,-3.88008471918883,-11.8118675921724));
#65996=CARTESIAN_POINT('Ctrl Pts',(41.3795952922897,-3.88640644983557,-11.7458939452252));
#65997=CARTESIAN_POINT('Ctrl Pts',(41.4480027589633,-3.89272818048231,-11.6766156138095));
#65998=CARTESIAN_POINT('Ctrl Pts',(41.5129444669172,-3.89904991112905,-11.6043793655457));
#65999=CARTESIAN_POINT('Ctrl Pts',(41.5779903041701,-3.90538177821047,-11.5320272917188));
#66000=CARTESIAN_POINT('Ctrl Pts',(41.6395590095688,-3.91171364529189,-11.4567081688672));
#66001=CARTESIAN_POINT('Ctrl Pts',(41.6973894671656,-3.91804551237331,-11.3788005562061));
#66002=CARTESIAN_POINT('Ctrl Pts',(41.7309783483266,-3.92172316494192,-11.3335505330877));
#66003=CARTESIAN_POINT('Ctrl Pts',(41.7633069582748,-3.92540081751053,-11.2874278227167));
#66004=CARTESIAN_POINT('Ctrl Pts',(41.794331205074,-3.92907847007914,-11.2405104929085));
#66005=CARTESIAN_POINT('Ctrl Pts',(41.8477524477669,-3.93541109022877,-11.1597226472469));
#66006=CARTESIAN_POINT('Ctrl Pts',(41.8974892705568,-3.9417437103784,-11.0762967821856));
#66007=CARTESIAN_POINT('Ctrl Pts',(41.9432714516952,-3.94807633052803,-10.9906030824252));
#66008=CARTESIAN_POINT('Ctrl Pts',(41.9889920173352,-3.95440042798309,-10.9050247126882));
#66009=CARTESIAN_POINT('Ctrl Pts',(42.0307683153435,-3.96072452543815,-10.8171849569883));
#66010=CARTESIAN_POINT('Ctrl Pts',(42.0683732639495,-3.96704862289321,-10.7274830441881));
#66011=CARTESIAN_POINT('Ctrl Pts',(42.1059388514021,-3.97336610090644,-10.6378750225079));
#66012=CARTESIAN_POINT('Ctrl Pts',(42.1393416013967,-3.97968357891967,-10.546409119865));
#66013=CARTESIAN_POINT('Ctrl Pts',(42.1684007319163,-3.98600105693291,-10.4535083454977));
#66014=CARTESIAN_POINT('Ctrl Pts',(42.1974392353083,-3.99231405059225,-10.3606735151586));
#66015=CARTESIAN_POINT('Ctrl Pts',(42.2221401187166,-3.99862704425159,-10.2664062541597));
#66016=CARTESIAN_POINT('Ctrl Pts',(42.2423713903786,-4.00494003791094,-10.1711477972613));
#66017=CARTESIAN_POINT('Ctrl Pts',(42.2625953510684,-4.01125075024452,-10.0759237639));
#66018=CARTESIAN_POINT('Ctrl Pts',(42.2783528186387,-4.0175614625781,-9.97970967370127));
#66019=CARTESIAN_POINT('Ctrl Pts',(42.2895624074209,-4.02387217491168,-9.88295919257854));
#66020=CARTESIAN_POINT('Ctrl Pts',(42.3007709815272,-4.03018231600861,-9.78621746917095));
#66021=CARTESIAN_POINT('Ctrl Pts',(42.3074324452119,-4.03649245710554,-9.68893988580377));
#66022=CARTESIAN_POINT('Ctrl Pts',(42.3095171483323,-4.04280259820247,-9.59158646354242));
#66023=CARTESIAN_POINT('Ctrl Pts',(42.3116022273844,-4.04911387719839,-9.49421548567346));
#66024=CARTESIAN_POINT('Ctrl Pts',(42.3091088973539,-4.05542515619432,-9.39676907895592));
#66025=CARTESIAN_POINT('Ctrl Pts',(42.3020596255315,-4.06173643519024,-9.29970745119377));
#66026=CARTESIAN_POINT('Ctrl Pts',(42.2950028149849,-4.06805446367639,-9.20254202252081));
#66027=CARTESIAN_POINT('Ctrl Pts',(42.2833803671463,-4.07437249216254,-9.10576263121383));
#66028=CARTESIAN_POINT('Ctrl Pts',(42.2672666489418,-4.08069052064869,-9.00982434336522));
#66029=CARTESIAN_POINT('Ctrl Pts',(42.2511434886192,-4.08701225129541,-8.9138298387795));
#66030=CARTESIAN_POINT('Ctrl Pts',(42.230523909995,-4.09333398194213,-8.81867784627415));
#66031=CARTESIAN_POINT('Ctrl Pts',(42.2055329772973,-4.09965571258885,-8.72481116273821));
#66032=CARTESIAN_POINT('Ctrl Pts',(42.1805019734591,-4.10598757967026,-8.63079397081134));
#66033=CARTESIAN_POINT('Ctrl Pts',(42.1510857516613,-4.11231944675168,-8.53806661968593));
#66034=CARTESIAN_POINT('Ctrl Pts',(42.1174585794742,-4.1186513138331,-8.44705469064864));
#66035=CARTESIAN_POINT('Ctrl Pts',(42.0979273646554,-4.12232896640177,-8.39419346499427));
#66036=CARTESIAN_POINT('Ctrl Pts',(42.076976489609,-4.12600661897045,-8.34191053978871));
#66037=CARTESIAN_POINT('Ctrl Pts',(42.0546472253936,-4.12968427153912,-8.2902855101471));
#66038=CARTESIAN_POINT('Ctrl Pts',(42.0161980391651,-4.13601689168875,-8.20139138629269));
#66039=CARTESIAN_POINT('Ctrl Pts',(41.9735258507318,-4.14234951183837,-8.11414053622946));
#66040=CARTESIAN_POINT('Ctrl Pts',(41.9267929375975,-4.14868213198799,-8.02896158860526));
#66041=CARTESIAN_POINT('Ctrl Pts',(41.8801229194947,-4.15500622944307,-7.94389727822993));
#66042=CARTESIAN_POINT('Ctrl Pts',(41.8294032473786,-4.16133032689815,-7.86089970828239));
#66043=CARTESIAN_POINT('Ctrl Pts',(41.7748441009242,-4.16765442435323,-7.78037725887913));
#66044=CARTESIAN_POINT('Ctrl Pts',(41.7203420616064,-4.17397190236645,-7.69993909243891));
#66045=CARTESIAN_POINT('Ctrl Pts',(41.6620087814985,-4.18028938037968,-7.6219712562158));
#66046=CARTESIAN_POINT('Ctrl Pts',(41.6000996618428,-4.1866068583929,-7.54685635857203));
#66047=CARTESIAN_POINT('Ctrl Pts',(41.5382344873185,-4.19291985205224,-7.47179477995561));
#66048=CARTESIAN_POINT('Ctrl Pts',(41.4727987967841,-4.19923284571157,-7.39958245038754));
#66049=CARTESIAN_POINT('Ctrl Pts',(41.404089922872,-4.20554583937091,-7.33057108458848));
#66050=CARTESIAN_POINT('Ctrl Pts',(41.3354058782774,-4.21185655170449,-7.26158465741842));
#66051=CARTESIAN_POINT('Ctrl Pts',(41.2634513088352,-4.21816726403806,-7.19579720516986));
#66052=CARTESIAN_POINT('Ctrl Pts',(41.188561619043,-4.22447797637164,-7.13352486105981));
#66053=CARTESIAN_POINT('Ctrl Pts',(41.1136787081582,-4.23078811746858,-7.07125815375307));
#66054=CARTESIAN_POINT('Ctrl Pts',(41.0358615415469,-4.23709825856552,-7.01250620140424));
#66055=CARTESIAN_POINT('Ctrl Pts',(40.9554791250099,-4.24340839966246,-6.95754528870432));
#66056=CARTESIAN_POINT('Ctrl Pts',(40.8750822132234,-4.24971967865839,-6.90257446497931));
#66057=CARTESIAN_POINT('Ctrl Pts',(40.7921194937645,-4.25603095765431,-6.85139628548057));
#66058=CARTESIAN_POINT('Ctrl Pts',(40.7069886171799,-4.26234223665024,-6.80424349479959));
#66059=CARTESIAN_POINT('Ctrl Pts',(40.6217666988239,-4.26866026513638,-6.75704027736681));
#66060=CARTESIAN_POINT('Ctrl Pts',(40.5343723773683,-4.27497829362253,-6.71387125545519));
#66061=CARTESIAN_POINT('Ctrl Pts',(40.4452273671073,-4.28129632210867,-6.67492290330472));
#66062=CARTESIAN_POINT('Ctrl Pts',(40.3560301207502,-4.2876180527554,-6.63595172867815));
#66063=CARTESIAN_POINT('Ctrl Pts',(40.2650805511827,-4.29393978340213,-6.60120630457832));
#66064=CARTESIAN_POINT('Ctrl Pts',(40.1728178107986,-4.30026151404886,-6.57082394568417));
#66065=CARTESIAN_POINT('Ctrl Pts',(40.0804071338296,-4.30659338113028,-6.54039287089023));
#66066=CARTESIAN_POINT('Ctrl Pts',(39.9866795026542,-4.3129252482117,-6.5143389478488));
#66067=CARTESIAN_POINT('Ctrl Pts',(39.8920865491162,-4.31925711529312,-6.49274887889666));
#66068=CARTESIAN_POINT('Ctrl Pts',(39.8371454055193,-4.32293476786178,-6.48020901166344));
#66069=CARTESIAN_POINT('Ctrl Pts',(39.7819125069031,-4.32661242043044,-6.46917405159658));
#66070=CARTESIAN_POINT('Ctrl Pts',(39.7264770642849,-4.3302900729991,-6.45965294726977));
#66071=CARTESIAN_POINT('Ctrl Pts',(39.6310217176002,-4.33662269314873,-6.44325837600969));
#66072=CARTESIAN_POINT('Ctrl Pts',(39.5346340451537,-4.34295531329836,-6.43129831318331));
#66073=CARTESIAN_POINT('Ctrl Pts',(39.4377616765962,-4.34928793344799,-6.4238711671325));
#66074=CARTESIAN_POINT('Ctrl Pts',(39.3410196827633,-4.35561203090306,-6.41645401683317));
#66075=CARTESIAN_POINT('Ctrl Pts',(39.2437947216939,-4.36193612835813,-6.41355769126737));
#66076=CARTESIAN_POINT('Ctrl Pts',(39.1465436515253,-4.3682602258132,-6.41522941815514));
#66077=CARTESIAN_POINT('Ctrl Pts',(39.0493943741911,-4.37457770382642,-6.41689939524398));
#66078=CARTESIAN_POINT('Ctrl Pts',(38.9522194770394,-4.38089518183964,-6.42312791168205));
#66079=CARTESIAN_POINT('Ctrl Pts',(38.8554789563812,-4.38721265985286,-6.43391024015739));
#66080=CARTESIAN_POINT('Ctrl Pts',(38.7588071053295,-4.3935256535122,-6.444684914981));
#66081=CARTESIAN_POINT('Ctrl Pts',(38.6625694511726,-4.39983864717155,-6.46000692724261));
#66082=CARTESIAN_POINT('Ctrl Pts',(38.5672230409478,-4.40615164083089,-6.47981955001142));
#66083=CARTESIAN_POINT('Ctrl Pts',(38.4719110860439,-4.41246235316447,-6.49962501309511));
#66084=CARTESIAN_POINT('Ctrl Pts',(38.3774901628507,-4.41877306549805,-6.52391777334063));
#66085=CARTESIAN_POINT('Ctrl Pts',(38.2844083339141,-4.42508377783163,-6.55258977361906));
#66086=CARTESIAN_POINT('Ctrl Pts',(38.1913349306115,-4.43139391892856,-6.58125917854902));
#66087=CARTESIAN_POINT('Ctrl Pts',(38.0996007984381,-4.43770406002549,-6.61430690643706));
#66088=CARTESIAN_POINT('Ctrl Pts',(38.0096389986286,-4.44401420112242,-6.65157498108719));
#66089=CARTESIAN_POINT('Ctrl Pts',(37.9196609761319,-4.45032548011838,-6.68884977623781));
#66090=CARTESIAN_POINT('Ctrl Pts',(37.8314563247676,-4.45663675911435,-6.73034626228963));
#66091=CARTESIAN_POINT('Ctrl Pts',(37.7454373038562,-4.46294803811032,-6.77585867662521));
#66092=CARTESIAN_POINT('Ctrl Pts',(37.6593262913632,-4.46926606659647,-6.82141976343968));
#66093=CARTESIAN_POINT('Ctrl Pts',(37.5754059629639,-4.47558409508262,-6.87100514794837));
#66094=CARTESIAN_POINT('Ctrl Pts',(37.494062985742,-4.48190212356877,-6.92436362474789));
#66095=CARTESIAN_POINT('Ctrl Pts',(37.4126723441633,-4.48822385421551,-6.97775336789099));
#66096=CARTESIAN_POINT('Ctrl Pts',(37.3338624149043,-4.49454558486224,-7.03492034918793));
#66097=CARTESIAN_POINT('Ctrl Pts',(37.2579882317365,-4.50086731550897,-7.09557188934801));
#66098=CARTESIAN_POINT('Ctrl Pts',(37.1819923898418,-4.5071991825904,-7.15632067983559));
#66099=CARTESIAN_POINT('Ctrl Pts',(37.1089420217795,-4.51353104967182,-7.22056489729979));
#66100=CARTESIAN_POINT('Ctrl Pts',(37.0391566009855,-4.51986291675324,-7.28797374672638));
#66101=CARTESIAN_POINT('Ctrl Pts',(36.9986240805244,-4.52354056932185,-7.32712591543949));
#66102=CARTESIAN_POINT('Ctrl Pts',(36.9591922626734,-4.52721822189046,-7.36734500511245));
#66103=CARTESIAN_POINT('Ctrl Pts',(36.9209174052313,-4.53089587445908,-7.40856120354915));
#66104=CARTESIAN_POINT('Ctrl Pts',(36.8553184770402,-4.53719896956857,-7.47920126917562));
#66105=CARTESIAN_POINT('Ctrl Pts',(36.7928785099401,-4.54350206467806,-7.55303258751636));
#66106=CARTESIAN_POINT('Ctrl Pts',(36.7339284141938,-4.54980515978755,-7.62973706663706));
#66107=CARTESIAN_POINT('Ctrl Pts',(36.6754872120085,-4.55605384269508,-7.70577938541652));
#66108=CARTESIAN_POINT('Ctrl Pts',(36.6204761746455,-4.56230252560262,-7.78464511883583));
#66109=CARTESIAN_POINT('Ctrl Pts',(36.569181482799,-4.56855120851016,-7.86598686489461));
#66110=CARTESIAN_POINT('Ctrl Pts',(36.5179349658241,-4.57479402278907,-7.94725221653455));
#66111=CARTESIAN_POINT('Ctrl Pts',(36.4703981015631,-4.58103683706799,-8.03098858612567));
#66112=CARTESIAN_POINT('Ctrl Pts',(36.4268156026728,-4.5872796513469,-8.11681714563738));
#66113=CARTESIAN_POINT('Ctrl Pts',(36.3832615433595,-4.59351839190352,-8.20258969808233));
#66114=CARTESIAN_POINT('Ctrl Pts',(36.3436569259494,-4.59975713246014,-8.29045132955641));
#66115=CARTESIAN_POINT('Ctrl Pts',(36.308201449891,-4.60599587301677,-8.37999703123199));
#66116=CARTESIAN_POINT('Ctrl Pts',(36.272125852573,-4.61234373002261,-8.4711088998159));
#66117=CARTESIAN_POINT('Ctrl Pts',(36.2403461461278,-4.61869158702844,-8.56396389225379));
#66118=CARTESIAN_POINT('Ctrl Pts',(36.2130219718117,-4.62503944403428,-8.65811309156248));
#66119=CARTESIAN_POINT('Ctrl Pts',(36.1861721018347,-4.63127711230808,-8.75062801006035));
#66120=CARTESIAN_POINT('Ctrl Pts',(36.1636244051878,-4.63751478058188,-8.84439210881212));
#66121=CARTESIAN_POINT('Ctrl Pts',(36.1454798590326,-4.64375244885568,-8.93896470983034));
#66122=CARTESIAN_POINT('Ctrl Pts',(36.1268545263607,-4.65015540022754,-9.03604325566669));
#66123=CARTESIAN_POINT('Ctrl Pts',(36.1128690938145,-4.6565583515994,-9.13397326884296));
#66124=CARTESIAN_POINT('Ctrl Pts',(36.1035763459161,-4.66296130297126,-9.23226939461385));
#66125=CARTESIAN_POINT('Ctrl Pts',(36.0942835980177,-4.66936425434312,-9.33056552038474));
#66126=CARTESIAN_POINT('Ctrl Pts',(36.0896835345435,-4.67576720571498,-9.42922724870747));
#66127=CARTESIAN_POINT('Ctrl Pts',(36.0897712316907,-4.68217015708684,-9.52776797424251));
#66128=CARTESIAN_POINT('',(36.0897047610518,-5.95217015708685,-9.52350960940354));
#66129=CARTESIAN_POINT('Ctrl Pts',(36.0901415350687,-4.68217037744286,-9.52777103554189));
#66130=CARTESIAN_POINT('Ctrl Pts',(36.0878821773097,-4.69861414360159,-9.78081088334408));
#66131=CARTESIAN_POINT('Ctrl Pts',(36.23139618657,-4.78192651024699,-11.0603082092272));
#66132=CARTESIAN_POINT('Ctrl Pts',(37.9960327313695,-4.93210747737905,-12.9917445733203));
#66133=CARTESIAN_POINT('Ctrl Pts',(41.4448765000052,-5.13271327883904,-12.4281680317038));
#66134=CARTESIAN_POINT('Ctrl Pts',(42.8581511280529,-5.33331908029901,-9.23210847586989));
#66135=CARTESIAN_POINT('Ctrl Pts',(40.9543526129433,-5.53392488175898,-6.30163188108486));
#66136=CARTESIAN_POINT('Ctrl Pts',(37.4597734733276,-5.73453068321898,-6.29398363414102));
#66137=CARTESIAN_POINT('Ctrl Pts',(36.1277880032688,-5.87394577499493,-8.32476719916938));
#66138=CARTESIAN_POINT('Ctrl Pts',(36.0851544239569,-5.94649226628422,-9.4364601111202));
#66139=CARTESIAN_POINT('Ctrl Pts',(36.0856727518626,-5.95217015708685,-9.52350767734625));
#66140=CARTESIAN_POINT('',(36.0897702898568,-7.22217015705017,-9.52365722578339));
#66141=CARTESIAN_POINT('Ctrl Pts',(36.089770357075,-5.95217015708685,-9.52350964083583));
#66142=CARTESIAN_POINT('Ctrl Pts',(36.089724436915,-5.95842920731442,-9.61934039494398));
#66143=CARTESIAN_POINT('Ctrl Pts',(36.0941117716707,-5.96468825754199,-9.71534736715066));
#66144=CARTESIAN_POINT('Ctrl Pts',(36.1029549177913,-5.97094730776956,-9.81108112777174));
#66145=CARTESIAN_POINT('Ctrl Pts',(36.1117869597681,-5.97719849864555,-9.90669467761718));
#66146=CARTESIAN_POINT('Ctrl Pts',(36.1250636570616,-5.98344968952154,-10.0020352547221));
#66147=CARTESIAN_POINT('Ctrl Pts',(36.142755544866,-5.98970088039753,-10.0966528618423));
#66148=CARTESIAN_POINT('Ctrl Pts',(36.1604303082252,-5.99594602058086,-10.1911788860831));
#66149=CARTESIAN_POINT('Ctrl Pts',(36.182511685981,-6.0021911607642,-10.2849828927258));
#66150=CARTESIAN_POINT('Ctrl Pts',(36.2089184721355,-6.00843630094753,-10.3776206346128));
#66151=CARTESIAN_POINT('Ctrl Pts',(36.235311544599,-6.01467819787661,-10.4702102674514));
#66152=CARTESIAN_POINT('Ctrl Pts',(36.2660254427374,-6.02092009480568,-10.5616344080258));
#66153=CARTESIAN_POINT('Ctrl Pts',(36.3009282168457,-6.02716199173475,-10.6514605847604));
#66154=CARTESIAN_POINT('Ctrl Pts',(36.335822844769,-6.03340243182698,-10.7412657963805));
#66155=CARTESIAN_POINT('Ctrl Pts',(36.3749042442181,-6.03964287191921,-10.8294733674587));
#66156=CARTESIAN_POINT('Ctrl Pts',(36.4179915011379,-6.04588331201144,-10.9156686755511));
#66157=CARTESIAN_POINT('Ctrl Pts',(36.4610810214978,-6.05212407992361,-11.001868511616));
#66158=CARTESIAN_POINT('Ctrl Pts',(36.5081766155351,-6.05836484783578,-11.0860554744702));
#66159=CARTESIAN_POINT('Ctrl Pts',(36.5590509280406,-6.06460561574796,-11.1678385959116));
#66160=CARTESIAN_POINT('Ctrl Pts',(36.6099747976654,-6.07085246284753,-11.2497013830173));
#66161=CARTESIAN_POINT('Ctrl Pts',(36.6646844987986,-6.07709930994711,-11.3291552714969));
#66162=CARTESIAN_POINT('Ctrl Pts',(36.7229089329688,-6.08334615704669,-11.4058377119077));
#66163=CARTESIAN_POINT('Ctrl Pts',(36.781162413407,-6.0895961204942,-11.4825584066829));
#66164=CARTESIAN_POINT('Ctrl Pts',(36.8429338296361,-6.09584608394171,-11.5565045573239));
#66165=CARTESIAN_POINT('Ctrl Pts',(36.9079127702298,-6.10209604738921,-11.6273479217352));
#66166=CARTESIAN_POINT('Ctrl Pts',(36.972999067908,-6.10835633691849,-11.6983083323309));
#66167=CARTESIAN_POINT('Ctrl Pts',(37.041303155336,-6.11461662644778,-11.766155402873));
#66168=CARTESIAN_POINT('Ctrl Pts',(37.1124789097127,-6.12087691597706,-11.8305989136244));
#66169=CARTESIAN_POINT('Ctrl Pts',(37.1688157042764,-6.12583203936435,-11.8816070252764));
#66170=CARTESIAN_POINT('Ctrl Pts',(37.226950855291,-6.13078716275165,-11.9304835512479));
#66171=CARTESIAN_POINT('Ctrl Pts',(37.2866998353367,-6.13574228613894,-11.9771038177042));
#66172=CARTESIAN_POINT('Ctrl Pts',(37.3630586997653,-6.14207490628857,-12.0366842591316));
#66173=CARTESIAN_POINT('Ctrl Pts',(37.4423358620394,-6.1484075264382,-12.092798054621));
#66174=CARTESIAN_POINT('Ctrl Pts',(37.5241834226642,-6.15474014658783,-12.145146837875));
#66175=CARTESIAN_POINT('Ctrl Pts',(37.6059208295544,-6.1610642440429,-12.1974251680338));
#66176=CARTESIAN_POINT('Ctrl Pts',(37.6902213938912,-6.16738834149797,-12.2459483234262));
#66177=CARTESIAN_POINT('Ctrl Pts',(37.7767048846497,-6.17371243895304,-12.2904586721772));
#66178=CARTESIAN_POINT('Ctrl Pts',(37.8630978530149,-6.18002991696628,-12.3349224318826));
#66179=CARTESIAN_POINT('Ctrl Pts',(37.951668818572,-6.18634739497951,-12.3753815360964));
#66180=CARTESIAN_POINT('Ctrl Pts',(38.0420102190963,-6.19266487299274,-12.4116226494335));
#66181=CARTESIAN_POINT('Ctrl Pts',(38.1322874923201,-6.19897786665208,-12.4478380376352));
#66182=CARTESIAN_POINT('Ctrl Pts',(38.2243322973688,-6.20529086031143,-12.479841224991));
#66183=CARTESIAN_POINT('Ctrl Pts',(38.3177150837064,-6.21160385397077,-12.5074660902315));
#66184=CARTESIAN_POINT('Ctrl Pts',(38.4110641243177,-6.21791456630435,-12.5350809726778));
#66185=CARTESIAN_POINT('Ctrl Pts',(38.5057497665624,-6.22422527863793,-12.5583205529172));
#66186=CARTESIAN_POINT('Ctrl Pts',(38.6013261060655,-6.23053599097151,-12.5770681875773));
#66187=CARTESIAN_POINT('Ctrl Pts',(38.6968937941349,-6.23684613206844,-12.5958141252283));
#66188=CARTESIAN_POINT('Ctrl Pts',(38.7933515899888,-6.24315627316536,-12.6100688417519));
#66189=CARTESIAN_POINT('Ctrl Pts',(38.8902432043774,-6.24946641426229,-12.619766773194));
#66190=CARTESIAN_POINT('Ctrl Pts',(38.9871522910966,-6.25577769325822,-12.6294664534506));
#66191=CARTESIAN_POINT('Ctrl Pts',(39.0844949165885,-6.26208897225415,-12.6346076730712));
#66192=CARTESIAN_POINT('Ctrl Pts',(39.1818105263284,-6.26840025125008,-12.6351768110427));
#66193=CARTESIAN_POINT('Ctrl Pts',(39.2792302085957,-6.27471827973623,-12.6357465576691));
#66194=CARTESIAN_POINT('Ctrl Pts',(39.3766223794049,-6.28103630822238,-12.6317344583957));
#66195=CARTESIAN_POINT('Ctrl Pts',(39.4735275481078,-6.28735433670852,-12.6231790350666));
#66196=CARTESIAN_POINT('Ctrl Pts',(39.570489500109,-6.29367606735526,-12.6146185985358));
#66197=CARTESIAN_POINT('Ctrl Pts',(39.6669634486199,-6.29999779800199,-12.601509595556));
#66198=CARTESIAN_POINT('Ctrl Pts',(39.7624981666,-6.30631952864872,-12.5839420500349));
#66199=CARTESIAN_POINT('Ctrl Pts',(39.8581860675425,-6.31265139573014,-12.566346336234));
#66200=CARTESIAN_POINT('Ctrl Pts',(39.9529313051179,-6.31898326281155,-12.5442779038389));
#66201=CARTESIAN_POINT('Ctrl Pts',(40.0462959640472,-6.32531512989297,-12.5178771765873));
#66202=CARTESIAN_POINT('Ctrl Pts',(40.100523693928,-6.32899278246162,-12.502543199872));
#66203=CARTESIAN_POINT('Ctrl Pts',(40.1542860108318,-6.33267043503027,-12.4857486556877));
#66204=CARTESIAN_POINT('Ctrl Pts',(40.2075003336219,-6.33634808759892,-12.4675284587667));
#66205=CARTESIAN_POINT('Ctrl Pts',(40.2991310916823,-6.34268070774852,-12.4361547539378));
#66206=CARTESIAN_POINT('Ctrl Pts',(40.3894541413373,-6.34901332789811,-12.4004423862849));
#66207=CARTESIAN_POINT('Ctrl Pts',(40.4780294677295,-6.35534594804771,-12.3605195877502));
#66208=CARTESIAN_POINT('Ctrl Pts',(40.5664855858895,-6.36167004550275,-12.3206505189214));
#66209=CARTESIAN_POINT('Ctrl Pts',(40.6531982604861,-6.36799414295779,-12.2765824599564));
#66210=CARTESIAN_POINT('Ctrl Pts',(40.7377439138879,-6.37431824041282,-12.2284929828281));
#66211=CARTESIAN_POINT('Ctrl Pts',(40.8222010732339,-6.38063571842606,-12.1804538410239));
#66212=CARTESIAN_POINT('Ctrl Pts',(40.904495342597,-6.38695319643929,-12.1284018642748));
#66213=CARTESIAN_POINT('Ctrl Pts',(40.9842252976564,-6.39327067445252,-12.0725617244932));
#66214=CARTESIAN_POINT('Ctrl Pts',(41.0638986577684,-6.39958366811184,-12.0167612218815));
#66215=CARTESIAN_POINT('Ctrl Pts',(41.1410109651289,-6.40589666177116,-11.9571781522152));
#66216=CARTESIAN_POINT('Ctrl Pts',(41.2151883124176,-6.41220965543048,-11.8940814081402));
#66217=CARTESIAN_POINT('Ctrl Pts',(41.2893388542473,-6.41852036776404,-11.8310074653279));
#66218=CARTESIAN_POINT('Ctrl Pts',(41.3605562106748,-6.4248310800976,-11.7644226541438));
#66219=CARTESIAN_POINT('Ctrl Pts',(41.4284989669377,-6.43114179243116,-11.6946366071897));
#66220=CARTESIAN_POINT('Ctrl Pts',(41.4964355731195,-6.43745193352806,-11.6248568771686));
#66221=CARTESIAN_POINT('Ctrl Pts',(41.5610978635619,-6.44376207462497,-11.5518768009912));
#66222=CARTESIAN_POINT('Ctrl Pts',(41.6221815198935,-6.45007221572188,-11.4760426283366));
#66223=CARTESIAN_POINT('Ctrl Pts',(41.6832761913563,-6.45638349471781,-11.4001947806105));
#66224=CARTESIAN_POINT('Ctrl Pts',(41.7407906727067,-6.46269477371374,-11.3214921547849));
#66225=CARTESIAN_POINT('Ctrl Pts',(41.7944618101514,-6.46900605270968,-11.2403129651949));
#66226=CARTESIAN_POINT('Ctrl Pts',(41.8481903452831,-6.47532408119581,-11.1590469598985));
#66227=CARTESIAN_POINT('Ctrl Pts',(41.8980670891438,-6.48164210968194,-11.0752994686089));
#66228=CARTESIAN_POINT('Ctrl Pts',(41.9438731329391,-6.48796013816807,-10.9894763170619));
#66229=CARTESIAN_POINT('Ctrl Pts',(41.9897060175962,-6.49428186881478,-10.9036028759207));
#66230=CARTESIAN_POINT('Ctrl Pts',(42.0314632649294,-6.5006035994615,-10.8156517474713));
#66231=CARTESIAN_POINT('Ctrl Pts',(42.0689736100634,-6.50692533010821,-10.726049989659));
#66232=CARTESIAN_POINT('Ctrl Pts',(42.1065441003039,-6.5132571971896,-10.6363045619539));
#66233=CARTESIAN_POINT('Ctrl Pts',(42.1398539411277,-6.519589064271,-10.544903630581));
#66234=CARTESIAN_POINT('Ctrl Pts',(42.1687813480053,-6.52592093135239,-10.4522906559626));
#66235=CARTESIAN_POINT('Ctrl Pts',(42.1855828618157,-6.52959858392123,-10.3984995166929));
#66236=CARTESIAN_POINT('Ctrl Pts',(42.2009069199183,-6.53327623649006,-10.3442997318519));
#66237=CARTESIAN_POINT('Ctrl Pts',(42.2147376188538,-6.5369538890589,-10.2897795384083));
#66238=CARTESIAN_POINT('Ctrl Pts',(42.2385529633224,-6.54328650920859,-10.1959001767492));
#66239=CARTESIAN_POINT('Ctrl Pts',(42.2580203736777,-6.54961912935828,-10.1007442708017));
#66240=CARTESIAN_POINT('Ctrl Pts',(42.2730067085367,-6.55595174950798,-10.0047503748703));
#66241=CARTESIAN_POINT('Ctrl Pts',(42.2879728741844,-6.5622758469631,-9.90888567138002));
#66242=CARTESIAN_POINT('Ctrl Pts',(42.2984698839692,-6.56859994441823,-9.81218564789262));
#66243=CARTESIAN_POINT('Ctrl Pts',(42.3044148978359,-6.57492404187336,-9.71510206467697));
#66244=CARTESIAN_POINT('Ctrl Pts',(42.3103536890481,-6.58124151988664,-9.6181200989866));
#66245=CARTESIAN_POINT('Ctrl Pts',(42.3117499299689,-6.58755899789992,-9.52075580591713));
#66246=CARTESIAN_POINT('Ctrl Pts',(42.3085723305793,-6.59387647591321,-9.42346814068221));
#66247=CARTESIAN_POINT('Ctrl Pts',(42.3053969867545,-6.6001894695726,-9.3262495334352));
#66248=CARTESIAN_POINT('Ctrl Pts',(42.2976542714137,-6.60650246323199,-9.22910788172664));
#66249=CARTESIAN_POINT('Ctrl Pts',(42.2853649654746,-6.61281545689138,-9.13250327043195));
#66250=CARTESIAN_POINT('Ctrl Pts',(42.2730801005206,-6.61912616922502,-9.03593356913402));
#66251=CARTESIAN_POINT('Ctrl Pts',(42.2562519647596,-6.62543688155865,-8.93990095600729));
#66252=CARTESIAN_POINT('Ctrl Pts',(42.2349532150411,-6.63174759389229,-8.84486057649043));
#66253=CARTESIAN_POINT('Ctrl Pts',(42.2136563932548,-6.63805773498928,-8.74982879989265));
#66254=CARTESIAN_POINT('Ctrl Pts',(42.1878898579292,-6.64436787608626,-8.65578950501199));
#66255=CARTESIAN_POINT('Ctrl Pts',(42.1577772059652,-6.65067801718325,-8.56318678904235));
#66256=CARTESIAN_POINT('Ctrl Pts',(42.1276591238284,-6.65698929617926,-8.47056737415298));
#66257=CARTESIAN_POINT('Ctrl Pts',(42.0931935037355,-6.66330057517527,-8.37938546855403));
#66258=CARTESIAN_POINT('Ctrl Pts',(42.0545532105356,-6.66961185417127,-8.29006817146812));
#66259=CARTESIAN_POINT('Ctrl Pts',(42.01587159413,-6.67592988265748,-8.20065535551486));
#66260=CARTESIAN_POINT('Ctrl Pts',(41.9730065653444,-6.68224791114369,-8.11311153115883));
#66261=CARTESIAN_POINT('Ctrl Pts',(41.926178295457,-6.6885659396299,-8.02784184059294));
#66262=CARTESIAN_POINT('Ctrl Pts',(41.8793225857162,-6.6948876702767,-7.94252218474294));
#66263=CARTESIAN_POINT('Ctrl Pts',(41.8284992386597,-6.70120940092349,-7.85947968902788));
#66264=CARTESIAN_POINT('Ctrl Pts',(41.7739722480919,-6.70753113157029,-7.77909120543114));
#66265=CARTESIAN_POINT('Ctrl Pts',(41.7193578274659,-6.71386299865176,-7.69857382475574));
#66266=CARTESIAN_POINT('Ctrl Pts',(41.6610281671869,-6.72019486573324,-7.62071930347723));
#66267=CARTESIAN_POINT('Ctrl Pts',(41.5992880430821,-6.72652673281471,-7.54587202555684));
#66268=CARTESIAN_POINT('Ctrl Pts',(41.5634283632996,-6.73020438538277,-7.50239949520928));
#66269=CARTESIAN_POINT('Ctrl Pts',(41.5264188860586,-6.73388203795083,-7.45994078554279));
#66270=CARTESIAN_POINT('Ctrl Pts',(41.4883248062323,-6.73755969051889,-7.41855744581492));
#66271=CARTESIAN_POINT('Ctrl Pts',(41.4227298831058,-6.74389231066848,-7.34729868328411));
#66272=CARTESIAN_POINT('Ctrl Pts',(41.3536893424341,-6.75022493081807,-7.27898301710029));
#66273=CARTESIAN_POINT('Ctrl Pts',(41.281497643882,-6.75655755096766,-7.213961659467));
#66274=CARTESIAN_POINT('Ctrl Pts',(41.2094031038176,-6.76288164842269,-7.14902781018855));
#66275=CARTESIAN_POINT('Ctrl Pts',(41.134166157167,-6.76920574587772,-7.08737974764538));
#66276=CARTESIAN_POINT('Ctrl Pts',(41.0561198176812,-6.77552984333275,-7.0293337812698));
#66277=CARTESIAN_POINT('Ctrl Pts',(40.9781551694107,-6.78184732134592,-6.97134857169034));
#66278=CARTESIAN_POINT('Ctrl Pts',(40.8973873234095,-6.78816479935909,-6.91695822231062));
#66279=CARTESIAN_POINT('Ctrl Pts',(40.8141834965666,-6.79448227737226,-6.86643980840906));
#66280=CARTESIAN_POINT('Ctrl Pts',(40.7310387305391,-6.80079527103157,-6.81595725414076));
#66281=CARTESIAN_POINT('Ctrl Pts',(40.6454617940483,-6.80710826469087,-6.76934139763099));
#66282=CARTESIAN_POINT('Ctrl Pts',(40.5578493128993,-6.81342125835017,-6.72682632841368));
#66283=CARTESIAN_POINT('Ctrl Pts',(40.470268492262,-6.81973197068373,-6.68432662286175));
#66284=CARTESIAN_POINT('Ctrl Pts',(40.3806539816182,-6.82604268301728,-6.64592495077549));
#66285=CARTESIAN_POINT('Ctrl Pts',(40.2894266269451,-6.83235339535084,-6.61180926175386));
#66286=CARTESIAN_POINT('Ctrl Pts',(40.1982075300416,-6.83866353644774,-6.57769666083561));
#66287=CARTESIAN_POINT('Ctrl Pts',(40.1053762890547,-6.84497367754465,-6.54786942460858));
#66288=CARTESIAN_POINT('Ctrl Pts',(40.0113723431609,-6.85128381864155,-6.52246680723534));
#66289=CARTESIAN_POINT('Ctrl Pts',(39.9173514456657,-6.85759509763746,-6.49705960904328));
#66290=CARTESIAN_POINT('Ctrl Pts',(39.8221578454268,-6.86390637663337,-6.47607872845315));
#66291=CARTESIAN_POINT('Ctrl Pts',(39.7262436786258,-6.87021765562928,-6.45961287214707));
#66292=CARTESIAN_POINT('Ctrl Pts',(39.6302269380468,-6.8765356841154,-6.44312940671043));
#66293=CARTESIAN_POINT('Ctrl Pts',(39.5334885241675,-6.88285371260151,-6.43117067953997));
#66294=CARTESIAN_POINT('Ctrl Pts',(39.4364880453472,-6.88917174108763,-6.42377378166186));
#66295=CARTESIAN_POINT('Ctrl Pts',(39.3394307273799,-6.89549347173433,-6.41637254944056));
#66296=CARTESIAN_POINT('Ctrl Pts',(39.2421114756232,-6.90181520238103,-6.41353848207697));
#66297=CARTESIAN_POINT('Ctrl Pts',(39.1449901629594,-6.90813693302774,-6.41525651046123));
#66298=CARTESIAN_POINT('Ctrl Pts',(39.047713123344,-6.91446880010912,-6.41697729357889));
#66299=CARTESIAN_POINT('Ctrl Pts',(38.9506350926986,-6.92080066719052,-6.42326471892864));
#66300=CARTESIAN_POINT('Ctrl Pts',(38.8542110480094,-6.9271325342719,-6.43405181965449));
#66301=CARTESIAN_POINT('Ctrl Pts',(38.7982063765427,-6.93081018684089,-6.44031714521905));
#66302=CARTESIAN_POINT('Ctrl Pts',(38.7424221587324,-6.93448783940988,-6.44809946345234));
#66303=CARTESIAN_POINT('Ctrl Pts',(38.6869455715382,-6.93816549197887,-6.4573778253612));
#66304=CARTESIAN_POINT('Ctrl Pts',(38.5914193772331,-6.94449811212838,-6.47335441381708));
#66305=CARTESIAN_POINT('Ctrl Pts',(38.4964742376763,-6.95083073227788,-6.49382505075428));
#66306=CARTESIAN_POINT('Ctrl Pts',(38.402565208688,-6.95716335242738,-6.51873514032692));
#66307=CARTESIAN_POINT('Ctrl Pts',(38.3087825662435,-6.9634874498823,-6.54361170490033));
#66308=CARTESIAN_POINT('Ctrl Pts',(38.21603368198,-6.96981154733722,-6.57291573575188));
#66309=CARTESIAN_POINT('Ctrl Pts',(38.1247654591753,-6.97613564479213,-6.6065412740425));
#66310=CARTESIAN_POINT('Ctrl Pts',(38.0335927669488,-6.98245312280528,-6.64013161643452));
#66311=CARTESIAN_POINT('Ctrl Pts',(37.9438980632769,-6.98877060081842,-6.67803432328299));
#66312=CARTESIAN_POINT('Ctrl Pts',(37.8561140935644,-6.99508807883156,-6.72009334854371));
#66313=CARTESIAN_POINT('Ctrl Pts',(37.7683924358044,-7.00140107249077,-6.76212251892326));
#66314=CARTESIAN_POINT('Ctrl Pts',(37.6825792088593,-7.00771406614998,-6.80830195393796));
#66315=CARTESIAN_POINT('Ctrl Pts',(37.5990872381363,-7.01402705980919,-6.85842748424088));
#66316=CARTESIAN_POINT('Ctrl Pts',(37.5156254388967,-7.02033777214265,-6.90853490068697));
#66317=CARTESIAN_POINT('Ctrl Pts',(37.4344836036633,-7.0266484844761,-6.96258535407638));
#66318=CARTESIAN_POINT('Ctrl Pts',(37.3560491603192,-7.03295919680955,-7.02032917257765));
#66319=CARTESIAN_POINT('Ctrl Pts',(37.2776218167489,-7.03926933790634,-7.07806776419099));
#66320=CARTESIAN_POINT('Ctrl Pts',(37.2019017298573,-7.04557947900313,-7.13949879677973));
#66321=CARTESIAN_POINT('Ctrl Pts',(37.1292457142642,-7.05188962009993,-7.20433041106518));
#66322=CARTESIAN_POINT('Ctrl Pts',(37.0565765967122,-7.05820089909575,-7.26917371634608));
#66323=CARTESIAN_POINT('Ctrl Pts',(36.9869729741417,-7.06451217809156,-7.33741853007999));
#66324=CARTESIAN_POINT('Ctrl Pts',(36.9207562740704,-7.07082345708738,-7.40873473054285));
#66325=CARTESIAN_POINT('Ctrl Pts',(36.8544687596731,-7.0771414855734,-7.48012719890586));
#66326=CARTESIAN_POINT('Ctrl Pts',(36.7915756971201,-7.08345951405943,-7.55459729060612));
#66327=CARTESIAN_POINT('Ctrl Pts',(36.7323593763675,-7.08977754254545,-7.6317804127628));
#66328=CARTESIAN_POINT('Ctrl Pts',(36.6731083567639,-7.09609927319207,-7.70900876173575));
#66329=CARTESIAN_POINT('Ctrl Pts',(36.6175386185544,-7.10242100383869,-7.78895294786212));
#66330=CARTESIAN_POINT('Ctrl Pts',(36.5658889183557,-7.1087427344853,-7.87121964503795));
#66331=CARTESIAN_POINT('Ctrl Pts',(36.5141564016244,-7.11507460156659,-7.95361825087106));
#66332=CARTESIAN_POINT('Ctrl Pts',(36.4663566886759,-7.12140646864787,-8.03834642324154));
#66333=CARTESIAN_POINT('Ctrl Pts',(36.4226824017246,-7.12773833572916,-8.12498656748948));
#66334=CARTESIAN_POINT('Ctrl Pts',(36.3973156573532,-7.13141598829906,-8.17530858863417));
#66335=CARTESIAN_POINT('Ctrl Pts',(36.3733397187133,-7.13509364086896,-8.22627522283438));
#66336=CARTESIAN_POINT('Ctrl Pts',(36.3507846960796,-7.13877129343886,-8.27780201860111));
#66337=CARTESIAN_POINT('Ctrl Pts',(36.3081456435135,-7.14572369706949,-8.37521064411829));
#66338=CARTESIAN_POINT('Ctrl Pts',(36.2704600196826,-7.15267610070013,-8.47491220946225));
#66339=CARTESIAN_POINT('Ctrl Pts',(36.2379556849738,-7.15962850433076,-8.57640939878109));
#66340=CARTESIAN_POINT('Ctrl Pts',(36.205535236877,-7.16656296532109,-8.67764464594909));
#66341=CARTESIAN_POINT('Ctrl Pts',(36.1782695210843,-7.17349742631141,-8.78066600847023));
#66342=CARTESIAN_POINT('Ctrl Pts',(36.1563385086826,-7.18043188730174,-8.8849567364844));
#66343=CARTESIAN_POINT('Ctrl Pts',(36.1343381803525,-7.18738826559314,-8.98957708943827));
#66344=CARTESIAN_POINT('Ctrl Pts',(36.1177065160083,-7.19434464388455,-9.09547459308052));
#66345=CARTESIAN_POINT('Ctrl Pts',(36.1065761150675,-7.20130102217595,-9.20210788020016));
#66346=CARTESIAN_POINT('Ctrl Pts',(36.0954457141266,-7.20825740046736,-9.30874116731979));
#66347=CARTESIAN_POINT('Ctrl Pts',(36.0898167210575,-7.21521377875877,-9.41610995679598));
#66348=CARTESIAN_POINT('Ctrl Pts',(36.0897702898568,-7.22217015705017,-9.52365722578337));
#66349=CARTESIAN_POINT('',(36.0897712258121,-8.49217015713119,-9.52776136080223));
#66350=CARTESIAN_POINT('Ctrl Pts',(36.0897702898566,-7.22217015708685,-9.52365722635048));
#66351=CARTESIAN_POINT('Ctrl Pts',(36.0897274329479,-7.228591033366,-9.62292550639579));
#66352=CARTESIAN_POINT('Ctrl Pts',(36.0944413978688,-7.23501190964515,-9.7221767087338));
#66353=CARTESIAN_POINT('Ctrl Pts',(36.1038809221781,-7.2414327859243,-9.82093463610625));
#66354=CARTESIAN_POINT('Ctrl Pts',(36.113324596391,-7.24785648501707,-9.91973598048454));
#66355=CARTESIAN_POINT('Ctrl Pts',(36.1274979248913,-7.25428018410984,-10.0180432047192));
#66356=CARTESIAN_POINT('Ctrl Pts',(36.1463179296204,-7.26070388320261,-10.1153867088123));
#66357=CARTESIAN_POINT('Ctrl Pts',(36.1655258423147,-7.26725998417729,-10.2147366056314));
#66358=CARTESIAN_POINT('Ctrl Pts',(36.1895740108885,-7.27381608515198,-10.3130821696095));
#66359=CARTESIAN_POINT('Ctrl Pts',(36.2183201842394,-7.28037218612667,-10.4099384889276));
#66360=CARTESIAN_POINT('Ctrl Pts',(36.2465490334199,-7.28681030167575,-10.5050517548516));
#66361=CARTESIAN_POINT('Ctrl Pts',(36.2793079921364,-7.29324841722484,-10.5987285623426));
#66362=CARTESIAN_POINT('Ctrl Pts',(36.3164133193158,-7.29968653277392,-10.6905292822921));
#66363=CARTESIAN_POINT('Ctrl Pts',(36.3545386393298,-7.30630162646141,-10.7848535233554));
#66364=CARTESIAN_POINT('Ctrl Pts',(36.3972525535177,-7.31291672014889,-10.8771966020305));
#66365=CARTESIAN_POINT('Ctrl Pts',(36.4443055470847,-7.31953181383638,-10.9671091273103));
#66366=CARTESIAN_POINT('Ctrl Pts',(36.4913585406517,-7.32614690752387,-11.0570216525902));
#66367=CARTESIAN_POINT('Ctrl Pts',(36.542750316339,-7.33276200121135,-11.1445032562025));
#66368=CARTESIAN_POINT('Ctrl Pts',(36.5981845410128,-7.33937709489884,-11.2291381898999));
#66369=CARTESIAN_POINT('Ctrl Pts',(36.6512516485568,-7.34570971504808,-11.310159096297));
#66370=CARTESIAN_POINT('Ctrl Pts',(36.7081990392816,-7.35204233519732,-11.3888395970014));
#66371=CARTESIAN_POINT('Ctrl Pts',(36.7687936114938,-7.35837495534656,-11.4647850781431));
#66372=CARTESIAN_POINT('Ctrl Pts',(36.8293066330968,-7.36469905280125,-11.5406283488058));
#66373=CARTESIAN_POINT('Ctrl Pts',(36.8934568098284,-7.37102315025593,-11.6137435769121));
#66374=CARTESIAN_POINT('Ctrl Pts',(36.9609673000875,-7.37734724771062,-11.6837642811624));
#66375=CARTESIAN_POINT('Ctrl Pts',(37.0284071270201,-7.38366472572347,-11.7537116946416));
#66376=CARTESIAN_POINT('Ctrl Pts',(37.09919997309,-7.38998220373633,-11.8205707104724));
#66377=CARTESIAN_POINT('Ctrl Pts',(37.1730288413559,-7.39629968174919,-11.8840079641504));
#66378=CARTESIAN_POINT('Ctrl Pts',(37.2468053034605,-7.40261267540816,-11.9474001879773));
#66379=CARTESIAN_POINT('Ctrl Pts',(37.3236131726091,-7.40892566906713,-12.0073751942156));
#66380=CARTESIAN_POINT('Ctrl Pts',(37.4030994131577,-7.4152386627261,-12.0636372198299));
#66381=CARTESIAN_POINT('Ctrl Pts',(37.4825569297732,-7.42154937505932,-12.1198789140429));
#66382=CARTESIAN_POINT('Ctrl Pts',(37.5646905380128,-7.42786008739254,-12.1724100413258));
#66383=CARTESIAN_POINT('Ctrl Pts',(37.649115767018,-7.43417079972576,-12.2209763998945));
#66384=CARTESIAN_POINT('Ctrl Pts',(37.7335333539723,-7.44048094082234,-12.2695383623059));
#66385=CARTESIAN_POINT('Ctrl Pts',(37.8202417700958,-7.44679108191891,-12.3141360516697));
#66386=CARTESIAN_POINT('Ctrl Pts',(37.9088302429844,-7.45310122301548,-12.3545602682163));
#66387=CARTESIAN_POINT('Ctrl Pts',(37.9974346909096,-7.45941250201106,-12.3949917744059));
#66388=CARTESIAN_POINT('Ctrl Pts',(38.0879194710936,-7.46572378100665,-12.4312481315165));
#66389=CARTESIAN_POINT('Ctrl Pts',(38.1798530238244,-7.47203506000223,-12.4631679325559));
#66390=CARTESIAN_POINT('Ctrl Pts',(38.2718848933332,-7.47835308848803,-12.4951218696848));
#66391=CARTESIAN_POINT('Ctrl Pts',(38.3653682148109,-7.48467111697383,-12.5227298482419));
#66392=CARTESIAN_POINT('Ctrl Pts',(38.4598556212435,-7.49098914545963,-12.5458801617236));
#66393=CARTESIAN_POINT('Ctrl Pts',(38.5543983942439,-7.49731087610601,-12.5690440405411));
#66394=CARTESIAN_POINT('Ctrl Pts',(38.6499459948069,-7.50363260675241,-12.5877449690213));
#66395=CARTESIAN_POINT('Ctrl Pts',(38.746042270378,-7.50995433739879,-12.6019226562617));
#66396=CARTESIAN_POINT('Ctrl Pts',(38.8422926293284,-7.51628620447987,-12.616123076391));
#66397=CARTESIAN_POINT('Ctrl Pts',(38.9390929851383,-7.52261807156095,-12.6257857295259));
#66398=CARTESIAN_POINT('Ctrl Pts',(39.0359835336316,-7.52894993864204,-12.6309023248744));
#66399=CARTESIAN_POINT('Ctrl Pts',(39.092259158235,-7.53262759121429,-12.6338741276308));
#66400=CARTESIAN_POINT('Ctrl Pts',(39.148565216592,-7.53630524378655,-12.6353133050688));
#66401=CARTESIAN_POINT('Ctrl Pts',(39.2048122801432,-7.53998289635881,-12.6352262771155));
#66402=CARTESIAN_POINT('Ctrl Pts',(39.3016651722967,-7.54631551650768,-12.635076422022));
#66403=CARTESIAN_POINT('Ctrl Pts',(39.3986792881586,-7.55264813665654,-12.6303979795902));
#66404=CARTESIAN_POINT('Ctrl Pts',(39.495396767583,-7.5589807568054,-12.621170441465));
#66405=CARTESIAN_POINT('Ctrl Pts',(39.5919840807385,-7.5653048542597,-12.6119553221313));
#66406=CARTESIAN_POINT('Ctrl Pts',(39.6882751192754,-7.57162895171399,-12.598203316755));
#66407=CARTESIAN_POINT('Ctrl Pts',(39.7838116716812,-7.57795304916828,-12.579945921765));
#66408=CARTESIAN_POINT('Ctrl Pts',(39.8792482258414,-7.58427052718075,-12.5617076368164));
#66409=CARTESIAN_POINT('Ctrl Pts',(39.9739314365919,-7.59058800519322,-12.5389734191424));
#66410=CARTESIAN_POINT('Ctrl Pts',(40.0674088741442,-7.5969054832057,-12.5118264927772));
#66411=CARTESIAN_POINT('Ctrl Pts',(40.1608199583334,-7.60321847686426,-12.4846988361942));
#66412=CARTESIAN_POINT('Ctrl Pts',(40.253026552129,-7.60953147052282,-12.4531648197075));
#66413=CARTESIAN_POINT('Ctrl Pts',(40.3435880130806,-7.61584446418138,-12.4173583991681));
#66414=CARTESIAN_POINT('Ctrl Pts',(40.4341167478479,-7.62215517651418,-12.3815649179906));
#66415=CARTESIAN_POINT('Ctrl Pts',(40.5230011247852,-7.62846588884698,-12.3415022611731));
#66416=CARTESIAN_POINT('Ctrl Pts',(40.6098181209827,-7.63477660117978,-12.2973534259991));
#66417=CARTESIAN_POINT('Ctrl Pts',(40.6966272586301,-7.64108674227594,-12.2532085871144));
#66418=CARTESIAN_POINT('Ctrl Pts',(40.781368997898,-7.64739688337209,-12.2049785036821));
#66419=CARTESIAN_POINT('Ctrl Pts',(40.863643622809,-7.65370702446825,-12.152892796365));
#66420=CARTESIAN_POINT('Ctrl Pts',(40.9459330841891,-7.66001830346341,-12.1007976965044));
#66421=CARTESIAN_POINT('Ctrl Pts',(41.0257541781318,-7.66632958245858,-12.0448458257896));
#66422=CARTESIAN_POINT('Ctrl Pts',(41.1027358467116,-7.67264086145374,-11.9853103362256));
#66423=CARTESIAN_POINT('Ctrl Pts',(41.1797998420304,-7.67895888993911,-11.9257111774428));
#66424=CARTESIAN_POINT('Ctrl Pts',(41.254018003129,-7.68527691842448,-11.8625210165279));
#66425=CARTESIAN_POINT('Ctrl Pts',(41.3250522497817,-7.69159494690984,-11.7960534094552));
#66426=CARTESIAN_POINT('Ctrl Pts',(41.3961281202081,-7.6979166775558,-11.729546854512));
#66427=CARTESIAN_POINT('Ctrl Pts',(41.4640160563314,-7.70423840820175,-11.6597593425411));
#66428=CARTESIAN_POINT('Ctrl Pts',(41.5284162300564,-7.7105601388477,-11.5870398911054));
#66429=CARTESIAN_POINT('Ctrl Pts',(41.5929196647699,-7.71689200592834,-11.5142038393253));
#66430=CARTESIAN_POINT('Ctrl Pts',(41.6539238960357,-7.72322387300899,-11.4384268011343));
#66431=CARTESIAN_POINT('Ctrl Pts',(41.7111706436439,-7.72955574008963,-11.3600892761391));
#66432=CARTESIAN_POINT('Ctrl Pts',(41.7444204965151,-7.73323339266602,-11.3145895527626));
#66433=CARTESIAN_POINT('Ctrl Pts',(41.7764035929619,-7.7369110452424,-11.2682265827518));
#66434=CARTESIAN_POINT('Ctrl Pts',(41.8070764255713,-7.74058869781879,-11.2210787611814));
#66435=CARTESIAN_POINT('Ctrl Pts',(41.8598925613776,-7.74692131797149,-11.1398940274875));
#66436=CARTESIAN_POINT('Ctrl Pts',(41.9090046698514,-7.7532539381242,-11.0560988765982));
#66437=CARTESIAN_POINT('Ctrl Pts',(41.9541453026649,-7.7595865582769,-10.9700655018749));
#66438=CARTESIAN_POINT('Ctrl Pts',(41.9992251834015,-7.76591065573503,-10.8841479143231));
#66439=CARTESIAN_POINT('Ctrl Pts',(42.0403440103906,-7.77223475319315,-10.7959984739827));
#66440=CARTESIAN_POINT('Ctrl Pts',(42.0772776910847,-7.77855885065128,-10.7060180952409));
#66441=CARTESIAN_POINT('Ctrl Pts',(42.1141727132427,-7.78487632866761,-10.6161318990894));
#66442=CARTESIAN_POINT('Ctrl Pts',(42.1468911327621,-7.79119380668394,-10.5244189769566));
#66443=CARTESIAN_POINT('Ctrl Pts',(42.1752553332348,-7.79751128470027,-10.4313036770077));
#66444=CARTESIAN_POINT('Ctrl Pts',(42.2035993998641,-7.80382427836268,-10.3382544733648));
#66445=CARTESIAN_POINT('Ctrl Pts',(42.2275952650091,-7.8101372720251,-10.2438052880763));
#66446=CARTESIAN_POINT('Ctrl Pts',(42.2471142373284,-7.81645026568751,-10.1483983297787));
#66447=CARTESIAN_POINT('Ctrl Pts',(42.2666261560789,-7.82276097802417,-10.053025848682));
#66448=CARTESIAN_POINT('Ctrl Pts',(42.2816643090541,-7.82907169036082,-9.9566967103053));
#66449=CARTESIAN_POINT('Ctrl Pts',(42.2921507024747,-7.83538240269748,-9.85986517598162));
#66450=CARTESIAN_POINT('Ctrl Pts',(42.3026361466819,-7.84169254379746,-9.76304240671011));
#66451=CARTESIAN_POINT('Ctrl Pts',(42.3085706036467,-7.84800268489745,-9.66571776670031));
#66452=CARTESIAN_POINT('Ctrl Pts',(42.3099278611548,-7.85431282599744,-9.56835148571194));
#66453=CARTESIAN_POINT('Ctrl Pts',(42.3112853634152,-7.86062410499642,-9.47096764679713));
#66454=CARTESIAN_POINT('Ctrl Pts',(42.3080640208104,-7.86693538399541,-9.37354258925499));
#66455=CARTESIAN_POINT('Ctrl Pts',(42.3002897384998,-7.87324666299439,-9.27653634017716));
#66456=CARTESIAN_POINT('Ctrl Pts',(42.2925071421151,-7.87956469148354,-9.17942634941327));
#66457=CARTESIAN_POINT('Ctrl Pts',(42.2801619201976,-7.8858827199727,-9.08273649793021));
#66458=CARTESIAN_POINT('Ctrl Pts',(42.263331837677,-7.89220074846185,-8.98692128347737));
#66459=CARTESIAN_POINT('Ctrl Pts',(42.2464918932718,-7.89852247911156,-8.89104992440469));
#66460=CARTESIAN_POINT('Ctrl Pts',(42.2251619509961,-7.90484420976127,-8.79605464940832));
#66461=CARTESIAN_POINT('Ctrl Pts',(42.1994703799956,-7.91116594041098,-8.70237730858601));
#66462=CARTESIAN_POINT('Ctrl Pts',(42.1737376144323,-7.91749780749531,-8.6085497629711));
#66463=CARTESIAN_POINT('Ctrl Pts',(42.1436293905051,-7.92382967457964,-8.51604478682144));
#66464=CARTESIAN_POINT('Ctrl Pts',(42.1093231507,-7.93016154166398,-8.42528664748446));
#66465=CARTESIAN_POINT('Ctrl Pts',(42.0893975224111,-7.93383919420225,-8.37257282752336));
#66466=CARTESIAN_POINT('Ctrl Pts',(42.0680565943838,-7.93751684674051,-8.32044789901571));
#66467=CARTESIAN_POINT('Ctrl Pts',(42.0453422312277,-7.94119449927878,-8.26899114649144));
#66468=CARTESIAN_POINT('Ctrl Pts',(42.0062299354827,-7.94752711942473,-8.18038678153596));
#66469=CARTESIAN_POINT('Ctrl Pts',(41.9629070333242,-7.95385973957068,-8.09345719715179));
#66470=CARTESIAN_POINT('Ctrl Pts',(41.9155390002746,-7.96019235971662,-8.00862979754696));
#66471=CARTESIAN_POINT('Ctrl Pts',(41.8682347170265,-7.96651645716803,-7.92391656206355));
#66472=CARTESIAN_POINT('Ctrl Pts',(41.8168963346975,-7.97284055461945,-7.84130026677639));
#66473=CARTESIAN_POINT('Ctrl Pts',(41.7617370783549,-7.97916465207086,-7.76118771002079));
#66474=CARTESIAN_POINT('Ctrl Pts',(41.7066355572845,-7.98548213008046,-7.68115900719233));
#66475=CARTESIAN_POINT('Ctrl Pts',(41.6477213597273,-7.99179960809007,-7.6036291911841));
#66476=CARTESIAN_POINT('Ctrl Pts',(41.5852527384994,-7.99811708609968,-7.52897895141828));
#66477=CARTESIAN_POINT('Ctrl Pts',(41.5228284595552,-8.00443007975542,-7.45438170085015));
#66478=CARTESIAN_POINT('Ctrl Pts',(41.4568550527625,-8.01074307341117,-7.38266029732104));
#66479=CARTESIAN_POINT('Ctrl Pts',(41.3876324703314,-8.01705606706692,-7.31416422417865));
#66480=CARTESIAN_POINT('Ctrl Pts',(41.3184349028563,-8.02336677939693,-7.24569290345364));
#66481=CARTESIAN_POINT('Ctrl Pts',(41.2459908033385,-8.02967749172695,-7.18044490445988));
#66482=CARTESIAN_POINT('Ctrl Pts',(41.1706379289395,-8.03598820405697,-7.11873384557626));
#66483=CARTESIAN_POINT('Ctrl Pts',(41.0952918753744,-8.04229834515037,-7.05702837268908));
#66484=CARTESIAN_POINT('Ctrl Pts',(41.0170379088886,-8.04860848624376,-6.99885948028117));
#66485=CARTESIAN_POINT('Ctrl Pts',(40.9362470892756,-8.05491862733716,-6.94450068826169));
#66486=CARTESIAN_POINT('Ctrl Pts',(40.855441700766,-8.06122990632957,-6.89013209379651));
#66487=CARTESIAN_POINT('Ctrl Pts',(40.772098913387,-8.06754118532197,-6.83957520841959));
#66488=CARTESIAN_POINT('Ctrl Pts',(40.6866181055634,-8.07385246431438,-6.79305979913337));
#66489=CARTESIAN_POINT('Ctrl Pts',(40.601045881739,-8.08017049279711,-6.74649464473128));
#66490=CARTESIAN_POINT('Ctrl Pts',(40.5133314574149,-8.08648852127983,-6.70397980460187));
#66491=CARTESIAN_POINT('Ctrl Pts',(40.4238979283777,-8.09280654976256,-6.66569859689246));
#66492=CARTESIAN_POINT('Ctrl Pts',(40.3344119941812,-8.0991282804059,-6.62739495763183));
#66493=CARTESIAN_POINT('Ctrl Pts',(40.2432053588737,-8.10545001104925,-6.59333004362667));
#66494=CARTESIAN_POINT('Ctrl Pts',(40.1507181885533,-8.11177174169259,-6.56363788454469));
#66495=CARTESIAN_POINT('Ctrl Pts',(40.0580827217895,-8.11810360877071,-6.5338981162476));
#66496=CARTESIAN_POINT('Ctrl Pts',(39.9641630419777,-8.12443547584883,-6.50854521729546));
#66497=CARTESIAN_POINT('Ctrl Pts',(39.8694114161616,-8.13076734292696,-6.48766251318487));
#66498=CARTESIAN_POINT('Ctrl Pts',(39.8143781125389,-8.13444499553089,-6.47553349496609));
#66499=CARTESIAN_POINT('Ctrl Pts',(39.7590643061235,-8.13812264813482,-6.46491152181761));
#66500=CARTESIAN_POINT('Ctrl Pts',(39.7035592723059,-8.14180030073875,-6.45580487551301));
#66501=CARTESIAN_POINT('Ctrl Pts',(39.6079840961829,-8.14813292088444,-6.44012396759189));
#66502=CARTESIAN_POINT('Ctrl Pts',(39.5115097532658,-8.15446554103013,-6.42888441029796));
#66503=CARTESIAN_POINT('Ctrl Pts',(39.4145845959796,-8.16079816117581,-6.42218126470974));
#66504=CARTESIAN_POINT('Ctrl Pts',(39.3177898844641,-8.16712225862689,-6.41548714048415));
#66505=CARTESIAN_POINT('Ctrl Pts',(39.2205459970585,-8.17344635607797,-6.41331732334219));
#66506=CARTESIAN_POINT('Ctrl Pts',(39.1233101320149,-8.17977045352904,-6.41571562621744));
#66507=CARTESIAN_POINT('Ctrl Pts',(39.0261760438908,-8.18608793153824,-6.41811141878562));
#66508=CARTESIAN_POINT('Ctrl Pts',(38.9290503963186,-8.19240540954744,-6.42506581487646));
#66509=CARTESIAN_POINT('Ctrl Pts',(38.8323931374479,-8.19872288755664,-6.43657065039451));
#66510=CARTESIAN_POINT('Ctrl Pts',(38.7358044890827,-8.2050358812119,-6.44806731940143));
#66511=CARTESIAN_POINT('Ctrl Pts',(38.6396840014497,-8.21134887486717,-6.46410795475885));
#66512=CARTESIAN_POINT('Ctrl Pts',(38.5444882849865,-8.21766186852243,-6.48463241623977));
#66513=CARTESIAN_POINT('Ctrl Pts',(38.4493269693882,-8.22397258085192,-6.50514946079845));
#66514=CARTESIAN_POINT('Ctrl Pts',(38.3550901879882,-8.23028329318141,-6.53014701981337));
#66515=CARTESIAN_POINT('Ctrl Pts',(38.2622251834637,-8.23659400551089,-6.55951369142086));
#66516=CARTESIAN_POINT('Ctrl Pts',(38.169368584947,-8.24290414660371,-6.58887770479914));
#66517=CARTESIAN_POINT('Ctrl Pts',(38.0778839333214,-8.24921428769652,-6.62260991239922));
#66518=CARTESIAN_POINT('Ctrl Pts',(37.9882030973958,-8.25552442878933,-6.66054910676779));
#66519=CARTESIAN_POINT('Ctrl Pts',(37.8985060894496,-8.26183570778113,-6.6984951426586));
#66520=CARTESIAN_POINT('Ctrl Pts',(37.8106139459859,-8.26814698677292,-6.74064950165813));
#66521=CARTESIAN_POINT('Ctrl Pts',(37.724937377438,-8.27445826576472,-6.78680334664938));
#66522=CARTESIAN_POINT('Ctrl Pts',(37.639169183538,-8.28077629424672,-6.83300655008687));
#66523=CARTESIAN_POINT('Ctrl Pts',(37.5556216805866,-8.28709432272872,-6.88321757093409));
#66524=CARTESIAN_POINT('Ctrl Pts',(37.4746796479639,-8.29341235121072,-6.9371823217719));
#66525=CARTESIAN_POINT('Ctrl Pts',(37.3936901859248,-8.29973408185332,-6.99117869421039));
#66526=CARTESIAN_POINT('Ctrl Pts',(37.3153095862391,-8.30605581249591,-7.0489329172736));
#66527=CARTESIAN_POINT('Ctrl Pts',(37.2398906859807,-8.3123775431385,-7.11014966716469));
#66528=CARTESIAN_POINT('Ctrl Pts',(37.1643508570083,-8.31870941021578,-7.17146457365599));
#66529=CARTESIAN_POINT('Ctrl Pts',(37.0917825361352,-8.32504127729307,-7.23625280210336));
#66530=CARTESIAN_POINT('Ctrl Pts',(37.0225027163061,-8.33137314437035,-7.3041811797435));
#66531=CARTESIAN_POINT('Ctrl Pts',(36.9822638567299,-8.33505079697982,-7.34363509945403));
#66532=CARTESIAN_POINT('Ctrl Pts',(36.9431336406883,-8.33872844958928,-7.38414768634009));
#66533=CARTESIAN_POINT('Ctrl Pts',(36.9051678028014,-8.34240610219874,-7.42564870981517));
#66534=CARTESIAN_POINT('Ctrl Pts',(36.840538557626,-8.34866657017196,-7.49629590135606));
#66535=CARTESIAN_POINT('Ctrl Pts',(36.7790497127769,-8.35492703814518,-7.57006721002526));
#66536=CARTESIAN_POINT('Ctrl Pts',(36.7210228966364,-8.3611875061184,-7.64664881507776));
#66537=CARTESIAN_POINT('Ctrl Pts',(36.663067628609,-8.36744025482145,-7.72313599362693));
#66538=CARTESIAN_POINT('Ctrl Pts',(36.6085661827415,-8.3736930035245,-7.80242623624781));
#66539=CARTESIAN_POINT('Ctrl Pts',(36.5578026363479,-8.37994575222754,-7.8841698002506));
#66540=CARTESIAN_POINT('Ctrl Pts',(36.5070871640247,-8.38619257945537,-7.96583595150082));
#66541=CARTESIAN_POINT('Ctrl Pts',(36.4601027966921,-8.3924394066832,-8.04995043222001));
#66542=CARTESIAN_POINT('Ctrl Pts',(36.4170919295187,-8.39868623391103,-8.13613235902414));
#66543=CARTESIAN_POINT('Ctrl Pts',(36.3741094987145,-8.40492893108761,-8.22225730717951));
#66544=CARTESIAN_POINT('Ctrl Pts',(36.335095548604,-8.41117162826419,-8.3104465863091));
#66545=CARTESIAN_POINT('Ctrl Pts',(36.3002472873748,-8.41741432544077,-8.40029343448054));
#66546=CARTESIAN_POINT('Ctrl Pts',(36.2654023210465,-8.42365643237072,-8.49013178763803));
#66547=CARTESIAN_POINT('Ctrl Pts',(36.2347224379543,-8.42989853930067,-8.58162698684104));
#66548=CARTESIAN_POINT('Ctrl Pts',(36.2083569558186,-8.43614064623061,-8.67435168894478));
#66549=CARTESIAN_POINT('Ctrl Pts',(36.1819945151201,-8.44238203309121,-8.76706569462549));
#66550=CARTESIAN_POINT('Ctrl Pts',(36.1599456030518,-8.4486234199518,-8.86100848840364));
#66551=CARTESIAN_POINT('Ctrl Pts',(36.1423093694155,-8.45486480681239,-8.9557384954734));
#66552=CARTESIAN_POINT('Ctrl Pts',(36.1246594966111,-8.46111102051567,-9.05054176299818));
#66553=CARTESIAN_POINT('Ctrl Pts',(36.1114291994719,-8.46735723421894,-9.14613301810445));
#66554=CARTESIAN_POINT('Ctrl Pts',(36.102666203883,-8.47360344792221,-9.24206182949071));
#66555=CARTESIAN_POINT('Ctrl Pts',(36.0939836110761,-8.47979235097709,-9.33711046888127));
#66556=CARTESIAN_POINT('Ctrl Pts',(36.0896866409204,-8.48598125403197,-9.4324900624374));
#66557=CARTESIAN_POINT('Ctrl Pts',(36.0897712258115,-8.49217015708684,-9.52776136011945));
#66558=CARTESIAN_POINT('',(36.089632242379,-9.76217020937298,-9.52362827152999));
#66559=CARTESIAN_POINT('Ctrl Pts',(36.0897712258121,-8.4921701571312,-9.52776136080225));
#66560=CARTESIAN_POINT('Ctrl Pts',(36.0898810476013,-8.50020559029366,-9.65145794128347));
#66561=CARTESIAN_POINT('Ctrl Pts',(36.0973737509533,-8.50824102345612,-9.77483167154566));
#66562=CARTESIAN_POINT('Ctrl Pts',(36.112112747417,-8.51627645661858,-9.89713299804683));
#66563=CARTESIAN_POINT('Ctrl Pts',(36.1271629019818,-8.52448152752612,-10.0220162539634));
#66564=CARTESIAN_POINT('Ctrl Pts',(36.1497685385396,-8.53268659843367,-10.1457816117599));
#66565=CARTESIAN_POINT('Ctrl Pts',(36.1797360223109,-8.54089166934121,-10.2676548040467));
#66566=CARTESIAN_POINT('Ctrl Pts',(36.1823172751409,-8.54159841411371,-10.2781523661675));
#66567=CARTESIAN_POINT('Ctrl Pts',(36.1849531182365,-8.54230515888621,-10.2886359026316));
#66568=CARTESIAN_POINT('Ctrl Pts',(36.1876434113821,-8.54301190365871,-10.2991049256466));
#66569=CARTESIAN_POINT('Ctrl Pts',(36.2117491496296,-8.54934452377532,-10.3929101412286));
#66570=CARTESIAN_POINT('Ctrl Pts',(36.2402825925639,-8.55567714389193,-10.4857512369077));
#66571=CARTESIAN_POINT('Ctrl Pts',(36.2731503405401,-8.56200976400854,-10.5771795112145));
#66572=CARTESIAN_POINT('Ctrl Pts',(36.3059738537809,-8.56833386143066,-10.6684847376775));
#66573=CARTESIAN_POINT('Ctrl Pts',(36.3431199314519,-8.57465795885278,-10.7583805138988));
#66574=CARTESIAN_POINT('Ctrl Pts',(36.3844446987308,-8.58098205627489,-10.8464306634837));
#66575=CARTESIAN_POINT('Ctrl Pts',(36.4257262113175,-8.58729953425532,-10.9343886508527));
#66576=CARTESIAN_POINT('Ctrl Pts',(36.4711775332836,-8.59361701223574,-11.0205044583357));
#66577=CARTESIAN_POINT('Ctrl Pts',(36.5206061004642,-8.59993449021616,-11.1043603084889));
#66578=CARTESIAN_POINT('Ctrl Pts',(36.5699995816227,-8.60624748384301,-11.1881566350026));
#66579=CARTESIAN_POINT('Ctrl Pts',(36.6233644739105,-8.61256047746985,-11.2696958177493));
#66580=CARTESIAN_POINT('Ctrl Pts',(36.6804619743907,-8.61887347109669,-11.3485840508211));
#66581=CARTESIAN_POINT('Ctrl Pts',(36.7375388415559,-8.62518418339798,-11.427443776064));
#66582=CARTESIAN_POINT('Ctrl Pts',(36.7983453805853,-8.63149489569927,-11.5036541012356));
#66583=CARTESIAN_POINT('Ctrl Pts',(36.8625996304447,-8.63780560800057,-11.5768504246906));
#66584=CARTESIAN_POINT('Ctrl Pts',(36.9268480641038,-8.64411574906545,-11.6500401225219));
#66585=CARTESIAN_POINT('Ctrl Pts',(36.9945432994472,-8.65042589013034,-11.720216032561));
#66586=CARTESIAN_POINT('Ctrl Pts',(37.0653639672428,-8.65673603119522,-11.7870476698236));
#66587=CARTESIAN_POINT('Ctrl Pts',(37.1361974060345,-8.66304731015939,-11.8538913587459));
#66588=CARTESIAN_POINT('Ctrl Pts',(37.2101570785947,-8.66935858912356,-11.9173892770119));
#66589=CARTESIAN_POINT('Ctrl Pts',(37.2868865272362,-8.67566986808774,-11.9772494761402));
#66590=CARTESIAN_POINT('Ctrl Pts',(37.3636980328925,-8.68198789654275,-12.0371736917487));
#66591=CARTESIAN_POINT('Ctrl Pts',(37.4432848829153,-8.68830592499776,-12.093452152018));
#66592=CARTESIAN_POINT('Ctrl Pts',(37.5252596299661,-8.69462395345278,-12.145834856659));
#66593=CARTESIAN_POINT('Ctrl Pts',(37.6072824115746,-8.70094568406868,-12.1982482558754));
#66594=CARTESIAN_POINT('Ctrl Pts',(37.6916954974715,-8.70726741468458,-12.2467611360026));
#66595=CARTESIAN_POINT('Ctrl Pts',(37.7780865442638,-8.71358914530048,-12.2911693327228));
#66596=CARTESIAN_POINT('Ctrl Pts',(37.8646161128191,-8.71992101235185,-12.3356487347581));
#66597=CARTESIAN_POINT('Ctrl Pts',(37.9531295775849,-8.72625287940321,-12.3760101298394));
#66598=CARTESIAN_POINT('Ctrl Pts',(38.0431943702978,-8.73258474645458,-12.4120973984245));
#66599=CARTESIAN_POINT('Ctrl Pts',(38.0955054883842,-8.73626239934262,-12.4330574796227));
#66600=CARTESIAN_POINT('Ctrl Pts',(38.1483396355488,-8.73994005223066,-12.4525766208612));
#66601=CARTESIAN_POINT('Ctrl Pts',(38.2016100902036,-8.7436177051187,-12.4706320613608));
#66602=CARTESIAN_POINT('Ctrl Pts',(38.293337494604,-8.74995032525292,-12.5017220661874));
#66603=CARTESIAN_POINT('Ctrl Pts',(38.3866778299206,-8.75628294538714,-12.5285773868489));
#66604=CARTESIAN_POINT('Ctrl Pts',(38.4812043078318,-8.76261556552136,-12.5510309657735));
#66605=CARTESIAN_POINT('Ctrl Pts',(38.575603568206,-8.76893966296063,-12.5734543257683));
#66606=CARTESIAN_POINT('Ctrl Pts',(38.6711853764568,-8.7752637603999,-12.5914876181216));
#66607=CARTESIAN_POINT('Ctrl Pts',(38.7675058418423,-8.78158785783918,-12.6050128986839));
#66608=CARTESIAN_POINT('Ctrl Pts',(38.8637254884537,-8.78790533583628,-12.618524022315));
#66609=CARTESIAN_POINT('Ctrl Pts',(38.9606818243439,-8.79422281383338,-12.6275364543537));
#66610=CARTESIAN_POINT('Ctrl Pts',(39.057919751197,-8.80054029183049,-12.6319830794197));
#66611=CARTESIAN_POINT('Ctrl Pts',(39.1550886553608,-8.80685328547324,-12.6364265481244));
#66612=CARTESIAN_POINT('Ctrl Pts',(39.2525383174916,-8.81316627911599,-12.636310633159));
#66613=CARTESIAN_POINT('Ctrl Pts',(39.3498084376071,-8.81947927275875,-12.6316200419301));
#66614=CARTESIAN_POINT('Ctrl Pts',(39.4470434072268,-8.82578998507547,-12.6269311457397));
#66615=CARTESIAN_POINT('Ctrl Pts',(39.544098527388,-8.8321006973922,-12.6176708791558));
#66616=CARTESIAN_POINT('Ctrl Pts',(39.6405143621856,-8.83841140970892,-12.6038760529791));
#66617=CARTESIAN_POINT('Ctrl Pts',(39.736921469556,-8.84472155078874,-12.5900824754909));
#66618=CARTESIAN_POINT('Ctrl Pts',(39.832688973743,-8.85103169186857,-12.5717552166475));
#66619=CARTESIAN_POINT('Ctrl Pts',(39.9273644662361,-8.85734183294839,-12.5489827357571));
#66620=CARTESIAN_POINT('Ctrl Pts',(40.0220570314264,-8.863653111927,-12.5262061483376));
#66621=CARTESIAN_POINT('Ctrl Pts',(40.1156567686407,-8.86996439090561,-12.4989828490951));
#66622=CARTESIAN_POINT('Ctrl Pts',(40.2077243591099,-8.87627566988422,-12.4674517445417));
#66623=CARTESIAN_POINT('Ctrl Pts',(40.2998904096979,-8.88259369835279,-12.4358869195848));
#66624=CARTESIAN_POINT('Ctrl Pts',(40.3905206279047,-8.88891172682137,-12.4000052337996));
#66625=CARTESIAN_POINT('Ctrl Pts',(40.479193882072,-8.89522975528994,-12.3599944735342));
#66626=CARTESIAN_POINT('Ctrl Pts',(40.5679190958995,-8.90155148591894,-12.3199602682569));
#66627=CARTESIAN_POINT('Ctrl Pts',(40.6546846727078,-8.90787321654794,-12.2757923689068));
#66628=CARTESIAN_POINT('Ctrl Pts',(40.7390942543784,-8.91419494717694,-12.2277244641361));
#66629=CARTESIAN_POINT('Ctrl Pts',(40.8236391806651,-8.92052681424055,-12.1795794859811));
#66630=CARTESIAN_POINT('Ctrl Pts',(40.9058201992784,-8.92685868130416,-12.1275222493807));
#66631=CARTESIAN_POINT('Ctrl Pts',(40.9852701286095,-8.93319054836777,-12.0718296411018));
#66632=CARTESIAN_POINT('Ctrl Pts',(41.0314159568653,-8.93686820110474,-12.0394824564234));
#66633=CARTESIAN_POINT('Ctrl Pts',(41.0766410663143,-8.94054585384171,-12.00590965195));
#66634=CARTESIAN_POINT('Ctrl Pts',(41.1208789938497,-8.94422350657868,-11.971171405255));
#66635=CARTESIAN_POINT('Ctrl Pts',(41.197053124029,-8.95055612688772,-11.9113549564886));
#66636=CARTESIAN_POINT('Ctrl Pts',(41.270562866356,-8.95688874719677,-11.8478731106357));
#66637=CARTESIAN_POINT('Ctrl Pts',(41.3410350393383,-8.96322136750582,-11.7809919355409));
#66638=CARTESIAN_POINT('Ctrl Pts',(41.4114123680475,-8.9695454651208,-11.7142007718104));
#66639=CARTESIAN_POINT('Ctrl Pts',(41.4787599381421,-8.97586956273577,-11.6440196702687));
#66640=CARTESIAN_POINT('Ctrl Pts',(41.5427363462967,-8.98219366035075,-11.5707558663341));
#66641=CARTESIAN_POINT('Ctrl Pts',(41.6066457902582,-8.98851113852419,-11.4975687477223));
#66642=CARTESIAN_POINT('Ctrl Pts',(41.6671908011738,-8.99482861669763,-11.4213056691599));
#66643=CARTESIAN_POINT('Ctrl Pts',(41.7240664125183,-9.00114609487107,-11.3423110350451));
#66644=CARTESIAN_POINT('Ctrl Pts',(41.7809016516801,-9.00745908869036,-11.2633724739242));
#66645=CARTESIAN_POINT('Ctrl Pts',(41.8340724146941,-9.01377208250966,-11.1817065658849));
#66646=CARTESIAN_POINT('Ctrl Pts',(41.8833142871499,-9.02008507632895,-11.0976903984184));
#66647=CARTESIAN_POINT('Ctrl Pts',(41.9325383650749,-9.02639578882227,-11.0137045918662));
#66648=CARTESIAN_POINT('Ctrl Pts',(41.9778361526619,-9.0327065013156,-10.927370590385));
#66649=CARTESIAN_POINT('Ctrl Pts',(42.01898733824,-9.03901721380892,-10.8390932386032));
#66650=CARTESIAN_POINT('Ctrl Pts',(42.0601347988691,-9.04532735506519,-10.7508238775664));
#66651=CARTESIAN_POINT('Ctrl Pts',(42.0971362191833,-9.05163749632146,-10.6606119124268));
#66652=CARTESIAN_POINT('Ctrl Pts',(42.1298183783233,-9.05794763757773,-10.5688845352523));
#66653=CARTESIAN_POINT('Ctrl Pts',(42.1625064309886,-9.0642589167324,-10.477140617016));
#66654=CARTESIAN_POINT('Ctrl Pts',(42.1908735287742,-9.07057019588707,-10.3838811559448));
#66655=CARTESIAN_POINT('Ctrl Pts',(42.2147958494762,-9.07688147504175,-10.2895499583944));
#66656=CARTESIAN_POINT('Ctrl Pts',(42.2387437534904,-9.08319950368475,-10.1951178799764));
#66657=CARTESIAN_POINT('Ctrl Pts',(42.2582372828619,-9.08951753232775,-10.0996122014463));
#66658=CARTESIAN_POINT('Ctrl Pts',(42.2732034878762,-9.09583556097075,-10.0034882182518));
#66659=CARTESIAN_POINT('Ctrl Pts',(42.2881784626009,-9.10215729177351,-9.90730790952249));
#66660=CARTESIAN_POINT('Ctrl Pts',(42.2986207835065,-9.10847902257626,-9.81050900927613));
#66661=CARTESIAN_POINT('Ctrl Pts',(42.3045094803033,-9.11480075337901,-9.71355115912394));
#66662=CARTESIAN_POINT('Ctrl Pts',(42.3104076191937,-9.1211326206136,-9.61643784416791));
#66663=CARTESIAN_POINT('Ctrl Pts',(42.3117375483811,-9.12746448784819,-9.51916550738235));
#66664=CARTESIAN_POINT('Ctrl Pts',(42.3085304193097,-9.13379635508278,-9.42219297141593));
#66665=CARTESIAN_POINT('Ctrl Pts',(42.3066676668305,-9.13747400606808,-9.36586975280906));
#66666=CARTESIAN_POINT('Ctrl Pts',(42.3032753221632,-9.14115165705338,-9.30964758006777));
#66667=CARTESIAN_POINT('Ctrl Pts',(42.2983674468807,-9.14482930803867,-9.25361500223825));
#66668=CARTESIAN_POINT('Ctrl Pts',(42.2899164794979,-9.15116192790624,-9.15713139979396));
#66669=CARTESIAN_POINT('Ctrl Pts',(42.2769397722392,-9.1574945477738,-9.06087533093716));
#66670=CARTESIAN_POINT('Ctrl Pts',(42.2594561373029,-9.16382716764137,-8.96530472860719));
#66671=CARTESIAN_POINT('Ctrl Pts',(42.2419960325448,-9.17015126481474,-8.86986274903271));
#66672=CARTESIAN_POINT('Ctrl Pts',(42.2200411338116,-9.17647536198812,-8.77510482895813));
#66673=CARTESIAN_POINT('Ctrl Pts',(42.1936620968134,-9.1827994591615,-8.68148479385209));
#66674=CARTESIAN_POINT('Ctrl Pts',(42.1673106707889,-9.18911693689381,-8.58796275096358));
#66675=CARTESIAN_POINT('Ctrl Pts',(42.1365444306355,-9.19543441462612,-8.49557664393902));
#66676=CARTESIAN_POINT('Ctrl Pts',(42.1014850737235,-9.20175189235842,-8.40477010401458));
#66677=CARTESIAN_POINT('Ctrl Pts',(42.0664506030861,-9.20806488573908,-8.31402802153248));
#66678=CARTESIAN_POINT('Ctrl Pts',(42.027129231155,-9.21437787911974,-8.22486368388727));
#66679=CARTESIAN_POINT('Ctrl Pts',(41.9836921900713,-9.2206908725004,-8.13770462992338));
#66680=CARTESIAN_POINT('Ctrl Pts',(41.9402708458164,-9.2270015845568,-8.05057707259705));
#66681=CARTESIAN_POINT('Ctrl Pts',(41.8927369825086,-9.23331229661319,-7.96545375007072));
#66682=CARTESIAN_POINT('Ctrl Pts',(41.8413091829943,-9.23962300866959,-7.88274044294757));
#66683=CARTESIAN_POINT('Ctrl Pts',(41.7898860386361,-9.24593314949116,-7.80003462289102));
#66684=CARTESIAN_POINT('Ctrl Pts',(41.7345698899532,-9.25224329031274,-7.71973875577314));
#66685=CARTESIAN_POINT('Ctrl Pts',(41.6756237738523,-9.25855343113431,-7.64223140475594));
#66686=CARTESIAN_POINT('Ctrl Pts',(41.6166670280592,-9.26486470985705,-7.56471007691832));
#66687=CARTESIAN_POINT('Ctrl Pts',(41.554079279504,-9.27117598857979,-7.4899786119637));
#66688=CARTESIAN_POINT('Ctrl Pts',(41.488164479829,-9.27748726730253,-7.41838328921731));
#66689=CARTESIAN_POINT('Ctrl Pts',(41.4221791886356,-9.2838052955204,-7.34671140000888));
#66690=CARTESIAN_POINT('Ctrl Pts',(41.3528600395366,-9.29012332373827,-7.27818267113638));
#66691=CARTESIAN_POINT('Ctrl Pts',(41.2805484127911,-9.29644135195615,-7.21310706239831));
#66692=CARTESIAN_POINT('Ctrl Pts',(41.2081944137392,-9.302763082337,-7.14799332142959));
#66693=CARTESIAN_POINT('Ctrl Pts',(41.1328447836484,-9.30908481271785,-7.08633700659209));
#66694=CARTESIAN_POINT('Ctrl Pts',(41.0548729551091,-9.3154065430987,-7.02840692676906));
#66695=CARTESIAN_POINT('Ctrl Pts',(40.9767761043376,-9.3217384099206,-6.97038396021979));
#66696=CARTESIAN_POINT('Ctrl Pts',(40.8960490221214,-9.3280702767425,-6.91609940308681));
#66697=CARTESIAN_POINT('Ctrl Pts',(40.81309294599,-9.3344021435644,-6.86577797081605));
#66698=CARTESIAN_POINT('Ctrl Pts',(40.7649106543247,-9.33807979887582,-6.83655043210212));
#66699=CARTESIAN_POINT('Ctrl Pts',(40.7159768708064,-9.34175745418723,-6.80865898229115));
#66700=CARTESIAN_POINT('Ctrl Pts',(40.6663734313878,-9.34543510949864,-6.78214024918883));
#66701=CARTESIAN_POINT('Ctrl Pts',(40.5809603861182,-9.35176772964116,-6.73647717062995));
#66702=CARTESIAN_POINT('Ctrl Pts',(40.4932640181722,-9.35810034978367,-6.69472823736366));
#66703=CARTESIAN_POINT('Ctrl Pts',(40.4036780752508,-9.36443296992618,-6.65712801121451));
#66704=CARTESIAN_POINT('Ctrl Pts',(40.3142127007285,-9.37075706737141,-6.61957838897624));
#66705=CARTESIAN_POINT('Ctrl Pts',(40.2228632055255,-9.37708116481664,-6.58616654420512));
#66706=CARTESIAN_POINT('Ctrl Pts',(40.130048236466,-9.38340526226186,-6.55708138070693));
#66707=CARTESIAN_POINT('Ctrl Pts',(40.0373304170062,-9.3897227402626,-6.52802666070316));
#66708=CARTESIAN_POINT('Ctrl Pts',(39.9431505882964,-9.39604021826333,-6.50328974869088));
#66709=CARTESIAN_POINT('Ctrl Pts',(39.8479467610354,-9.40235769626406,-6.48301123477358));
#66710=CARTESIAN_POINT('Ctrl Pts',(39.7528105126443,-9.40867068990701,-6.46274711522564));
#66711=CARTESIAN_POINT('Ctrl Pts',(39.6566521372651,-9.41498368354997,-6.44693519296503));
#66712=CARTESIAN_POINT('Ctrl Pts',(39.5599232467678,-9.42129667719292,-6.43566578218929));
#66713=CARTESIAN_POINT('Ctrl Pts',(39.4632293112145,-9.42760738950773,-6.42440044384343));
#66714=CARTESIAN_POINT('Ctrl Pts',(39.365965704134,-9.43391810182253,-6.41767440580317));
#66715=CARTESIAN_POINT('Ctrl Pts',(39.268591700239,-9.44022881413734,-6.41552643819596));
#66716=CARTESIAN_POINT('Ctrl Pts',(39.1712265105358,-9.44653895521315,-6.4133786650205));
#66717=CARTESIAN_POINT('Ctrl Pts',(39.0737513810958,-9.45284909628896,-6.41580814778705));
#66718=CARTESIAN_POINT('Ctrl Pts',(38.9766270946817,-9.45915923736477,-6.42280155404758));
#66719=CARTESIAN_POINT('Ctrl Pts',(38.879485294015,-9.46547051633727,-6.4297962214168));
#66720=CARTESIAN_POINT('Ctrl Pts',(38.7826948982055,-9.47178179530978,-6.44135641542825));
#66721=CARTESIAN_POINT('Ctrl Pts',(38.6867120208982,-9.47809307428228,-6.4574168954355));
#66722=CARTESIAN_POINT('Ctrl Pts',(38.5906264963822,-9.48441110274165,-6.47349455104208));
#66723=CARTESIAN_POINT('Ctrl Pts',(38.4953506464988,-9.49072913120102,-6.49408202875086));
#66724=CARTESIAN_POINT('Ctrl Pts',(38.4013306307846,-9.49704715966039,-6.51906289294385));
#66725=CARTESIAN_POINT('Ctrl Pts',(38.307255522407,-9.50336889027841,-6.54405839510869));
#66726=CARTESIAN_POINT('Ctrl Pts',(38.2144381302551,-9.50969062089644,-6.5734522780838));
#66727=CARTESIAN_POINT('Ctrl Pts',(38.1233076752637,-9.51601235151446,-6.60707877235282));
#66728=CARTESIAN_POINT('Ctrl Pts',(38.0320310992633,-9.52234421856445,-6.64075918424217));
#66729=CARTESIAN_POINT('Ctrl Pts',(37.9424472640501,-9.52867608561444,-6.67868558885452));
#66730=CARTESIAN_POINT('Ctrl Pts',(37.8549636662382,-9.53500795266442,-6.72064483102433));
#66731=CARTESIAN_POINT('Ctrl Pts',(37.8041517504443,-9.53868560542916,-6.74501545058311));
#66732=CARTESIAN_POINT('Ctrl Pts',(37.7540478701526,-9.54236325819389,-6.77074568509546));
#66733=CARTESIAN_POINT('Ctrl Pts',(37.7047274297335,-9.54604091095863,-6.79778702820835));
#66734=CARTESIAN_POINT('Ctrl Pts',(37.6198016118814,-9.55237353220384,-6.84435003859853));
#66735=CARTESIAN_POINT('Ctrl Pts',(37.5369053206938,-9.55870615344906,-6.89496460821624));
#66736=CARTESIAN_POINT('Ctrl Pts',(37.456450203917,-9.56503877469427,-6.94942923578501));
#66737=CARTESIAN_POINT('Ctrl Pts',(37.3761033667938,-9.57136287324929,-7.00382056272055));
#66738=CARTESIAN_POINT('Ctrl Pts',(37.2981915332185,-9.57768697180431,-7.06205140593578));
#66739=CARTESIAN_POINT('Ctrl Pts',(37.2231017280754,-9.58401107035933,-7.12387445655967));
#66740=CARTESIAN_POINT('Ctrl Pts',(37.1480905194909,-9.59032854947539,-7.18563279694752));
#66741=CARTESIAN_POINT('Ctrl Pts',(37.0758958028394,-9.59664602859145,-7.25097559324891));
#66742=CARTESIAN_POINT('Ctrl Pts',(37.0068747306551,-9.6029635077075,-7.31961291246618));
#66743=CARTESIAN_POINT('Ctrl Pts',(36.9379026518954,-9.60927650246933,-7.38820151065927));
#66744=CARTESIAN_POINT('Ctrl Pts',(36.8721000481953,-9.61558949723116,-7.46007967508075));
#66745=CARTESIAN_POINT('Ctrl Pts',(36.809789406625,-9.62190249199298,-7.53491860161005));
#66746=CARTESIAN_POINT('Ctrl Pts',(36.7475012822458,-9.62821320542843,-7.60973048360285));
#66747=CARTESIAN_POINT('Ctrl Pts',(36.6887028921384,-9.63452391886388,-7.68750066600639));
#66748=CARTESIAN_POINT('Ctrl Pts',(36.6336777499718,-9.64083463229933,-7.76786575301988));
#66749=CARTESIAN_POINT('Ctrl Pts',(36.5786575886188,-9.64714477449615,-7.84822356547685));
#66750=CARTESIAN_POINT('Ctrl Pts',(36.5274102430144,-9.65345491669297,-7.93117545457953));
#66751=CARTESIAN_POINT('Ctrl Pts',(36.4801764214208,-9.6597650588898,-8.01632828146589));
#66752=CARTESIAN_POINT('Ctrl Pts',(36.4329340822439,-9.66607633898231,-8.10149646379606));
#66753=CARTESIAN_POINT('Ctrl Pts',(36.3897069166311,-9.67238761907482,-8.18886598975324));
#66754=CARTESIAN_POINT('Ctrl Pts',(36.3506896136501,-9.67869889916732,-8.27801925630812));
#66755=CARTESIAN_POINT('Ctrl Pts',(36.3116305843562,-9.68501692873832,-8.36726786612877));
#66756=CARTESIAN_POINT('Ctrl Pts',(36.2767905816254,-9.69133495830932,-8.45830362365475));
#66757=CARTESIAN_POINT('Ctrl Pts',(36.2463159836989,-9.69765298788032,-8.55068927710535));
#66758=CARTESIAN_POINT('Ctrl Pts',(36.21582352867,-9.70397471960686,-8.64312906548131));
#66759=CARTESIAN_POINT('Ctrl Pts',(36.1897016893659,-9.71029645133341,-8.73691990377445));
#66760=CARTESIAN_POINT('Ctrl Pts',(36.1680462737751,-9.71661818305996,-8.83161175743245));
#66761=CARTESIAN_POINT('Ctrl Pts',(36.1463561353721,-9.72295005120263,-8.92645544227755));
#66762=CARTESIAN_POINT('Ctrl Pts',(36.1291467983957,-9.7292819193453,-9.02220259717521));
#66763=CARTESIAN_POINT('Ctrl Pts',(36.1164625160446,-9.73561378748798,-9.11839547722381));
#66764=CARTESIAN_POINT('Ctrl Pts',(36.109095299302,-9.73929142913152,-9.17426570912192));
#66765=CARTESIAN_POINT('Ctrl Pts',(36.103253615341,-9.74296907077507,-9.23028623541386));
#66766=CARTESIAN_POINT('Ctrl Pts',(36.0989380633046,-9.74664671241861,-9.28636740021731));
#66767=CARTESIAN_POINT('Ctrl Pts',(36.0928660349285,-9.75182119397469,-9.36527420545974));
#66768=CARTESIAN_POINT('Ctrl Pts',(36.089805257095,-9.75699567553077,-9.4444156691509));
#66769=CARTESIAN_POINT('Ctrl Pts',(36.0897703028187,-9.76217015708685,-9.52362753095574));
#66770=CARTESIAN_POINT('',(36.0899227214263,-11.0321701121905,-9.5235494817152));
#66771=CARTESIAN_POINT('Ctrl Pts',(36.0855288150644,-9.76217176341955,-9.52365028285052));
#66772=CARTESIAN_POINT('Ctrl Pts',(36.0907961189434,-9.8238653469059,-10.4693569116554));
#66773=CARTESIAN_POINT('Ctrl Pts',(37.0531323133709,-9.95242753087891,-12.44936419088));
#66774=CARTESIAN_POINT('Ctrl Pts',(40.4146891398233,-10.1478583153386,-12.9880019777843));
#66775=CARTESIAN_POINT('Ctrl Pts',(42.7638264718393,-10.3484641167986,-10.4007848696135));
#66776=CARTESIAN_POINT('Ctrl Pts',(41.8814197118133,-10.5490699182586,-7.01943676244128));
#66777=CARTESIAN_POINT('Ctrl Pts',(38.5676048507788,-10.7496757197186,-5.9100433496554));
#66778=CARTESIAN_POINT('Ctrl Pts',(36.3678047754139,-10.9107087127355,-7.65077367760187));
#66779=CARTESIAN_POINT('Ctrl Pts',(36.092255627385,-11.0048731052659,-9.10216184953282));
#66780=CARTESIAN_POINT('Ctrl Pts',(36.0940461619714,-11.0321688973096,-9.5235326496095));
#66781=CARTESIAN_POINT('',(36.0897713719083,-12.3021701571198,-9.52792128380894));
#66782=CARTESIAN_POINT('Ctrl Pts',(36.0897703379492,-11.0321701570869,-9.52355010375274));
#66783=CARTESIAN_POINT('Ctrl Pts',(36.0897241617295,-11.0385779524537,-9.62260453497503));
#66784=CARTESIAN_POINT('Ctrl Pts',(36.0944143525894,-11.0449857478205,-9.72164861444106));
#66785=CARTESIAN_POINT('Ctrl Pts',(36.1038115441062,-11.0513935431873,-9.82020789029057));
#66786=CARTESIAN_POINT('Ctrl Pts',(36.1132122425988,-11.0578037299051,-9.91880394787363));
#66787=CARTESIAN_POINT('Ctrl Pts',(36.1273233973644,-11.0642139166229,-10.0169144255494));
#66788=CARTESIAN_POINT('Ctrl Pts',(36.1460638966692,-11.0706241033407,-10.1140712432912));
#66789=CARTESIAN_POINT('Ctrl Pts',(36.1656183557366,-11.0773127049489,-10.2154478920533));
#66790=CARTESIAN_POINT('Ctrl Pts',(36.1902132986866,-11.084001306557,-10.3157856690931));
#66791=CARTESIAN_POINT('Ctrl Pts',(36.2196981073553,-11.0906899081652,-10.4145680308993));
#66792=CARTESIAN_POINT('Ctrl Pts',(36.2480163797545,-11.0971138820983,-10.5094421696908));
#66793=CARTESIAN_POINT('Ctrl Pts',(36.2808447273581,-11.1035378560314,-10.6028812604354));
#66794=CARTESIAN_POINT('Ctrl Pts',(36.3180000700141,-11.1099618299644,-10.6944473294942));
#66795=CARTESIAN_POINT('Ctrl Pts',(36.3551891151171,-11.116391630883,-10.7860964552649));
#66796=CARTESIAN_POINT('Ctrl Pts',(36.3967127984438,-11.1228214318015,-10.8758687966678));
#66797=CARTESIAN_POINT('Ctrl Pts',(36.442341679746,-11.12925123272,-10.9633501804617));
#66798=CARTESIAN_POINT('Ctrl Pts',(36.4880483250545,-11.1356919917656,-11.050980656293));
#66799=CARTESIAN_POINT('Ctrl Pts',(36.5378739228314,-11.1421327508112,-11.1363120218029));
#66800=CARTESIAN_POINT('Ctrl Pts',(36.5915453137922,-11.1485735098568,-11.2189583238382));
#66801=CARTESIAN_POINT('Ctrl Pts',(36.5979723797916,-11.1493447807841,-11.2288550905937));
#66802=CARTESIAN_POINT('Ctrl Pts',(36.6044545459733,-11.1501160517113,-11.2387133935015));
#66803=CARTESIAN_POINT('Ctrl Pts',(36.6109913052643,-11.1508873226385,-11.2485326023847));
#66804=CARTESIAN_POINT('Ctrl Pts',(36.6646633149648,-11.1572200723766,-11.3291561424247));
#66805=CARTESIAN_POINT('Ctrl Pts',(36.7221981354031,-11.1635528221147,-11.407410242574));
#66806=CARTESIAN_POINT('Ctrl Pts',(36.7833597112063,-11.1698855718528,-11.4829020321454));
#66807=CARTESIAN_POINT('Ctrl Pts',(36.8444389669447,-11.1762097980635,-11.5582922139847));
#66808=CARTESIAN_POINT('Ctrl Pts',(36.9091350030548,-11.1825340242742,-11.6309271378762));
#66809=CARTESIAN_POINT('Ctrl Pts',(36.9771682360055,-11.1888582504848,-11.7004423922221));
#66810=CARTESIAN_POINT('Ctrl Pts',(37.0451302492573,-11.1951758562621,-11.7698848754344));
#66811=CARTESIAN_POINT('Ctrl Pts',(37.1164222098382,-11.2014934620394,-11.8362138707592));
#66812=CARTESIAN_POINT('Ctrl Pts',(37.1907246276679,-11.2078110678167,-11.8990983827634));
#66813=CARTESIAN_POINT('Ctrl Pts',(37.2649742809055,-11.2141241872542,-11.9619382384061));
#66814=CARTESIAN_POINT('Ctrl Pts',(37.3422298084112,-11.2204373066918,-12.0213381919138));
#66815=CARTESIAN_POINT('Ctrl Pts',(37.4221359635795,-11.2267504261293,-12.0770051177265));
#66816=CARTESIAN_POINT('Ctrl Pts',(37.5020132275409,-11.2330612629687,-12.1326519163706));
#66817=CARTESIAN_POINT('Ctrl Pts',(37.5845388564222,-11.2393720998081,-12.1845681195381));
#66818=CARTESIAN_POINT('Ctrl Pts',(37.669326479712,-11.2456829366476,-12.2325023965251));
#66819=CARTESIAN_POINT('Ctrl Pts',(37.7541064092692,-11.2519932008339,-12.2804323238971));
#66820=CARTESIAN_POINT('Ctrl Pts',(37.8411475443659,-11.2583034650203,-12.3243808284582));
#66821=CARTESIAN_POINT('Ctrl Pts',(37.9300375495852,-11.2646137292066,-12.364141776565));
#66822=CARTESIAN_POINT('Ctrl Pts',(38.018943561905,-11.2709251297303,-12.4039098847286));
#66823=CARTESIAN_POINT('Ctrl Pts',(38.1096987064192,-11.277236530254,-12.4394887602099));
#66824=CARTESIAN_POINT('Ctrl Pts',(38.2018702174821,-11.2835479307777,-12.4707202158642));
#66825=CARTESIAN_POINT('Ctrl Pts',(38.294140252596,-11.2898660776891,-12.5019850554729));
#66826=CARTESIAN_POINT('Ctrl Pts',(38.3878292619987,-11.2961842246005,-12.528893057107));
#66827=CARTESIAN_POINT('Ctrl Pts',(38.4824890439523,-11.3025023715119,-12.5513358506371));
#66828=CARTESIAN_POINT('Ctrl Pts',(38.5772042688076,-11.3088242190065,-12.5737917890697));
#66829=CARTESIAN_POINT('Ctrl Pts',(38.6728909688513,-11.3151460665011,-12.5917772308581));
#66830=CARTESIAN_POINT('Ctrl Pts',(38.7690925400138,-11.3214679139956,-12.6052352854657));
#66831=CARTESIAN_POINT('Ctrl Pts',(38.8654483054211,-11.3277998943029,-12.6187149109744));
#66832=CARTESIAN_POINT('Ctrl Pts',(38.9623201546527,-11.3341318746102,-12.6276526189722));
#66833=CARTESIAN_POINT('Ctrl Pts',(39.0592482195775,-11.3404638549174,-12.6320435447879));
#66834=CARTESIAN_POINT('Ctrl Pts',(39.11552580665,-11.3441402779778,-12.6345929685292));
#66835=CARTESIAN_POINT('Ctrl Pts',(39.1718223593645,-11.3478167010381,-12.6356106023868));
#66836=CARTESIAN_POINT('Ctrl Pts',(39.2280485906473,-11.3514931240985,-12.6351035239141));
#66837=CARTESIAN_POINT('Ctrl Pts',(39.3249020817444,-11.357826011792,-12.6342300469048));
#66838=CARTESIAN_POINT('Ctrl Pts',(39.4218828453814,-11.3641588994855,-12.6288264923168));
#66839=CARTESIAN_POINT('Ctrl Pts',(39.5185328446035,-11.370491787179,-12.6188758022598));
#66840=CARTESIAN_POINT('Ctrl Pts',(39.615052809339,-11.376816154502,-12.6089385000236));
#66841=CARTESIAN_POINT('Ctrl Pts',(39.7112424628503,-11.3831405218251,-12.5944662661471));
#66842=CARTESIAN_POINT('Ctrl Pts',(39.8066438092959,-11.3894648891481,-12.5754940487637));
#66843=CARTESIAN_POINT('Ctrl Pts',(39.9019453324034,-11.3957826389602,-12.5565416829878));
#66844=CARTESIAN_POINT('Ctrl Pts',(39.9964597616624,-11.4021003887722,-12.5330987794212));
#66845=CARTESIAN_POINT('Ctrl Pts',(40.0897352726025,-11.4084181385842,-12.5052519688085));
#66846=CARTESIAN_POINT('Ctrl Pts',(40.1829446018916,-11.4147314057715,-12.4774249163069));
#66847=CARTESIAN_POINT('Ctrl Pts',(40.2749163426568,-11.4210446729589,-12.4452002935937));
#66848=CARTESIAN_POINT('Ctrl Pts',(40.3652108391374,-11.4273579401462,-12.4087153731353));
#66849=CARTESIAN_POINT('Ctrl Pts',(40.4554727210744,-11.4336689269694,-12.3722436310994));
#66850=CARTESIAN_POINT('Ctrl Pts',(40.5440581574955,-11.4399799137926,-12.3315148126457));
#66851=CARTESIAN_POINT('Ctrl Pts',(40.6305454802007,-11.4462909006158,-12.2867150979016));
#66852=CARTESIAN_POINT('Ctrl Pts',(40.7170249830089,-11.4526013168205,-12.2419194337991));
#66853=CARTESIAN_POINT('Ctrl Pts',(40.8014063611047,-11.4589117330252,-12.1930538065363));
#66854=CARTESIAN_POINT('Ctrl Pts',(40.8832916023835,-11.4652221492299,-12.1403508434329));
#66855=CARTESIAN_POINT('Ctrl Pts',(40.9651916128401,-11.4715337036087,-12.0876383745942));
#66856=CARTESIAN_POINT('Ctrl Pts',(41.0445942246253,-11.4778452579875,-12.0310874319583));
#66857=CARTESIAN_POINT('Ctrl Pts',(41.1211304090095,-11.4841568123663,-11.9709739582585));
#66858=CARTESIAN_POINT('Ctrl Pts',(41.1977484247345,-11.4904751149644,-11.910796212134));
#66859=CARTESIAN_POINT('Ctrl Pts',(41.2714935500206,-11.4967934175625,-11.8470486010112));
#66860=CARTESIAN_POINT('Ctrl Pts',(41.342030035329,-11.5031117201606,-11.7800472235961));
#66861=CARTESIAN_POINT('Ctrl Pts',(41.4126078473937,-11.5094337246011,-11.7130065906158));
#66862=CARTESIAN_POINT('Ctrl Pts',(41.4799729736348,-11.5157557290416,-11.6427087108299));
#66863=CARTESIAN_POINT('Ctrl Pts',(41.5438281804137,-11.5220777334821,-11.5695048578076));
#66864=CARTESIAN_POINT('Ctrl Pts',(41.6077857375214,-11.5284098711484,-11.4961836699772));
#66865=CARTESIAN_POINT('Ctrl Pts',(41.6682218698025,-11.5347420088148,-11.4199475504585));
#66866=CARTESIAN_POINT('Ctrl Pts',(41.7248811254073,-11.5410741464812,-11.3411789436787));
#66867=CARTESIAN_POINT('Ctrl Pts',(41.7577639531156,-11.5447490728403,-11.2954647086802));
#66868=CARTESIAN_POINT('Ctrl Pts',(41.7893754825444,-11.5484239991994,-11.2488980050405));
#66869=CARTESIAN_POINT('Ctrl Pts',(41.8196728876223,-11.5520989255585,-11.2015573699568));
#66870=CARTESIAN_POINT('Ctrl Pts',(41.8718724618999,-11.5584304774175,-11.1199939162207));
#66871=CARTESIAN_POINT('Ctrl Pts',(41.9203500411026,-11.5647620292766,-11.035848339955));
#66872=CARTESIAN_POINT('Ctrl Pts',(41.9648409709928,-11.5710935811357,-10.9494946675996));
#66873=CARTESIAN_POINT('Ctrl Pts',(42.0092720006465,-11.577416608528,-10.8632572572645));
#66874=CARTESIAN_POINT('Ctrl Pts',(42.0497268502101,-11.5837396359203,-10.7748180450956));
#66875=CARTESIAN_POINT('Ctrl Pts',(42.0859844286908,-11.5900626633125,-10.6845794626735));
#66876=CARTESIAN_POINT('Ctrl Pts',(42.1222040480089,-11.596379070935,-10.5944353537702));
#66877=CARTESIAN_POINT('Ctrl Pts',(42.1542349699074,-11.6026954785574,-10.5024960234953));
#66878=CARTESIAN_POINT('Ctrl Pts',(42.1819027494922,-11.6090118861799,-10.4091869968908));
#66879=CARTESIAN_POINT('Ctrl Pts',(42.2095509033465,-11.6153238133519,-10.3159441576651));
#66880=CARTESIAN_POINT('Ctrl Pts',(42.2328419437029,-11.621635740524,-10.2213339718679));
#66881=CARTESIAN_POINT('Ctrl Pts',(42.2516504805008,-11.627947667696,-10.125799465512));
#66882=CARTESIAN_POINT('Ctrl Pts',(42.2704522276816,-11.6342573163513,-10.0302994457677));
#66883=CARTESIAN_POINT('Ctrl Pts',(42.2847746020702,-11.6405669650065,-9.93387619725917));
#66884=CARTESIAN_POINT('Ctrl Pts',(42.2945429989377,-11.6468766136617,-9.83698442369069));
#66885=CARTESIAN_POINT('Ctrl Pts',(42.3043105177682,-11.6531856951712,-9.74010135928578));
#66886=CARTESIAN_POINT('Ctrl Pts',(42.3095248292482,-11.6594947766806,-9.64275028884194));
#66887=CARTESIAN_POINT('Ctrl Pts',(42.3101631532206,-11.66580385819,-9.54539149943055));
#66888=CARTESIAN_POINT('Ctrl Pts',(42.3108015928644,-11.672114082975,-9.44801506752728));
#66889=CARTESIAN_POINT('Ctrl Pts',(42.3068623952391,-11.6784243077599,-9.35063135134026));
#66890=CARTESIAN_POINT('Ctrl Pts',(42.2983748946307,-11.6847345325449,-9.25370004566518));
#66891=CARTESIAN_POINT('Ctrl Pts',(42.289878296095,-11.6910515213902,-9.15666483731997));
#66892=CARTESIAN_POINT('Ctrl Pts',(42.2768236993154,-11.6973685102355,-9.06008344418471));
#66893=CARTESIAN_POINT('Ctrl Pts',(42.2592922556029,-11.7036854990808,-8.96440964358261));
#66894=CARTESIAN_POINT('Ctrl Pts',(42.2417505187476,-11.710006196786,-8.86867967053394));
#66895=CARTESIAN_POINT('Ctrl Pts',(42.2197267999755,-11.7163268944912,-8.77385877703149));
#66896=CARTESIAN_POINT('Ctrl Pts',(42.1933527578327,-11.7226475921964,-8.68038771020335));
#66897=CARTESIAN_POINT('Ctrl Pts',(42.1669363335332,-11.7289784470401,-8.58676643866337));
#66898=CARTESIAN_POINT('Ctrl Pts',(42.1361557648325,-11.7353093018838,-8.49449973986808));
#66899=CARTESIAN_POINT('Ctrl Pts',(42.1011916494707,-11.7416401567276,-8.40401040774618));
#66900=CARTESIAN_POINT('Ctrl Pts',(42.0808224722886,-11.7453283468245,-8.35129369462442));
#66901=CARTESIAN_POINT('Ctrl Pts',(42.0590343231343,-11.7490165369215,-8.29917979824462));
#66902=CARTESIAN_POINT('Ctrl Pts',(42.0358700493032,-11.7527047270185,-8.2477483739039));
#66903=CARTESIAN_POINT('Ctrl Pts',(41.9960890758525,-11.7590386096775,-8.15942304408162));
#66904=CARTESIAN_POINT('Ctrl Pts',(41.9521087431886,-11.7653724923366,-8.07280481370756));
#66905=CARTESIAN_POINT('Ctrl Pts',(41.9040978289802,-11.7717063749956,-7.9883199473526));
#66906=CARTESIAN_POINT('Ctrl Pts',(41.8561515555157,-11.7780317298669,-7.90394882939622));
#66907=CARTESIAN_POINT('Ctrl Pts',(41.804185700536,-11.7843570847382,-7.82170574339922));
#66908=CARTESIAN_POINT('Ctrl Pts',(41.7484166328061,-11.7906824396095,-7.74199598471091));
#66909=CARTESIAN_POINT('Ctrl Pts',(41.6927059860422,-11.7970011683463,-7.66236972609333));
#66910=CARTESIAN_POINT('Ctrl Pts',(41.6332002963815,-11.8033198970831,-7.58527187516194));
#66911=CARTESIAN_POINT('Ctrl Pts',(41.5701607612321,-11.8096386258199,-7.51108127800159));
#66912=CARTESIAN_POINT('Ctrl Pts',(41.5071661144676,-11.8159528551973,-7.43694350953161));
#66913=CARTESIAN_POINT('Ctrl Pts',(41.440642907176,-11.8222670845747,-7.36570921132328));
#66914=CARTESIAN_POINT('Ctrl Pts',(41.3708937990263,-11.8285813139521,-7.29772570924704));
#66915=CARTESIAN_POINT('Ctrl Pts',(41.3011699986349,-11.8348932522752,-7.22976687429672));
#66916=CARTESIAN_POINT('Ctrl Pts',(41.2282229358957,-11.8412051905983,-7.16505679652928));
#66917=CARTESIAN_POINT('Ctrl Pts',(41.1523928059093,-11.8475171289215,-7.10390665517963));
#66918=CARTESIAN_POINT('Ctrl Pts',(41.0765696728215,-11.8538284848377,-7.04276215619577));
#66919=CARTESIAN_POINT('Ctrl Pts',(40.9978643418071,-11.8601398407539,-6.98517721476751));
#66920=CARTESIAN_POINT('Ctrl Pts',(40.9166500115214,-11.8664511966701,-6.93142266534353));
#66921=CARTESIAN_POINT('Ctrl Pts',(40.835421201202,-11.8727636778637,-6.87765853180205));
#66922=CARTESIAN_POINT('Ctrl Pts',(40.7516828676701,-11.8790761590573,-6.82772638789288));
#66923=CARTESIAN_POINT('Ctrl Pts',(40.6658362042823,-11.8853886402508,-6.78185310726617));
#66924=CARTESIAN_POINT('Ctrl Pts',(40.579898110483,-11.89170784451,-6.73593096961045));
#66925=CARTESIAN_POINT('Ctrl Pts',(40.4918475900371,-11.8980270487692,-6.69407653199056));
#66926=CARTESIAN_POINT('Ctrl Pts',(40.4021092098581,-11.9043462530284,-6.65647004539357));
#66927=CARTESIAN_POINT('Ctrl Pts',(40.3123184430967,-11.9106691462501,-6.61884160525448));
#66928=CARTESIAN_POINT('Ctrl Pts',(40.2208382649942,-11.9169920394717,-6.58546620401095));
#66929=CARTESIAN_POINT('Ctrl Pts',(40.1281099534859,-11.9233149326934,-6.55647468140485));
#66930=CARTESIAN_POINT('Ctrl Pts',(40.0352334573929,-11.9296479302218,-6.52743682886276));
#66931=CARTESIAN_POINT('Ctrl Pts',(39.941105267667,-11.9359809277502,-6.50279695473534));
#66932=CARTESIAN_POINT('Ctrl Pts',(39.8461783926739,-11.9423139252787,-6.48263510772599));
#66933=CARTESIAN_POINT('Ctrl Pts',(39.7912347859215,-11.9459794596786,-6.47096544522459));
#66934=CARTESIAN_POINT('Ctrl Pts',(39.7360237571867,-11.9496449940785,-6.4607949974646));
#66935=CARTESIAN_POINT('Ctrl Pts',(39.6806337417642,-11.9533105284784,-6.45213133063294));
#66936=CARTESIAN_POINT('Ctrl Pts',(39.5849202251457,-11.9596445434634,-6.43716058160992));
#66937=CARTESIAN_POINT('Ctrl Pts',(39.4883410379946,-11.9659785584484,-6.42664011360705));
#66938=CARTESIAN_POINT('Ctrl Pts',(39.3913454556738,-11.9723125734334,-6.42066149244433));
#66939=CARTESIAN_POINT('Ctrl Pts',(39.294480113299,-11.9786380834767,-6.41469089902142));
#66940=CARTESIAN_POINT('Ctrl Pts',(39.1971999196214,-11.98496359352,-6.41325005783559));
#66941=CARTESIAN_POINT('Ctrl Pts',(39.0999625889811,-11.9912891035633,-6.41637921751517));
#66942=CARTESIAN_POINT('Ctrl Pts',(39.0028267741711,-11.9976080097704,-6.4195051103502));
#66943=CARTESIAN_POINT('Ctrl Pts',(38.9057341680089,-12.0039269159775,-6.42719150479397));
#66944=CARTESIAN_POINT('Ctrl Pts',(38.809144825332,-12.0102458221846,-6.43942665208957));
#66945=CARTESIAN_POINT('Ctrl Pts',(38.7126237677838,-12.0165602611563,-6.451653149584));
#66946=CARTESIAN_POINT('Ctrl Pts',(38.6166056987806,-12.0228747001281,-6.46842195190101));
#66947=CARTESIAN_POINT('Ctrl Pts',(38.521546930115,-12.0291891390999,-6.48966936152523));
#66948=CARTESIAN_POINT('Ctrl Pts',(38.4265223544631,-12.035501306743,-6.51090912837251));
#66949=CARTESIAN_POINT('Ctrl Pts',(38.3324568196193,-12.0418134743862,-6.536624206213));
#66950=CARTESIAN_POINT('Ctrl Pts',(38.2397968720151,-12.0481256420294,-6.56669970998413));
#66951=CARTESIAN_POINT('Ctrl Pts',(38.1471451904813,-12.0544372465726,-6.59677253075963));
#66952=CARTESIAN_POINT('Ctrl Pts',(38.0558992625411,-12.0607488511157,-6.63120486891768));
#66953=CARTESIAN_POINT('Ctrl Pts',(37.9664898776547,-12.0670604556588,-6.66983215362533));
#66954=CARTESIAN_POINT('Ctrl Pts',(37.8770642844406,-12.0733732043833,-6.70846644077115));
#66955=CARTESIAN_POINT('Ctrl Pts',(37.7894762967557,-12.0796859531078,-6.75129701150839));
#66956=CARTESIAN_POINT('Ctrl Pts',(37.7041351823981,-12.0859987018324,-6.79811182840939));
#66957=CARTESIAN_POINT('Ctrl Pts',(37.6187028162322,-12.0923182005243,-6.84497670250415));
#66958=CARTESIAN_POINT('Ctrl Pts',(37.5355225036806,-12.0986376992161,-6.89583411745703));
#66959=CARTESIAN_POINT('Ctrl Pts',(37.4549772386612,-12.104957197908,-6.95042698388459));
#66960=CARTESIAN_POINT('Ctrl Pts',(37.3743847570931,-12.1112804011618,-7.00505185327026));
#66961=CARTESIAN_POINT('Ctrl Pts',(37.2964307487401,-12.1176036044155,-7.06341627276901));
#66962=CARTESIAN_POINT('Ctrl Pts',(37.2214659560914,-12.1239268076693,-7.12522215819994));
#66963=CARTESIAN_POINT('Ctrl Pts',(37.1463811192866,-12.1302601365243,-7.18712701589631));
#66964=CARTESIAN_POINT('Ctrl Pts',(37.0742953801205,-12.1365934653793,-7.252484050578));
#66965=CARTESIAN_POINT('Ctrl Pts',(37.0055233541049,-12.1429267942343,-7.32095759942762));
#66966=CARTESIAN_POINT('Ctrl Pts',(36.9657458188551,-12.1465899728023,-7.36056249637255));
#66967=CARTESIAN_POINT('Ctrl Pts',(36.927076136464,-12.1502531513704,-7.40120935512828));
#66968=CARTESIAN_POINT('Ctrl Pts',(36.8895688620344,-12.1539163299384,-7.44282839092957));
#66969=CARTESIAN_POINT('Ctrl Pts',(36.8254868610798,-12.1601749508609,-7.51393542636495));
#66970=CARTESIAN_POINT('Ctrl Pts',(36.764565764203,-12.1664335717834,-7.58814229296622));
#66971=CARTESIAN_POINT('Ctrl Pts',(36.7071249514657,-12.1726921927059,-7.66513316463385));
#66972=CARTESIAN_POINT('Ctrl Pts',(36.649755496101,-12.1789430386907,-7.74202839234961));
#66973=CARTESIAN_POINT('Ctrl Pts',(36.5958580071872,-12.1851938846754,-7.82170040393273));
#66974=CARTESIAN_POINT('Ctrl Pts',(36.5457140776744,-12.1914447306601,-7.90379770064187));
#66975=CARTESIAN_POINT('Ctrl Pts',(36.4956180854176,-12.1976896008785,-7.98581651289304));
#66976=CARTESIAN_POINT('Ctrl Pts',(36.4492687590421,-12.203934471097,-8.07025562599238));
#66977=CARTESIAN_POINT('Ctrl Pts',(36.4069058032,-12.2101793413154,-8.1567326793706));
#66978=CARTESIAN_POINT('Ctrl Pts',(36.3645712237582,-12.2164200284703,-8.2431518069637));
#66979=CARTESIAN_POINT('Ctrl Pts',(36.3262179067279,-12.2226607156251,-8.3316057616338));
#66980=CARTESIAN_POINT('Ctrl Pts',(36.2920401973097,-12.22890140278,-8.42168660896501));
#66981=CARTESIAN_POINT('Ctrl Pts',(36.2578666116568,-12.235141336955,-8.51175658744959));
#66982=CARTESIAN_POINT('Ctrl Pts',(36.2278678053593,-12.2413812711299,-8.6034526550614));
#66983=CARTESIAN_POINT('Ctrl Pts',(36.2021900878147,-12.2476212053048,-8.69634664466751));
#66984=CARTESIAN_POINT('Ctrl Pts',(36.1765154905506,-12.2538603812214,-8.78922934607045));
#66985=CARTESIAN_POINT('Ctrl Pts',(36.155161052167,-12.2600995571379,-8.88330924623595));
#66986=CARTESIAN_POINT('Ctrl Pts',(36.1382228227054,-12.2663387330545,-8.97814428822788));
#66987=CARTESIAN_POINT('Ctrl Pts',(36.1212723595305,-12.2725824152443,-9.07304782526019));
#66988=CARTESIAN_POINT('Ctrl Pts',(36.1087445529449,-12.278826097434,-9.16870715093872));
#66989=CARTESIAN_POINT('Ctrl Pts',(36.1006839684518,-12.2850697796238,-9.26467176586364));
#66990=CARTESIAN_POINT('Ctrl Pts',(36.0933251144286,-12.2907699054448,-9.35228198733494));
#66991=CARTESIAN_POINT('Ctrl Pts',(36.0896889292421,-12.2964700312659,-9.44014631837954));
#66992=CARTESIAN_POINT('Ctrl Pts',(36.0897713719079,-12.3021701570869,-9.52792128330179));
#66993=CARTESIAN_POINT('',(41.0695067500478,-12.749987293334,-12.0106538705994));
#66994=CARTESIAN_POINT('Ctrl Pts',(36.0897713719083,-12.3021701571198,-9.52792128380894));
#66995=CARTESIAN_POINT('Ctrl Pts',(36.0898859550271,-12.3100924880381,-9.64991548889901));
#66996=CARTESIAN_POINT('Ctrl Pts',(36.0971817230537,-12.3180148189564,-9.77159152110514));
#66997=CARTESIAN_POINT('Ctrl Pts',(36.1115251314279,-12.3259371498747,-9.89222423544519));
#66998=CARTESIAN_POINT('Ctrl Pts',(36.1261440100273,-12.3340116319572,-10.015173743683));
#66999=CARTESIAN_POINT('Ctrl Pts',(36.1480838130826,-12.3420861140396,-10.1370396621098));
#67000=CARTESIAN_POINT('Ctrl Pts',(36.1771548843577,-12.3501605961221,-10.2570779055111));
#67001=CARTESIAN_POINT('Ctrl Pts',(36.1823892552886,-12.3516144412142,-10.2786913055096));
#67002=CARTESIAN_POINT('Ctrl Pts',(36.1878546946538,-12.3530682863063,-10.3002455094091));
#67003=CARTESIAN_POINT('Ctrl Pts',(36.1935499325926,-12.3545221313983,-10.3217362456208));
#67004=CARTESIAN_POINT('Ctrl Pts',(36.2184018099668,-12.3608661648413,-10.4155137395126));
#67005=CARTESIAN_POINT('Ctrl Pts',(36.2476880166877,-12.3672101982842,-10.508287686898));
#67006=CARTESIAN_POINT('Ctrl Pts',(36.2813108665629,-12.3735542317272,-10.5996089499237));
#67007=CARTESIAN_POINT('Ctrl Pts',(36.3148883928595,-12.3798897134174,-10.6908071119496));
#67008=CARTESIAN_POINT('Ctrl Pts',(36.3527907932599,-12.3862251951077,-10.7805560766052));
#67009=CARTESIAN_POINT('Ctrl Pts',(36.3948700214694,-12.3925606767979,-10.8684196873832));
#67010=CARTESIAN_POINT('Ctrl Pts',(36.436904991161,-12.3988894948909,-10.9561908840806));
#67011=CARTESIAN_POINT('Ctrl Pts',(36.4831078669681,-12.4052183129839,-11.0420802786785));
#67012=CARTESIAN_POINT('Ctrl Pts',(36.5332820736652,-12.4115471310769,-11.1256705327034));
#67013=CARTESIAN_POINT('Ctrl Pts',(36.5834198380218,-12.4178713524466,-11.2092000737703));
#67014=CARTESIAN_POINT('Ctrl Pts',(36.6375229743783,-12.4241955738163,-11.2904334222201));
#67015=CARTESIAN_POINT('Ctrl Pts',(36.6953488730092,-12.430519795186,-11.3689775988237));
#67016=CARTESIAN_POINT('Ctrl Pts',(36.7531532351144,-12.4368416611793,-11.4474925226406));
#67017=CARTESIAN_POINT('Ctrl Pts',(36.8146773462053,-12.4431635271727,-11.5233199145098));
#67018=CARTESIAN_POINT('Ctrl Pts',(36.8796356676765,-12.449485393166,-11.5960963324242));
#67019=CARTESIAN_POINT('Ctrl Pts',(36.9445872192859,-12.4558066003036,-11.6688651656861));
#67020=CARTESIAN_POINT('Ctrl Pts',(37.0129719793865,-12.4621278074413,-11.7385833324219));
#67021=CARTESIAN_POINT('Ctrl Pts',(37.0844652528387,-12.4684490145789,-11.8049217939336));
#67022=CARTESIAN_POINT('Ctrl Pts',(37.1559702507216,-12.4747712583533,-11.8712711345204));
#67023=CARTESIAN_POINT('Ctrl Pts',(37.2305844550788,-12.4810935021277,-11.9342393728276));
#67024=CARTESIAN_POINT('Ctrl Pts',(37.307948348546,-12.4874157459021,-11.9935362466713));
#67025=CARTESIAN_POINT('Ctrl Pts',(37.3853921374805,-12.4937445188027,-12.0528943577568));
#67026=CARTESIAN_POINT('Ctrl Pts',(37.4655909386642,-12.5000732917032,-12.1085732691621));
#67027=CARTESIAN_POINT('Ctrl Pts',(37.5481545341936,-12.5064020646038,-12.1603248775046));
#67028=CARTESIAN_POINT('Ctrl Pts',(37.6307650023221,-12.5127344304443,-12.2121058660162));
#67029=CARTESIAN_POINT('Ctrl Pts',(37.7157425591651,-12.5190667962847,-12.2599548972531));
#67030=CARTESIAN_POINT('Ctrl Pts',(37.802672363057,-12.5253991621252,-12.3036698486749));
#67031=CARTESIAN_POINT('Ctrl Pts',(37.8897375398657,-12.5317413891501,-12.347452875949));
#67032=CARTESIAN_POINT('Ctrl Pts',(37.9787606369115,-12.5380836161751,-12.387088790452));
#67033=CARTESIAN_POINT('Ctrl Pts',(38.0693068804957,-12.5444258432,-12.4224236353018));
#67034=CARTESIAN_POINT('Ctrl Pts',(38.1202371511642,-12.5479932064195,-12.4422987084246));
#67035=CARTESIAN_POINT('Ctrl Pts',(38.171649027407,-12.5515605696389,-12.4608139017796));
#67036=CARTESIAN_POINT('Ctrl Pts',(38.2234634008129,-12.5551279328584,-12.4779488521388));
#67037=CARTESIAN_POINT('Ctrl Pts',(38.3150843011274,-12.5614359321341,-12.5082477726036));
#67038=CARTESIAN_POINT('Ctrl Pts',(38.4082797221892,-12.5677439314098,-12.534332451525));
#67039=CARTESIAN_POINT('Ctrl Pts',(38.5026246672537,-12.5740519306855,-12.556039144943));
#67040=CARTESIAN_POINT('Ctrl Pts',(38.5968442865265,-12.5803515505509,-12.5777170036573));
#67041=CARTESIAN_POINT('Ctrl Pts',(38.6922099691279,-12.5866511704163,-12.5950283357082));
#67042=CARTESIAN_POINT('Ctrl Pts',(38.7882798848438,-12.5929507902817,-12.607858608447));
#67043=CARTESIAN_POINT('Ctrl Pts',(38.8880642364851,-12.5994939779089,-12.6211849493424));
#67044=CARTESIAN_POINT('Ctrl Pts',(38.9886079299138,-12.6060371655361,-12.6296765276222));
#67045=CARTESIAN_POINT('Ctrl Pts',(39.0894019424228,-12.6125803531633,-12.6332629751294));
#67046=CARTESIAN_POINT('Ctrl Pts',(39.1862778293985,-12.6188691900619,-12.63671000809));
#67047=CARTESIAN_POINT('Ctrl Pts',(39.2833844506666,-12.6251580269606,-12.6356261437977));
#67048=CARTESIAN_POINT('Ctrl Pts',(39.3802641991579,-12.6314468638593,-12.6300016862156));
#67049=CARTESIAN_POINT('Ctrl Pts',(39.4771131819549,-12.6377337036385,-12.6243790147689));
#67050=CARTESIAN_POINT('Ctrl Pts',(39.5737349951434,-12.6440205434176,-12.6142186404297));
#67051=CARTESIAN_POINT('Ctrl Pts',(39.6696735849597,-12.6503073831968,-12.5995629569893));
#67052=CARTESIAN_POINT('Ctrl Pts',(39.7656082253187,-12.6565939641687,-12.5849078768724));
#67053=CARTESIAN_POINT('Ctrl Pts',(39.860859262293,-12.6628805451406,-12.565757922853));
#67054=CARTESIAN_POINT('Ctrl Pts',(39.9549784023291,-12.6691671261125,-12.542207030503));
#67055=CARTESIAN_POINT('Ctrl Pts',(40.0491196823481,-12.6754551858994,-12.5186505981921));
#67056=CARTESIAN_POINT('Ctrl Pts',(40.1421281089206,-12.6817432456863,-12.4906912788937));
#67057=CARTESIAN_POINT('Ctrl Pts',(40.2335692412759,-12.6880313054732,-12.4584732445325));
#67058=CARTESIAN_POINT('Ctrl Pts',(40.3251097880169,-12.6943262016102,-12.4262201828701));
#67059=CARTESIAN_POINT('Ctrl Pts',(40.415079223903,-12.7006210977473,-12.389699313691));
#67060=CARTESIAN_POINT('Ctrl Pts',(40.5030621364958,-12.7069159938843,-12.3491033482029));
#67061=CARTESIAN_POINT('Ctrl Pts',(40.5911018509854,-12.7132149540155,-12.3084811739003));
#67062=CARTESIAN_POINT('Ctrl Pts',(40.6771520989339,-12.7195139141467,-12.2637788700992));
#67063=CARTESIAN_POINT('Ctrl Pts',(40.7608230186359,-12.7258128742779,-12.2152345915173));
#67064=CARTESIAN_POINT('Ctrl Pts',(40.8446201610862,-12.7321213367794,-12.166617080894));
#67065=CARTESIAN_POINT('Ctrl Pts',(40.9260304439932,-12.7384297992808,-12.1141462693586));
#67066=CARTESIAN_POINT('Ctrl Pts',(41.0046941210115,-12.7447382617822,-12.0581027974574));
#67067=CARTESIAN_POINT('Ctrl Pts',(41.0265118049324,-12.7464879389662,-12.0425589174595));
#67068=CARTESIAN_POINT('Ctrl Pts',(41.0481184108033,-12.7482376161501,-12.0267404404404));
#67069=CARTESIAN_POINT('Ctrl Pts',(41.0695067500478,-12.749987293334,-12.0106538705994));
#67070=CARTESIAN_POINT('',(38.2853957334119,-12.75,-12.4977141955524));
#67071=CARTESIAN_POINT('Origin',(39.2,-12.75,-9.525));
#67072=CARTESIAN_POINT('',(36.0919483849455,-12.4928298429131,-9.52879526530289));
#67073=CARTESIAN_POINT('Ctrl Pts',(38.2853957334118,-12.75,-12.4977141955524));
#67074=CARTESIAN_POINT('Ctrl Pts',(37.3019474236971,-12.6831313995133,-12.1951401972246));
#67075=CARTESIAN_POINT('Ctrl Pts',(36.2593719387647,-12.5974080138178,-11.1359917255917));
#67076=CARTESIAN_POINT('Ctrl Pts',(36.0895541491445,-12.5116846281221,-9.81920730742513));
#67077=CARTESIAN_POINT('Ctrl Pts',(36.0919483849455,-12.4928298429131,-9.52879526530289));
#67078=CARTESIAN_POINT('',(36.0900673707834,-11.222829801326,-9.52326984187138));
#67079=CARTESIAN_POINT('Ctrl Pts',(36.0919483849455,-12.4928298429131,-9.52879526530289));
#67080=CARTESIAN_POINT('Ctrl Pts',(36.0980453197133,-12.4448160276354,-8.78925938672623));
#67081=CARTESIAN_POINT('Ctrl Pts',(36.7293203004083,-12.3299336118711,-7.0075733048701));
#67082=CARTESIAN_POINT('Ctrl Pts',(39.6920471758748,-12.14818259562,-5.88918093587763));
#67083=CARTESIAN_POINT('Ctrl Pts',(42.5136842856469,-11.94757679416,-7.94804692653049));
#67084=CARTESIAN_POINT('Ctrl Pts',(42.3317557451001,-11.7469709927,-11.4386305882703));
#67085=CARTESIAN_POINT('Ctrl Pts',(39.3094778593138,-11.5463651912402,-13.1930895342595));
#67086=CARTESIAN_POINT('Ctrl Pts',(36.59108955988,-11.3716514746445,-11.8247205883103));
#67087=CARTESIAN_POINT('Ctrl Pts',(36.096963550306,-11.2638063585355,-10.1556712558172));
#67088=CARTESIAN_POINT('Ctrl Pts',(36.0937128061288,-11.2228298429131,-9.52327251182905));
#67089=CARTESIAN_POINT('',(36.0897701688195,-9.95282984294777,-9.52397523911836));
#67090=CARTESIAN_POINT('Ctrl Pts',(36.089770481347,-11.2228297979391,-9.52326962442624));
#67091=CARTESIAN_POINT('Ctrl Pts',(36.0898309229459,-11.2157993567217,-9.41463006205864));
#67092=CARTESIAN_POINT('Ctrl Pts',(36.0955876081903,-11.2087689155044,-9.30619309129701));
#67093=CARTESIAN_POINT('Ctrl Pts',(36.1069524548467,-11.201738474287,-9.19852253321102));
#67094=CARTESIAN_POINT('Ctrl Pts',(36.1183588864254,-11.1946823080986,-9.09045799956816));
#67095=CARTESIAN_POINT('Ctrl Pts',(36.1354144747909,-11.1876261419101,-8.98316573382048));
#67096=CARTESIAN_POINT('Ctrl Pts',(36.1579801913597,-11.1805699757217,-8.87719899912097));
#67097=CARTESIAN_POINT('Ctrl Pts',(36.1806584687337,-11.1734786124347,-8.77070368820889));
#67098=CARTESIAN_POINT('Ctrl Pts',(36.2089018643949,-11.1663872491478,-8.66554739650279));
#67099=CARTESIAN_POINT('Ctrl Pts',(36.2425206599758,-11.1592958858608,-8.56227127069456));
#67100=CARTESIAN_POINT('Ctrl Pts',(36.2648693015945,-11.1545817866806,-8.49361678490559));
#67101=CARTESIAN_POINT('Ctrl Pts',(36.2895924108059,-11.1498676875004,-8.42579274376721));
#67102=CARTESIAN_POINT('Ctrl Pts',(36.3166228666883,-11.1451535883202,-8.35895241949765));
#67103=CARTESIAN_POINT('Ctrl Pts',(36.3529354112524,-11.1388206971065,-8.26915954792089));
#67104=CARTESIAN_POINT('Ctrl Pts',(36.3935094163776,-11.1324878058927,-8.18090867255315));
#67105=CARTESIAN_POINT('Ctrl Pts',(36.4381928691988,-11.126154914679,-8.09463220633452));
#67106=CARTESIAN_POINT('Ctrl Pts',(36.4828162017387,-11.1198305441855,-8.00847182258245));
#67107=CARTESIAN_POINT('Ctrl Pts',(36.5315377931203,-11.113506173692,-7.92428095303794));
#67108=CARTESIAN_POINT('Ctrl Pts',(36.5841572587825,-11.1071818031986,-7.84247291073221));
#67109=CARTESIAN_POINT('Ctrl Pts',(36.6367216630998,-11.1008640505668,-7.76075047288447));
#67110=CARTESIAN_POINT('Ctrl Pts',(36.6931755975997,-11.0945462979349,-7.6814062710863));
#67111=CARTESIAN_POINT('Ctrl Pts',(36.753272853838,-11.0882285453031,-7.60482893336719));
#67112=CARTESIAN_POINT('Ctrl Pts',(36.8133274642926,-11.0819152758296,-7.52830593590889));
#67113=CARTESIAN_POINT('Ctrl Pts',(36.8770199874541,-11.0756020063561,-7.4545462421718));
#67114=CARTESIAN_POINT('Ctrl Pts',(36.9440615576594,-11.0692887368826,-7.38390859670361));
#67115=CARTESIAN_POINT('Ctrl Pts',(37.0110789088195,-11.0629777481038,-7.31329646937764));
#67116=CARTESIAN_POINT('Ctrl Pts',(37.0814426023051,-11.0566667593251,-7.24580446610108));
#67117=CARTESIAN_POINT('Ctrl Pts',(37.1548248613583,-11.0503557705463,-7.1817566696602));
#67118=CARTESIAN_POINT('Ctrl Pts',(37.2282004815662,-11.0440453527186,-7.11771466758188));
#67119=CARTESIAN_POINT('Ctrl Pts',(37.3045937948049,-11.0377349348909,-7.05711654018844));
#67120=CARTESIAN_POINT('Ctrl Pts',(37.3836424801294,-11.0314245170632,-7.00024733629027));
#67121=CARTESIAN_POINT('Ctrl Pts',(37.4627054188214,-11.0251129613961,-6.9433678782346));
#67122=CARTESIAN_POINT('Ctrl Pts',(37.5444243255732,-11.0188014057291,-6.89021893441362));
#67123=CARTESIAN_POINT('Ctrl Pts',(37.6284072016717,-11.012489850062,-6.84104271100627));
#67124=CARTESIAN_POINT('Ctrl Pts',(37.7124798640876,-11.0061715466939,-6.79181391316701));
#67125=CARTESIAN_POINT('Ctrl Pts',(37.7988209501189,-10.9998532433258,-6.7465665364544));
#67126=CARTESIAN_POINT('Ctrl Pts',(37.8870132974164,-10.9935349399577,-6.70549710556298));
#67127=CARTESIAN_POINT('Ctrl Pts',(37.9752573118236,-10.9872129350386,-6.66440361432102));
#67128=CARTESIAN_POINT('Ctrl Pts',(38.0653543426938,-10.9808909301195,-6.62749310851382));
#67129=CARTESIAN_POINT('Ctrl Pts',(38.1568686178513,-10.9745689252004,-6.59491338481667));
#67130=CARTESIAN_POINT('Ctrl Pts',(38.2485295699489,-10.9682367875196,-6.56228144310026));
#67131=CARTESIAN_POINT('Ctrl Pts',(38.3416118840624,-10.9619046498389,-6.53399427107727));
#67132=CARTESIAN_POINT('Ctrl Pts',(38.4356661006116,-10.9555725121581,-6.51014936636229));
#67133=CARTESIAN_POINT('Ctrl Pts',(38.4902512424626,-10.9518976037254,-6.49631077885345));
#67134=CARTESIAN_POINT('Ctrl Pts',(38.5451635539952,-10.9482226952928,-6.48396745765534));
#67135=CARTESIAN_POINT('Ctrl Pts',(38.6003142679106,-10.9445477868601,-6.47313046222019));
#67136=CARTESIAN_POINT('Ctrl Pts',(38.6953519381646,-10.9382150540441,-6.45445576654372));
#67137=CARTESIAN_POINT('Ctrl Pts',(38.7914277571371,-10.9318823212281,-6.44019219959787));
#67138=CARTESIAN_POINT('Ctrl Pts',(38.8880965579976,-10.9255495884122,-6.43044883775255));
#67139=CARTESIAN_POINT('Ctrl Pts',(38.9846353012854,-10.9192253756135,-6.42071858456255));
#67140=CARTESIAN_POINT('Ctrl Pts',(39.0817650093881,-10.9129011628148,-6.41549649276756));
#67141=CARTESIAN_POINT('Ctrl Pts',(39.1790300674642,-10.9065769500162,-6.41484069301435));
#67142=CARTESIAN_POINT('Ctrl Pts',(39.2761933584161,-10.9002593541565,-6.41418557941563));
#67143=CARTESIAN_POINT('Ctrl Pts',(39.3734912828146,-10.8939417582968,-6.41808726258191));
#67144=CARTESIAN_POINT('Ctrl Pts',(39.4704638476505,-10.887624162437,-6.42655200785715));
#67145=CARTESIAN_POINT('Ctrl Pts',(39.5673676294268,-10.8813110476754,-6.43501074905195));
#67146=CARTESIAN_POINT('Ctrl Pts',(39.6639460760389,-10.8749979329137,-6.44802607988394));
#67147=CARTESIAN_POINT('Ctrl Pts',(39.7597409005073,-10.8686848181521,-6.46555221041456));
#67148=CARTESIAN_POINT('Ctrl Pts',(39.8555011381581,-10.8623739827468,-6.48307201311813));
#67149=CARTESIAN_POINT('Ctrl Pts',(39.9504778861266,-10.8560631473416,-6.50509930079477));
#67150=CARTESIAN_POINT('Ctrl Pts',(40.0442206129504,-10.8497523119364,-6.53153675326226));
#67151=CARTESIAN_POINT('Ctrl Pts',(40.137954881549,-10.8434420459457,-6.55797182032949));
#67152=CARTESIAN_POINT('Ctrl Pts',(40.2304549295605,-10.8371317799549,-6.58881614213147));
#67153=CARTESIAN_POINT('Ctrl Pts',(40.3212840296132,-10.8308215139642,-6.62392213516521));
#67154=CARTESIAN_POINT('Ctrl Pts',(40.4121295325585,-10.824510108398,-6.65903446801553));
#67155=CARTESIAN_POINT('Ctrl Pts',(40.5013030803449,-10.8181987028317,-6.69840984297876));
#67156=CARTESIAN_POINT('Ctrl Pts',(40.5883875993672,-10.8118872972655,-6.74185240656854));
#67157=CARTESIAN_POINT('Ctrl Pts',(40.6755652724881,-10.8055691404041,-6.78534144056311));
#67158=CARTESIAN_POINT('Ctrl Pts',(40.7606490635793,-10.7992509835427,-6.83290615351406));
#67159=CARTESIAN_POINT('Ctrl Pts',(40.8432463974884,-10.7929328266812,-6.8843046502784));
#67160=CARTESIAN_POINT('Ctrl Pts',(40.9258921455622,-10.7866109664522,-6.93573327410819));
#67161=CARTESIAN_POINT('Ctrl Pts',(41.006048174458,-10.7802891062233,-6.99099990834741));
#67162=CARTESIAN_POINT('Ctrl Pts',(41.0833525415978,-10.7739672459943,-7.0498204394515));
#67163=CARTESIAN_POINT('Ctrl Pts',(41.1607808659939,-10.7676352486867,-7.10873528905162));
#67164=CARTESIAN_POINT('Ctrl Pts',(41.2353480629236,-10.761303251379,-7.17121513406714));
#67165=CARTESIAN_POINT('Ctrl Pts',(41.3067268284427,-10.7549712540714,-7.23693690576073));
#67166=CARTESIAN_POINT('Ctrl Pts',(41.3481700752881,-10.751294831181,-7.27509564369365));
#67167=CARTESIAN_POINT('Ctrl Pts',(41.3885391791425,-10.7476184082906,-7.31434658483823));
#67168=CARTESIAN_POINT('Ctrl Pts',(41.4277762873863,-10.7439419854002,-7.35462135417361));
#67169=CARTESIAN_POINT('Ctrl Pts',(41.4953605833667,-10.7376094990398,-7.42399297846341));
#67170=CARTESIAN_POINT('Ctrl Pts',(41.5598189499684,-10.7312770126794,-7.49664495904801));
#67171=CARTESIAN_POINT('Ctrl Pts',(41.6208167091706,-10.724944526319,-7.57226419772146));
#67172=CARTESIAN_POINT('Ctrl Pts',(41.6817323540334,-10.7186205646641,-7.6477816388222));
#67173=CARTESIAN_POINT('Ctrl Pts',(41.7391963784556,-10.7122966030092,-7.72625806128481));
#67174=CARTESIAN_POINT('Ctrl Pts',(41.7929110505019,-10.7059726413543,-7.80734376632425));
#67175=CARTESIAN_POINT('Ctrl Pts',(41.8465694827374,-10.6996553009519,-7.88834457380142));
#67176=CARTESIAN_POINT('Ctrl Pts',(41.8964861266362,-10.6933379605496,-7.97194886994616));
#67177=CARTESIAN_POINT('Ctrl Pts',(41.9424042851038,-10.6870206201472,-8.05777493548391));
#67178=CARTESIAN_POINT('Ctrl Pts',(41.9882898331519,-10.6807077662296,-8.14354004857711));
#67179=CARTESIAN_POINT('Ctrl Pts',(42.0301823354706,-10.6743949123121,-8.23152340964769));
#67180=CARTESIAN_POINT('Ctrl Pts',(42.0678696155352,-10.6680820583945,-8.32131627028119));
#67181=CARTESIAN_POINT('Ctrl Pts',(42.1055432686988,-10.6617714870677,-8.41107666376871));
#67182=CARTESIAN_POINT('Ctrl Pts',(42.1390145518075,-10.6554609157409,-8.50264485392143));
#67183=CARTESIAN_POINT('Ctrl Pts',(42.1681186764902,-10.649150344414,-8.59559041581756));
#67184=CARTESIAN_POINT('Ctrl Pts',(42.1972201616111,-10.6428403454165,-8.68852754813379));
#67185=CARTESIAN_POINT('Ctrl Pts',(42.2219551453044,-10.6365303464189,-8.78284138641357));
#67186=CARTESIAN_POINT('Ctrl Pts',(42.2422084733341,-10.6302203474213,-8.87808558705612));
#67187=CARTESIAN_POINT('Ctrl Pts',(42.2624654507439,-10.6239092114459,-8.97334694943624));
#67188=CARTESIAN_POINT('Ctrl Pts',(42.2782390776999,-10.6175980754705,-9.0695385793586));
#67189=CARTESIAN_POINT('Ctrl Pts',(42.2894653629619,-10.611286939495,-9.16620420298098));
#67190=CARTESIAN_POINT('Ctrl Pts',(42.3007036532935,-10.6049690545707,-9.26297319806607));
#67191=CARTESIAN_POINT('Ctrl Pts',(42.3073848430886,-10.5986511696463,-9.36021676366926));
#67192=CARTESIAN_POINT('Ctrl Pts',(42.3094968866886,-10.592333284722,-9.45747397113558));
#67193=CARTESIAN_POINT('Ctrl Pts',(42.3116101677337,-10.5860116981524,-9.55478816154437));
#67194=CARTESIAN_POINT('Ctrl Pts',(42.3091489828831,-10.5796901115829,-9.65211557273019));
#67195=CARTESIAN_POINT('Ctrl Pts',(42.3021533838499,-10.5733685250134,-9.74899784813421));
#67196=CARTESIAN_POINT('Ctrl Pts',(42.295146566964,-10.5670368014096,-9.84603547993994));
#67197=CARTESIAN_POINT('Ctrl Pts',(42.2835908685082,-10.5607050778058,-9.94262611666422));
#67198=CARTESIAN_POINT('Ctrl Pts',(42.2675778949649,-10.5543733542021,-10.0383191124656));
#67199=CARTESIAN_POINT('Ctrl Pts',(42.2582735345488,-10.5506942974481,-10.093921659977));
#67200=CARTESIAN_POINT('Ctrl Pts',(42.2474652583428,-10.5470152406942,-10.1492213645));
#67201=CARTESIAN_POINT('Ctrl Pts',(42.2351787567165,-10.5433361839402,-10.2041322166387));
#67202=CARTESIAN_POINT('Ctrl Pts',(42.2140303184225,-10.5370035184584,-10.2986488498879));
#67203=CARTESIAN_POINT('Ctrl Pts',(42.1884260203412,-10.5306708529766,-10.392340839025));
#67204=CARTESIAN_POINT('Ctrl Pts',(42.1584451326556,-10.5243381874949,-10.4847567660436));
#67205=CARTESIAN_POINT('Ctrl Pts',(42.1285045921532,-10.5180140442829,-10.5770483230842));
#67206=CARTESIAN_POINT('Ctrl Pts',(42.0941993022163,-10.5116899010709,-10.6680668187252));
#67207=CARTESIAN_POINT('Ctrl Pts',(42.0556593764814,-10.505365757859,-10.7573717695623));
#67208=CARTESIAN_POINT('Ctrl Pts',(42.0171597880662,-10.4990482337305,-10.8465832505161));
#67209=CARTESIAN_POINT('Ctrl Pts',(41.9744345475036,-10.4927307096021,-10.934084352748));
#67210=CARTESIAN_POINT('Ctrl Pts',(41.9276630113239,-10.4864131854736,-11.019451454399));
#67211=CARTESIAN_POINT('Ctrl Pts',(41.8809246723569,-10.4801001453585,-11.1047579647148));
#67212=CARTESIAN_POINT('Ctrl Pts',(41.8301459569201,-10.4737871052434,-11.1879331032524));
#67213=CARTESIAN_POINT('Ctrl Pts',(41.7755531900407,-10.4674740651283,-11.2685757563614));
#67214=CARTESIAN_POINT('Ctrl Pts',(41.7209801495324,-10.4611633061464,-11.3491892703188));
#67215=CARTESIAN_POINT('Ctrl Pts',(41.6625960408975,-10.4548525471645,-11.4272717553604));
#67216=CARTESIAN_POINT('Ctrl Pts',(41.6006712428079,-10.4485417881826,-11.5024499328314));
#67217=CARTESIAN_POINT('Ctrl Pts',(41.5387520486998,-10.4422316003026,-11.5776213069357));
#67218=CARTESIAN_POINT('Ctrl Pts',(41.4732930804004,-10.4359214124227,-11.64988855863));
#67219=CARTESIAN_POINT('Ctrl Pts',(41.4046051764515,-10.4296112245428,-11.7189112718757));
#67220=CARTESIAN_POINT('Ctrl Pts',(41.3359048853634,-10.4232998986871,-11.78794643264));
#67221=CARTESIAN_POINT('Ctrl Pts',(41.2639748105852,-10.4169885728313,-11.8537355828928));
#67222=CARTESIAN_POINT('Ctrl Pts',(41.1891620717469,-10.4106772469755,-11.9159757224246));
#67223=CARTESIAN_POINT('Ctrl Pts',(41.1142693282935,-10.4043591717987,-11.9782824214551));
#67224=CARTESIAN_POINT('Ctrl Pts',(41.0364881030367,-10.3980410966219,-12.037032252502));
#67225=CARTESIAN_POINT('Ctrl Pts',(40.9561978070758,-10.391723021445,-12.0919631698414));
#67226=CARTESIAN_POINT('Ctrl Pts',(40.8758604642909,-10.385401244135,-12.146926274448));
#67227=CARTESIAN_POINT('Ctrl Pts',(40.7930114951643,-10.3790794668249,-12.1980657798235));
#67228=CARTESIAN_POINT('Ctrl Pts',(40.7080566338598,-10.3727576895149,-12.2451646718483));
#67229=CARTESIAN_POINT('Ctrl Pts',(40.6229655613931,-10.3664257762736,-12.2923390792081));
#67230=CARTESIAN_POINT('Ctrl Pts',(40.5357622463171,-10.3600938630323,-12.3354597431534));
#67231=CARTESIAN_POINT('Ctrl Pts',(40.4468741463487,-10.3537619497909,-12.3743570355551));
#67232=CARTESIAN_POINT('Ctrl Pts',(40.3952533580996,-10.3500847606874,-12.3969462111055));
#67233=CARTESIAN_POINT('Ctrl Pts',(40.3430646999005,-10.3464075715838,-12.4181119386258));
#67234=CARTESIAN_POINT('Ctrl Pts',(40.2903941024023,-10.3427303824802,-12.4378287547239));
#67235=CARTESIAN_POINT('Ctrl Pts',(40.1996880264142,-10.3363977527002,-12.4717838473977));
#67236=CARTESIAN_POINT('Ctrl Pts',(40.107236841428,-10.3300651229201,-12.5015569736709));
#67237=CARTESIAN_POINT('Ctrl Pts',(40.0134618815896,-10.32373249314,-12.5269677580049));
#67238=CARTESIAN_POINT('Ctrl Pts',(39.9198131233972,-10.3174083857661,-12.5523443446936));
#67239=CARTESIAN_POINT('Ctrl Pts',(39.8248445497447,-10.3110842783923,-12.5733701445375));
#67240=CARTESIAN_POINT('Ctrl Pts',(39.7289961307342,-10.3047601710184,-12.5899133342671));
#67241=CARTESIAN_POINT('Ctrl Pts',(39.6332480321042,-10.2984426828133,-12.606439208958));
#67242=CARTESIAN_POINT('Ctrl Pts',(39.5366223475779,-10.2921251946082,-12.6184917269789));
#67243=CARTESIAN_POINT('Ctrl Pts',(39.4395718451484,-10.2858077064031,-12.6259895168982));
#67244=CARTESIAN_POINT('Ctrl Pts',(39.3425902266162,-10.2794947021852,-12.6334819850831));
#67245=CARTESIAN_POINT('Ctrl Pts',(39.2451848244055,-10.2731816979672,-12.636426118629));
#67246=CARTESIAN_POINT('Ctrl Pts',(39.1478152327065,-10.2668686937493,-12.6347921800279));
#67247=CARTESIAN_POINT('Ctrl Pts',(39.0504808239462,-10.2605579706341,-12.6331588318243));
#67248=CARTESIAN_POINT('Ctrl Pts',(38.9531826367933,-10.2542472475189,-12.6269507057427));
#67249=CARTESIAN_POINT('Ctrl Pts',(38.856381037686,-10.2479365244037,-12.6161901691158));
#67250=CARTESIAN_POINT('Ctrl Pts',(38.7595881976793,-10.2416263723147,-12.6054306061569));
#67251=CARTESIAN_POINT('Ctrl Pts',(38.663292290989,-10.2353162202258,-12.5901195001764));
#67252=CARTESIAN_POINT('Ctrl Pts',(38.5679482817613,-10.2290060681369,-12.5703310621953));
#67253=CARTESIAN_POINT('Ctrl Pts',(38.4725870763213,-10.2226947779512,-12.5505390551784));
#67254=CARTESIAN_POINT('Ctrl Pts',(38.3781785375033,-10.2163834877655,-12.5262682012066));
#67255=CARTESIAN_POINT('Ctrl Pts',(38.285166130107,-10.2100721975797,-12.4976435446243));
#67256=CARTESIAN_POINT('Ctrl Pts',(38.1920542488689,-10.2037541576678,-12.4689882748729));
#67257=CARTESIAN_POINT('Ctrl Pts',(38.1003418986366,-10.1974361177559,-12.4359700353948));
#67258=CARTESIAN_POINT('Ctrl Pts',(38.0104559008266,-10.191118077844,-12.3987632973197));
#67259=CARTESIAN_POINT('Ctrl Pts',(37.9205172306873,-10.1847963356215,-12.3615347564543));
#67260=CARTESIAN_POINT('Ctrl Pts',(37.8324074396652,-10.178474593399,-12.3201130155421));
#67261=CARTESIAN_POINT('Ctrl Pts',(37.7465300291259,-10.1721528511766,-12.2747192032401));
#67262=CARTESIAN_POINT('Ctrl Pts',(37.6605149189724,-10.1658209723948,-12.2292526045044));
#67263=CARTESIAN_POINT('Ctrl Pts',(37.5767397132873,-10.159489093613,-12.1798014387739));
#67264=CARTESIAN_POINT('Ctrl Pts',(37.4955801076958,-10.1531572148312,-12.1266309276333));
#67265=CARTESIAN_POINT('Ctrl Pts',(37.4484427445428,-10.1494796702275,-12.0957495837134));
#67266=CARTESIAN_POINT('Ctrl Pts',(37.4021871093497,-10.1458021256239,-12.0636143887629));
#67267=CARTESIAN_POINT('Ctrl Pts',(37.3568815158417,-10.1421245810202,-12.0302833983911));
#67268=CARTESIAN_POINT('Ctrl Pts',(37.2795150877967,-10.1358445950862,-11.9733654889544));
#67269=CARTESIAN_POINT('Ctrl Pts',(37.2046422003673,-10.1295646091522,-11.9127532616935));
#67270=CARTESIAN_POINT('Ctrl Pts',(37.1326407205089,-10.1232846232183,-11.8486945286337));
#67271=CARTESIAN_POINT('Ctrl Pts',(37.0607364833283,-10.1170131188134,-11.7847223110559));
#67272=CARTESIAN_POINT('Ctrl Pts',(36.9916962788464,-10.1107416144085,-11.7173131289113));
#67273=CARTESIAN_POINT('Ctrl Pts',(36.9258678285865,-10.1044701100037,-11.6467571773986));
#67274=CARTESIAN_POINT('Ctrl Pts',(36.8595477246366,-10.098151765543,-11.5756742638537));
#67275=CARTESIAN_POINT('Ctrl Pts',(36.7964879299382,-10.0918334210823,-11.5013976382766));
#67276=CARTESIAN_POINT('Ctrl Pts',(36.7370090233934,-10.0855150766217,-11.4242646213875));
#67277=CARTESIAN_POINT('Ctrl Pts',(36.6780731830441,-10.0792544211719,-11.3478358597793));
#67278=CARTESIAN_POINT('Ctrl Pts',(36.6226533882408,-10.0729937657222,-11.2686030111864));
#67279=CARTESIAN_POINT('Ctrl Pts',(36.5710225829619,-10.0667331102724,-11.1869291181046));
#67280=CARTESIAN_POINT('Ctrl Pts',(36.5194087470668,-10.0604745124986,-11.1052820686024));
#67281=CARTESIAN_POINT('Ctrl Pts',(36.4715816646951,-10.0542159147247,-11.0211959445787));
#67282=CARTESIAN_POINT('Ctrl Pts',(36.4277710784546,-10.0479573169509,-10.9350629274778));
#67283=CARTESIAN_POINT('Ctrl Pts',(36.3839625177518,-10.041699008537,-10.848933892649));
#67284=CARTESIAN_POINT('Ctrl Pts',(36.3441702851032,-10.035440700123,-10.7607585503843));
#67285=CARTESIAN_POINT('Ctrl Pts',(36.3085777172643,-10.0291823917091,-10.6709528069686));
#67286=CARTESIAN_POINT('Ctrl Pts',(36.2723913778188,-10.0228196793123,-10.5796488827869));
#67287=CARTESIAN_POINT('Ctrl Pts',(36.2405462905674,-10.0164569669155,-10.4866600999831));
#67288=CARTESIAN_POINT('Ctrl Pts',(36.2131831840949,-10.0100942545187,-10.3924421946889));
#67289=CARTESIAN_POINT('Ctrl Pts',(36.1862342561534,-10.0038278505903,-10.2996504079402));
#67290=CARTESIAN_POINT('Ctrl Pts',(36.1636326108138,-9.99756144666187,-10.2056669037343));
#67291=CARTESIAN_POINT('Ctrl Pts',(36.1454612557528,-9.99129504273344,-10.1109383182494));
#67292=CARTESIAN_POINT('Ctrl Pts',(36.1268709868953,-9.9848841761025,-10.0140259049072));
#67293=CARTESIAN_POINT('Ctrl Pts',(36.1129178675833,-9.97847330947155,-9.91633412434151));
#67294=CARTESIAN_POINT('Ctrl Pts',(36.1036345934322,-9.9720624428406,-9.81834607873639));
#67295=CARTESIAN_POINT('Ctrl Pts',(36.094351319281,-9.96565157620966,-9.7203580331313));
#67296=CARTESIAN_POINT('Ctrl Pts',(36.0897378470939,-9.95924070957871,-9.62207421712648));
#67297=CARTESIAN_POINT('Ctrl Pts',(36.0897701688195,-9.95282984294777,-9.52397523911838));
#67298=CARTESIAN_POINT('',(36.0897711821211,-8.68282986586788,-9.52771170347425));
#67299=CARTESIAN_POINT('Ctrl Pts',(36.0897701688197,-9.95282984291314,-9.52397523858839));
#67300=CARTESIAN_POINT('Ctrl Pts',(36.0897891778604,-9.94905948846218,-9.46628133546143));
#67301=CARTESIAN_POINT('Ctrl Pts',(36.091413392757,-9.94528913401121,-9.40861613371628));
#67302=CARTESIAN_POINT('Ctrl Pts',(36.0946386559873,-9.94151877956024,-9.35104145317981));
#67303=CARTESIAN_POINT('Ctrl Pts',(36.1000557567198,-9.9351861522987,-9.25433993710724));
#67304=CARTESIAN_POINT('Ctrl Pts',(36.1100035216219,-9.92885352503716,-9.15772373237964));
#67305=CARTESIAN_POINT('Ctrl Pts',(36.1244775265326,-9.92252089777562,-9.06165113780548));
#67306=CARTESIAN_POINT('Ctrl Pts',(36.1389320519434,-9.91619679313193,-8.96570784027888));
#67307=CARTESIAN_POINT('Ctrl Pts',(36.1579006455556,-9.90987268848823,-8.87030712758677));
#67308=CARTESIAN_POINT('Ctrl Pts',(36.1813269362864,-9.90354858384453,-8.77590482092732));
#67309=CARTESIAN_POINT('Ctrl Pts',(36.2047287069587,-9.8972310985764,-8.68160132419543));
#67310=CARTESIAN_POINT('Ctrl Pts',(36.2325787940897,-9.89091361330827,-8.58829457815231));
#67311=CARTESIAN_POINT('Ctrl Pts',(36.2647694900105,-9.88459612804013,-8.49643181746348));
#67312=CARTESIAN_POINT('Ctrl Pts',(36.2969373362904,-9.87828312705746,-8.40463426291674));
#67313=CARTESIAN_POINT('Ctrl Pts',(36.3334395218242,-9.87197012607479,-8.31427906755525));
#67314=CARTESIAN_POINT('Ctrl Pts',(36.3741183233008,-9.86565712509212,-8.22579893696325));
#67315=CARTESIAN_POINT('Ctrl Pts',(36.4147824249554,-9.8593464053957,-8.13735077983468));
#67316=CARTESIAN_POINT('Ctrl Pts',(36.4596199611181,-9.85303568569929,-8.05077673804627));
#67317=CARTESIAN_POINT('Ctrl Pts',(36.5084251979139,-9.84672496600288,-7.96648925647748));
#67318=CARTESIAN_POINT('Ctrl Pts',(36.5572260171697,-9.84041481751273,-7.88220940407609));
#67319=CARTESIAN_POINT('Ctrl Pts',(36.6099936037103,-9.83410466902258,-7.80021607874136));
#67320=CARTESIAN_POINT('Ctrl Pts',(36.6664769368874,-9.82779452053243,-7.72089591719979));
#67321=CARTESIAN_POINT('Ctrl Pts',(36.7229704558046,-9.82148323412194,-7.64156145171203));
#67322=CARTESIAN_POINT('Ctrl Pts',(36.7831807985061,-9.81517194771146,-7.56490146364139));
#67323=CARTESIAN_POINT('Ctrl Pts',(36.8468150360541,-9.80886066130098,-7.49127160654161));
#67324=CARTESIAN_POINT('Ctrl Pts',(36.9105173259497,-9.80254262541296,-7.41756300748115));
#67325=CARTESIAN_POINT('Ctrl Pts',(36.9776505344837,-9.79622458952494,-7.34689134030989));
#67326=CARTESIAN_POINT('Ctrl Pts',(37.0478831820992,-9.78990655363693,-7.27957713225137));
#67327=CARTESIAN_POINT('Ctrl Pts',(37.1181569837697,-9.78358481558467,-7.21222348024881));
#67328=CARTESIAN_POINT('Ctrl Pts',(37.1915335115763,-9.77726307753242,-7.14823149221863));
#67329=CARTESIAN_POINT('Ctrl Pts',(37.267647957252,-9.77094133948016,-7.08788157124288));
#67330=CARTESIAN_POINT('Ctrl Pts',(37.3438844459462,-9.76460946506039,-7.02743488431868));
#67331=CARTESIAN_POINT('Ctrl Pts',(37.4228672637757,-9.75827759064061,-6.97064218053304));
#67332=CARTESIAN_POINT('Ctrl Pts',(37.50420242666,-9.75194571622084,-6.91774066438448));
#67333=CARTESIAN_POINT('Ctrl Pts',(37.5514422323692,-9.74826813684732,-6.88701524064454));
#67334=CARTESIAN_POINT('Ctrl Pts',(37.5994750806433,-9.74459055747381,-6.85760159529307));
#67335=CARTESIAN_POINT('Ctrl Pts',(37.6482203312017,-9.7409129781003,-6.8295389054182));
#67336=CARTESIAN_POINT('Ctrl Pts',(37.7321573860576,-9.73458035742289,-6.78121625834086));
#67337=CARTESIAN_POINT('Ctrl Pts',(37.8184995468397,-9.72824773674547,-6.73673412833242));
#67338=CARTESIAN_POINT('Ctrl Pts',(37.9068606253913,-9.72191511606806,-6.69633932562838));
#67339=CARTESIAN_POINT('Ctrl Pts',(37.9951027844579,-9.71559101805699,-6.65599888768778));
#67340=CARTESIAN_POINT('Ctrl Pts',(38.0853580665042,-9.70926692004591,-6.61973502410073));
#67341=CARTESIAN_POINT('Ctrl Pts',(38.1772139628289,-9.70294282203483,-6.58774969145156));
#67342=CARTESIAN_POINT('Ctrl Pts',(38.2689737138614,-9.69662534343825,-6.55579783775452));
#67343=CARTESIAN_POINT('Ctrl Pts',(38.3623303376579,-9.69030786484167,-6.52811575492159));
#67344=CARTESIAN_POINT('Ctrl Pts',(38.4568504540997,-9.68399038624509,-6.50485771770135));
#67345=CARTESIAN_POINT('Ctrl Pts',(38.5513034776338,-9.67767739196384,-6.48161618965821));
#67346=CARTESIAN_POINT('Ctrl Pts',(38.6469179284761,-9.67136439768259,-6.4627925683058));
#67347=CARTESIAN_POINT('Ctrl Pts',(38.7432452533336,-9.66505140340134,-6.44849130436827));
#67348=CARTESIAN_POINT('Ctrl Pts',(38.8395377687616,-9.6587406904222,-6.43419520842267));
#67349=CARTESIAN_POINT('Ctrl Pts',(38.9365422142011,-9.65242997744306,-6.42441828682276));
#67350=CARTESIAN_POINT('Ctrl Pts',(39.0338007587653,-9.64611926446391,-6.41921371226013));
#67351=CARTESIAN_POINT('Ctrl Pts',(39.1310504999795,-9.63980912269849,-6.41400960878917));
#67352=CARTESIAN_POINT('Ctrl Pts',(39.2285538578922,-9.63349898093307,-6.41337705265527));
#67353=CARTESIAN_POINT('Ctrl Pts',(39.3258498582418,-9.62718883916764,-6.41731718702173));
#67354=CARTESIAN_POINT('Ctrl Pts',(39.4231634041853,-9.62087755948098,-6.42125803192098));
#67355=CARTESIAN_POINT('Ctrl Pts',(39.5202690813507,-9.61456627979432,-6.42977318735595));
#67356=CARTESIAN_POINT('Ctrl Pts',(39.6167089523252,-9.60825500010766,-6.44281176727443));
#67357=CARTESIAN_POINT('Ctrl Pts',(39.71325195973,-9.6019369709008,-6.45586429114134));
#67358=CARTESIAN_POINT('Ctrl Pts',(39.8091273053147,-9.59561894169395,-6.47344983864871));
#67359=CARTESIAN_POINT('Ctrl Pts',(39.9038853932927,-9.58930091248709,-6.49546604144974));
#67360=CARTESIAN_POINT('Ctrl Pts',(39.9986990067124,-9.58297918110165,-6.51749514509557));
#67361=CARTESIAN_POINT('Ctrl Pts',(40.0923936382179,-9.57665744971622,-6.54395995502503));
#67362=CARTESIAN_POINT('Ctrl Pts',(40.1845350731388,-9.57033571833079,-6.57470826143251));
#67363=CARTESIAN_POINT('Ctrl Pts',(40.276824250434,-9.56400385048931,-6.60550587060807));
#67364=CARTESIAN_POINT('Ctrl Pts',(40.3675548505607,-9.55767198264784,-6.64060053336553));
#67365=CARTESIAN_POINT('Ctrl Pts',(40.4563128844983,-9.55134011480636,-6.67979199545207));
#67366=CARTESIAN_POINT('Ctrl Pts',(40.5078649133095,-9.547662468751,-6.70255499833763));
#67367=CARTESIAN_POINT('Ctrl Pts',(40.5587519517666,-9.54398482269563,-6.72669917366006));
#67368=CARTESIAN_POINT('Ctrl Pts',(40.6088971099685,-9.54030717664027,-6.75217840703331));
#67369=CARTESIAN_POINT('Ctrl Pts',(40.695243138506,-9.53397455864416,-6.79605164805693));
#67370=CARTESIAN_POINT('Ctrl Pts',(40.7796878691838,-9.52764194064806,-6.84403817627217));
#67371=CARTESIAN_POINT('Ctrl Pts',(40.8618135300702,-9.52130932265195,-6.89594951661712));
#67372=CARTESIAN_POINT('Ctrl Pts',(40.943828662441,-9.51498522738624,-6.94779099227758));
#67373=CARTESIAN_POINT('Ctrl Pts',(41.0235305618395,-9.50866113212053,-7.00354654977566));
#67374=CARTESIAN_POINT('Ctrl Pts',(41.1005246285842,-9.50233703685482,-7.06298115583068));
#67375=CARTESIAN_POINT('Ctrl Pts',(41.1774381051049,-9.49601956106352,-7.12235355127105));
#67376=CARTESIAN_POINT('Ctrl Pts',(41.2516490393578,-9.48970208527221,-7.18539707370326));
#67377=CARTESIAN_POINT('Ctrl Pts',(41.3227913507861,-9.48338460948091,-7.25183314868272));
#67378=CARTESIAN_POINT('Ctrl Pts',(41.3938831625975,-9.47707161808294,-7.31822206471739));
#67379=CARTESIAN_POINT('Ctrl Pts',(41.4619103633229,-9.47075862668498,-7.3879984480901));
#67380=CARTESIAN_POINT('Ctrl Pts',(41.5265403001393,-9.46444563528701,-7.46084378383622));
#67381=CARTESIAN_POINT('Ctrl Pts',(41.5911468813939,-9.45813492523835,-7.53366279519109));
#67382=CARTESIAN_POINT('Ctrl Pts',(41.6523583482207,-9.45182421518967,-7.60954822845637));
#67383=CARTESIAN_POINT('Ctrl Pts',(41.7098799157295,-9.44551350514101,-7.68814577020454));
#67384=CARTESIAN_POINT('Ctrl Pts',(41.7673962762773,-9.43920336634975,-7.76673619715462));
#67385=CARTESIAN_POINT('Ctrl Pts',(41.821223143508,-9.43289322755849,-7.84803789144386));
#67386=CARTESIAN_POINT('Ctrl Pts',(41.8711075828414,-9.42658308876723,-7.93166546708255));
#67387=CARTESIAN_POINT('Ctrl Pts',(41.9210010176277,-9.42027181209495,-8.0153081229332));
#67388=CARTESIAN_POINT('Ctrl Pts',(41.9669503885398,-9.41396053542268,-8.10127711756356));
#67389=CARTESIAN_POINT('Ctrl Pts',(42.0087479892801,-9.4076492587504,-8.18916116779949));
#67390=CARTESIAN_POINT('Ctrl Pts',(42.0505902896826,-9.40133123260137,-8.27713920398867));
#67391=CARTESIAN_POINT('Ctrl Pts',(42.088271767496,-9.39501320645234,-8.36703598896984));
#67392=CARTESIAN_POINT('Ctrl Pts',(42.1216323864224,-9.38869518030331,-8.45841908346919));
#67393=CARTESIAN_POINT('Ctrl Pts',(42.1550125535429,-9.38237345200471,-8.54985572537026));
#67394=CARTESIAN_POINT('Ctrl Pts',(42.1840666896732,-9.37605172370611,-8.64277999384018));
#67395=CARTESIAN_POINT('Ctrl Pts',(42.2086849024328,-9.36972999540751,-8.73674508515785));
#67396=CARTESIAN_POINT('Ctrl Pts',(42.2333425887402,-9.3633981306686,-8.83086084279547));
#67397=CARTESIAN_POINT('Ctrl Pts',(42.2535500581075,-9.35706626592969,-8.92602032824715));
#67398=CARTESIAN_POINT('Ctrl Pts',(42.2692487054047,-9.35073440119079,-9.02176741235114));
#67399=CARTESIAN_POINT('Ctrl Pts',(42.2783667978414,-9.34705672585397,-9.07737925882956));
#67400=CARTESIAN_POINT('Ctrl Pts',(42.2859648013331,-9.34337905051714,-9.13318923338017));
#67401=CARTESIAN_POINT('Ctrl Pts',(42.2920393016566,-9.33970137518032,-9.18910774062048));
#67402=CARTESIAN_POINT('Ctrl Pts',(42.3024990367058,-9.33336875396508,-9.28539430559504));
#67403=CARTESIAN_POINT('Ctrl Pts',(42.3084750904721,-9.32703613274984,-9.38233715826476));
#67404=CARTESIAN_POINT('Ctrl Pts',(42.3098969268498,-9.3207035115346,-9.47948343960724));
#67405=CARTESIAN_POINT('Ctrl Pts',(42.3113168496662,-9.31437941300128,-9.57649897779818));
#67406=CARTESIAN_POINT('Ctrl Pts',(42.3081947308959,-9.30805531446795,-9.67371696693394));
#67407=CARTESIAN_POINT('Ctrl Pts',(42.300511687823,-9.30173121593463,-9.77067850246445));
#67408=CARTESIAN_POINT('Ctrl Pts',(42.2928366865873,-9.29541373683206,-9.86753854840454));
#67409=CARTESIAN_POINT('Ctrl Pts',(42.2806102861883,-9.28909625772948,-9.96414224073453));
#67410=CARTESIAN_POINT('Ctrl Pts',(42.2638656535685,-9.28277877862691,-10.060030755923));
#67411=CARTESIAN_POINT('Ctrl Pts',(42.2471329068064,-9.27646578386628,-10.1558512064796));
#67412=CARTESIAN_POINT('Ctrl Pts',(42.2258883789053,-9.27015278910564,-10.2509570595708));
#67413=CARTESIAN_POINT('Ctrl Pts',(42.2002169544868,-9.26383979434501,-10.3448956512325));
#67414=CARTESIAN_POINT('Ctrl Pts',(42.1745548069178,-9.25752908090316,-10.4388002964264));
#67415=CARTESIAN_POINT('Ctrl Pts',(42.1444690567,-9.25121836746131,-10.5315380969185));
#67416=CARTESIAN_POINT('Ctrl Pts',(42.110095264744,-9.24490765401946,-10.622668530575));
#67417=CARTESIAN_POINT('Ctrl Pts',(42.0757245842234,-9.23859751180864,-10.7137907153174));
#67418=CARTESIAN_POINT('Ctrl Pts',(42.0370667882152,-9.23228736959783,-10.8033054134044));
#67419=CARTESIAN_POINT('Ctrl Pts',(41.9943063333778,-9.22597722738702,-10.8907901625597));
#67420=CARTESIAN_POINT('Ctrl Pts',(41.9515381675793,-9.21966594727296,-10.9782906877748));
#67421=CARTESIAN_POINT('Ctrl Pts',(41.9046660656227,-9.21335466715889,-11.0637601441468));
#67422=CARTESIAN_POINT('Ctrl Pts',(41.8539208926113,-9.20704338704483,-11.1467997868606));
#67423=CARTESIAN_POINT('Ctrl Pts',(41.8031214510481,-9.20072535744087,-11.229928234891));
#67424=CARTESIAN_POINT('Ctrl Pts',(41.7484408975837,-9.19440732783692,-11.310621307687));
#67425=CARTESIAN_POINT('Ctrl Pts',(41.6901538703592,-9.18808929823297,-11.3885086141028));
#67426=CARTESIAN_POINT('Ctrl Pts',(41.6318326888123,-9.18176756646698,-11.4664415599737));
#67427=CARTESIAN_POINT('Ctrl Pts',(41.5699011034469,-9.17544583470099,-11.5415651283521));
#67428=CARTESIAN_POINT('Ctrl Pts',(41.5046731905301,-9.169124102935,-11.6135430658121));
#67429=CARTESIAN_POINT('Ctrl Pts',(41.4393406895139,-9.16279223474305,-11.685636414533));
#67430=CARTESIAN_POINT('Ctrl Pts',(41.3707016152595,-9.1564603665511,-11.7545737510813));
#67431=CARTESIAN_POINT('Ctrl Pts',(41.2991058875574,-9.15012849835915,-11.8200566715709));
#67432=CARTESIAN_POINT('Ctrl Pts',(41.2575220429871,-9.14645085681287,-11.8580901084119));
#67433=CARTESIAN_POINT('Ctrl Pts',(41.2149413990742,-9.14277321526659,-11.8949589726356));
#67434=CARTESIAN_POINT('Ctrl Pts',(41.1714371129706,-9.13909557372031,-11.9306114321524));
#67435=CARTESIAN_POINT('Ctrl Pts',(41.0965260282759,-9.13276295360344,-11.9920022663353));
#67436=CARTESIAN_POINT('Ctrl Pts',(41.0186145161548,-9.12643033348657,-12.0499972896543));
#67437=CARTESIAN_POINT('Ctrl Pts',(40.9380432358095,-9.12009771336969,-12.104289895176));
#67438=CARTESIAN_POINT('Ctrl Pts',(40.857580391501,-9.11377361594509,-12.1585094315475));
#67439=CARTESIAN_POINT('Ctrl Pts',(40.7744652532317,-9.10744951852048,-12.2090362114775));
#67440=CARTESIAN_POINT('Ctrl Pts',(40.6890717773488,-9.10112542109588,-12.2556035770143));
#67441=CARTESIAN_POINT('Ctrl Pts',(40.6037676829078,-9.09480794311076,-12.3021222004401));
#67442=CARTESIAN_POINT('Ctrl Pts',(40.5161903737469,-9.08849046512565,-12.3446894403163));
#67443=CARTESIAN_POINT('Ctrl Pts',(40.4267421897094,-9.08217298714054,-12.3830822683903));
#67444=CARTESIAN_POINT('Ctrl Pts',(40.337357498887,-9.07585999350571,-12.4214478439927));
#67445=CARTESIAN_POINT('Ctrl Pts',(40.2461049740665,-9.06954699987087,-12.4556447266813));
#67446=CARTESIAN_POINT('Ctrl Pts',(40.1534100670551,-9.06323400623604,-12.4854965625614));
#67447=CARTESIAN_POINT('Ctrl Pts',(40.0607486571582,-9.05692329392471,-12.5153376108979));
#67448=CARTESIAN_POINT('Ctrl Pts',(39.9666463166037,-9.05061258161338,-12.5408365984476));
#67449=CARTESIAN_POINT('Ctrl Pts',(39.8715460304821,-9.04430186930205,-12.5618662436538));
#67450=CARTESIAN_POINT('Ctrl Pts',(39.7764543526678,-9.03799172822508,-12.5828939852942));
#67451=CARTESIAN_POINT('Ctrl Pts',(39.6803653359286,-9.03168158714811,-12.5994530947248));
#67452=CARTESIAN_POINT('Ctrl Pts',(39.583733569712,-9.02537144607114,-12.6114671066409));
#67453=CARTESIAN_POINT('Ctrl Pts',(39.487084377987,-9.01906016709284,-12.6234832850316));
#67454=CARTESIAN_POINT('Ctrl Pts',(39.3898926763658,-9.01274888811454,-12.6309526841345));
#67455=CARTESIAN_POINT('Ctrl Pts',(39.2926185614714,-9.00643760913624,-12.6338506646301));
#67456=CARTESIAN_POINT('Ctrl Pts',(39.1952404183684,-9.00011958066403,-12.6367517443235));
#67457=CARTESIAN_POINT('Ctrl Pts',(39.0977801238736,-8.99380155219182,-12.6350716320868));
#67458=CARTESIAN_POINT('Ctrl Pts',(39.0006979589456,-8.98748352371961,-12.6288378419839));
#67459=CARTESIAN_POINT('Ctrl Pts',(38.9035589069733,-8.98116179308475,-12.6226003990795));
#67460=CARTESIAN_POINT('Ctrl Pts',(38.8067988602019,-8.9748400624499,-12.6118040134485));
#67461=CARTESIAN_POINT('Ctrl Pts',(38.7108710709203,-8.96851833181504,-12.5965278842357));
#67462=CARTESIAN_POINT('Ctrl Pts',(38.614789468363,-8.96218646474209,-12.581227260854));
#67463=CARTESIAN_POINT('Ctrl Pts',(38.5195432158814,-8.95585459766914,-12.5614326397369));
#67464=CARTESIAN_POINT('Ctrl Pts',(38.425573464008,-8.94952273059619,-12.5372739240068));
#67465=CARTESIAN_POINT('Ctrl Pts',(38.3709942830016,-8.94584507781758,-12.5232421436474));
#67466=CARTESIAN_POINT('Ctrl Pts',(38.3168454266995,-8.94216742503896,-12.5077390755156));
#67467=CARTESIAN_POINT('Ctrl Pts',(38.2632102881944,-8.93848977226034,-12.4907976479786));
#67468=CARTESIAN_POINT('Ctrl Pts',(38.1708549285897,-8.93215715237089,-12.4616258834225));
#67469=CARTESIAN_POINT('Ctrl Pts',(38.0797030675351,-8.92582453248145,-12.428085402372));
#67470=CARTESIAN_POINT('Ctrl Pts',(37.9901976627439,-8.919491912592,-12.3902938693387));
#67471=CARTESIAN_POINT('Ctrl Pts',(37.9008127179915,-8.91316781540169,-12.3525531976979));
#67472=CARTESIAN_POINT('Ctrl Pts',(37.8130702248328,-8.90684371821139,-12.3105730139726));
#67473=CARTESIAN_POINT('Ctrl Pts',(37.7273978892981,-8.90051962102109,-12.264520701958));
#67474=CARTESIAN_POINT('Ctrl Pts',(37.6418152271798,-8.8942021432768,-12.2185165929966));
#67475=CARTESIAN_POINT('Ctrl Pts',(37.5582987980726,-8.88788466553251,-12.1684490353812));
#67476=CARTESIAN_POINT('Ctrl Pts',(37.477255288265,-8.88156718778823,-12.114533029542));
#67477=CARTESIAN_POINT('Ctrl Pts',(37.3962693058775,-8.87525419440299,-12.0606552951046));
#67478=CARTESIAN_POINT('Ctrl Pts',(37.3177531160937,-8.86894120101776,-12.0029347848817));
#67479=CARTESIAN_POINT('Ctrl Pts',(37.242086954399,-8.86262820763253,-11.9416313659235));
#67480=CARTESIAN_POINT('Ctrl Pts',(37.166448136214,-8.85631749557613,-11.8803501002053));
#67481=CARTESIAN_POINT('Ctrl Pts',(37.0936576391097,-8.85000678351973,-11.8154887734607));
#67482=CARTESIAN_POINT('Ctrl Pts',(37.0240641903321,-8.84369607146334,-11.7473487586571));
#67483=CARTESIAN_POINT('Ctrl Pts',(36.9544770410844,-8.83738593064634,-11.6792149118201));
#67484=CARTESIAN_POINT('Ctrl Pts',(36.8880866771076,-8.83107578982933,-11.6078032730928));
#67485=CARTESIAN_POINT('Ctrl Pts',(36.8252056162223,-8.82476564901233,-11.5334527098436));
#67486=CARTESIAN_POINT('Ctrl Pts',(36.7623132161059,-8.81845437029873,-11.459088739088));
#67487=CARTESIAN_POINT('Ctrl Pts',(36.7029316583213,-8.81214309158513,-11.3817851251468));
#67488=CARTESIAN_POINT('Ctrl Pts',(36.647333072897,-8.80583181287153,-11.3019136760615));
#67489=CARTESIAN_POINT('Ctrl Pts',(36.5916750285238,-8.79951378466971,-11.2219568098318));
#67490=CARTESIAN_POINT('Ctrl Pts',(36.5398082836528,-8.79319575646789,-11.1394269854742));
#67491=CARTESIAN_POINT('Ctrl Pts',(36.491961396797,-8.78687772826606,-11.0547246734176));
#67492=CARTESIAN_POINT('Ctrl Pts',(36.4440864732217,-8.7805559979052,-10.9699727285609));
#67493=CARTESIAN_POINT('Ctrl Pts',(36.4002362949917,-8.77423426754433,-10.8830461513752));
#67494=CARTESIAN_POINT('Ctrl Pts',(36.3605922984875,-8.76791253718347,-10.7943677786565));
#67495=CARTESIAN_POINT('Ctrl Pts',(36.3208847357169,-8.76158067038753,-10.7055472166138));
#67496=CARTESIAN_POINT('Ctrl Pts',(36.2853969812979,-8.7552488035916,-10.6149696571239));
#67497=CARTESIAN_POINT('Ctrl Pts',(36.2542613979903,-8.74891693679567,-10.5230755189512));
#67498=CARTESIAN_POINT('Ctrl Pts',(36.2361773245804,-8.7452392814639,-10.4697018492103));
#67499=CARTESIAN_POINT('Ctrl Pts',(36.2195605060004,-8.74156162613213,-10.41588429103));
#67500=CARTESIAN_POINT('Ctrl Pts',(36.2044289529257,-8.73788397080036,-10.3617106756999));
#67501=CARTESIAN_POINT('Ctrl Pts',(36.1717147563767,-8.72993293373437,-10.2445881112859));
#67502=CARTESIAN_POINT('Ctrl Pts',(36.145853683177,-8.72198189666838,-10.1254742577294));
#67503=CARTESIAN_POINT('Ctrl Pts',(36.1270448627367,-8.71403085960239,-10.0050805945535));
#67504=CARTESIAN_POINT('Ctrl Pts',(36.1085403106784,-8.70620844565722,-9.88663452746552));
#67505=CARTESIAN_POINT('Ctrl Pts',(36.0968616954961,-8.69838603171205,-9.76694960462697));
#67506=CARTESIAN_POINT('Ctrl Pts',(36.0921528599655,-8.69056361776688,-9.64672430767749));
#67507=CARTESIAN_POINT('Ctrl Pts',(36.0906010386658,-8.68798570046722,-9.60710343424426));
#67508=CARTESIAN_POINT('Ctrl Pts',(36.0898058059764,-8.68540778316755,-9.56742405163508));
#67509=CARTESIAN_POINT('Ctrl Pts',(36.0897711821211,-8.68282986586788,-9.52771170347425));
#67510=CARTESIAN_POINT('',(36.0898198219825,-7.4128297998923,-9.52336150973275));
#67511=CARTESIAN_POINT('Ctrl Pts',(36.0909909580655,-8.68282984291315,-9.5277102865178));
#67512=CARTESIAN_POINT('Ctrl Pts',(36.097370143227,-8.63431261838889,-8.78059823168395));
#67513=CARTESIAN_POINT('Ctrl Pts',(36.7410355037994,-8.51892679337797,-6.99391762846478));
#67514=CARTESIAN_POINT('Ctrl Pts',(39.7185698196114,-8.33667236788041,-5.89196606192947));
#67515=CARTESIAN_POINT('Ctrl Pts',(42.5256954705718,-8.1360665664204,-7.97335575183573));
#67516=CARTESIAN_POINT('Ctrl Pts',(42.3172061964241,-7.93546076496045,-11.4617177794319));
#67517=CARTESIAN_POINT('Ctrl Pts',(39.2821521939203,-7.73485496350045,-13.193937346696));
#67518=CARTESIAN_POINT('Ctrl Pts',(36.5817564488487,-7.56064465615136,-11.8091234637841));
#67519=CARTESIAN_POINT('Ctrl Pts',(36.0968486952276,-7.45330294928892,-10.1480485640383));
#67520=CARTESIAN_POINT('Ctrl Pts',(36.0938362662056,-7.41282984291315,-9.5233642896731));
#67521=CARTESIAN_POINT('',(36.0897702134563,-6.14282984295053,-9.52384769963274));
#67522=CARTESIAN_POINT('Ctrl Pts',(36.0897704316019,-7.41282979936327,-9.52336147554771));
#67523=CARTESIAN_POINT('Ctrl Pts',(36.0898273887419,-7.4058341701422,-9.41524604241845));
#67524=CARTESIAN_POINT('Ctrl Pts',(36.0955258185163,-7.39883854092113,-9.30732612022363));
#67525=CARTESIAN_POINT('Ctrl Pts',(36.106780042231,-7.39184291170005,-9.2001601228919));
#67526=CARTESIAN_POINT('Ctrl Pts',(36.1180725251958,-7.38482350051631,-9.09262980983287));
#67527=CARTESIAN_POINT('Ctrl Pts',(36.1349585203378,-7.37780408933257,-8.98585880502142));
#67528=CARTESIAN_POINT('Ctrl Pts',(36.1573013842396,-7.37078467814884,-8.88039485997273));
#67529=CARTESIAN_POINT('Ctrl Pts',(36.1797517784313,-7.36373148439706,-8.77442334487207));
#67530=CARTESIAN_POINT('Ctrl Pts',(36.2077115733386,-7.35667829064528,-8.66977174456544));
#67531=CARTESIAN_POINT('Ctrl Pts',(36.2409934482374,-7.3496250968935,-8.56697553291882));
#67532=CARTESIAN_POINT('Ctrl Pts',(36.2661310982796,-7.34429785145583,-8.48933401777315));
#67533=CARTESIAN_POINT('Ctrl Pts',(36.2943038279069,-7.33897060601816,-8.41275055453054));
#67534=CARTESIAN_POINT('Ctrl Pts',(36.325413315959,-7.3336433605805,-8.3374470332511));
#67535=CARTESIAN_POINT('Ctrl Pts',(36.3623938855919,-7.32731074043165,-8.24793199180745));
#67536=CARTESIAN_POINT('Ctrl Pts',(36.4036239373028,-7.3209781202828,-8.15999048092687));
#67537=CARTESIAN_POINT('Ctrl Pts',(36.4489482718138,-7.31464550013395,-8.07405374264119));
#67538=CARTESIAN_POINT('Ctrl Pts',(36.4942116070148,-7.30832140267967,-7.98823266146978));
#67539=CARTESIAN_POINT('Ctrl Pts',(36.5435580708494,-7.30199730522538,-7.90441137383109));
#67540=CARTESIAN_POINT('Ctrl Pts',(36.5967842350216,-7.2956732077711,-7.82300166455189));
#67541=CARTESIAN_POINT('Ctrl Pts',(36.649954687292,-7.28935572975863,-7.74167716693145));
#67542=CARTESIAN_POINT('Ctrl Pts',(36.7069965286074,-7.28303825174617,-7.66275959353606));
#67543=CARTESIAN_POINT('Ctrl Pts',(36.767660690969,-7.2767207737337,-7.58663570538395));
#67544=CARTESIAN_POINT('Ctrl Pts',(36.8282817919105,-7.27040778007515,-7.51056585247427));
#67545=CARTESIAN_POINT('Ctrl Pts',(36.8925198303435,-7.2640947864166,-7.43728608341478));
#67546=CARTESIAN_POINT('Ctrl Pts',(36.9600833039791,-7.25778179275805,-7.36715296005788));
#67547=CARTESIAN_POINT('Ctrl Pts',(37.0276223622105,-7.25147108042526,-7.29704518069929));
#67548=CARTESIAN_POINT('Ctrl Pts',(37.0984841647337,-7.24516036809247,-7.23008210223094));
#67549=CARTESIAN_POINT('Ctrl Pts',(37.1723385567986,-7.23884965575968,-7.16658533657574));
#67550=CARTESIAN_POINT('Ctrl Pts',(37.2461862636697,-7.23253951466354,-7.10309431855691));
#67551=CARTESIAN_POINT('Ctrl Pts',(37.3230256897622,-7.22622937356739,-7.04306927445219));
#67552=CARTESIAN_POINT('Ctrl Pts',(37.402492427576,-7.21991923247124,-6.98679252621495));
#67553=CARTESIAN_POINT('Ctrl Pts',(37.4819734955165,-7.21360795347609,-6.93050562966963));
#67554=CARTESIAN_POINT('Ctrl Pts',(37.5640824592646,-7.20729667448094,-6.8779686241699));
#67555=CARTESIAN_POINT('Ctrl Pts',(37.6484255536837,-7.20098539548579,-6.82942076902972));
#67556=CARTESIAN_POINT('Ctrl Pts',(37.7328588473938,-7.19466736700043,-6.78082099520979));
#67557=CARTESIAN_POINT('Ctrl Pts',(37.8195306621525,-7.18834933851507,-6.73621910736065));
#67558=CARTESIAN_POINT('Ctrl Pts',(37.908022410618,-7.18203131002971,-6.69580849686087));
#67559=CARTESIAN_POINT('Ctrl Pts',(37.9965660123893,-7.17570957938377,-6.65537420704884));
#67560=CARTESIAN_POINT('Ctrl Pts',(38.0869312656922,-7.16938784873782,-6.61913624775709));
#67561=CARTESIAN_POINT('Ctrl Pts',(38.1786813381664,-7.16306611809187,-6.58723914453703));
#67562=CARTESIAN_POINT('Ctrl Pts',(38.2705785252,-7.15673425101123,-6.55529089663493));
#67563=CARTESIAN_POINT('Ctrl Pts',(38.3638645461799,-7.15040238393059,-6.52769752715895));
#67564=CARTESIAN_POINT('Ctrl Pts',(38.4580892577887,-7.14407051684995,-6.50455316161806));
#67565=CARTESIAN_POINT('Ctrl Pts',(38.5128165205381,-7.14039286427346,-6.49111053332556));
#67566=CARTESIAN_POINT('Ctrl Pts',(38.5678602730804,-7.13671521169698,-6.479167805297));
#67567=CARTESIAN_POINT('Ctrl Pts',(38.6231314638014,-7.13303755912049,-6.46873539351645));
#67568=CARTESIAN_POINT('Ctrl Pts',(38.7183039818019,-7.1267049389712,-6.45077162459775));
#67569=CARTESIAN_POINT('Ctrl Pts',(38.8144817016523,-7.1203723188219,-6.43722641490242));
#67570=CARTESIAN_POINT('Ctrl Pts',(38.9112186743944,-7.11403969867261,-6.42820552847279));
#67571=CARTESIAN_POINT('Ctrl Pts',(39.0078254546328,-7.10771560121789,-6.41919678271448));
#67572=CARTESIAN_POINT('Ctrl Pts',(39.1049895600594,-7.10139150376317,-6.41470029827978));
#67573=CARTESIAN_POINT('Ctrl Pts',(39.2022549719265,-7.09506740630845,-6.41477081744743));
#67574=CARTESIAN_POINT('Ctrl Pts',(39.2994185759482,-7.08874992829556,-6.41484126280258));
#67575=CARTESIAN_POINT('Ctrl Pts',(39.3966828405869,-7.08243245028267,-6.41946920799966));
#67576=CARTESIAN_POINT('Ctrl Pts',(39.4935877540451,-7.07611497226978,-6.42865749898775));
#67577=CARTESIAN_POINT('Ctrl Pts',(39.5904238812048,-7.0698019786108,-6.43783926782436));
#67578=CARTESIAN_POINT('Ctrl Pts',(39.6869007301712,-7.06348898495182,-6.45157490577345));
#67579=CARTESIAN_POINT('Ctrl Pts',(39.7825603819843,-7.05717599129284,-6.46981521765995));
#67580=CARTESIAN_POINT('Ctrl Pts',(39.8781854652806,-7.05086527895962,-6.48804893804712));
#67581=CARTESIAN_POINT('Ctrl Pts',(39.9729935090707,-7.0445545666264,-6.51078401598165));
#67582=CARTESIAN_POINT('Ctrl Pts',(40.0665347326534,-7.03824385429318,-6.53791978514046));
#67583=CARTESIAN_POINT('Ctrl Pts',(40.1600674890183,-7.03193371319662,-6.56505309800825));
#67584=CARTESIAN_POINT('Ctrl Pts',(40.2523332332299,-7.02562357210006,-6.5965861880615));
#67585=CARTESIAN_POINT('Ctrl Pts',(40.3428963620796,-7.0193134310035,-6.63236822971793));
#67586=CARTESIAN_POINT('Ctrl Pts',(40.4334758220529,-7.01300215200794,-6.66815672390034));
#67587=CARTESIAN_POINT('Ctrl Pts',(40.5223516501643,-7.00669087301236,-6.7081955307434));
#67588=CARTESIAN_POINT('Ctrl Pts',(40.6091082556239,-7.0003795940168,-6.75228570227067));
#67589=CARTESIAN_POINT('Ctrl Pts',(40.6959576414627,-6.99406156553103,-6.79642302528356));
#67590=CARTESIAN_POINT('Ctrl Pts',(40.7806828894738,-6.98774353704526,-6.8446201644518));
#67591=CARTESIAN_POINT('Ctrl Pts',(40.8628932495411,-6.98142550855949,-6.89663231386275));
#67592=CARTESIAN_POINT('Ctrl Pts',(40.9451517822235,-6.97510377791315,-6.94867494071292));
#67593=CARTESIAN_POINT('Ctrl Pts',(41.0248921345258,-6.9687820472668,-7.00453677843929));
#67594=CARTESIAN_POINT('Ctrl Pts',(41.1017545025994,-6.96246031662045,-7.06393103210355));
#67595=CARTESIAN_POINT('Ctrl Pts',(41.1787401138824,-6.95612844953942,-7.12342052012791));
#67596=CARTESIAN_POINT('Ctrl Pts',(41.2528381934284,-6.94979658245839,-7.18645345087234));
#67597=CARTESIAN_POINT('Ctrl Pts',(41.3237238654314,-6.94346471537735,-7.25270433343348));
#67598=CARTESIAN_POINT('Ctrl Pts',(41.3648954299389,-6.93978706280508,-7.29118393598174));
#67599=CARTESIAN_POINT('Ctrl Pts',(41.4049840050208,-6.9361094102328,-7.33074843506157));
#67600=CARTESIAN_POINT('Ctrl Pts',(41.4439321912292,-6.93243175766053,-7.37132895407274));
#67601=CARTESIAN_POINT('Ctrl Pts',(41.5109978163644,-6.92609913751051,-7.44120532421315));
#67602=CARTESIAN_POINT('Ctrl Pts',(41.574912884085,-6.9197665173605,-7.51433869978135));
#67603=CARTESIAN_POINT('Ctrl Pts',(41.6353450654081,-6.91343389721048,-7.59041346399488));
#67604=CARTESIAN_POINT('Ctrl Pts',(41.6956959146744,-6.90710979975502,-7.6663858437351));
#67605=CARTESIAN_POINT('Ctrl Pts',(41.7525729242711,-6.90078570229956,-7.74529140461175));
#67606=CARTESIAN_POINT('Ctrl Pts',(41.8056809855595,-6.8944616048441,-7.82677820812661));
#67607=CARTESIAN_POINT('Ctrl Pts',(41.8587334585644,-6.88814412683046,-7.9081797192881));
#67608=CARTESIAN_POINT('Ctrl Pts',(41.9080245885148,-6.88182664881682,-7.99215673735205));
#67609=CARTESIAN_POINT('Ctrl Pts',(41.9533005411212,-6.87550917080318,-8.07832561259919));
#67610=CARTESIAN_POINT('Ctrl Pts',(41.9985443553659,-6.86919617714343,-8.16443332234162));
#67611=CARTESIAN_POINT('Ctrl Pts',(42.0397784556136,-6.86288318348368,-8.25272941011052));
#67612=CARTESIAN_POINT('Ctrl Pts',(42.0767937298344,-6.85657018982393,-8.34280353202805));
#67613=CARTESIAN_POINT('Ctrl Pts',(42.1137956278501,-6.85025947748994,-8.43284510387106));
#67614=CARTESIAN_POINT('Ctrl Pts',(42.1465815630955,-6.84394876515594,-8.5246630290721));
#67615=CARTESIAN_POINT('Ctrl Pts',(42.1749899730535,-6.83763805282195,-8.6178256434779));
#67616=CARTESIAN_POINT('Ctrl Pts',(42.2033958115229,-6.8313279117246,-8.71097982493722));
#67617=CARTESIAN_POINT('Ctrl Pts',(42.227424785183,-6.82501777062725,-8.80547803523857));
#67618=CARTESIAN_POINT('Ctrl Pts',(42.2469650836379,-6.8187076295299,-8.90087306419978));
#67619=CARTESIAN_POINT('Ctrl Pts',(42.2665089057679,-6.81239635053354,-8.9962852956145));
#67620=CARTESIAN_POINT('Ctrl Pts',(42.2815623573302,-6.80608507153719,-9.09259423847046));
#67621=CARTESIAN_POINT('Ctrl Pts',(42.292064863898,-6.79977379254083,-9.18934313600433));
#67622=CARTESIAN_POINT('Ctrl Pts',(42.3025786021932,-6.79345576405426,-9.28619550000468));
#67623=CARTESIAN_POINT('Ctrl Pts',(42.3085316316604,-6.7871377355677,-9.38348832253946));
#67624=CARTESIAN_POINT('Ctrl Pts',(42.3099153568417,-6.78081970708113,-9.48076058115117));
#67625=CARTESIAN_POINT('Ctrl Pts',(42.3112998928413,-6.77449797643398,-9.578089838164));
#67626=CARTESIAN_POINT('Ctrl Pts',(42.3081098073144,-6.76817624578682,-9.67539807037417));
#67627=CARTESIAN_POINT('Ctrl Pts',(42.3003885814515,-6.76185451513967,-9.77222721716105));
#67628=CARTESIAN_POINT('Ctrl Pts',(42.2926549751652,-6.75552264805783,-9.86921162243274));
#67629=CARTESIAN_POINT('Ctrl Pts',(42.280375776071,-6.74919078097599,-9.96571497482189));
#67630=CARTESIAN_POINT('Ctrl Pts',(42.2636459609728,-6.74285891389416,-10.0612873098584));
#67631=CARTESIAN_POINT('Ctrl Pts',(42.2539290091472,-6.73918126132962,-10.1167972942758));
#67632=CARTESIAN_POINT('Ctrl Pts',(42.2427116025523,-6.73550360876508,-10.1719934283378));
#67633=CARTESIAN_POINT('Ctrl Pts',(42.2300200415556,-6.73182595620054,-10.2267899975574));
#67634=CARTESIAN_POINT('Ctrl Pts',(42.2081662004202,-6.72549333605104,-10.3211452560473));
#67635=CARTESIAN_POINT('Ctrl Pts',(42.1818628489603,-6.71916071590154,-10.4146426367809));
#67636=CARTESIAN_POINT('Ctrl Pts',(42.1511926215263,-6.71282809575204,-10.506831331517));
#67637=CARTESIAN_POINT('Ctrl Pts',(42.1205636713164,-6.70650399829711,-10.5988959550047));
#67638=CARTESIAN_POINT('Ctrl Pts',(42.0855796630611,-6.70017990084217,-10.6896549816782));
#67639=CARTESIAN_POINT('Ctrl Pts',(42.0463739915869,-6.69385580338724,-10.778668916787));
#67640=CARTESIAN_POINT('Ctrl Pts',(42.0072093567449,-6.68753832537413,-10.8675896808831));
#67641=CARTESIAN_POINT('Ctrl Pts',(41.9638320188586,-6.68122084736102,-10.9547685866518));
#67642=CARTESIAN_POINT('Ctrl Pts',(41.9164244884842,-6.67490336934791,-11.039783367767));
#67643=CARTESIAN_POINT('Ctrl Pts',(41.8690506095358,-6.6685903756887,-11.1247378025913));
#67644=CARTESIAN_POINT('Ctrl Pts',(41.8176524378495,-6.66227738202948,-11.2075307858949));
#67645=CARTESIAN_POINT('Ctrl Pts',(41.7624592832083,-6.65596438837028,-11.2877629094123));
#67646=CARTESIAN_POINT('Ctrl Pts',(41.7072860737107,-6.64965367603682,-11.3679660394569));
#67647=CARTESIAN_POINT('Ctrl Pts',(41.6483208538315,-6.64334296370337,-11.4456097886015));
#67648=CARTESIAN_POINT('Ctrl Pts',(41.5858367780203,-6.63703225136992,-11.5203229115974));
#67649=CARTESIAN_POINT('Ctrl Pts',(41.5233583581783,-6.63072211027312,-11.5950292716684));
#67650=CARTESIAN_POINT('Ctrl Pts',(41.4573619964096,-6.62441196917632,-11.6668051976961));
#67651=CARTESIAN_POINT('Ctrl Pts',(41.3881610605712,-6.61810182807952,-11.7353126081846));
#67652=CARTESIAN_POINT('Ctrl Pts',(41.3189476458239,-6.61179054908371,-11.8038323725195));
#67653=CARTESIAN_POINT('Ctrl Pts',(41.2465288200725,-6.6054792700879,-11.8690821430423));
#67654=CARTESIAN_POINT('Ctrl Pts',(41.1712539518533,-6.5991679910921,-11.9307615239676));
#67655=CARTESIAN_POINT('Ctrl Pts',(41.0958985822038,-6.59284996260608,-11.9925068668601));
#67656=CARTESIAN_POINT('Ctrl Pts',(41.0176814110704,-6.58653193412006,-12.050673919519));
#67657=CARTESIAN_POINT('Ctrl Pts',(40.9369837916899,-6.58021390563404,-12.1050034806772));
#67658=CARTESIAN_POINT('Ctrl Pts',(40.8562388861115,-6.57389217498744,-12.1593648772031));
#67659=CARTESIAN_POINT('Ctrl Pts',(40.7730110117137,-6.56757044434084,-12.2098840777438));
#67660=CARTESIAN_POINT('Ctrl Pts',(40.6877075076263,-6.56124871369424,-12.2563471080498));
#67661=CARTESIAN_POINT('Ctrl Pts',(40.6022672255828,-6.55491684661295,-12.3028846384411));
#67662=CARTESIAN_POINT('Ctrl Pts',(40.5147450613693,-6.54858497953166,-12.3453528209146));
#67663=CARTESIAN_POINT('Ctrl Pts',(40.4255697230247,-6.54225311245038,-12.3835852282039));
#67664=CARTESIAN_POINT('Ctrl Pts',(40.3737752194401,-6.53857545988044,-12.4057912393404));
#67665=CARTESIAN_POINT('Ctrl Pts',(40.3214233513951,-6.53489780731049,-12.4265692408719));
#67666=CARTESIAN_POINT('Ctrl Pts',(40.2686002708934,-6.53122015474055,-12.4458944030804));
#67667=CARTESIAN_POINT('Ctrl Pts',(40.1776432004288,-6.52488753459096,-12.4791707687154));
#67668=CARTESIAN_POINT('Ctrl Pts',(40.0849723144736,-6.51855491444136,-12.5082522645267));
#67669=CARTESIAN_POINT('Ctrl Pts',(39.9910102810063,-6.51222229429177,-12.5329616666843));
#67670=CARTESIAN_POINT('Ctrl Pts',(39.8971747054179,-6.50589819683673,-12.557637813936));
#67671=CARTESIAN_POINT('Ctrl Pts',(39.8020518553959,-6.4995740993817,-12.5779534522547));
#67672=CARTESIAN_POINT('Ctrl Pts',(39.7060826718468,-6.49325000192667,-12.5937800478621));
#67673=CARTESIAN_POINT('Ctrl Pts',(39.6102139393791,-6.48693252391347,-12.6095900777492));
#67674=CARTESIAN_POINT('Ctrl Pts',(39.513501063732,-6.48061504590026,-12.620920335358));
#67675=CARTESIAN_POINT('Ctrl Pts',(39.4163974066349,-6.47429756788705,-12.6276928328956));
#67676=CARTESIAN_POINT('Ctrl Pts',(39.3193626769108,-6.46798457422775,-12.6344605230914));
#67677=CARTESIAN_POINT('Ctrl Pts',(39.2219381522197,-6.46167158056845,-12.6366768547426));
#67678=CARTESIAN_POINT('Ctrl Pts',(39.1245836347157,-6.45535858690914,-12.6343155235111));
#67679=CARTESIAN_POINT('Ctrl Pts',(39.0272642982019,-6.44904787457559,-12.6319550455936));
#67680=CARTESIAN_POINT('Ctrl Pts',(38.9300153553479,-6.44273716224204,-12.6250202023584));
#67681=CARTESIAN_POINT('Ctrl Pts',(38.8332969914423,-6.4364264499085,-12.6135367986175));
#67682=CARTESIAN_POINT('Ctrl Pts',(38.7365873823446,-6.4301163088116,-12.602054434338));
#67683=CARTESIAN_POINT('Ctrl Pts',(38.6404086909423,-6.4238061677147,-12.5860243799323));
#67684=CARTESIAN_POINT('Ctrl Pts',(38.5452153132195,-6.4174960266178,-12.5655242421099));
#67685=CARTESIAN_POINT('Ctrl Pts',(38.4500047694067,-6.4111847476219,-12.5450204075259));
#67686=CARTESIAN_POINT('Ctrl Pts',(38.3557803196677,-6.404873468626,-12.52004498064));
#67687=CARTESIAN_POINT('Ctrl Pts',(38.2629844813214,-6.39856218963009,-12.490726314186));
#67688=CARTESIAN_POINT('Ctrl Pts',(38.1700894040406,-6.39224416114398,-12.4613762933818));
#67689=CARTESIAN_POINT('Ctrl Pts',(38.0786264060121,-6.38592613265787,-12.4276738918791));
#67690=CARTESIAN_POINT('Ctrl Pts',(37.9890209924694,-6.37960810417175,-12.3897967635105));
#67691=CARTESIAN_POINT('Ctrl Pts',(37.8993630730492,-6.37328637352506,-12.3518974403684));
#67692=CARTESIAN_POINT('Ctrl Pts',(37.8115652997706,-6.36696464287836,-12.3098187081198));
#67693=CARTESIAN_POINT('Ctrl Pts',(37.7260295099797,-6.36064291223166,-12.2637847026463));
#67694=CARTESIAN_POINT('Ctrl Pts',(37.6403565697794,-6.35431104515028,-12.2176768849977));
#67695=CARTESIAN_POINT('Ctrl Pts',(37.5569532300908,-6.3479791780689,-12.1676013552421));
#67696=CARTESIAN_POINT('Ctrl Pts',(37.4761931939458,-6.34164731098752,-12.1138261332699));
#67697=CARTESIAN_POINT('Ctrl Pts',(37.4292864363366,-6.33796965841854,-12.0825925996705));
#67698=CARTESIAN_POINT('Ctrl Pts',(37.3832708016008,-6.33429200584956,-12.0501117623405));
#67699=CARTESIAN_POINT('Ctrl Pts',(37.3382141739985,-6.33061435328058,-12.016442190981));
#67700=CARTESIAN_POINT('Ctrl Pts',(37.2613403634718,-6.32433968999983,-11.9589965190133));
#67701=CARTESIAN_POINT('Ctrl Pts',(37.1869821423794,-6.31806502671907,-11.8978805724172));
#67702=CARTESIAN_POINT('Ctrl Pts',(37.115515165223,-6.31179036343831,-11.8333443474674));
#67703=CARTESIAN_POINT('Ctrl Pts',(37.0441447272916,-6.30552417611602,-11.7688952995242));
#67704=CARTESIAN_POINT('Ctrl Pts',(36.975658102416,-6.29925798879374,-11.7010354484271));
#67705=CARTESIAN_POINT('Ctrl Pts',(36.9104005139929,-6.29299180147145,-11.6300569699122));
#67706=CARTESIAN_POINT('Ctrl Pts',(36.8452155369337,-6.28673258646332,-11.5591574683294));
#67707=CARTESIAN_POINT('Ctrl Pts',(36.783252753632,-6.2804733714552,-11.4851465648293));
#67708=CARTESIAN_POINT('Ctrl Pts',(36.7248220139306,-6.27421415644708,-11.4083546108414));
#67709=CARTESIAN_POINT('Ctrl Pts',(36.6664270297752,-6.2679587716429,-11.3316096481846));
#67710=CARTESIAN_POINT('Ctrl Pts',(36.6115600668311,-6.26170338683871,-11.2520873684212));
#67711=CARTESIAN_POINT('Ctrl Pts',(36.5604914148224,-6.25544800203453,-11.1701519934868));
#67712=CARTESIAN_POINT('Ctrl Pts',(36.5094395360291,-6.24919467177677,-11.0882435297717));
#67713=CARTESIAN_POINT('Ctrl Pts',(36.4621837258304,-6.24294134151901,-11.0039239236958));
#67714=CARTESIAN_POINT('Ctrl Pts',(36.4189508886379,-6.23668801126125,-10.917586260557));
#67715=CARTESIAN_POINT('Ctrl Pts',(36.3757199953772,-6.23043496217974,-10.8312524795257));
#67716=CARTESIAN_POINT('Ctrl Pts',(36.3365119143669,-6.22418191309823,-10.7429012213437));
#67717=CARTESIAN_POINT('Ctrl Pts',(36.3015069900995,-6.21792886401671,-10.6529489901842));
#67718=CARTESIAN_POINT('Ctrl Pts',(36.2664716805982,-6.21167038711718,-10.5629186780223));
#67719=CARTESIAN_POINT('Ctrl Pts',(36.2356469794486,-6.20541191021766,-10.4712850331532));
#67720=CARTESIAN_POINT('Ctrl Pts',(36.2091644294996,-6.19915343331813,-10.3784830069365));
#67721=CARTESIAN_POINT('Ctrl Pts',(36.1826710455795,-6.1928923960852,-10.2856430155517));
#67722=CARTESIAN_POINT('Ctrl Pts',(36.1605234540233,-6.18663135885228,-10.1916341254886));
#67723=CARTESIAN_POINT('Ctrl Pts',(36.142802276078,-6.18037032161936,-10.096902727521));
#67724=CARTESIAN_POINT('Ctrl Pts',(36.1250519834966,-6.17409899794718,-10.0020156925982));
#67725=CARTESIAN_POINT('Ctrl Pts',(36.1117426976542,-6.167827674275,-9.90640422079789));
#67726=CARTESIAN_POINT('Ctrl Pts',(36.1029032457584,-6.16155635060282,-9.81052118619469));
#67727=CARTESIAN_POINT('Ctrl Pts',(36.094104887165,-6.15531418138539,-9.71508389761573));
#67728=CARTESIAN_POINT('Ctrl Pts',(36.0897348207007,-6.14907201216796,-9.61937800194409));
#67729=CARTESIAN_POINT('Ctrl Pts',(36.0897702134563,-6.14282984295053,-9.52384769963273));
#67730=CARTESIAN_POINT('',(36.0897712021404,-4.87282984294947,-9.52773456847233));
#67731=CARTESIAN_POINT('Ctrl Pts',(36.0897702134565,-6.14282984291314,-9.52384769906051));
#67732=CARTESIAN_POINT('Ctrl Pts',(36.0897944454732,-6.13855607921562,-9.458441920427));
#67733=CARTESIAN_POINT('Ctrl Pts',(36.0918816780826,-6.13428231551811,-9.39307717011422));
#67734=CARTESIAN_POINT('Ctrl Pts',(36.096025077601,-6.1300085518206,-9.32784439135976));
#67735=CARTESIAN_POINT('Ctrl Pts',(36.1021645315192,-6.12367593167103,-9.23118616727646));
#67736=CARTESIAN_POINT('Ctrl Pts',(36.1128338748575,-6.11734331152145,-9.13464709945906));
#67737=CARTESIAN_POINT('Ctrl Pts',(36.1280252602644,-6.11101069137187,-9.03868543993983));
#67738=CARTESIAN_POINT('Ctrl Pts',(36.1431962004947,-6.10468659391685,-8.94285292947643));
#67739=CARTESIAN_POINT('Ctrl Pts',(36.1628770188918,-6.09836249646183,-8.84759671107667));
#67740=CARTESIAN_POINT('Ctrl Pts',(36.18700794114,-6.0920383990068,-8.75337217122086));
#67741=CARTESIAN_POINT('Ctrl Pts',(36.2111136055174,-6.0857209209936,-8.65924625632523));
#67742=CARTESIAN_POINT('Ctrl Pts',(36.2396600056321,-6.07940344298039,-8.56615029457657));
#67743=CARTESIAN_POINT('Ctrl Pts',(36.2725360961542,-6.07308596496719,-8.47453070269516));
#67744=CARTESIAN_POINT('Ctrl Pts',(36.3053888501448,-6.06677297130788,-8.38297614541677));
#67745=CARTESIAN_POINT('Ctrl Pts',(36.3425650372436,-6.06045997764858,-8.29289628501466));
#67746=CARTESIAN_POINT('Ctrl Pts',(36.3839037064072,-6.05414698398928,-8.20472263591588));
#67747=CARTESIAN_POINT('Ctrl Pts',(36.425227437021,-6.04783627165573,-8.11658085011804));
#67748=CARTESIAN_POINT('Ctrl Pts',(36.4707104753977,-6.04152555932218,-8.03034430243137));
#67749=CARTESIAN_POINT('Ctrl Pts',(36.5201440126228,-6.03521484698863,-7.9464238884937));
#67750=CARTESIAN_POINT('Ctrl Pts',(36.5695730751947,-6.02890470589173,-7.86251107091183));
#67751=CARTESIAN_POINT('Ctrl Pts',(36.6229517035027,-6.02259456479483,-7.78091434693321));
#67752=CARTESIAN_POINT('Ctrl Pts',(36.680025995923,-6.01628442369793,-7.70201846644678));
#67753=CARTESIAN_POINT('Ctrl Pts',(36.7371105804714,-6.00997314470202,-7.62310835877551));
#67754=CARTESIAN_POINT('Ctrl Pts',(36.7978918964089,-6.00366186570612,-7.5469004162128));
#67755=CARTESIAN_POINT('Ctrl Pts',(36.8620743664621,-5.99735058671021,-7.4737480932498));
#67756=CARTESIAN_POINT('Ctrl Pts',(36.9263254753686,-5.99103255822409,-7.40051753877649));
#67757=CARTESIAN_POINT('Ctrl Pts',(36.9939847111832,-5.98471452973798,-7.3303494571126));
#67758=CARTESIAN_POINT('Ctrl Pts',(37.0647182095184,-5.97839650125186,-7.26356188938593));
#67759=CARTESIAN_POINT('Ctrl Pts',(37.1354931553986,-5.97207477060516,-7.19673518630221));
#67760=CARTESIAN_POINT('Ctrl Pts',(37.2093456193398,-5.96575303995846,-7.13329322644822));
#67761=CARTESIAN_POINT('Ctrl Pts',(37.2859087089586,-5.95943130931176,-7.07351367891653));
#67762=CARTESIAN_POINT('Ctrl Pts',(37.3625945619155,-5.95309944223037,-7.01363827923407));
#67763=CARTESIAN_POINT('Ctrl Pts',(37.4419993626041,-5.94676757514898,-6.95743727053224));
#67764=CARTESIAN_POINT('Ctrl Pts',(37.5237273663984,-5.9404357080676,-6.90514490653809));
#67765=CARTESIAN_POINT('Ctrl Pts',(37.571196335543,-5.93675805549859,-6.87477264124715));
#67766=CARTESIAN_POINT('Ctrl Pts',(37.6194485560584,-5.93308040292958,-6.84571809514552));
#67767=CARTESIAN_POINT('Ctrl Pts',(37.6684030922134,-5.92940275036057,-6.81801984400356));
#67768=CARTESIAN_POINT('Ctrl Pts',(37.7526988423567,-5.92307013021093,-6.77032569671804));
#67769=CARTESIAN_POINT('Ctrl Pts',(37.8393709364328,-5.91673751006129,-6.72648992809303));
#67770=CARTESIAN_POINT('Ctrl Pts',(37.9280313531574,-5.91040488991165,-6.68675645612477));
#67771=CARTESIAN_POINT('Ctrl Pts',(38.0165724471319,-5.90408079245658,-6.64707645905908));
#67772=CARTESIAN_POINT('Ctrl Pts',(38.1070961494503,-5.8977566950015,-6.61148796266889));
#67773=CARTESIAN_POINT('Ctrl Pts',(38.1991884541281,-5.89143259754643,-6.58018983590632));
#67774=CARTESIAN_POINT('Ctrl Pts',(38.2911843656593,-5.88511511953318,-6.54892446893764));
#67775=CARTESIAN_POINT('Ctrl Pts',(38.3847452035775,-5.87879764151992,-6.52194068377684));
#67776=CARTESIAN_POINT('Ctrl Pts',(38.4794364473037,-5.87248016350667,-6.499389512937));
#67777=CARTESIAN_POINT('Ctrl Pts',(38.5740604760673,-5.86616716984732,-6.47685434966073));
#67778=CARTESIAN_POINT('Ctrl Pts',(38.6698128912126,-5.85985417618798,-6.45874564647037));
#67779=CARTESIAN_POINT('Ctrl Pts',(38.7662443716592,-5.85354118252863,-6.44516449988272));
#67780=CARTESIAN_POINT('Ctrl Pts',(38.8626410046733,-5.84723047019504,-6.43158826111238));
#67781=CARTESIAN_POINT('Ctrl Pts',(38.9597157827883,-5.84091975786145,-6.42253638887785));
#67782=CARTESIAN_POINT('Ctrl Pts',(39.0570104906991,-5.83460904552786,-6.41805863377986));
#67783=CARTESIAN_POINT('Ctrl Pts',(39.1542963916323,-5.82829890443091,-6.41358128400185));
#67784=CARTESIAN_POINT('Ctrl Pts',(39.2518017459218,-5.82198876333397,-6.41367724804504));
#67785=CARTESIAN_POINT('Ctrl Pts',(39.349065583702,-5.81567862223703,-6.41834422494935));
#67786=CARTESIAN_POINT('Ctrl Pts',(39.4463469609353,-5.80936734324108,-6.42301204344313));
#67787=CARTESIAN_POINT('Ctrl Pts',(39.5433862983558,-5.80305606424513,-6.43225249093647));
#67788=CARTESIAN_POINT('Ctrl Pts',(39.6397260515868,-5.79674478524918,-6.44601126139509));
#67789=CARTESIAN_POINT('Ctrl Pts',(39.7361688337319,-5.79042675676303,-6.45978474593726));
#67790=CARTESIAN_POINT('Ctrl Pts',(39.8319101043967,-5.78410872827687,-6.47808613842611));
#67791=CARTESIAN_POINT('Ctrl Pts',(39.9265010452396,-5.77779069979071,-6.5008097142928));
#67792=CARTESIAN_POINT('Ctrl Pts',(40.021147413318,-5.77146896914397,-6.52354660544084));
#67793=CARTESIAN_POINT('Ctrl Pts',(40.1146416895832,-5.76514723849724,-6.55071071790727));
#67794=CARTESIAN_POINT('Ctrl Pts',(40.2065508087619,-5.7588255078505,-6.58214660197272));
#67795=CARTESIAN_POINT('Ctrl Pts',(40.2986072975196,-5.75249364076907,-6.61363289118881));
#67796=CARTESIAN_POINT('Ctrl Pts',(40.3890731474761,-5.74616177368765,-6.64940446849916));
#67797=CARTESIAN_POINT('Ctrl Pts',(40.4775358774011,-5.73982990660623,-6.68925799219093));
#67798=CARTESIAN_POINT('Ctrl Pts',(40.5289164862711,-5.7361522540377,-6.71240557439457));
#67799=CARTESIAN_POINT('Ctrl Pts',(40.5796218014761,-5.73247460146918,-6.73692932702247));
#67800=CARTESIAN_POINT('Ctrl Pts',(40.6295752793794,-5.72879694890065,-6.76278256223605));
#67801=CARTESIAN_POINT('Ctrl Pts',(40.715591126396,-5.72246432875102,-6.80729974138662));
#67802=CARTESIAN_POINT('Ctrl Pts',(40.7996749930196,-5.7161317086014,-6.85591588969245));
#67803=CARTESIAN_POINT('Ctrl Pts',(40.881410527064,-5.70979908845177,-6.90843941549633));
#67804=CARTESIAN_POINT('Ctrl Pts',(40.9630360581437,-5.7034749909967,-6.96089225302942));
#67805=CARTESIAN_POINT('Ctrl Pts',(41.0423191734523,-5.69715089354164,-7.01724178172022));
#67806=CARTESIAN_POINT('Ctrl Pts',(41.1188670403116,-5.69082679608657,-7.0772500261453));
#67807=CARTESIAN_POINT('Ctrl Pts',(41.1953347844096,-5.68450931807333,-7.13719545985538));
#67808=CARTESIAN_POINT('Ctrl Pts',(41.2690726294599,-5.67819184006008,-7.20079172751996));
#67809=CARTESIAN_POINT('Ctrl Pts',(41.3397165864681,-5.67187436204684,-7.26775752687196));
#67810=CARTESIAN_POINT('Ctrl Pts',(41.4103103980697,-5.66556136838749,-7.33467579169472));
#67811=CARTESIAN_POINT('Ctrl Pts',(41.4778143712153,-5.65924837472814,-7.40495853315345));
#67812=CARTESIAN_POINT('Ctrl Pts',(41.5418982421559,-5.6529353810688,-7.47828475935532));
#67813=CARTESIAN_POINT('Ctrl Pts',(41.6059589551157,-5.64662466873521,-7.55158448766765));
#67814=CARTESIAN_POINT('Ctrl Pts',(41.6666017341748,-5.64031395640162,-7.62792518641353));
#67815=CARTESIAN_POINT('Ctrl Pts',(41.723534449953,-5.63400324406803,-7.70695034919272));
#67816=CARTESIAN_POINT('Ctrl Pts',(41.7804620122632,-5.62769310297109,-7.78596835872728));
#67817=CARTESIAN_POINT('Ctrl Pts',(41.8336799235433,-5.62138296187415,-7.86766999422618));
#67818=CARTESIAN_POINT('Ctrl Pts',(41.8829381357321,-5.61507282077721,-7.95166799030393));
#67819=CARTESIAN_POINT('Ctrl Pts',(41.9322052305862,-5.60876154178126,-8.03568113362403));
#67820=CARTESIAN_POINT('Ctrl Pts',(41.9775109869771,-5.60245026278531,-8.12199108273024));
#67821=CARTESIAN_POINT('Ctrl Pts',(42.0186507773681,-5.59613898378937,-8.21018501372167));
#67822=CARTESIAN_POINT('Ctrl Pts',(42.0598345640097,-5.58982095530321,-8.29847326221576));
#67823=CARTESIAN_POINT('Ctrl Pts',(42.0968433048717,-5.58350292681706,-8.38864911804939));
#67824=CARTESIAN_POINT('Ctrl Pts',(42.1295201991624,-5.5771848983309,-8.48027895799909));
#67825=CARTESIAN_POINT('Ctrl Pts',(42.1622162410575,-5.57086316768416,-8.57196249007483));
#67826=CARTESIAN_POINT('Ctrl Pts',(42.1905752545655,-5.56454143703742,-8.6651012846412));
#67827=CARTESIAN_POINT('Ctrl Pts',(42.2144906887407,-5.55821970639069,-8.75924772909551));
#67828=CARTESIAN_POINT('Ctrl Pts',(42.2384444695729,-5.55188783930926,-8.85354513051687));
#67829=CARTESIAN_POINT('Ctrl Pts',(42.2579403562005,-5.54555597222784,-8.94885297991142));
#67830=CARTESIAN_POINT('Ctrl Pts',(42.272923153174,-5.53922410514642,-9.04471472270413));
#67831=CARTESIAN_POINT('Ctrl Pts',(42.2816254081433,-5.53554645257782,-9.1003927999724));
#67832=CARTESIAN_POINT('Ctrl Pts',(42.2888061551775,-5.53186880000923,-9.15625763958687));
#67833=CARTESIAN_POINT('Ctrl Pts',(42.2944626496101,-5.52819114744063,-9.21221962486703));
#67834=CARTESIAN_POINT('Ctrl Pts',(42.3042026753334,-5.521858527291,-9.30858163541264));
#67835=CARTESIAN_POINT('Ctrl Pts',(42.309454243118,-5.51552590714138,-9.40556641534358));
#67836=CARTESIAN_POINT('Ctrl Pts',(42.3101502022979,-5.50919328699175,-9.50272059142064));
#67837=CARTESIAN_POINT('Ctrl Pts',(42.3108452248279,-5.50286918953669,-9.59974401350508));
#67838=CARTESIAN_POINT('Ctrl Pts',(42.306996821536,-5.49654509208163,-9.69693594500563));
#67839=CARTESIAN_POINT('Ctrl Pts',(42.2985895388713,-5.49022099462656,-9.79383735324039));
#67840=CARTESIAN_POINT('Ctrl Pts',(42.2901910561214,-5.48390351661333,-9.89063733463299));
#67841=CARTESIAN_POINT('Ctrl Pts',(42.2772432181393,-5.47758603860009,-9.98714696391991));
#67842=CARTESIAN_POINT('Ctrl Pts',(42.2597826189743,-5.47126856058685,-10.0829076783148));
#67843=CARTESIAN_POINT('Ctrl Pts',(42.2423344139175,-5.46495556692751,-10.1786004186017));
#67844=CARTESIAN_POINT('Ctrl Pts',(42.2203798942647,-5.45864257326817,-10.2735448718582));
#67845=CARTESIAN_POINT('Ctrl Pts',(42.1940073242801,-5.45232957960883,-10.367289021095));
#67846=CARTESIAN_POINT('Ctrl Pts',(42.1676442845479,-5.44601886727525,-10.4609992940199));
#67847=CARTESIAN_POINT('Ctrl Pts',(42.1368664851563,-5.43970815494167,-10.5535097042536));
#67848=CARTESIAN_POINT('Ctrl Pts',(42.1018127745279,-5.43339744260809,-10.6443807549206));
#67849=CARTESIAN_POINT('Ctrl Pts',(42.0667622369112,-5.42708730151116,-10.7352435800702));
#67850=CARTESIAN_POINT('Ctrl Pts',(42.0274367151852,-5.42077716041423,-10.8244669327597));
#67851=CARTESIAN_POINT('Ctrl Pts',(41.984023817222,-5.41446701931729,-10.911629740789));
#67852=CARTESIAN_POINT('Ctrl Pts',(41.9406030906711,-5.40815574032136,-10.9988082667667));
#67853=CARTESIAN_POINT('Ctrl Pts',(41.893093718963,-5.40184446132542,-11.0839251186632));
#67854=CARTESIAN_POINT('Ctrl Pts',(41.8417295399151,-5.39553318232948,-11.166583287817));
#67855=CARTESIAN_POINT('Ctrl Pts',(41.7903104303177,-5.38921515384333,-11.2493298543469));
#67856=CARTESIAN_POINT('Ctrl Pts',(41.7350285143128,-5.38289712535718,-11.3296121166364));
#67857=CARTESIAN_POINT('Ctrl Pts',(41.6761611896886,-5.37657909687103,-11.4070617459531));
#67858=CARTESIAN_POINT('Ctrl Pts',(41.617259370714,-5.3702573662243,-11.4845567582504));
#67859=CARTESIAN_POINT('Ctrl Pts',(41.5547682401544,-5.36393563557758,-11.5592154972016));
#67860=CARTESIAN_POINT('Ctrl Pts',(41.4890043777611,-5.35761390493085,-11.6307040655065));
#67861=CARTESIAN_POINT('Ctrl Pts',(41.423135067804,-5.35128203784943,-11.7023072605241));
#67862=CARTESIAN_POINT('Ctrl Pts',(41.3539828581687,-5.34495017076802,-11.7707298273728));
#67863=CARTESIAN_POINT('Ctrl Pts',(41.2818998883338,-5.3386183036866,-11.8356759850433));
#67864=CARTESIAN_POINT('Ctrl Pts',(41.2400329135915,-5.33494065111796,-11.8733977818703));
#67865=CARTESIAN_POINT('Ctrl Pts',(41.1971778625174,-5.33126299854931,-11.9099475839306));
#67866=CARTESIAN_POINT('Ctrl Pts',(41.1534082781751,-5.32758534598067,-11.9452741067195));
#67867=CARTESIAN_POINT('Ctrl Pts',(41.0780405955099,-5.32125272583104,-12.0061035205517));
#67868=CARTESIAN_POINT('Ctrl Pts',(40.9996979413289,-5.31492010568141,-12.0635148002651));
#67869=CARTESIAN_POINT('Ctrl Pts',(40.9187232561712,-5.30858748553178,-12.1172038927515));
#67870=CARTESIAN_POINT('Ctrl Pts',(40.8378575499975,-5.30226338807672,-12.1708207283007));
#67871=CARTESIAN_POINT('Ctrl Pts',(40.7543672147178,-5.29593929062166,-12.2207250935565));
#67872=CARTESIAN_POINT('Ctrl Pts',(40.6686281886044,-5.2896151931666,-12.2666531320604));
#67873=CARTESIAN_POINT('Ctrl Pts',(40.5829789056518,-5.28329771515335,-12.312533097621));
#67874=CARTESIAN_POINT('Ctrl Pts',(40.4950859946145,-5.2769802371401,-12.3544448053281));
#67875=CARTESIAN_POINT('Ctrl Pts',(40.4053534504851,-5.27066275912686,-12.3921682392744));
#67876=CARTESIAN_POINT('Ctrl Pts',(40.31568460147,-5.26434976546752,-12.4298648958852));
#67877=CARTESIAN_POINT('Ctrl Pts',(40.2241791174292,-5.25803677180818,-12.4633790201888));
#67878=CARTESIAN_POINT('Ctrl Pts',(40.1312637559423,-5.25172377814884,-12.4925374420162));
#67879=CARTESIAN_POINT('Ctrl Pts',(40.0383819712683,-5.24541306581526,-12.5216853268683));
#67880=CARTESIAN_POINT('Ctrl Pts',(39.9440917383314,-5.23910235348167,-12.546480506031));
#67881=CARTESIAN_POINT('Ctrl Pts',(39.8488369808566,-5.23279164114809,-12.5667990113045));
#67882=CARTESIAN_POINT('Ctrl Pts',(39.753590845706,-5.22648150005116,-12.587115677376));
#67883=CARTESIAN_POINT('Ctrl Pts',(39.6573807873376,-5.22017135895423,-12.6029563842081));
#67884=CARTESIAN_POINT('Ctrl Pts',(39.560661953831,-5.2138612178573,-12.614248065138));
#67885=CARTESIAN_POINT('Ctrl Pts',(39.4639256791511,-5.20754993886136,-12.625541782281));
#67886=CARTESIAN_POINT('Ctrl Pts',(39.3666808814735,-5.20123865986541,-12.6322847935888));
#67887=CARTESIAN_POINT('Ctrl Pts',(39.2693878286774,-5.19492738086947,-12.6344558980843));
#67888=CARTESIAN_POINT('Ctrl Pts',(39.1719907274772,-5.18860935238332,-12.6366293244307));
#67889=CARTESIAN_POINT('Ctrl Pts',(39.0745457060551,-5.18229132389718,-12.6342210728767));
#67890=CARTESIAN_POINT('Ctrl Pts',(38.977512826952,-5.17597329541103,-12.6272620957503));
#67891=CARTESIAN_POINT('Ctrl Pts',(38.8804230897165,-5.16965156476429,-12.6202990408882));
#67892=CARTESIAN_POINT('Ctrl Pts',(38.7837464097462,-5.16332983411757,-12.6087800022855));
#67893=CARTESIAN_POINT('Ctrl Pts',(38.6879354349393,-5.15700810347083,-12.5927875633931));
#67894=CARTESIAN_POINT('Ctrl Pts',(38.5919708342123,-5.15067623638942,-12.5767694817896));
#67895=CARTESIAN_POINT('Ctrl Pts',(38.4968751376486,-5.144344369308,-12.556263769252));
#67896=CARTESIAN_POINT('Ctrl Pts',(38.4030885128886,-5.13801250222659,-12.5314036213739));
#67897=CARTESIAN_POINT('Ctrl Pts',(38.3486156983116,-5.13433484965795,-12.5169644385033));
#67898=CARTESIAN_POINT('Ctrl Pts',(38.2945841892687,-5.13065719708931,-12.5010572242992));
#67899=CARTESIAN_POINT('Ctrl Pts',(38.241077130484,-5.12697954452068,-12.4837155292828));
#67900=CARTESIAN_POINT('Ctrl Pts',(38.1489423047267,-5.12064692437105,-12.4538545336504));
#67901=CARTESIAN_POINT('Ctrl Pts',(38.0580435855754,-5.11431430422142,-12.4196339351882));
#67902=CARTESIAN_POINT('Ctrl Pts',(37.9688230392589,-5.10798168407179,-12.3811747047826));
#67903=CARTESIAN_POINT('Ctrl Pts',(37.8797225695374,-5.10165758661673,-12.3427672343542));
#67904=CARTESIAN_POINT('Ctrl Pts',(37.7922961818727,-5.09533348916167,-12.3001326416317));
#67905=CARTESIAN_POINT('Ctrl Pts',(37.7069703197477,-5.0890093917066,-12.253441501441));
#67906=CARTESIAN_POINT('Ctrl Pts',(37.621733768324,-5.08269191369335,-12.2067992329333));
#67907=CARTESIAN_POINT('Ctrl Pts',(37.538593753088,-5.0763744356801,-12.1561090670222));
#67908=CARTESIAN_POINT('Ctrl Pts',(37.4579553425894,-5.07005695766685,-12.1015890367863));
#67909=CARTESIAN_POINT('Ctrl Pts',(37.3773741718898,-5.06374396400751,-12.047107706663));
#67910=CARTESIAN_POINT('Ctrl Pts',(37.2992914369405,-5.05743097034817,-11.9888021611274));
#67911=CARTESIAN_POINT('Ctrl Pts',(37.224085420997,-5.05111797668883,-11.9269351009932));
#67912=CARTESIAN_POINT('Ctrl Pts',(37.1489065822425,-5.04480726435524,-11.8650903977512));
#67913=CARTESIAN_POINT('Ctrl Pts',(37.0766027342587,-5.03849655202166,-11.7996870147826));
#67914=CARTESIAN_POINT('Ctrl Pts',(37.007520342822,-5.03218583968808,-11.7310289222403));
#67915=CARTESIAN_POINT('Ctrl Pts',(36.9384442046246,-5.02587569859115,-11.6623770445304));
#67916=CARTESIAN_POINT('Ctrl Pts',(36.8725892532328,-5.01956555749422,-11.5904713514222));
#67917=CARTESIAN_POINT('Ctrl Pts',(36.8102654658623,-5.01325541639729,-11.5156530358779));
#67918=CARTESIAN_POINT('Ctrl Pts',(36.7479304397294,-5.00694413740134,-11.4408212284502));
#67919=CARTESIAN_POINT('Ctrl Pts',(36.6891281221875,-5.0006328584054,-11.3630760914411));
#67920=CARTESIAN_POINT('Ctrl Pts',(36.6341278576655,-4.99432157940945,-11.2827914558023));
#67921=CARTESIAN_POINT('Ctrl Pts',(36.5790687740441,-4.9880035509233,-11.2024209611226));
#67922=CARTESIAN_POINT('Ctrl Pts',(36.5278201086319,-4.98168552243715,-11.119505907188));
#67923=CARTESIAN_POINT('Ctrl Pts',(36.4806074214034,-4.975367493951,-11.0344484609862));
#67924=CARTESIAN_POINT('Ctrl Pts',(36.4333670690655,-4.96904576330426,-10.9493411738688));
#67925=CARTESIAN_POINT('Ctrl Pts',(36.3901675981309,-4.96272403265752,-10.8620893864293));
#67926=CARTESIAN_POINT('Ctrl Pts',(36.3511872806435,-4.95640230201078,-10.7731172793183));
#67927=CARTESIAN_POINT('Ctrl Pts',(36.312144461056,-4.95007043492936,-10.6840025119134));
#67928=CARTESIAN_POINT('Ctrl Pts',(36.2773344600279,-4.94373856784794,-10.5931623248813));
#67929=CARTESIAN_POINT('Ctrl Pts',(36.2468863459858,-4.93740670076652,-10.5010381136896));
#67930=CARTESIAN_POINT('Ctrl Pts',(36.2292015804377,-4.93372904819791,-10.4475308562624));
#67931=CARTESIAN_POINT('Ctrl Pts',(36.2129873431153,-4.93005139562931,-10.3935906862479));
#67932=CARTESIAN_POINT('Ctrl Pts',(36.1982609879107,-4.9263737430607,-10.3393055668488));
#67933=CARTESIAN_POINT('Ctrl Pts',(36.1660748354605,-4.91833580803964,-10.2206591601533));
#67934=CARTESIAN_POINT('Ctrl Pts',(36.1409082916263,-4.91029787301858,-10.1000336223966));
#67935=CARTESIAN_POINT('Ctrl Pts',(36.1229598946395,-4.90225993799752,-9.97816094591516));
#67936=CARTESIAN_POINT('Ctrl Pts',(36.1053275701443,-4.89436355155888,-9.85843445555557));
#67937=CARTESIAN_POINT('Ctrl Pts',(36.0946614047826,-4.88646716512023,-9.73750420175503));
#67938=CARTESIAN_POINT('Ctrl Pts',(36.0911040387368,-4.87857077868159,-9.61608542661328));
#67939=CARTESIAN_POINT('Ctrl Pts',(36.0902419309021,-4.87665713343755,-9.58666026316763));
#67940=CARTESIAN_POINT('Ctrl Pts',(36.0897971143992,-4.87474348819351,-9.55720651418373));
#67941=CARTESIAN_POINT('Ctrl Pts',(36.0897712021404,-4.87282984294947,-9.52773456847233));
#67942=CARTESIAN_POINT('',(36.0898800655558,-3.60282980867964,-9.52346476277984));
#67943=CARTESIAN_POINT('Ctrl Pts',(36.0897712021399,-4.87282984291314,-9.52773456791281));
#67944=CARTESIAN_POINT('Ctrl Pts',(36.089686528353,-4.86657660100476,-9.43142873138466));
#67945=CARTESIAN_POINT('Ctrl Pts',(36.0940791608739,-4.86032335909639,-9.33502132983258));
#67946=CARTESIAN_POINT('Ctrl Pts',(36.1029506472896,-4.85407011718802,-9.23896510741516));
#67947=CARTESIAN_POINT('Ctrl Pts',(36.1118176278476,-4.84782005132219,-9.14295767227547));
#67948=CARTESIAN_POINT('Ctrl Pts',(36.1251589041781,-4.84156998545637,-9.04730150610461));
#67949=CARTESIAN_POINT('Ctrl Pts',(36.1429239802186,-4.83531991959055,-8.95244706604761));
#67950=CARTESIAN_POINT('Ctrl Pts',(36.1606850819456,-4.82907125195803,-8.85761384634896));
#67951=CARTESIAN_POINT('Ctrl Pts',(36.1828679350296,-4.82282258432551,-8.76358243547113));
#67952=CARTESIAN_POINT('Ctrl Pts',(36.2093706344023,-4.816573916693,-8.67079472576857));
#67953=CARTESIAN_POINT('Ctrl Pts',(36.2358749365348,-4.81032487117019,-8.5780014046978));
#67954=CARTESIAN_POINT('Ctrl Pts',(36.2666994798357,-4.80407582564738,-8.48645236351399));
#67955=CARTESIAN_POINT('Ctrl Pts',(36.3016923605483,-4.79782678012457,-8.39657477873092));
#67956=CARTESIAN_POINT('Ctrl Pts',(36.3367199778045,-4.79157153133306,-8.30660797475332));
#67957=CARTESIAN_POINT('Ctrl Pts',(36.3759240331927,-4.78531628254155,-8.2183163578517));
#67958=CARTESIAN_POINT('Ctrl Pts',(36.4191043846771,-4.77906103375005,-8.13210724405014));
#67959=CARTESIAN_POINT('Ctrl Pts',(36.4623064306282,-4.77280264222621,-8.04585481747588));
#67960=CARTESIAN_POINT('Ctrl Pts',(36.509488531073,-4.76654425070238,-7.96168736670024));
#67961=CARTESIAN_POINT('Ctrl Pts',(36.5604055732342,-4.76028585917854,-7.87998574015689));
#67962=CARTESIAN_POINT('Ctrl Pts',(36.6114083467711,-4.75401693011184,-7.79814654881139));
#67963=CARTESIAN_POINT('Ctrl Pts',(36.6661583687463,-4.74774800104514,-7.71878184229606));
#67964=CARTESIAN_POINT('Ctrl Pts',(36.7243683708865,-4.74147907197844,-7.64224173356406));
#67965=CARTESIAN_POINT('Ctrl Pts',(36.7729968220505,-4.7362420285192,-7.57830036949065));
#67966=CARTESIAN_POINT('Ctrl Pts',(36.8240391302687,-4.73100498505996,-7.51632976422507));
#67967=CARTESIAN_POINT('Ctrl Pts',(36.8773082980014,-4.72576794160072,-7.45651410196568));
#67968=CARTESIAN_POINT('Ctrl Pts',(36.9417212454141,-4.7194353214511,-7.3841851493734));
#67969=CARTESIAN_POINT('Ctrl Pts',(37.0096277937264,-4.71310270130147,-7.31474217133556));
#67970=CARTESIAN_POINT('Ctrl Pts',(37.0807393049553,-4.70677008115185,-7.24854117995982));
#67971=CARTESIAN_POINT('Ctrl Pts',(37.1517551114562,-4.70044598369678,-7.18242928453731));
#67972=CARTESIAN_POINT('Ctrl Pts',(37.2259669904762,-4.6941218862417,-7.11955099918333));
#67973=CARTESIAN_POINT('Ctrl Pts',(37.3030471805889,-4.68779778878663,-7.06022807265494));
#67974=CARTESIAN_POINT('Ctrl Pts',(37.3800466907567,-4.68148031077339,-7.00096723951837));
#67975=CARTESIAN_POINT('Ctrl Pts',(37.4599081986313,-4.67516283276015,-6.94525463220614));
#67976=CARTESIAN_POINT('Ctrl Pts',(37.5422690983968,-4.6688453547469,-6.8933733337022));
#67977=CARTESIAN_POINT('Ctrl Pts',(37.6245715356838,-4.66253236108756,-6.84152886225219));
#67978=CARTESIAN_POINT('Ctrl Pts',(37.7093694687744,-4.65621936742822,-6.79351052532837));
#67979=CARTESIAN_POINT('Ctrl Pts',(37.7962701792758,-4.64990637376888,-6.74955891013526));
#67980=CARTESIAN_POINT('Ctrl Pts',(37.8831394864779,-4.64359566143529,-6.70562317773202));
#67981=CARTESIAN_POINT('Ctrl Pts',(37.9721096713557,-4.63728494910171,-6.6657514441378));
#67982=CARTESIAN_POINT('Ctrl Pts',(38.0627630390549,-4.63097423676812,-6.63013856159568));
#67983=CARTESIAN_POINT('Ctrl Pts',(38.1534082009409,-4.62466409567119,-6.59452890268074));
#67984=CARTESIAN_POINT('Ctrl Pts',(38.2457358356171,-4.61835395457426,-6.56317748805104));
#67985=CARTESIAN_POINT('Ctrl Pts',(38.3393088559079,-4.61204381347733,-6.53623078719995));
#67986=CARTESIAN_POINT('Ctrl Pts',(38.432898750092,-4.60573253448138,-6.50927922708757));
#67987=CARTESIAN_POINT('Ctrl Pts',(38.5277340556931,-4.59942125548543,-6.48673407930736));
#67988=CARTESIAN_POINT('Ctrl Pts',(38.6233641581208,-4.59310997648948,-6.46869148174464));
#67989=CARTESIAN_POINT('Ctrl Pts',(38.7190965305384,-4.58679194800333,-6.4506295888322));
#67990=CARTESIAN_POINT('Ctrl Pts',(38.8156249662858,-4.58047391951718,-6.43707994058349));
#67991=CARTESIAN_POINT('Ctrl Pts',(38.9124905298923,-4.57415589103103,-6.42808718923209));
#67992=CARTESIAN_POINT('Ctrl Pts',(39.0094128535899,-4.5678341603843,-6.41908916841891));
#67993=CARTESIAN_POINT('Ctrl Pts',(39.1066722618487,-4.56151242973756,-6.41465338150445));
#67994=CARTESIAN_POINT('Ctrl Pts',(39.2038086960325,-4.55519069909083,-6.41477233200936));
#67995=CARTESIAN_POINT('Ctrl Pts',(39.3011008814141,-4.54885883200941,-6.41489147324274));
#67996=CARTESIAN_POINT('Ctrl Pts',(39.3982692624579,-4.542526964928,-6.41957991402117));
#67997=CARTESIAN_POINT('Ctrl Pts',(39.4948578214015,-4.53619509784658,-6.42877818655408));
#67998=CARTESIAN_POINT('Ctrl Pts',(39.5509580454476,-4.53251744527797,-6.43412069456515));
#67999=CARTESIAN_POINT('Ctrl Pts',(39.6068628189766,-4.52883979270935,-6.4409836188567));
#68000=CARTESIAN_POINT('Ctrl Pts',(39.6624846319725,-4.52516214014074,-6.44934744841209));
#68001=CARTESIAN_POINT('Ctrl Pts',(39.758260893369,-4.51882951999112,-6.46374928615569));
#68002=CARTESIAN_POINT('Ctrl Pts',(39.853530161358,-4.51249689984149,-6.48265412890254));
#68003=CARTESIAN_POINT('Ctrl Pts',(39.9478365430096,-4.50616427969187,-6.50601487949353));
#68004=CARTESIAN_POINT('Ctrl Pts',(40.0420160033448,-4.4998401822368,-6.52934419024806));
#68005=CARTESIAN_POINT('Ctrl Pts',(40.1352347320877,-4.49351608478173,-6.55711738538795));
#68006=CARTESIAN_POINT('Ctrl Pts',(40.2270441421906,-4.48719198732666,-6.58923587751127));
#68007=CARTESIAN_POINT('Ctrl Pts',(40.318757455253,-4.48087450931341,-6.62132075116313));
#68008=CARTESIAN_POINT('Ctrl Pts',(40.4090639717026,-4.47455703130016,-6.65774173605245));
#68009=CARTESIAN_POINT('Ctrl Pts',(40.4975284358924,-4.4682395532869,-6.6983499312878));
#68010=CARTESIAN_POINT('Ctrl Pts',(40.5859301050926,-4.46192655962756,-6.73892930148905));
#68011=CARTESIAN_POINT('Ctrl Pts',(40.6724919252063,-4.45561356596822,-6.78368979116446));
#68012=CARTESIAN_POINT('Ctrl Pts',(40.7567977656624,-4.44930057230888,-6.83243405471126));
#68013=CARTESIAN_POINT('Ctrl Pts',(40.841073140527,-4.4429898599753,-6.88116070354941));
#68014=CARTESIAN_POINT('Ctrl Pts',(40.9230937774273,-4.43667914764172,-6.93386804705558));
#68015=CARTESIAN_POINT('Ctrl Pts',(41.0024681907966,-4.43036843530814,-6.99031282520575));
#68016=CARTESIAN_POINT('Ctrl Pts',(41.0818354193077,-4.4240582942112,-7.04675249405542));
#68017=CARTESIAN_POINT('Ctrl Pts',(41.1585565442667,-4.41774815311426,-7.10692867131198));
#68018=CARTESIAN_POINT('Ctrl Pts',(41.2322699947175,-4.41143801201733,-7.17055541125491));
#68019=CARTESIAN_POINT('Ctrl Pts',(41.3059967378123,-4.40512673302141,-7.23419362491946));
#68020=CARTESIAN_POINT('Ctrl Pts',(41.3767143981656,-4.3988154540255,-7.3012833513382));
#68021=CARTESIAN_POINT('Ctrl Pts',(41.4440961572377,-4.39250417502958,-7.37149980497542));
#68022=CARTESIAN_POINT('Ctrl Pts',(41.5115499765888,-4.38618614654343,-7.44179135040758));
#68023=CARTESIAN_POINT('Ctrl Pts',(41.5756604690033,-4.37986811805728,-7.51521598277214));
#68024=CARTESIAN_POINT('Ctrl Pts',(41.6361393807236,-4.37355008957113,-7.5914138057517));
#68025=CARTESIAN_POINT('Ctrl Pts',(41.6966537311323,-4.3672283589244,-7.6676562781939));
#68026=CARTESIAN_POINT('Ctrl Pts',(41.7535320080731,-4.36090662827766,-7.7466748223001));
#68027=CARTESIAN_POINT('Ctrl Pts',(41.8065290122119,-4.35458489763093,-7.82808009576247));
#68028=CARTESIAN_POINT('Ctrl Pts',(41.8596109931871,-4.34825303054952,-7.90961589665206));
#68029=CARTESIAN_POINT('Ctrl Pts',(41.9087990534684,-4.34192116346811,-7.99354569158422));
#68030=CARTESIAN_POINT('Ctrl Pts',(41.9538937223544,-4.33558929638669,-8.07945511350316));
#68031=CARTESIAN_POINT('Ctrl Pts',(41.9800854479115,-4.33191164381805,-8.12935271907964));
#68032=CARTESIAN_POINT('Ctrl Pts',(42.0048971680573,-4.3282339912494,-8.17991774628832));
#68033=CARTESIAN_POINT('Ctrl Pts',(42.0282973863272,-4.32455633868076,-8.23106625077054));
#68034=CARTESIAN_POINT('Ctrl Pts',(42.0685906687826,-4.31822371853114,-8.31913983685877));
#68035=CARTESIAN_POINT('Ctrl Pts',(42.104836085978,-4.31189109838151,-8.40925030370235));
#68036=CARTESIAN_POINT('Ctrl Pts',(42.1368238765099,-4.30555847823189,-8.50099015079872));
#68037=CARTESIAN_POINT('Ctrl Pts',(42.1687686165885,-4.29923438077683,-8.59260653072394));
#68038=CARTESIAN_POINT('Ctrl Pts',(42.1964669760499,-4.29291028332177,-8.68584752299583));
#68039=CARTESIAN_POINT('Ctrl Pts',(42.2197563040006,-4.28658618586671,-8.78028359938236));
#68040=CARTESIAN_POINT('Ctrl Pts',(42.2430212549784,-4.28026870785348,-8.87462082939295));
#68041=CARTESIAN_POINT('Ctrl Pts',(42.2618862450071,-4.27395122984026,-8.97015023431466));
#68042=CARTESIAN_POINT('Ctrl Pts',(42.276238041974,-4.26763375182703,-9.06642594707965));
#68043=CARTESIAN_POINT('Ctrl Pts',(42.290579651563,-4.26132075816769,-9.16263332017403));
#68044=CARTESIAN_POINT('Ctrl Pts',(42.3004143727697,-4.25500776450834,-9.25958551662242));
#68045=CARTESIAN_POINT('Ctrl Pts',(42.3056799943147,-4.248694770849,-9.35682620354653));
#68046=CARTESIAN_POINT('Ctrl Pts',(42.3109437130226,-4.24238405851542,-9.45403175061534));
#68047=CARTESIAN_POINT('Ctrl Pts',(42.3116415892697,-4.23607334618183,-9.55152514478004));
#68048=CARTESIAN_POINT('Ctrl Pts',(42.3077633310885,-4.22976263384824,-9.64884559274261));
#68049=CARTESIAN_POINT('Ctrl Pts',(42.3038854239617,-4.22345249275131,-9.74615723139746));
#68050=CARTESIAN_POINT('Ctrl Pts',(42.2954322236033,-4.21714235165438,-9.84329551801961));
#68051=CARTESIAN_POINT('Ctrl Pts',(42.2824455341499,-4.21083221055745,-9.93980137644355));
#68052=CARTESIAN_POINT('Ctrl Pts',(42.2694565028247,-4.20452093156151,-10.0363246376352));
#68053=CARTESIAN_POINT('Ctrl Pts',(42.2519324170684,-4.19820965256559,-10.1322148107252));
#68054=CARTESIAN_POINT('Ctrl Pts',(42.2299666010881,-4.19189837356966,-10.2270206900018));
#68055=CARTESIAN_POINT('Ctrl Pts',(42.2079772941387,-4.18558034508351,-10.3219279578171));
#68056=CARTESIAN_POINT('Ctrl Pts',(42.1815368724549,-4.17926231659735,-10.4157481900525));
#68057=CARTESIAN_POINT('Ctrl Pts',(42.1507891416017,-4.1729442881112,-10.5080432822138));
#68058=CARTESIAN_POINT('Ctrl Pts',(42.1200233935715,-4.16662255746446,-10.6003924563177));
#68059=CARTESIAN_POINT('Ctrl Pts',(42.0849454679997,-4.16030082681771,-10.6912143030178));
#68060=CARTESIAN_POINT('Ctrl Pts',(42.0457473623408,-4.15397909617096,-10.7800906750632));
#68061=CARTESIAN_POINT('Ctrl Pts',(42.0064864053742,-4.14764722908955,-10.8691095538983));
#68062=CARTESIAN_POINT('Ctrl Pts',(41.9630922714297,-4.14131536200813,-10.9561763379827));
#68063=CARTESIAN_POINT('Ctrl Pts',(41.9158029093577,-4.13498349492671,-11.0408974933763));
#68064=CARTESIAN_POINT('Ctrl Pts',(41.8883364698924,-4.13130584235806,-11.0901049342062));
#68065=CARTESIAN_POINT('Ctrl Pts',(41.8595568068561,-4.12762818978942,-11.1385216093164));
#68066=CARTESIAN_POINT('Ctrl Pts',(41.829516997139,-4.12395053722077,-11.1860752585771));
#68067=CARTESIAN_POINT('Ctrl Pts',(41.7777908754473,-4.11761791707114,-11.267958794848));
#68068=CARTESIAN_POINT('Ctrl Pts',(41.7221464678276,-4.11128529692151,-11.3475661211635));
#68069=CARTESIAN_POINT('Ctrl Pts',(41.6628103481133,-4.10495267677189,-11.4244988397275));
#68070=CARTESIAN_POINT('Ctrl Pts',(41.6035540853321,-4.09862857931681,-11.5013280191488));
#68071=CARTESIAN_POINT('Ctrl Pts',(41.5406162503143,-4.09230448186174,-11.5754894018221));
#68072=CARTESIAN_POINT('Ctrl Pts',(41.4742676140015,-4.08598038440666,-11.6466119986473));
#68073=CARTESIAN_POINT('Ctrl Pts',(41.407988424901,-4.07966290639342,-11.7176601513489));
#68074=CARTESIAN_POINT('Ctrl Pts',(41.3383058287592,-4.07334542838017,-11.7856755234971));
#68075=CARTESIAN_POINT('Ctrl Pts',(41.2655312915966,-4.06702795036693,-11.8503195772485));
#68076=CARTESIAN_POINT('Ctrl Pts',(41.1928084121967,-4.06071495670759,-11.9149177445221));
#68077=CARTESIAN_POINT('Ctrl Pts',(41.1169982811168,-4.05440196304824,-11.9761490613708));
#68078=CARTESIAN_POINT('Ctrl Pts',(41.0384490172052,-4.0480889693889,-12.0337119930429));
#68079=CARTESIAN_POINT('Ctrl Pts',(40.9599281386316,-4.04177825705531,-12.0912541232053));
#68080=CARTESIAN_POINT('Ctrl Pts',(40.8786704464283,-4.03546754472172,-12.1451302440273));
#68081=CARTESIAN_POINT('Ctrl Pts',(40.7950561745941,-4.02915683238813,-12.1950798588786));
#68082=CARTESIAN_POINT('Ctrl Pts',(40.711449471404,-4.02284669129119,-12.2450249523624));
#68083=CARTESIAN_POINT('Ctrl Pts',(40.625486988232,-4.01653655019425,-12.2910440224433));
#68084=CARTESIAN_POINT('Ctrl Pts',(40.537575997897,-4.01022640909731,-12.3329211354221));
#68085=CARTESIAN_POINT('Ctrl Pts',(40.449649154695,-4.00391513010138,-12.3748058000425));
#68086=CARTESIAN_POINT('Ctrl Pts',(40.3597735012785,-3.99760385110545,-12.4125468360616));
#68087=CARTESIAN_POINT('Ctrl Pts',(40.2683778817386,-3.99129257210951,-12.4459757538726));
#68088=CARTESIAN_POINT('Ctrl Pts',(40.1768845207044,-3.98497454362336,-12.4794404216725));
#68089=CARTESIAN_POINT('Ctrl Pts',(40.0838683597006,-3.9786565151372,-12.5085836141476));
#68090=CARTESIAN_POINT('Ctrl Pts',(39.9897748661653,-3.97233848665105,-12.5332862752194));
#68091=CARTESIAN_POINT('Ctrl Pts',(39.8956262368825,-3.96601675600431,-12.5580034112527));
#68092=CARTESIAN_POINT('Ctrl Pts',(39.8003994455534,-3.95969502535756,-12.5782747435621));
#68093=CARTESIAN_POINT('Ctrl Pts',(39.7045495903878,-3.95337329471082,-12.5940324800724));
#68094=CARTESIAN_POINT('Ctrl Pts',(39.6085460469604,-3.94704142762941,-12.6098154829656));
#68095=CARTESIAN_POINT('Ctrl Pts',(39.511917878896,-3.940709560548,-12.6210703880341));
#68096=CARTESIAN_POINT('Ctrl Pts',(39.4151246915751,-3.93437769346659,-12.6277813361522));
#68097=CARTESIAN_POINT('Ctrl Pts',(39.3589056160012,-3.93070004089799,-12.6316791652234));
#68098=CARTESIAN_POINT('Ctrl Pts',(39.3026308801833,-3.92702238832939,-12.634045077682));
#68099=CARTESIAN_POINT('Ctrl Pts',(39.2463900062488,-3.92334473576079,-12.6348840203809));
#68100=CARTESIAN_POINT('Ctrl Pts',(39.1495477720066,-3.91701211561117,-12.6363286118261));
#68101=CARTESIAN_POINT('Ctrl Pts',(39.0524697847135,-3.91067949546155,-12.6332478837387));
#68102=CARTESIAN_POINT('Ctrl Pts',(38.9556135048535,-3.90434687531193,-12.6256137930884));
#68103=CARTESIAN_POINT('Ctrl Pts',(38.8588875780654,-3.89802277785687,-12.617989976704));
#68104=CARTESIAN_POINT('Ctrl Pts',(38.76238319794,-3.89169868040181,-12.6058250117094));
#68105=CARTESIAN_POINT('Ctrl Pts',(38.6665590324013,-3.88537458294675,-12.5891428470271));
#68106=CARTESIAN_POINT('Ctrl Pts',(38.5708351661537,-3.87905710493354,-12.5724781435904));
#68107=CARTESIAN_POINT('Ctrl Pts',(38.4757905276088,-3.87273962692033,-12.5513057148846));
#68108=CARTESIAN_POINT('Ctrl Pts',(38.381878855308,-3.86642214890712,-12.5257013256084));
#68109=CARTESIAN_POINT('Ctrl Pts',(38.2880338446038,-3.86010915524777,-12.5001151111705));
#68110=CARTESIAN_POINT('Ctrl Pts',(38.195320622029,-3.85379616158843,-12.4701033052074));
#68111=CARTESIAN_POINT('Ctrl Pts',(38.1041819755489,-3.84748316792909,-12.4357925914067));
#68112=CARTESIAN_POINT('Ctrl Pts',(38.0130762638306,-3.8411724555955,-12.4014942764645));
#68113=CARTESIAN_POINT('Ctrl Pts',(37.9235444064454,-3.83486174326192,-12.3629002944186));
#68114=CARTESIAN_POINT('Ctrl Pts',(37.8360123815432,-3.82855103092834,-12.3201866538027));
#68115=CARTESIAN_POINT('Ctrl Pts',(37.7484882799147,-3.8222408898314,-12.2774768795643));
#68116=CARTESIAN_POINT('Ctrl Pts',(37.662964043779,-3.81593074873447,-12.2306483801479));
#68117=CARTESIAN_POINT('Ctrl Pts',(37.5798431150426,-3.80962060763754,-12.179924164835));
#68118=CARTESIAN_POINT('Ctrl Pts',(37.4967071972242,-3.8033093286416,-12.1291908024947));
#68119=CARTESIAN_POINT('Ctrl Pts',(37.415975820834,-3.79699804964566,-12.0745605568153));
#68120=CARTESIAN_POINT('Ctrl Pts',(37.338024490238,-3.79068677064972,-12.0163004343007));
#68121=CARTESIAN_POINT('Ctrl Pts',(37.2599897959144,-3.78436874216357,-11.9579780064867));
#68122=CARTESIAN_POINT('Ctrl Pts',(37.1847414338276,-3.77805071367743,-11.8960182140504));
#68123=CARTESIAN_POINT('Ctrl Pts',(37.1126226002573,-3.77173268519128,-11.8307290048796));
#68124=CARTESIAN_POINT('Ctrl Pts',(37.0404615073804,-3.76541095454456,-11.7654015383417));
#68125=CARTESIAN_POINT('Ctrl Pts',(36.9714339045352,-3.75908922389784,-11.696741078499));
#68126=CARTESIAN_POINT('Ctrl Pts',(36.9058453248355,-3.75276749325112,-11.6250916597427));
#68127=CARTESIAN_POINT('Ctrl Pts',(36.8401515786248,-3.74643562616969,-11.5533273563614));
#68128=CARTESIAN_POINT('Ctrl Pts',(36.7779081461245,-3.74010375908826,-11.4785648599999));
#68129=CARTESIAN_POINT('Ctrl Pts',(36.7193795364619,-3.73377189200683,-11.4011803668027));
#68130=CARTESIAN_POINT('Ctrl Pts',(36.685385157095,-3.73009423943816,-11.3562341800741));
#68131=CARTESIAN_POINT('Ctrl Pts',(36.652643151416,-3.72641658686948,-11.3104040099088));
#68132=CARTESIAN_POINT('Ctrl Pts',(36.6211983115091,-3.7227389343008,-11.2637675245231));
#68133=CARTESIAN_POINT('Ctrl Pts',(36.5662323739882,-3.71631035581507,-11.182246418056));
#68134=CARTESIAN_POINT('Ctrl Pts',(36.5150453840929,-3.70988177732934,-11.0979827664567));
#68135=CARTESIAN_POINT('Ctrl Pts',(36.467916808164,-3.70345319884361,-11.0113553026741));
#68136=CARTESIAN_POINT('Ctrl Pts',(36.4208567825603,-3.69703397097238,-10.9248538418673));
#68137=CARTESIAN_POINT('Ctrl Pts',(36.3778436321412,-3.69061474310115,-10.8359957709156));
#68138=CARTESIAN_POINT('Ctrl Pts',(36.339113950261,-3.68419551522991,-10.7451891916045));
#68139=CARTESIAN_POINT('Ctrl Pts',(36.3004312822952,-3.67778407965171,-10.6544928422914));
#68140=CARTESIAN_POINT('Ctrl Pts',(36.2660219051206,-3.6713726440735,-10.561853072782));
#68141=CARTESIAN_POINT('Ctrl Pts',(36.2360764098612,-3.6649612084953,-10.4677022884871));
#68142=CARTESIAN_POINT('Ctrl Pts',(36.2061647874513,-3.65855702521297,-10.3736580028596));
#68143=CARTESIAN_POINT('Ctrl Pts',(36.1807071210664,-3.65215284193065,-10.2781065038215));
#68144=CARTESIAN_POINT('Ctrl Pts',(36.1598454211839,-3.64574865864833,-10.1814988878921));
#68145=CARTESIAN_POINT('Ctrl Pts',(36.1389974530624,-3.63934869078057,-10.0849548618279));
#68146=CARTESIAN_POINT('Ctrl Pts',(36.122739522412,-3.63294872291281,-9.98735651102084));
#68147=CARTESIAN_POINT('Ctrl Pts',(36.1111633069834,-3.62654875504505,-9.889168280846));
#68148=CARTESIAN_POINT('Ctrl Pts',(36.0995920289091,-3.62015151681797,-9.7910219287856));
#68149=CARTESIAN_POINT('Ctrl Pts',(36.092698541246,-3.61375427859088,-9.692286614564));
#68150=CARTESIAN_POINT('Ctrl Pts',(36.0905229700006,-3.60735704036379,-9.59343429553861));
#68151=CARTESIAN_POINT('Ctrl Pts',(36.0900097672587,-3.60584797454691,-9.5701156930002));
#68152=CARTESIAN_POINT('Ctrl Pts',(36.0897588686184,-3.60433890873002,-9.54679059957209));
#68153=CARTESIAN_POINT('Ctrl Pts',(36.0897703786693,-3.60282984291314,-9.52346523708319));
#68154=CARTESIAN_POINT('',(36.0895800927968,-2.33282991063404,-9.52372422996978));
#68155=CARTESIAN_POINT('Ctrl Pts',(36.0939567706053,-3.60282853633159,-9.52344713446587));
#68156=CARTESIAN_POINT('Ctrl Pts',(36.0920877916079,-3.57593006850133,-9.10824092314765));
#68157=CARTESIAN_POINT('Ctrl Pts',(36.3622061427194,-3.48216300018445,-7.66318432907408));
#68158=CARTESIAN_POINT('Ctrl Pts',(38.5462979006151,-3.32152733138084,-5.91383345726613));
#68159=CARTESIAN_POINT('Ctrl Pts',(41.8665981283961,-3.12092152992086,-7.00367006210291));
#68160=CARTESIAN_POINT('Ctrl Pts',(42.768927986537,-2.92031572846088,-10.3797533334323));
#68161=CARTESIAN_POINT('Ctrl Pts',(40.435088873085,-2.71970992700091,-12.9807785967394));
#68162=CARTESIAN_POINT('Ctrl Pts',(37.0635739275412,-2.52388181452703,-12.460917710667));
#68163=CARTESIAN_POINT('Ctrl Pts',(36.0904109778155,-2.39492230253986,-10.475455999417));
#68164=CARTESIAN_POINT('Ctrl Pts',(36.0854229188962,-2.33283139103934,-9.52374521463249));
#68165=CARTESIAN_POINT('',(36.0897712174216,-1.06282984297027,-9.52775189410162));
#68166=CARTESIAN_POINT('Ctrl Pts',(36.0897702620449,-2.33282984291314,-9.52372327002978));
#68167=CARTESIAN_POINT('Ctrl Pts',(36.0898002776313,-2.32805266996907,-9.45060258528132));
#68168=CARTESIAN_POINT('Ctrl Pts',(36.092408661042,-2.323275497025,-9.37753813353249));
#68169=CARTESIAN_POINT('Ctrl Pts',(36.0975847896046,-2.31849832408093,-9.30465818552244));
#68170=CARTESIAN_POINT('Ctrl Pts',(36.1044462652967,-2.31216570393131,-9.20804853109387));
#68171=CARTESIAN_POINT('Ctrl Pts',(36.1158366136766,-2.30583308378168,-9.1115918752));
#68172=CARTESIAN_POINT('Ctrl Pts',(36.1317445637288,-2.29950046363206,-9.01574639844953));
#68173=CARTESIAN_POINT('Ctrl Pts',(36.1476311042228,-2.293176366177,-8.92002991439162));
#68174=CARTESIAN_POINT('Ctrl Pts',(36.1680230911667,-2.28685226872195,-8.82492340238974));
#68175=CARTESIAN_POINT('Ctrl Pts',(36.1928573494404,-2.28052817126689,-8.73088178960229));
#68176=CARTESIAN_POINT('Ctrl Pts',(36.2176656136605,-2.27421069325365,-8.63693861030494));
#68177=CARTESIAN_POINT('Ctrl Pts',(36.2469067942496,-2.26789321524041,-8.54405853487825));
#68178=CARTESIAN_POINT('Ctrl Pts',(36.2804665135229,-2.26157573722717,-8.45268713789364));
#68179=CARTESIAN_POINT('Ctrl Pts',(36.3140024110025,-2.25526274356783,-8.36138059933508));
#68180=CARTESIAN_POINT('Ctrl Pts',(36.3518506025418,-2.2489497499085,-8.27158101952218));
#68181=CARTESIAN_POINT('Ctrl Pts',(36.3938469174799,-2.24263675624916,-8.18371869827279));
#68182=CARTESIAN_POINT('Ctrl Pts',(36.4358280562148,-2.23632604391558,-8.09588812781981));
#68183=CARTESIAN_POINT('Ctrl Pts',(36.4819541514066,-2.23001533158199,-8.00999381904815));
#68184=CARTESIAN_POINT('Ctrl Pts',(36.5320133299145,-2.22370461924841,-7.92644509598633));
#68185=CARTESIAN_POINT('Ctrl Pts',(36.5820679771372,-2.21739447815148,-7.84290393563538));
#68186=CARTESIAN_POINT('Ctrl Pts',(36.6360547748898,-2.21108433705455,-7.76170831387778));
#68187=CARTESIAN_POINT('Ctrl Pts',(36.6937169539322,-2.20477419595762,-7.68324107280751));
#68188=CARTESIAN_POINT('Ctrl Pts',(36.7513895311155,-2.19846291696169,-7.60475968184839));
#68189=CARTESIAN_POINT('Ctrl Pts',(36.8127385469611,-2.19215163796576,-7.52900800113037));
#68190=CARTESIAN_POINT('Ctrl Pts',(36.8774657915695,-2.18584035896983,-7.45633726683872));
#68191=CARTESIAN_POINT('Ctrl Pts',(36.9422622576313,-2.17952233048368,-7.38358881606356));
#68192=CARTESIAN_POINT('Ctrl Pts',(37.0104438738492,-2.17320430199754,-7.31392821683122));
#68193=CARTESIAN_POINT('Ctrl Pts',(37.0816744088738,-2.16688627351139,-7.24767100688552));
#68194=CARTESIAN_POINT('Ctrl Pts',(37.1529466826908,-2.16056454286467,-7.18137497235528));
#68195=CARTESIAN_POINT('Ctrl Pts',(37.2272710991643,-2.15424281221793,-7.11848658061029));
#68196=CARTESIAN_POINT('Ctrl Pts',(37.304278701515,-2.14792108157121,-7.05928075171351));
#68197=CARTESIAN_POINT('Ctrl Pts',(37.3814097799477,-2.14158921448979,-6.99997999058203));
#68198=CARTESIAN_POINT('Ctrl Pts',(37.4612322765795,-2.13525734740838,-6.94437383280194));
#68199=CARTESIAN_POINT('Ctrl Pts',(37.5433487075768,-2.12892548032697,-6.89269356870965));
#68200=CARTESIAN_POINT('Ctrl Pts',(37.5910432816265,-2.1252478277583,-6.86267682111454));
#68201=CARTESIAN_POINT('Ctrl Pts',(37.6395112396921,-2.12157017518962,-6.83398360808067));
#68202=CARTESIAN_POINT('Ctrl Pts',(37.6886713600782,-2.11789252262095,-6.80665189958092));
#68203=CARTESIAN_POINT('Ctrl Pts',(37.7733211096405,-2.11155990247132,-6.7595889090625));
#68204=CARTESIAN_POINT('Ctrl Pts',(37.8603183084808,-2.10522728232169,-6.7164019446356));
#68205=CARTESIAN_POINT('Ctrl Pts',(37.9492731236839,-2.09889466217206,-6.67733201834192));
#68206=CARTESIAN_POINT('Ctrl Pts',(38.0381082199237,-2.09257056471699,-6.63831467392438));
#68207=CARTESIAN_POINT('Ctrl Pts',(38.1288952990446,-2.08624646726192,-6.60340352926506));
#68208=CARTESIAN_POINT('Ctrl Pts',(38.2212188807458,-2.07992236980685,-6.5727943544713));
#68209=CARTESIAN_POINT('Ctrl Pts',(38.3134458272225,-2.0736048917936,-6.54221721834442));
#68210=CARTESIAN_POINT('Ctrl Pts',(38.4072056660689,-2.06728741378035,-6.51593323704319));
#68211=CARTESIAN_POINT('Ctrl Pts',(38.5020627603779,-2.0609699357671,-6.49409019229397));
#68212=CARTESIAN_POINT('Ctrl Pts',(38.596852521998,-2.05465694210776,-6.47226265245712));
#68213=CARTESIAN_POINT('Ctrl Pts',(38.6927375656928,-2.04834394844841,-6.45486988002064));
#68214=CARTESIAN_POINT('Ctrl Pts',(38.7892678275694,-2.04203095478907,-6.44200961152481));
#68215=CARTESIAN_POINT('Ctrl Pts',(38.8857632063168,-2.03572024245548,-6.42915399034266));
#68216=CARTESIAN_POINT('Ctrl Pts',(38.9829029069063,-2.02940953012189,-6.42082767624792));
#68217=CARTESIAN_POINT('Ctrl Pts',(39.0802283551054,-2.02309881778831,-6.41707699484379));
#68218=CARTESIAN_POINT('Ctrl Pts',(39.1775449935443,-2.01678867669137,-6.41332665294597));
#68219=CARTESIAN_POINT('Ctrl Pts',(39.2750469091687,-2.01047853559443,-6.41415113688605));
#68220=CARTESIAN_POINT('Ctrl Pts',(39.3722731621719,-2.00416839449749,-6.41954470157832));
#68221=CARTESIAN_POINT('Ctrl Pts',(39.4695169478507,-1.99785711550154,-6.42493923888464));
#68222=CARTESIAN_POINT('Ctrl Pts',(39.5664845355442,-1.99154583650559,-6.43490446912655));
#68223=CARTESIAN_POINT('Ctrl Pts',(39.6627187994011,-1.98523455750964,-6.44938266918967));
#68224=CARTESIAN_POINT('Ctrl Pts',(39.7590559793581,-1.97891652902349,-6.46387635271813));
#68225=CARTESIAN_POINT('Ctrl Pts',(39.8546578366261,-1.97259850053733,-6.48289257638167));
#68226=CARTESIAN_POINT('Ctrl Pts',(39.9490763553248,-1.96628047205118,-6.50632226516421));
#68227=CARTESIAN_POINT('Ctrl Pts',(40.0435502002251,-1.95995874140444,-6.52976568298745));
#68228=CARTESIAN_POINT('Ctrl Pts',(40.1368389069724,-1.95363701075771,-6.55762759056469));
#68229=CARTESIAN_POINT('Ctrl Pts',(40.2285105838422,-1.94731528011097,-6.58974930681813));
#68230=CARTESIAN_POINT('Ctrl Pts',(40.3203292495694,-1.94098341302955,-6.62192252790419));
#68231=CARTESIAN_POINT('Ctrl Pts',(40.4105253028673,-1.93465154594813,-6.65836903282714));
#68232=CARTESIAN_POINT('Ctrl Pts',(40.4986877933102,-1.92831967886671,-6.69888240364859));
#68233=CARTESIAN_POINT('Ctrl Pts',(40.5498940181504,-1.92464202629813,-6.72241323592088));
#68234=CARTESIAN_POINT('Ctrl Pts',(40.6004146859581,-1.92096437372955,-6.74731515466951));
#68235=CARTESIAN_POINT('Ctrl Pts',(40.6501736040664,-1.91728672116097,-6.77354090145443));
#68236=CARTESIAN_POINT('Ctrl Pts',(40.7358544348572,-1.91095410101134,-6.81869951538878));
#68237=CARTESIAN_POINT('Ctrl Pts',(40.8195727132583,-1.90462148086172,-6.86794254904839));
#68238=CARTESIAN_POINT('Ctrl Pts',(40.9009135302045,-1.89828886071209,-6.92107530530023));
#68239=CARTESIAN_POINT('Ctrl Pts',(40.982144875412,-1.89196476325703,-6.97413655335452));
#68240=CARTESIAN_POINT('Ctrl Pts',(41.0610047556517,-1.88564066580197,-7.0310768821671));
#68241=CARTESIAN_POINT('Ctrl Pts',(41.1371021272715,-1.87931656834691,-7.09165538786217));
#68242=CARTESIAN_POINT('Ctrl Pts',(41.2131198476639,-1.87299909033367,-7.15217048594894));
#68243=CARTESIAN_POINT('Ctrl Pts',(41.2863804675783,-1.86668161232043,-7.21631591932709));
#68244=CARTESIAN_POINT('Ctrl Pts',(41.3565221099628,-1.86036413430719,-7.28380767399548));
#68245=CARTESIAN_POINT('Ctrl Pts',(41.4266139635002,-1.85405114064785,-7.35125152079422));
#68246=CARTESIAN_POINT('Ctrl Pts',(41.49359092675,-1.84773814698851,-7.42203666422981));
#68247=CARTESIAN_POINT('Ctrl Pts',(41.5571251435103,-1.84142515332918,-7.49583965376528));
#68248=CARTESIAN_POINT('Ctrl Pts',(41.6206364009184,-1.8351144409956,-7.5696159731233));
#68249=CARTESIAN_POINT('Ctrl Pts',(41.6807070988664,-1.82880372866201,-7.64640764054255));
#68250=CARTESIAN_POINT('Ctrl Pts',(41.7370477798076,-1.82249301632844,-7.72585597689531));
#68251=CARTESIAN_POINT('Ctrl Pts',(41.793383360871,-1.8161828752315,-7.8052971216984));
#68252=CARTESIAN_POINT('Ctrl Pts',(41.8459893434284,-1.80987273413457,-7.88739410046962));
#68253=CARTESIAN_POINT('Ctrl Pts',(41.8946185798966,-1.80356259303764,-7.97175779037008));
#68254=CARTESIAN_POINT('Ctrl Pts',(41.9432565856077,-1.7972513140417,-8.0561366934579));
#68255=CARTESIAN_POINT('Ctrl Pts',(41.9879162025771,-1.79094003504576,-8.14278274062103));
#68256=CARTESIAN_POINT('Ctrl Pts',(42.0283958934414,-1.78462875604982,-8.23128159058329));
#68257=CARTESIAN_POINT('Ctrl Pts',(42.0689188746241,-1.77831072756368,-8.31987508413867));
#68258=CARTESIAN_POINT('Ctrl Pts',(42.1052528230875,-1.77199269907753,-8.41032493800567));
#68259=CARTESIAN_POINT('Ctrl Pts',(42.1372441822829,-1.76567467059138,-8.5021963695092));
#68260=CARTESIAN_POINT('Ctrl Pts',(42.1692542873814,-1.75935293994465,-8.59412163470362));
#68261=CARTESIAN_POINT('Ctrl Pts',(42.1969166119891,-1.75303120929792,-8.6874697171569));
#68262=CARTESIAN_POINT('Ctrl Pts',(42.2201279525242,-1.74670947865119,-8.78179222065277));
#68263=CARTESIAN_POINT('Ctrl Pts',(42.2433765107533,-1.74037761156977,-8.87626596341354));
#68264=CARTESIAN_POINT('Ctrl Pts',(42.2621597495313,-1.73404574448836,-8.97171681826881));
#68265=CARTESIAN_POINT('Ctrl Pts',(42.27642588615,-1.72771387740694,-9.06768783098812));
#68266=CARTESIAN_POINT('Ctrl Pts',(42.2847118929953,-1.72403622483829,-9.12342937402826));
#68267=CARTESIAN_POINT('Ctrl Pts',(42.2914750389586,-1.72035857226964,-9.17934630607834));
#68268=CARTESIAN_POINT('Ctrl Pts',(42.2967132490314,-1.71668091970099,-9.23534899245219));
#68269=CARTESIAN_POINT('Ctrl Pts',(42.3057330229322,-1.71034829955137,-9.33178108698647));
#68270=CARTESIAN_POINT('Ctrl Pts',(42.3102598110864,-1.70401567940174,-9.42880239748814));
#68271=CARTESIAN_POINT('Ctrl Pts',(42.3102298521332,-1.69768305925211,-9.52595906164897));
#68272=CARTESIAN_POINT('Ctrl Pts',(42.3101999335,-1.69135896179705,-9.62298496846862));
#68273=CARTESIAN_POINT('Ctrl Pts',(42.3056254568274,-1.68503486434198,-9.72014543326724));
#68274=CARTESIAN_POINT('Ctrl Pts',(42.296494398712,-1.67871076688692,-9.81698132071288));
#68275=CARTESIAN_POINT('Ctrl Pts',(42.2873728980881,-1.67239328887368,-9.91371584989706));
#68276=CARTESIAN_POINT('Ctrl Pts',(42.2737043386173,-1.66607581086044,-10.0101260440443));
#68277=CARTESIAN_POINT('Ctrl Pts',(42.2555287395324,-1.65975833284719,-10.1057536265848));
#68278=CARTESIAN_POINT('Ctrl Pts',(42.2373660420863,-1.65344533918785,-10.2013133295186));
#68279=CARTESIAN_POINT('Ctrl Pts',(42.2147027467418,-1.64713234552851,-10.2960910968563));
#68280=CARTESIAN_POINT('Ctrl Pts',(42.1876304925971,-1.64081935186917,-10.3896355837021));
#68281=CARTESIAN_POINT('Ctrl Pts',(42.1605680215496,-1.63450863953558,-10.483146266388));
#68282=CARTESIAN_POINT('Ctrl Pts',(42.1290998789849,-1.628197927202,-10.5754241344851));
#68283=CARTESIAN_POINT('Ctrl Pts',(42.0933681932019,-1.62188721486841,-10.6660307408074));
#68284=CARTESIAN_POINT('Ctrl Pts',(42.0576397418,-1.61557707377148,-10.7566291455495));
#68285=CARTESIAN_POINT('Ctrl Pts',(42.0176486751247,-1.60926693267455,-10.8455561825538));
#68286=CARTESIAN_POINT('Ctrl Pts',(41.9735857419016,-1.60295679157761,-10.9323921931075));
#68287=CARTESIAN_POINT('Ctrl Pts',(41.9295148628708,-1.59664551258167,-11.0192438626788));
#68288=CARTESIAN_POINT('Ctrl Pts',(41.8813708568461,-1.59033423358572,-11.1040033669291));
#68289=CARTESIAN_POINT('Ctrl Pts',(41.829390521414,-1.58402295458978,-11.1862754554251));
#68290=CARTESIAN_POINT('Ctrl Pts',(41.7773545964945,-1.57770492610363,-11.2686355284099));
#68291=CARTESIAN_POINT('Ctrl Pts',(41.7214743853249,-1.57138689761748,-11.3485025045336));
#68292=CARTESIAN_POINT('Ctrl Pts',(41.6620300299614,-1.56506886913133,-11.4255101379547));
#68293=CARTESIAN_POINT('Ctrl Pts',(41.602550842126,-1.5587471384846,-11.5025628953611));
#68294=CARTESIAN_POINT('Ctrl Pts',(41.5395036344395,-1.55242540783787,-11.5767526406318));
#68295=CARTESIAN_POINT('Ctrl Pts',(41.4732074725687,-1.54610367719113,-11.647747851149));
#68296=CARTESIAN_POINT('Ctrl Pts',(41.4068050096307,-1.53977181010971,-11.7188568973157));
#68297=CARTESIAN_POINT('Ctrl Pts',(41.3371435030825,-1.5334399430283,-11.7867608755279));
#68298=CARTESIAN_POINT('Ctrl Pts',(41.2645772925355,-1.52710807594688,-11.8511666440836));
#68299=CARTESIAN_POINT('Ctrl Pts',(41.2224296436379,-1.52343042337825,-11.8885745740223));
#68300=CARTESIAN_POINT('Ctrl Pts',(41.1793027026836,-1.51975277080963,-11.924803159381));
#68301=CARTESIAN_POINT('Ctrl Pts',(41.1352703938616,-1.51607511824101,-11.9598016665722));
#68302=CARTESIAN_POINT('Ctrl Pts',(41.0594503208998,-1.50974249809138,-12.0200662640866));
#68303=CARTESIAN_POINT('Ctrl Pts',(40.9806808984483,-1.50340987794174,-12.0768905950471));
#68304=CARTESIAN_POINT('Ctrl Pts',(40.8993073292417,-1.49707725779211,-12.1299731771528));
#68305=CARTESIAN_POINT('Ctrl Pts',(40.8180432758533,-1.49075316033705,-12.1829843185872));
#68306=CARTESIAN_POINT('Ctrl Pts',(40.7341824047728,-1.48442906288198,-12.232263483133));
#68307=CARTESIAN_POINT('Ctrl Pts',(40.6481026152132,-1.47810496542692,-12.2775496305631));
#68308=CARTESIAN_POINT('Ctrl Pts',(40.5621129254919,-1.47178748741368,-12.3227883769181));
#68309=CARTESIAN_POINT('Ctrl Pts',(40.4739093196116,-1.46547000940043,-12.3640422126576));
#68310=CARTESIAN_POINT('Ctrl Pts',(40.3838974251622,-1.45915253138719,-12.4010941465109));
#68311=CARTESIAN_POINT('Ctrl Pts',(40.2939494241192,-1.45283953772784,-12.4381197796817));
#68312=CARTESIAN_POINT('Ctrl Pts',(40.202196089592,-1.4465265440685,-12.4709492746601));
#68313=CARTESIAN_POINT('Ctrl Pts',(40.1090654611092,-1.44021355040915,-12.4994126546796));
#68314=CARTESIAN_POINT('Ctrl Pts',(40.0159684872305,-1.43390283807557,-12.5278657488909));
#68315=CARTESIAN_POINT('Ctrl Pts',(39.9214956261486,-1.42759212574198,-12.5519557355248));
#68316=CARTESIAN_POINT('Ctrl Pts',(39.8260917154402,-1.4212814134084,-12.5715619666695));
#68317=CARTESIAN_POINT('Ctrl Pts',(39.7306964405573,-1.41497127231146,-12.5911664230862));
#68318=CARTESIAN_POINT('Ctrl Pts',(39.6343707120116,-1.40866113121453,-12.6062878431363));
#68319=CARTESIAN_POINT('Ctrl Pts',(39.5375702111042,-1.40235099011759,-12.6168565628882));
#68320=CARTESIAN_POINT('Ctrl Pts',(39.4407522542966,-1.39603971112165,-12.6274271884827));
#68321=CARTESIAN_POINT('Ctrl Pts',(39.3434597898127,-1.38972843212572,-12.6334434357768));
#68322=CARTESIAN_POINT('Ctrl Pts',(39.2461532310898,-1.38341715312978,-12.6348875433301));
#68323=CARTESIAN_POINT('Ctrl Pts',(39.1487426095192,-1.37709912464362,-12.6363331952598));
#68324=CARTESIAN_POINT('Ctrl Pts',(39.0513183016025,-1.37078109615747,-12.6331969391355));
#68325=CARTESIAN_POINT('Ctrl Pts',(38.9543401257753,-1.36446306767132,-12.6255131638321));
#68326=CARTESIAN_POINT('Ctrl Pts',(38.85730512387,-1.35814133702458,-12.6178248860845));
#68327=CARTESIAN_POINT('Ctrl Pts',(38.7607172082617,-1.35181960637785,-12.6055838379726));
#68328=CARTESIAN_POINT('Ctrl Pts',(38.6650283971823,-1.34549787573111,-12.5888759826531));
#68329=CARTESIAN_POINT('Ctrl Pts',(38.5691861560632,-1.33916600864969,-12.5721413375045));
#68330=CARTESIAN_POINT('Ctrl Pts',(38.4742463247096,-1.33283414156828,-12.5509256788029));
#68331=CARTESIAN_POINT('Ctrl Pts',(38.3806480632887,-1.32650227448686,-12.5253654871878));
#68332=CARTESIAN_POINT('Ctrl Pts',(38.3262846532383,-1.32282462191824,-12.5105197073982));
#68333=CARTESIAN_POINT('Ctrl Pts',(38.2723735049704,-1.31914696934963,-12.4942092345176));
#68334=CARTESIAN_POINT('Ctrl Pts',(38.2189975102117,-1.31546931678102,-12.4764682393563));
#68335=CARTESIAN_POINT('Ctrl Pts',(38.1270883661017,-1.30913669663139,-12.4459196811832));
#68336=CARTESIAN_POINT('Ctrl Pts',(38.0364478673732,-1.30280407648177,-12.4110208775835));
#68337=CARTESIAN_POINT('Ctrl Pts',(37.9475171640674,-1.29647145633214,-12.3718960990163));
#68338=CARTESIAN_POINT('Ctrl Pts',(37.8587061472744,-1.29014735887709,-12.3328239761477));
#68339=CARTESIAN_POINT('Ctrl Pts',(37.7716007492447,-1.28382326142203,-12.2895373570747));
#68340=CARTESIAN_POINT('Ctrl Pts',(37.6866261270882,-1.27749916396698,-12.242209998084));
#68341=CARTESIAN_POINT('Ctrl Pts',(37.6017404479898,-1.27118168595374,-12.1949321767075));
#68342=CARTESIAN_POINT('Ctrl Pts',(37.518981490894,-1.2648642079405,-12.1436222354299));
#68343=CARTESIAN_POINT('Ctrl Pts',(37.4387526839846,-1.25854672992727,-12.0885012277603));
#68344=CARTESIAN_POINT('Ctrl Pts',(37.3585808261239,-1.25223373626793,-12.0334193467969));
#68345=CARTESIAN_POINT('Ctrl Pts',(37.2809359073443,-1.2459207426086,-11.9745320245189));
#68346=CARTESIAN_POINT('Ctrl Pts',(37.2061942375429,-1.23960774894926,-11.9121047807947));
#68347=CARTESIAN_POINT('Ctrl Pts',(37.1314795771296,-1.23329703661568,-11.849700096396));
#68348=CARTESIAN_POINT('Ctrl Pts',(37.0596664163264,-1.2269863242821,-11.7837583124312));
#68349=CARTESIAN_POINT('Ctrl Pts',(36.9910989400906,-1.22067561194852,-11.7145859792279));
#68350=CARTESIAN_POINT('Ctrl Pts',(36.9225376704846,-1.21436547085158,-11.6454199074051));
#68351=CARTESIAN_POINT('Ctrl Pts',(36.8572218090311,-1.20805532975465,-11.5730241784787));
#68352=CARTESIAN_POINT('Ctrl Pts',(36.7954587750304,-1.20174518865771,-11.497742291918));
#68353=CARTESIAN_POINT('Ctrl Pts',(36.7336846033874,-1.19543390966177,-11.4224468298789));
#68354=CARTESIAN_POINT('Ctrl Pts',(36.6754648090073,-1.18912263066584,-11.3442645146203));
#68355=CARTESIAN_POINT('Ctrl Pts',(36.6210659356797,-1.1828113516699,-11.2635711790975));
#68356=CARTESIAN_POINT('Ctrl Pts',(36.5666088864003,-1.17649332318375,-11.1827915474565));
#68357=CARTESIAN_POINT('Ctrl Pts',(36.5159811609401,-1.17017529469761,-11.0994958975688));
#68358=CARTESIAN_POINT('Ctrl Pts',(36.4694053081403,-1.16385726621147,-11.014088070494));
#68359=CARTESIAN_POINT('Ctrl Pts',(36.4228021633954,-1.15753553556474,-10.9286301971917));
#68360=CARTESIAN_POINT('Ctrl Pts',(36.3802558101443,-1.15121380491802,-10.8410580753411));
#68361=CARTESIAN_POINT('Ctrl Pts',(36.3419413461397,-1.14489207427129,-10.751797205733));
#68362=CARTESIAN_POINT('Ctrl Pts',(36.3035654476824,-1.13856020718988,-10.6623932128213));
#68363=CARTESIAN_POINT('Ctrl Pts',(36.2694351413073,-1.13222834010846,-10.5712954744392));
#68364=CARTESIAN_POINT('Ctrl Pts',(36.2396761939009,-1.12589647302705,-10.4789463380835));
#68365=CARTESIAN_POINT('Ctrl Pts',(36.2223917076723,-1.12221882045838,-10.4253084404198));
#68366=CARTESIAN_POINT('Ctrl Pts',(36.2065809431792,-1.11854116788971,-10.3712486294749));
#68367=CARTESIAN_POINT('Ctrl Pts',(36.1922605966023,-1.11486351532104,-10.3168549956581));
#68368=CARTESIAN_POINT('Ctrl Pts',(36.160600384436,-1.10673275815172,-10.1965985494974));
#68369=CARTESIAN_POINT('Ctrl Pts',(36.1361386046844,-1.0986020009824,-10.0743742818528));
#68370=CARTESIAN_POINT('Ctrl Pts',(36.1190733990765,-1.09047124381308,-9.95093653590859));
#68371=CARTESIAN_POINT('Ctrl Pts',(36.1023366837152,-1.08249699659095,-9.82987485835468));
#68372=CARTESIAN_POINT('Ctrl Pts',(36.0927145179575,-1.07452274936882,-9.70764575813965));
#68373=CARTESIAN_POINT('Ctrl Pts',(36.0903484504941,-1.06654850214669,-9.58498244372551));
#68374=CARTESIAN_POINT('Ctrl Pts',(36.0899806582649,-1.06530894908788,-9.56591510327944));
#68375=CARTESIAN_POINT('Ctrl Pts',(36.0897881039816,-1.06406939602907,-9.54683731773078));
#68376=CARTESIAN_POINT('Ctrl Pts',(36.0897712174216,-1.06282984297026,-9.52775189410163));
#68377=CARTESIAN_POINT('',(36.0899362460626,0.207170205182039,-9.52357073843679));
#68378=CARTESIAN_POINT('Ctrl Pts',(36.0897712174209,-1.06282984291314,-9.52775189322205));
#68379=CARTESIAN_POINT('Ctrl Pts',(36.0896860844236,-1.05658067781646,-9.43153337126958));
#68380=CARTESIAN_POINT('Ctrl Pts',(36.0940701443256,-1.05033151271977,-9.3352083438086));
#68381=CARTESIAN_POINT('Ctrl Pts',(36.1029262969847,-1.04408234762309,-9.23922888356096));
#68382=CARTESIAN_POINT('Ctrl Pts',(36.1117776524504,-1.03783656756891,-9.14330141338673));
#68383=CARTESIAN_POINT('Ctrl Pts',(36.1250962497593,-1.03159078751473,-9.04771958335936));
#68384=CARTESIAN_POINT('Ctrl Pts',(36.1428329414513,-1.02534500746055,-8.95293337011782));
#68385=CARTESIAN_POINT('Ctrl Pts',(36.1605650823694,-1.01910082991111,-8.85817147655383));
#68386=CARTESIAN_POINT('Ctrl Pts',(36.1827129836568,-1.01285665236168,-8.76420523396972));
#68387=CARTESIAN_POINT('Ctrl Pts',(36.2091760613553,-1.00661247481225,-8.67147623294382));
#68388=CARTESIAN_POINT('Ctrl Pts',(36.2356398940563,-1.00036811911387,-8.57874458632138));
#68389=CARTESIAN_POINT('Ctrl Pts',(36.2664190235894,-0.994123763415482,
-8.48725068141378));
#68390=CARTESIAN_POINT('Ctrl Pts',(36.3013628189955,-0.987879407717097,
-8.39742155669849));
#68391=CARTESIAN_POINT('Ctrl Pts',(36.336340477737,-0.981629000738119,-8.30750538036965));
#68392=CARTESIAN_POINT('Ctrl Pts',(36.3754907006624,-0.975378593759137,
-8.2192576245062));
#68393=CARTESIAN_POINT('Ctrl Pts',(36.4186145503963,-0.969128186780159,
-8.13308562273654));
#68394=CARTESIAN_POINT('Ctrl Pts',(36.4617589066273,-0.96287480757228,-8.04687264396891));
#68395=CARTESIAN_POINT('Ctrl Pts',(36.5088804328319,-0.956621428364402,
-7.96273777518549));
#68396=CARTESIAN_POINT('Ctrl Pts',(36.559735136623,-0.950368049156523,-7.88106201329952));
#68397=CARTESIAN_POINT('Ctrl Pts',(36.6106765485517,-0.944104007830401,
-7.79924699284601));
#68398=CARTESIAN_POINT('Ctrl Pts',(36.6653635991613,-0.937839966504279,
-7.71989982409718));
#68399=CARTESIAN_POINT('Ctrl Pts',(36.7235100063757,-0.931575925178158,
-7.64337092805759));
#68400=CARTESIAN_POINT('Ctrl Pts',(36.7770958473711,-0.925803188072458,
-7.57284438220232));
#68401=CARTESIAN_POINT('Ctrl Pts',(36.8336190328546,-0.92003045096676,-7.50471118571648));
#68402=CARTESIAN_POINT('Ctrl Pts',(36.8928280636448,-0.914257713861061,
-7.43921757870213));
#68403=CARTESIAN_POINT('Ctrl Pts',(36.9577796272717,-0.907925093711437,
-7.36737191383699));
#68404=CARTESIAN_POINT('Ctrl Pts',(37.0262031313875,-0.901592473561813,
-7.29843824581509));
#68405=CARTESIAN_POINT('Ctrl Pts',(37.0978072860804,-0.895259853412189,
-7.23277042021453));
#68406=CARTESIAN_POINT('Ctrl Pts',(37.169315073026,-0.888935755957113,-7.16719097301123));
#68407=CARTESIAN_POINT('Ctrl Pts',(37.2439946829859,-0.882611658502038,
-7.10486892544389));
#68408=CARTESIAN_POINT('Ctrl Pts',(37.3215159596994,-0.876287561046962,
-7.04612356838108));
#68409=CARTESIAN_POINT('Ctrl Pts',(37.3989560947817,-0.869970083033735,
-6.9874397001675));
#68410=CARTESIAN_POINT('Ctrl Pts',(37.4792316367028,-0.863652605020507,
-6.93232534248509));
#68411=CARTESIAN_POINT('Ctrl Pts',(37.561977874681,-0.85733512700728,-6.88106086116467));
#68412=CARTESIAN_POINT('Ctrl Pts',(37.6446653766551,-0.851022133347939,
-6.82983276906089));
#68413=CARTESIAN_POINT('Ctrl Pts',(37.729819717368,-0.844709139688599,-6.78244935007139));
#68414=CARTESIAN_POINT('Ctrl Pts',(37.8170463918134,-0.838396146029258,
-6.73914825044412));
#68415=CARTESIAN_POINT('Ctrl Pts',(37.9042415451658,-0.83208543369568,-6.69586279853004));
#68416=CARTESIAN_POINT('Ctrl Pts',(37.9935071529134,-0.825774721362104,
-6.6566569289384));
#68417=CARTESIAN_POINT('Ctrl Pts',(38.0844240759997,-0.819464009028525,
-6.62172236761779));
#68418=CARTESIAN_POINT('Ctrl Pts',(38.1753327694161,-0.813153867931602,
-6.5867909685237));
#68419=CARTESIAN_POINT('Ctrl Pts',(38.2678920726935,-0.806843726834677,
-6.55613026564564));
#68420=CARTESIAN_POINT('Ctrl Pts',(38.3616638164926,-0.800533585737753,
-6.529883458641));
#68421=CARTESIAN_POINT('Ctrl Pts',(38.4554524700205,-0.794222306741826,
-6.50363191858602));
#68422=CARTESIAN_POINT('Ctrl Pts',(38.5504535771808,-0.7879110277459,-6.48179597310336));
#68423=CARTESIAN_POINT('Ctrl Pts',(38.646215817656,-0.781599748749973,-6.46446839057565));
#68424=CARTESIAN_POINT('Ctrl Pts',(38.7420804694343,-0.775281720263821,
-6.44712227735884));
#68425=CARTESIAN_POINT('Ctrl Pts',(38.8387074485619,-0.76896369177767,-6.43429423073547));
#68426=CARTESIAN_POINT('Ctrl Pts',(38.9356374987543,-0.762645663291519,
-6.42602547270309));
#68427=CARTESIAN_POINT('Ctrl Pts',(39.0326243468245,-0.756323932644797,
-6.41775186944565));
#68428=CARTESIAN_POINT('Ctrl Pts',(39.1299141827867,-0.750002201998074,
-6.4140428913081));
#68429=CARTESIAN_POINT('Ctrl Pts',(39.227047016857,-0.743680471351352,-6.41488760463884));
#68430=CARTESIAN_POINT('Ctrl Pts',(39.3243355963527,-0.737348604269936,
-6.41573367240589));
#68431=CARTESIAN_POINT('Ctrl Pts',(39.4214662349143,-0.731016737188519,
-6.42114798715704));
#68432=CARTESIAN_POINT('Ctrl Pts',(39.5179833718286,-0.724684870107102,
-6.431067675572));
#68433=CARTESIAN_POINT('Ctrl Pts',(39.5740421127861,-0.721007217538426,
-6.43682919379571));
#68434=CARTESIAN_POINT('Ctrl Pts',(39.6298940487152,-0.71732956496975,-6.44410962552948));
#68435=CARTESIAN_POINT('Ctrl Pts',(39.6854518178217,-0.713651912401074,
-6.45288880646003));
#68436=CARTESIAN_POINT('Ctrl Pts',(39.7811178008206,-0.707319292251471,
-6.4680058456636));
#68437=CARTESIAN_POINT('Ctrl Pts',(39.8762431598389,-0.700986672101865,
-6.48762197611831));
#68438=CARTESIAN_POINT('Ctrl Pts',(39.970372366564,-0.694654051952262,-6.51168669572269));
#68439=CARTESIAN_POINT('Ctrl Pts',(40.0643748904216,-0.688329954497225,
-6.53571902806079));
#68440=CARTESIAN_POINT('Ctrl Pts',(40.1573835065057,-0.682005857042191,
-6.56418794252481));
#68441=CARTESIAN_POINT('Ctrl Pts',(40.2489503768969,-0.675681759587154,
-6.59699150279447));
#68442=CARTESIAN_POINT('Ctrl Pts',(40.3404214041147,-0.669364281573921,
-6.62976072753093));
#68443=CARTESIAN_POINT('Ctrl Pts',(40.4304532762286,-0.66304680356069,-6.6668554314271));
#68444=CARTESIAN_POINT('Ctrl Pts',(40.5186118622718,-0.656729325547457,
-6.7081234656847));
#68445=CARTESIAN_POINT('Ctrl Pts',(40.6067078704477,-0.650416331888136,
-6.74936220653274));
#68446=CARTESIAN_POINT('Ctrl Pts',(40.692932841173,-0.644103338228813,-6.79476820350162));
#68447=CARTESIAN_POINT('Ctrl Pts',(40.7768721299827,-0.637790344569493,
-6.84414100732919));
#68448=CARTESIAN_POINT('Ctrl Pts',(40.8607810856617,-0.631479632235927,
-6.89349596931263));
#68449=CARTESIAN_POINT('Ctrl Pts',(40.9424056240902,-0.62516891990236,-6.94681466831479));
#68450=CARTESIAN_POINT('Ctrl Pts',(41.0213560881748,-0.618858207568794,
-7.0038509260719));
#68451=CARTESIAN_POINT('Ctrl Pts',(41.1002994057763,-0.612548066471879,
-7.06088202098856));
#68452=CARTESIAN_POINT('Ctrl Pts',(41.17656877593,-0.606237925374965,-7.12162974934534));
#68453=CARTESIAN_POINT('Ctrl Pts',(41.2498047742485,-0.59992778427805,-7.18580547188391));
#68454=CARTESIAN_POINT('Ctrl Pts',(41.3230539791133,-0.593616505282114,
-7.24999276714181));
#68455=CARTESIAN_POINT('Ctrl Pts',(41.3932683968505,-0.587305226286178,
-7.31760899610106));
#68456=CARTESIAN_POINT('Ctrl Pts',(41.4601236447158,-0.580993947290242,
-7.38832694042902));
#68457=CARTESIAN_POINT('Ctrl Pts',(41.5270503897912,-0.574675918804115,
-7.45912051286214));
#68458=CARTESIAN_POINT('Ctrl Pts',(41.5906104920292,-0.568357890317988,
-7.53302210471867));
#68459=CARTESIAN_POINT('Ctrl Pts',(41.6505183947253,-0.56203986183186,-7.60966967600554));
#68460=CARTESIAN_POINT('Ctrl Pts',(41.710461401517,-0.555718131185156,-7.68636216029295));
#68461=CARTESIAN_POINT('Ctrl Pts',(41.7667476945924,-0.549396400538453,
-7.76580347141102));
#68462=CARTESIAN_POINT('Ctrl Pts',(41.8191349904781,-0.543074669891748,
-7.84760244588428));
#68463=CARTESIAN_POINT('Ctrl Pts',(41.8716062855774,-0.53674280281035,-7.92953257905585));
#68464=CARTESIAN_POINT('Ctrl Pts',(41.9201658816691,-0.53041093572895,-8.01382754556607));
#68465=CARTESIAN_POINT('Ctrl Pts',(41.9646174096111,-0.524079068647551,
-8.10007149955682));
#68466=CARTESIAN_POINT('Ctrl Pts',(41.9904355883287,-0.520401416078733,
-8.15016340686659));
#68467=CARTESIAN_POINT('Ctrl Pts',(42.0148688134366,-0.516723763509916,
-8.20091240630828));
#68468=CARTESIAN_POINT('Ctrl Pts',(42.0378862165493,-0.513046110941098,
-8.25223432053687));
#68469=CARTESIAN_POINT('Ctrl Pts',(42.0775203222778,-0.506713490791419,
-8.3406065041737));
#68470=CARTESIAN_POINT('Ctrl Pts',(42.1130914569429,-0.50038087064174,-8.43098526761534));
#68471=CARTESIAN_POINT('Ctrl Pts',(42.1443929096834,-0.49404825049206,-8.5229615544771));
#68472=CARTESIAN_POINT('Ctrl Pts',(42.1756522356715,-0.487724153036946,
-8.61481405595751));
#68473=CARTESIAN_POINT('Ctrl Pts',(42.2026531610915,-0.481400055581832,
-8.70825939711112));
#68474=CARTESIAN_POINT('Ctrl Pts',(42.2252362488598,-0.475075958126719,
-8.80286684643024));
#68475=CARTESIAN_POINT('Ctrl Pts',(42.247795698878,-0.468758480113422,-8.89737526999737));
#68476=CARTESIAN_POINT('Ctrl Pts',(42.2659464032894,-0.462441002100126,
-8.99304296037945));
#68477=CARTESIAN_POINT('Ctrl Pts',(42.2795784644896,-0.456123524086829,
-9.08942321692722));
#68478=CARTESIAN_POINT('Ctrl Pts',(42.2932008492039,-0.449810530427428,
-9.18573505959558));
#68479=CARTESIAN_POINT('Ctrl Pts',(42.3023109063022,-0.443497536768026,
-9.28275803108793));
#68480=CARTESIAN_POINT('Ctrl Pts',(42.3068498357854,-0.437184543108625,
-9.38003534644477));
#68481=CARTESIAN_POINT('Ctrl Pts',(42.3113871250362,-0.430873830774989,
-9.47727750870977));
#68482=CARTESIAN_POINT('Ctrl Pts',(42.311356548589,-0.424563118441352,-9.57477339581393));
#68483=CARTESIAN_POINT('Ctrl Pts',(42.3067512576344,-0.418252406107716,
-9.67206215042368));
#68484=CARTESIAN_POINT('Ctrl Pts',(42.3021463835441,-0.411942265010724,
-9.76934209859467));
#68485=CARTESIAN_POINT('Ctrl Pts',(42.2929676391518,-0.405632123913731,
-9.86641451473711));
#68486=CARTESIAN_POINT('Ctrl Pts',(42.2792602574679,-0.399321982816739,
-9.9628206478441));
#68487=CARTESIAN_POINT('Ctrl Pts',(42.2655504039509,-0.393010703820751,
-10.0592441657354));
#68488=CARTESIAN_POINT('Ctrl Pts',(42.2473103527805,-0.386699424824764,
-10.1550007290107));
#68489=CARTESIAN_POINT('Ctrl Pts',(42.2246367967948,-0.380388145828777,
-10.2496398418352));
#68490=CARTESIAN_POINT('Ctrl Pts',(42.2019389929594,-0.374070117342578,
-10.3443801648528));
#68491=CARTESIAN_POINT('Ctrl Pts',(42.1747983205458,-0.367752088856378,
-10.4380002256121));
#68492=CARTESIAN_POINT('Ctrl Pts',(42.1433618544534,-0.361434060370179,
-10.5300630063079));
#68493=CARTESIAN_POINT('Ctrl Pts',(42.1119069676073,-0.35511232972338,-10.6221797328193));
#68494=CARTESIAN_POINT('Ctrl Pts',(42.0761514351891,-0.348790599076581,
-10.712736955624));
#68495=CARTESIAN_POINT('Ctrl Pts',(42.0362903735297,-0.342468868429782,
-10.8013179736739));
#68496=CARTESIAN_POINT('Ctrl Pts',(41.996365397561,-0.336137001348314,-10.8900410249347));
#68497=CARTESIAN_POINT('Ctrl Pts',(41.9523219452859,-0.329805134266847,
-10.9767811544218));
#68498=CARTESIAN_POINT('Ctrl Pts',(41.9044008992474,-0.323473267185379,
-11.0611466170421));
#68499=CARTESIAN_POINT('Ctrl Pts',(41.8765675673468,-0.319795614617291,
-11.1101474656498));
#68500=CARTESIAN_POINT('Ctrl Pts',(41.8474269568295,-0.316117962049202,
-11.1583477587084));
#68501=CARTESIAN_POINT('Ctrl Pts',(41.8170326830038,-0.312440309481113,
-11.2056756346749));
#68502=CARTESIAN_POINT('Ctrl Pts',(41.7646962027907,-0.30610768933152,-11.2871704076135));
#68503=CARTESIAN_POINT('Ctrl Pts',(41.7084585529873,-0.299775069181927,
-11.3663597582041));
#68504=CARTESIAN_POINT('Ctrl Pts',(41.648549277778,-0.293442449032334,-11.4428469926437));
#68505=CARTESIAN_POINT('Ctrl Pts',(41.5887206308779,-0.287118351577308,
-11.5192312874909));
#68506=CARTESIAN_POINT('Ctrl Pts',(41.5252304472576,-0.280794254122283,
-11.5929203527617));
#68507=CARTESIAN_POINT('Ctrl Pts',(41.4583522621891,-0.274470156667257,
-11.6635452328079));
#68508=CARTESIAN_POINT('Ctrl Pts',(41.391544078612,-0.268152678654027,-11.7340961896918));
#68509=CARTESIAN_POINT('Ctrl Pts',(41.3213552427646,-0.261835200640793,
-11.8015890217252));
#68510=CARTESIAN_POINT('Ctrl Pts',(41.2480997413983,-0.255517722627563,
-11.8656875276688));
#68511=CARTESIAN_POINT('Ctrl Pts',(41.1748962391992,-0.249204728968255,
-11.9297405343821));
#68512=CARTESIAN_POINT('Ctrl Pts',(41.0986307273081,-0.242891735308945,
-11.9904037178899));
#68513=CARTESIAN_POINT('Ctrl Pts',(41.0196535678084,-0.236578741649637,
-12.0473781528673));
#68514=CARTESIAN_POINT('Ctrl Pts',(40.9407049482752,-0.230268029316084,
-12.1043319990001));
#68515=CARTESIAN_POINT('Ctrl Pts',(40.8590469825193,-0.223957316982531,
-12.1575994897006));
#68516=CARTESIAN_POINT('Ctrl Pts',(40.7750618402567,-0.217646604648978,
-12.2069229765725));
#68517=CARTESIAN_POINT('Ctrl Pts',(40.6910843002089,-0.211336463552075,
-12.2562419987529));
#68518=CARTESIAN_POINT('Ctrl Pts',(40.6047803796756,-0.205026322455174,
-12.3016175056337));
#68519=CARTESIAN_POINT('Ctrl Pts',(40.5165589534812,-0.198716181358271,
-12.342836612529));
#68520=CARTESIAN_POINT('Ctrl Pts',(40.4283216184387,-0.192404902362335,
-12.3840631524088));
#68521=CARTESIAN_POINT('Ctrl Pts',(40.338166487181,-0.1860936233664,-12.4211316185863));
#68522=CARTESIAN_POINT('Ctrl Pts',(40.2465236507183,-0.179782344370464,
-12.4538767303161));
#68523=CARTESIAN_POINT('Ctrl Pts',(40.15478280838,-0.173464315884345,-12.4866568607498));
#68524=CARTESIAN_POINT('Ctrl Pts',(40.0615514969825,-0.167146287398224,
-12.5151042587068));
#68525=CARTESIAN_POINT('Ctrl Pts',(39.967276061071,-0.160828258912105,-12.5391031997938));
#68526=CARTESIAN_POINT('Ctrl Pts',(39.8729453827998,-0.154506528265406,
-12.563116203485));
#68527=CARTESIAN_POINT('Ctrl Pts',(39.7775697899156,-0.148184797618707,
-12.5826754719348));
#68528=CARTESIAN_POINT('Ctrl Pts',(39.6816048744415,-0.141863066972008,
-12.5977166152794));
#68529=CARTESIAN_POINT('Ctrl Pts',(39.5854860862143,-0.135531199890615,
-12.6127818760019));
#68530=CARTESIAN_POINT('Ctrl Pts',(39.488776522994,-0.129199332809222,-12.6233144983368));
#68531=CARTESIAN_POINT('Ctrl Pts',(39.3919358958253,-0.122867465727829,
-12.6293020575958));
#68532=CARTESIAN_POINT('Ctrl Pts',(39.3356892664025,-0.119189813158928,
-12.6327797305172));
#68533=CARTESIAN_POINT('Ctrl Pts',(39.2793984241823,-0.115512160590027,
-12.634725113714));
#68534=CARTESIAN_POINT('Ctrl Pts',(39.2231528518321,-0.111834508021126,
-12.6351438227761));
#68535=CARTESIAN_POINT('Ctrl Pts',(39.126302527308,-0.105501887871624,-12.6358648059014));
#68536=CARTESIAN_POINT('Ctrl Pts',(39.0292502677637,-0.0991692677221215,
-12.6320588343527));
#68537=CARTESIAN_POINT('Ctrl Pts',(38.9324537304411,-0.0928366475726188,
-12.6237012838519));
#68538=CARTESIAN_POINT('Ctrl Pts',(38.8357874657868,-0.0865125501176967,
-12.6153549812782));
#68539=CARTESIAN_POINT('Ctrl Pts',(38.7393766713302,-0.080188452662775,
-12.6024693121629));
#68540=CARTESIAN_POINT('Ctrl Pts',(38.6436798232554,-0.0738643552078528,
-12.5850716517505));
#68541=CARTESIAN_POINT('Ctrl Pts',(38.5480831412077,-0.067546877194739,
-12.567692201494));
#68542=CARTESIAN_POINT('Ctrl Pts',(38.4531993478962,-0.0612293991816249,
-12.5458102267209));
#68543=CARTESIAN_POINT('Ctrl Pts',(38.3594816031123,-0.054911921168511,
-12.5195048801752));
#68544=CARTESIAN_POINT('Ctrl Pts',(38.2658303822694,-0.0485989275093033,
-12.4932182060307));
#68545=CARTESIAN_POINT('Ctrl Pts',(38.1733439842851,-0.0422859338500956,
-12.4625145201786));
#68546=CARTESIAN_POINT('Ctrl Pts',(38.0824642382336,-0.0359729401908879,
-12.4275238111122));
#68547=CARTESIAN_POINT('Ctrl Pts',(37.991617333385,-0.0296622278574401,
-12.3925457466342));
#68548=CARTESIAN_POINT('Ctrl Pts',(37.9023763345141,-0.0233515155239927,
-12.3532838941925));
#68549=CARTESIAN_POINT('Ctrl Pts',(37.8151658928123,-0.0170408031905449,
-12.3099174401532));
#68550=CARTESIAN_POINT('Ctrl Pts',(37.7279633452747,-0.0107306620937389,
-12.2665549115832));
#68551=CARTESIAN_POINT('Ctrl Pts',(37.6427913809412,-0.00442052099693118,
-12.2190887150281));
#68552=CARTESIAN_POINT('Ctrl Pts',(37.5600517642171,0.00188962009987481,
-12.1677448679077));
#68553=CARTESIAN_POINT('Ctrl Pts',(37.4772972271731,0.00820089909564809,
-12.1163917620229));
#68554=CARTESIAN_POINT('Ctrl Pts',(37.3969762804557,0.014512178091419,-12.0611598473829));
#68555=CARTESIAN_POINT('Ctrl Pts',(37.3194624229793,0.0208234570871921,
-12.0023189286632));
#68556=CARTESIAN_POINT('Ctrl Pts',(37.2418656696231,0.0271414855732131,
-11.9434150835213));
#68557=CARTESIAN_POINT('Ctrl Pts',(37.1670823477209,0.0334595140592348,
-11.8808947936913));
#68558=CARTESIAN_POINT('Ctrl Pts',(37.0954533431046,0.0397775425452558,
-11.8150685626964));
#68559=CARTESIAN_POINT('Ctrl Pts',(37.0237823662056,0.0460992731918534,
-11.7492037596568));
#68560=CARTESIAN_POINT('Ctrl Pts',(36.9552696947197,0.0524210038384517,
-11.6800294685806));
#68561=CARTESIAN_POINT('Ctrl Pts',(36.8902182827396,0.0587427344850493,
-11.6078919970823));
#68562=CARTESIAN_POINT('Ctrl Pts',(36.825062565558,0.0650746015663302,-11.5356388584022));
#68563=CARTESIAN_POINT('Ctrl Pts',(36.7633794671254,0.0714064686476086,
-11.4604133898497));
#68564=CARTESIAN_POINT('Ctrl Pts',(36.7054306783924,0.0777383357288892,
-11.3825937533794));
#68565=CARTESIAN_POINT('Ctrl Pts',(36.6717730685476,0.0814159882988748,
-11.337394828262));
#68566=CARTESIAN_POINT('Ctrl Pts',(36.6393744022191,0.0850936408688613,
-11.2913213016371));
#68567=CARTESIAN_POINT('Ctrl Pts',(36.6082788899335,0.0887712934388469,
-11.2444511742227));
#68568=CARTESIAN_POINT('Ctrl Pts',(36.553808851527,0.0952134409389027,-11.1623487275114));
#68569=CARTESIAN_POINT('Ctrl Pts',(36.5031554741128,0.101655588438959,-11.0775225261828));
#68570=CARTESIAN_POINT('Ctrl Pts',(36.4565960757825,0.108097735939015,-10.990355097404));
#68571=CARTESIAN_POINT('Ctrl Pts',(36.410105389827,0.114530376115748,-10.9033163103443));
#68572=CARTESIAN_POINT('Ctrl Pts',(36.3676968630231,0.120963016292481,-10.8139435316009));
#68573=CARTESIAN_POINT('Ctrl Pts',(36.3296046919639,0.127395656469215,-10.7226482908202));
#68574=CARTESIAN_POINT('Ctrl Pts',(36.2902379643555,0.134043531520685,-10.6282983292447));
#68575=CARTESIAN_POINT('Ctrl Pts',(36.2554817982704,0.140691406572158,-10.5318953484093));
#68576=CARTESIAN_POINT('Ctrl Pts',(36.2255435723802,0.147339281623628,-10.4339222260958));
#68577=CARTESIAN_POINT('Ctrl Pts',(36.1966455897759,0.153756167457046,-10.3393533095983));
#68578=CARTESIAN_POINT('Ctrl Pts',(36.172236440122,0.160173053290463,-10.2433219900157));
#68579=CARTESIAN_POINT('Ctrl Pts',(36.1524536760506,0.166589939123881,-10.1462825897148));
#68580=CARTESIAN_POINT('Ctrl Pts',(36.1326843947812,0.173002451574465,-10.0493093259259));
#68581=CARTESIAN_POINT('Ctrl Pts',(36.1175353100499,0.179414964025047,-9.95132975601396));
#68582=CARTESIAN_POINT('Ctrl Pts',(36.1070935047393,0.185827476475631,-9.85281101945179));
#68583=CARTESIAN_POINT('Ctrl Pts',(36.0966567355883,0.192236896124194,-9.75433979920243));
#68584=CARTESIAN_POINT('Ctrl Pts',(36.09092277005,0.198646315772756,-9.65533034449738));
#68585=CARTESIAN_POINT('Ctrl Pts',(36.0899270638497,0.205055735421318,-9.55625675487976));
#68586=CARTESIAN_POINT('Ctrl Pts',(36.0898175717336,0.205760542643165,-9.54536219885355));
#68587=CARTESIAN_POINT('Ctrl Pts',(36.0897653235704,0.206465349865013,-9.53446687122886));
#68588=CARTESIAN_POINT('Ctrl Pts',(36.0897703280922,0.20717015708686,-9.52357140469285));
#68589=CARTESIAN_POINT('',(36.089648114499,1.47717011009206,-9.52360304152045));
#68590=CARTESIAN_POINT('Ctrl Pts',(36.0940691872287,0.207171403211074,-9.52355414230154));
#68591=CARTESIAN_POINT('Ctrl Pts',(36.0923009265865,0.234573300440328,-9.10053859340738));
#68592=CARTESIAN_POINT('Ctrl Pts',(36.3693104484986,0.328843798156245,-7.64746453123767));
#68593=CARTESIAN_POINT('Ctrl Pts',(38.573297397462,0.489982896358807,-5.90905004425038));
#68594=CARTESIAN_POINT('Ctrl Pts',(41.8853621052223,0.690588697818804,-7.02366423740838));
#68595=CARTESIAN_POINT('Ctrl Pts',(42.7624419786364,0.891194499278781,-10.4063951343764));
#68596=CARTESIAN_POINT('Ctrl Pts',(40.4092341470354,1.09180030073876,-12.9899102462532));
#68597=CARTESIAN_POINT('Ctrl Pts',(37.050354743051,1.28712498014314,-12.4462743804594));
#68598=CARTESIAN_POINT('Ctrl Pts',(36.0908975709741,1.41558105906088,-10.4677289734402));
#68599=CARTESIAN_POINT('Ctrl Pts',(36.0855589174695,1.47716853749195,-9.52362531105487));
#68600=CARTESIAN_POINT('',(36.0897712274935,2.74717015704593,-9.52776325396536));
#68601=CARTESIAN_POINT('Ctrl Pts',(36.0897703140206,1.47717015708686,-9.52360237602881));
#68602=CARTESIAN_POINT('Ctrl Pts',(36.0898066400594,1.48245073927748,-9.4427635192502));
#68603=CARTESIAN_POINT('Ctrl Pts',(36.0929943645843,1.4877313214681,-9.36199917881014));
#68604=CARTESIAN_POINT('Ctrl Pts',(36.0993176964666,1.49301190365872,-9.28148428088808));
#68605=CARTESIAN_POINT('Ctrl Pts',(36.1069008108343,1.49934452377502,-9.18492858989839));
#68606=CARTESIAN_POINT('Ctrl Pts',(36.1190115282862,1.50567714389132,-9.08855973115984));
#68607=CARTESIAN_POINT('Ctrl Pts',(36.1356351547736,1.51200976400762,-8.9928357882755));
#68608=CARTESIAN_POINT('Ctrl Pts',(36.1522364085168,1.51833386142944,-8.89724067451801));
#68609=CARTESIAN_POINT('Ctrl Pts',(36.1733384254317,1.52465795885125,-8.80228917874195));
#68610=CARTESIAN_POINT('Ctrl Pts',(36.1988746331224,1.53098205627306,-8.70843574338361));
#68611=CARTESIAN_POINT('Ctrl Pts',(36.2243841120284,1.53729953425319,-8.61468054454834));
#68612=CARTESIAN_POINT('Ctrl Pts',(36.254318440425,1.54361701223332,-8.52202154094052));
#68613=CARTESIAN_POINT('Ctrl Pts',(36.2885599146599,1.54993449021344,-8.43090344010476));
#68614=CARTESIAN_POINT('Ctrl Pts',(36.3227770831705,1.55624748383999,-8.33985001789291));
#68615=CARTESIAN_POINT('Ctrl Pts',(36.3612951659185,1.56256047746653,-8.25033573214745));
#68616=CARTESIAN_POINT('Ctrl Pts',(36.4039467817926,1.56887347109307,-8.16278964405193));
#68617=CARTESIAN_POINT('Ctrl Pts',(36.4465829846588,1.57518418339406,-8.07527519247295));
#68618=CARTESIAN_POINT('Ctrl Pts',(36.493349561246,1.58149489569505,-7.98972791802753));
#68619=CARTESIAN_POINT('Ctrl Pts',(36.5440315860174,1.58780560799605,-7.90655555028078));
#68620=CARTESIAN_POINT('Ctrl Pts',(36.5947090231266,1.59411574906064,-7.82339071117447));
#68621=CARTESIAN_POINT('Ctrl Pts',(36.6493009760121,1.60042589012524,-7.74260072468242));
#68622=CARTESIAN_POINT('Ctrl Pts',(36.707547822154,1.60673603118983,-7.664566503728));
#68623=CARTESIAN_POINT('Ctrl Pts',(36.7658051718718,1.61304731015373,-7.58651821096692));
#68624=CARTESIAN_POINT('Ctrl Pts',(36.8277184622553,1.61935858911762,-7.51122702116066));
#68625=CARTESIAN_POINT('Ctrl Pts',(36.8929868674292,1.62566986808151,-7.4390419325773));
#68626=CARTESIAN_POINT('Ctrl Pts',(36.9583250727981,1.63198789653623,-7.36677964686851));
#68627=CARTESIAN_POINT('Ctrl Pts',(37.0270252625657,1.63830592499096,-7.2976304190209));
#68628=CARTESIAN_POINT('Ctrl Pts',(37.0987488571929,1.64462395344569,-7.2319072657758));
#68629=CARTESIAN_POINT('Ctrl Pts',(37.1705144795331,1.6509456840613,-7.16614560088277));
#68630=CARTESIAN_POINT('Ctrl Pts',(37.2453066987127,1.65726741467692,-7.10381428805981));
#68631=CARTESIAN_POINT('Ctrl Pts',(37.3227545141559,1.66358914529253,-7.04518548298915));
#68632=CARTESIAN_POINT('Ctrl Pts',(37.400326511541,1.66992101234362,-6.98646267089164));
#68633=CARTESIAN_POINT('Ctrl Pts',(37.4805622473205,1.67625287939471,-6.93145446822313));
#68634=CARTESIAN_POINT('Ctrl Pts',(37.5630625206456,1.6825847464458,-6.88038918901383));
#68635=CARTESIAN_POINT('Ctrl Pts',(37.6109800410629,1.68626239933677,-6.85072963201479));
#68636=CARTESIAN_POINT('Ctrl Pts',(37.6596610351012,1.68994005222774,-6.82239935129324));
#68637=CARTESIAN_POINT('Ctrl Pts',(37.7090239996132,1.69361770511871,-6.79543570891425));
#68638=CARTESIAN_POINT('Ctrl Pts',(37.7940230226877,1.69995032525265,-6.74900650265803));
#68639=CARTESIAN_POINT('Ctrl Pts',(37.8813404693319,1.70628294538659,-6.70647075351165));
#68640=CARTESIAN_POINT('Ctrl Pts',(37.9705847167663,1.71261556552053,-6.66806655410885));
#68641=CARTESIAN_POINT('Ctrl Pts',(38.0597088557022,1.71893966295953,-6.62971404062263));
#68642=CARTESIAN_POINT('Ctrl Pts',(38.1507542430837,1.72526376039853,-6.59548219671587));
#68643=CARTESIAN_POINT('Ctrl Pts',(38.2433039474916,1.73158785783753,-6.56556368272354));
#68644=CARTESIAN_POINT('Ctrl Pts',(38.3357567799864,1.73790533583434,-6.53567648448427));
#68645=CARTESIAN_POINT('Ctrl Pts',(38.4297103852599,1.74422281383116,-6.51009377439101));
#68646=CARTESIAN_POINT('Ctrl Pts',(38.5247280343997,1.75054029182797,-6.488960075135));
#68647=CARTESIAN_POINT('Ctrl Pts',(38.6196782368767,1.75685328547043,-6.46784137727609));
#68648=CARTESIAN_POINT('Ctrl Pts',(38.7156905559805,1.7631662791129,-6.45116550652999));
#68649=CARTESIAN_POINT('Ctrl Pts',(38.8123142101335,1.76947927275536,-6.43902683400591));
#68650=CARTESIAN_POINT('Ctrl Pts',(38.908902947404,1.77578998507179,-6.426892548033));
#68651=CARTESIAN_POINT('Ctrl Pts',(39.0061021472945,1.78210069738822,-6.41929225682063));
#68652=CARTESIAN_POINT('Ctrl Pts',(39.1034529022483,1.78841140970466,-6.41626885839002));
#68653=CARTESIAN_POINT('Ctrl Pts',(39.2007948451471,1.79472155078419,-6.41324573363323));
#68654=CARTESIAN_POINT('Ctrl Pts',(39.2982878787266,1.80103169186372,-6.41479869131284));
#68655=CARTESIAN_POINT('Ctrl Pts',(39.3954711189734,1.80734183294325,-6.42091854253995));
#68656=CARTESIAN_POINT('Ctrl Pts',(39.4926718841358,1.81365311192156,-6.42703949735114));
#68657=CARTESIAN_POINT('Ctrl Pts',(39.5895623085709,1.81996439089987,-6.43772895384787));
#68658=CARTESIAN_POINT('Ctrl Pts',(39.6856857104737,1.82627566987818,-6.45292577505985));
#68659=CARTESIAN_POINT('Ctrl Pts',(39.781911909914,1.83259369834646,-6.46813884825383));
#68660=CARTESIAN_POINT('Ctrl Pts',(39.8773690165199,1.83891172681473,-6.48786884127477));
#68661=CARTESIAN_POINT('Ctrl Pts',(39.971609841885,1.84522975528301,-6.51200333475024));
#68662=CARTESIAN_POINT('Ctrl Pts',(40.065905889327,1.85155148591172,-6.53615197025862));
#68663=CARTESIAN_POINT('Ctrl Pts',(40.1589838184526,1.85787321654042,-6.56471011727024));
#68664=CARTESIAN_POINT('Ctrl Pts',(40.2504129351984,1.86419494716912,-6.59751587220905));
#68665=CARTESIAN_POINT('Ctrl Pts',(40.3419886518735,1.87052681423244,-6.63037422878645));
#68666=CARTESIAN_POINT('Ctrl Pts',(40.4319098730917,1.87685868129575,-6.66749362636479));
#68667=CARTESIAN_POINT('Ctrl Pts',(40.5197672021754,1.88319054835907,-6.7086645823052));
#68668=CARTESIAN_POINT('Ctrl Pts',(40.5707961868006,1.88686820109894,-6.73257735201492));
#68669=CARTESIAN_POINT('Ctrl Pts',(40.6211293892347,1.89054585383882,-6.75785604784021));
#68670=CARTESIAN_POINT('Ctrl Pts',(40.6706909720238,1.89422350657869,-6.78445284337091));
#68671=CARTESIAN_POINT('Ctrl Pts',(40.7560320055585,1.90055612688944,-6.83025037225457));
#68672=CARTESIAN_POINT('Ctrl Pts',(40.8393800241139,1.90688874720019,-6.88011754359707));
#68673=CARTESIAN_POINT('Ctrl Pts',(40.9203215848964,1.91322136751093,-6.93385656563757));
#68674=CARTESIAN_POINT('Ctrl Pts',(41.0011542112844,1.91954546512762,-6.98752326354975));
#68675=CARTESIAN_POINT('Ctrl Pts',(41.0795864557308,1.9258695627443,-7.04505121542693));
#68676=CARTESIAN_POINT('Ctrl Pts',(41.1552290854296,1.93219366036099,-7.10619660236922));
#68677=CARTESIAN_POINT('Ctrl Pts',(41.2307925398855,1.93851113853614,-7.16727798835221));
#68678=CARTESIAN_POINT('Ctrl Pts',(41.303571846174,1.94482861671129,-7.23196900843589));
#68679=CARTESIAN_POINT('Ctrl Pts',(41.3732072593789,1.95114609488644,-7.29998295272083));
#68680=CARTESIAN_POINT('Ctrl Pts',(41.4427932430732,1.95745908870744,-7.36794861846727));
#68681=CARTESIAN_POINT('Ctrl Pts',(41.5092394583548,1.96377208252843,-7.43923221443983));
#68682=CARTESIAN_POINT('Ctrl Pts',(41.5722204748629,1.97008507634943,-7.51350784949553));
#68683=CARTESIAN_POINT('Ctrl Pts',(41.6351787319272,1.97639578884446,-7.58775664357211));
#68684=CARTESIAN_POINT('Ctrl Pts',(41.6946739958512,1.98270650133949,-7.66499499510333));
#68685=CARTESIAN_POINT('Ctrl Pts',(41.7504194970726,1.98901721383451,-7.74486207223943));
#68686=CARTESIAN_POINT('Ctrl Pts',(41.8061599522876,1.99532735509248,-7.82472191991698));
#68687=CARTESIAN_POINT('Ctrl Pts',(41.8581510695283,2.00163749635045,-7.90720966138386));
#68688=CARTESIAN_POINT('Ctrl Pts',(41.906148615479,2.00794763760841,-7.99193433805305));
#68689=CARTESIAN_POINT('Ctrl Pts',(41.954154816756,2.01425891676477,-8.07667429299728));
#68690=CARTESIAN_POINT('Ctrl Pts',(41.9981658009022,2.02057019592113,-8.16365160380412));
#68691=CARTESIAN_POINT('Ctrl Pts',(42.0379831319713,2.0268814750775,-8.25245043493534));
#68692=CARTESIAN_POINT('Ctrl Pts',(42.0778430449963,2.03319950372217,-8.34134423044031));
#68693=CARTESIAN_POINT('Ctrl Pts',(42.1135001720061,2.03951753236684,-8.43206303564065));
#68694=CARTESIAN_POINT('Ctrl Pts',(42.14480420926,2.04583556101151,-8.52417093266402));
#68695=CARTESIAN_POINT('Ctrl Pts',(42.1761265896638,2.05215729181592,-8.6163328019258));
#68696=CARTESIAN_POINT('Ctrl Pts',(42.2030906799729,2.05847902262034,-8.70988496381116));
#68697=CARTESIAN_POINT('Ctrl Pts',(42.2255966297227,2.06480075342475,-8.80437826350402));
#68698=CARTESIAN_POINT('Ctrl Pts',(42.2481386661128,2.07113262066097,-8.89902307627427));
#68699=CARTESIAN_POINT('Ctrl Pts',(42.2662082068624,2.07746448789719,-8.99461161071951));
#68700=CARTESIAN_POINT('Ctrl Pts',(42.2797568848875,2.08379635513341,-9.09068653844481));
#68701=CARTESIAN_POINT('Ctrl Pts',(42.287626176362,2.08747400610183,-9.14648841138497));
#68702=CARTESIAN_POINT('Ctrl Pts',(42.2939713403462,2.09115165707025,-9.20245429005291));
#68703=CARTESIAN_POINT('Ctrl Pts',(42.2987909716045,2.09482930803867,-9.25849452688035));
#68704=CARTESIAN_POINT('Ctrl Pts',(42.3070899898936,2.10116192790374,-9.35499131790932));
#68705=CARTESIAN_POINT('Ctrl Pts',(42.3108917458408,2.10749454776881,-9.45204373863104));
#68706=CARTESIAN_POINT('Ctrl Pts',(42.3101358709359,2.11382716763389,-9.54919746304091));
#68707=CARTESIAN_POINT('Ctrl Pts',(42.3093810133178,2.12015126480478,-9.64622043406605));
#68708=CARTESIAN_POINT('Ctrl Pts',(42.3040807195195,2.12647536197567,-9.74334400419317));
#68709=CARTESIAN_POINT('Ctrl Pts',(42.2942263969418,2.13279945914657,-9.84010896110503));
#68710=CARTESIAN_POINT('Ctrl Pts',(42.2843823888969,2.13911693687639,-9.93677263400554));
#68711=CARTESIAN_POINT('Ctrl Pts',(42.2699938725908,2.14543441460622,-10.0330780071489));
#68712=CARTESIAN_POINT('Ctrl Pts',(42.2511042901921,2.15175189233604,-10.1285671157971));
#68713=CARTESIAN_POINT('Ctrl Pts',(42.2322281162346,2.15806488571424,-10.2239884431632));
#68714=CARTESIAN_POINT('Ctrl Pts',(42.2088573126661,2.16437787909245,-10.318594230155));
#68715=CARTESIAN_POINT('Ctrl Pts',(42.1810868882884,2.17069087247065,-10.4119338291975));
#68716=CARTESIAN_POINT('Ctrl Pts',(42.1533264992995,2.1770015845246,-10.5052396981411));
#68717=CARTESIAN_POINT('Ctrl Pts',(42.1211697732094,2.18331229657855,-10.5972798695859));
#68718=CARTESIAN_POINT('Ctrl Pts',(42.0847621102454,2.1896230086325,-10.687616970542));
#68719=CARTESIAN_POINT('Ctrl Pts',(42.0483577428405,2.19593314945165,-10.777945894339));
#68720=CARTESIAN_POINT('Ctrl Pts',(42.0077033672699,2.20224329027079,-10.8665716486195));
#68721=CARTESIAN_POINT('Ctrl Pts',(41.96299286245,2.20855343108994,-10.9530760116151));
#68722=CARTESIAN_POINT('Ctrl Pts',(41.9182742950308,2.21486470981027,-11.0395959738533));
#68723=CARTESIAN_POINT('Ctrl Pts',(41.8694983464578,2.2211759885306,-11.1239933965491));
#68724=CARTESIAN_POINT('Ctrl Pts',(41.8169047608535,2.22748726725093,-11.2058748095924));
#68725=CARTESIAN_POINT('Ctrl Pts',(41.7642549298878,2.23380529546644,-11.2878437893915));
#68726=CARTESIAN_POINT('Ctrl Pts',(41.7077795477114,2.24012332368196,-11.3672910191359));
#68727=CARTESIAN_POINT('Ctrl Pts',(41.6477614849951,2.24644135189747,-11.4438523563512));
#68728=CARTESIAN_POINT('Ctrl Pts',(41.5877082536086,2.25276308227597,-11.5204585560679));
#68729=CARTESIAN_POINT('Ctrl Pts',(41.5241084935469,2.25908481265448,-11.5941751649656));
#68730=CARTESIAN_POINT('Ctrl Pts',(41.4572837385655,2.26540654303299,-11.6646730536481));
#68731=CARTESIAN_POINT('Ctrl Pts',(41.3903518348838,2.2717384098526,-11.7352839806374));
#68732=CARTESIAN_POINT('Ctrl Pts',(41.3201849258317,2.27807027667222,-11.8026655791142));
#68733=CARTESIAN_POINT('Ctrl Pts',(41.2471395313558,2.28440214349183,-11.8665273630817));
#68734=CARTESIAN_POINT('Ctrl Pts',(41.2047135308746,2.28807979882744,-11.9036193672632));
#68735=CARTESIAN_POINT('Ctrl Pts',(41.1613170758136,2.29175745416305,-11.939524741118));
#68736=CARTESIAN_POINT('Ctrl Pts',(41.1170244675346,2.29543510949865,-11.9741933046973));
#68737=CARTESIAN_POINT('Ctrl Pts',(41.0407562374487,2.30176772964027,-12.0338897210192));
#68738=CARTESIAN_POINT('Ctrl Pts',(40.9615644445541,2.30810034978189,-12.0901239304866));
#68739=CARTESIAN_POINT('Ctrl Pts',(40.879796534497,2.3144329699235,-12.1425970384289));
#68740=CARTESIAN_POINT('Ctrl Pts',(40.7981386710133,2.32075706736781,-12.194999525932));
#68741=CARTESIAN_POINT('Ctrl Pts',(40.7139119462155,2.32708116481211,-12.2436507383664));
#68742=CARTESIAN_POINT('Ctrl Pts',(40.627496199149,2.33340526225642,-12.2882924663009));
#68743=CARTESIAN_POINT('Ctrl Pts',(40.5411709036052,2.33972274025621,-12.332887467656));
#68744=CARTESIAN_POINT('Ctrl Pts',(40.4526615274063,2.34604021825601,-12.3734811281637));
#68745=CARTESIAN_POINT('Ctrl Pts',(40.362375308086,2.3523576962558,-12.4098594932946));
#68746=CARTESIAN_POINT('Ctrl Pts',(40.272153176953,2.35867068989778,-12.4462120358415));
#68747=CARTESIAN_POINT('Ctrl Pts',(40.180157114639,2.36498368353976,-12.4783550686288));
#68748=CARTESIAN_POINT('Ctrl Pts',(40.0868164187175,2.37129667718173,-12.5061218177715));
#68749=CARTESIAN_POINT('Ctrl Pts',(39.9935094533476,2.37760738949555,-12.5338785328367));
#68750=CARTESIAN_POINT('Ctrl Pts',(39.8988592386145,2.38391810180936,-12.5572619820688));
#68751=CARTESIAN_POINT('Ctrl Pts',(39.803311501106,2.39022881412317,-12.5761548445684));
#68752=CARTESIAN_POINT('Ctrl Pts',(39.7077724124777,2.39653895519797,-12.5950459969061));
#68753=CARTESIAN_POINT('Ctrl Pts',(39.6113363916488,2.40284909627276,-12.6094472860701));
#68754=CARTESIAN_POINT('Ctrl Pts',(39.5144596276978,2.40915923734756,-12.6192924547379));
#68755=CARTESIAN_POINT('Ctrl Pts',(39.4175653941298,2.41547051631904,-12.6291393987678));
#68756=CARTESIAN_POINT('Ctrl Pts',(39.3202306946555,2.42178179529052,-12.6344285463271));
#68757=CARTESIAN_POINT('Ctrl Pts',(39.2229160625637,2.42809307426199,-12.6351455764926));
#68758=CARTESIAN_POINT('Ctrl Pts',(39.1254973590417,2.43441110272032,-12.6358633734735));
#68759=CARTESIAN_POINT('Ctrl Pts',(39.0280992037688,2.44072913117864,-12.6319992880725));
#68760=CARTESIAN_POINT('Ctrl Pts',(38.9311811454028,2.44704715963696,-12.6235911437802));
#68761=CARTESIAN_POINT('Ctrl Pts',(38.8342062962151,2.45336889025393,-12.6151780725895));
#68762=CARTESIAN_POINT('Ctrl Pts',(38.7377125373498,2.45969062087089,-12.6022156986011));
#68763=CARTESIAN_POINT('Ctrl Pts',(38.6421512321369,2.46601235148786,-12.5847933598682));
#68764=CARTESIAN_POINT('Ctrl Pts',(38.5464367013714,2.47234421853678,-12.5673430856914));
#68765=CARTESIAN_POINT('Ctrl Pts',(38.4516580355461,2.4786760855857,-12.5454186655204));
#68766=CARTESIAN_POINT('Ctrl Pts',(38.3582533628398,2.48500795263461,-12.5191598574107));
#68767=CARTESIAN_POINT('Ctrl Pts',(38.3040023889813,2.48868560540929,-12.503908308735));
#68768=CARTESIAN_POINT('Ctrl Pts',(38.2502146079462,2.49236325818397,-12.4871954868035));
#68769=CARTESIAN_POINT('Ctrl Pts',(38.1969726538517,2.49604091095864,-12.4690561808122));
#68770=CARTESIAN_POINT('Ctrl Pts',(38.1052943060448,2.50237353221427,-12.4378217599138));
#68771=CARTESIAN_POINT('Ctrl Pts',(38.0149170724324,2.50870615346988,-12.4022466924457));
#68772=CARTESIAN_POINT('Ctrl Pts',(37.9262811623457,2.5150387747255,-12.3624585416363));
#68773=CARTESIAN_POINT('Ctrl Pts',(37.8377645419445,2.52136287329097,-12.3227239392813));
#68774=CARTESIAN_POINT('Ctrl Pts',(37.7509849827616,2.52768697185644,-12.2787877008172));
#68775=CARTESIAN_POINT('Ctrl Pts',(37.666366331892,2.53401107042191,-12.230826754422));
#68776=CARTESIAN_POINT('Ctrl Pts',(37.5818362514309,2.54032854954844,-12.1829160087871));
#68777=CARTESIAN_POINT('Ctrl Pts',(37.4994629611205,2.54664602867496,-12.1309891447054));
#68778=CARTESIAN_POINT('Ctrl Pts',(37.4196482263398,2.55296350780148,-12.0752702239027));
#68779=CARTESIAN_POINT('Ctrl Pts',(37.33989014668,2.55927650257376,-12.0195908542206));
#68780=CARTESIAN_POINT('Ctrl Pts',(37.2626873695045,2.56558949734605,-11.9601250287466));
#68781=CARTESIAN_POINT('Ctrl Pts',(37.1884142104197,2.57190249211833,-11.8971410717027));
#68782=CARTESIAN_POINT('Ctrl Pts',(37.1141678914201,2.57821320556423,-11.834179875166));
#68783=CARTESIAN_POINT('Ctrl Pts',(37.0428494201068,2.58452391901013,-11.7677033557909));
#68784=CARTESIAN_POINT('Ctrl Pts',(36.9748006814745,2.59083463245603,-11.6980206270843));
#68785=CARTESIAN_POINT('Ctrl Pts',(36.9067581025372,2.59714477466328,-11.6283442059795));
#68786=CARTESIAN_POINT('Ctrl Pts',(36.8419849732057,2.60345491687054,-11.55546246559));
#68787=CARTESIAN_POINT('Ctrl Pts',(36.7807861377721,2.60976505907779,-11.4797211928315));
#68788=CARTESIAN_POINT('Ctrl Pts',(36.7195762664718,2.6160763391807,-11.4039662617968));
#68789=CARTESIAN_POINT('Ctrl Pts',(36.6619422440296,2.6223876192836,-11.3253511144098));
#68790=CARTESIAN_POINT('Ctrl Pts',(36.6081477987834,2.62869889938651,-11.2442535647626));
#68791=CARTESIAN_POINT('Ctrl Pts',(36.5542958240918,2.63501692896779,-11.1630692868846));
#68792=CARTESIAN_POINT('Ctrl Pts',(36.5042918664585,2.64133495854907,-11.0793976716945));
#68793=CARTESIAN_POINT('Ctrl Pts',(36.4583554512351,2.64765298813035,-10.9936442118933));
#68794=CARTESIAN_POINT('Ctrl Pts',(36.4123921187981,2.65397471986712,-10.9078405034127));
#68795=CARTESIAN_POINT('Ctrl Pts',(36.3705012629379,2.6602964516039,-10.8199529157724));
#68796=CARTESIAN_POINT('Ctrl Pts',(36.3328547974104,2.66661818334068,-10.7304082462666));
#68797=CARTESIAN_POINT('Ctrl Pts',(36.2951479686393,2.6729500514934,-10.640719998695));
#68798=CARTESIAN_POINT('Ctrl Pts',(36.2616992699725,2.67928191964612,-10.5493697740765));
#68799=CARTESIAN_POINT('Ctrl Pts',(36.2326311598061,2.68561378779884,-10.456800847363));
#68800=CARTESIAN_POINT('Ctrl Pts',(36.2157479766986,2.68929142933876,-10.4030354621756));
#68801=CARTESIAN_POINT('Ctrl Pts',(36.2003416177388,2.69296907087869,-10.3488591891142));
#68802=CARTESIAN_POINT('Ctrl Pts',(36.1864281203344,2.69664671241861,-10.2943602400623));
#68803=CARTESIAN_POINT('Ctrl Pts',(36.1545708458623,2.70506728652316,-10.1695758003257));
#68804=CARTESIAN_POINT('Ctrl Pts',(36.1304509100632,2.71348786062771,-10.042742164824));
#68805=CARTESIAN_POINT('Ctrl Pts',(36.1142797500045,2.72190843473227,-9.91469371520203));
#68806=CARTESIAN_POINT('Ctrl Pts',(36.0981085899458,2.73032900883682,-9.78664526558008));
#68807=CARTESIAN_POINT('Ctrl Pts',(36.0898863856997,2.73874958294137,-9.65738158475599));
#68808=CARTESIAN_POINT('Ctrl Pts',(36.0897712274935,2.74717015704592,-9.52776325396536));
#68809=CARTESIAN_POINT('',(36.0897702810346,4.01717015712308,-9.52367781839343));
#68810=CARTESIAN_POINT('Ctrl Pts',(36.0897712274929,2.74717015708686,-9.52776325333526));
#68811=CARTESIAN_POINT('Ctrl Pts',(36.0896857067451,2.75342358861985,-9.43150385974016));
#68812=CARTESIAN_POINT('Ctrl Pts',(36.0940731888462,2.75967702015284,-9.33513286548138));
#68813=CARTESIAN_POINT('Ctrl Pts',(36.1029378738701,2.76593045168583,-9.23910344564557));
#68814=CARTESIAN_POINT('Ctrl Pts',(36.1117861814384,2.77217233003931,-9.1432514396215));
#68815=CARTESIAN_POINT('Ctrl Pts',(36.1250951477522,2.7784142083928,-9.04774019554694));
#68816=CARTESIAN_POINT('Ctrl Pts',(36.1428168738931,2.78465608674629,-8.95301924302696));
#68817=CARTESIAN_POINT('Ctrl Pts',(36.1605334922914,2.79089616607027,-8.85832559090906));
#68818=CARTESIAN_POINT('Ctrl Pts',(36.1826602619927,2.79713624539425,-8.76442221820453));
#68819=CARTESIAN_POINT('Ctrl Pts',(36.2090978226404,2.80337632471823,-8.67175043605885));
#68820=CARTESIAN_POINT('Ctrl Pts',(36.2355353226703,2.80961638973452,-8.57907886639747));
#68821=CARTESIAN_POINT('Ctrl Pts',(36.2662834698003,2.81585645475081,-8.48763931238116));
#68822=CARTESIAN_POINT('Ctrl Pts',(36.3011928119984,2.8220965197671,-8.3978586869028));
#68823=CARTESIAN_POINT('Ctrl Pts',(36.3362304586393,2.8283595192764,-8.30774808519484));
#68824=CARTESIAN_POINT('Ctrl Pts',(36.3754597886764,2.83462251878569,-8.21930905567815));
#68825=CARTESIAN_POINT('Ctrl Pts',(36.4186812940064,2.84088551829498,-8.1329522606642));
#68826=CARTESIAN_POINT('Ctrl Pts',(36.4618047166418,2.84713430516028,-8.04679143538992));
#68827=CARTESIAN_POINT('Ctrl Pts',(36.5089019591111,2.85338309202559,-7.96270377705377));
#68828=CARTESIAN_POINT('Ctrl Pts',(36.5597299468514,2.85963187889089,-7.88107034841914));
#68829=CARTESIAN_POINT('Ctrl Pts',(36.6107313442735,2.86590198472218,-7.7991584112795));
#68830=CARTESIAN_POINT('Ctrl Pts',(36.6654887176831,2.87217209055346,-7.7197178436163));
#68831=CARTESIAN_POINT('Ctrl Pts',(36.7237151099566,2.87844219638475,-7.64310101327331));
#68832=CARTESIAN_POINT('Ctrl Pts',(36.7819415022302,2.88471230221603,-7.56648418293031));
#68833=CARTESIAN_POINT('Ctrl Pts',(36.8436365754505,2.89098240804732,-7.4926913920379));
#68834=CARTESIAN_POINT('Ctrl Pts',(36.9084766575112,2.8972525138786,-7.4220374649726));
#68835=CARTESIAN_POINT('Ctrl Pts',(36.9739632171509,2.90358513478866,-7.35067909432449));
#68836=CARTESIAN_POINT('Ctrl Pts',(37.0428998635996,2.90991775569873,-7.28225858062534));
#68837=CARTESIAN_POINT('Ctrl Pts',(37.1149926712673,2.91625037660879,-7.21712758324237));
#68838=CARTESIAN_POINT('Ctrl Pts',(37.1869884533318,2.9225744748051,-7.15208424195867));
#68839=CARTESIAN_POINT('Ctrl Pts',(37.2621316323609,2.92889857300141,-7.09032190846517));
#68840=CARTESIAN_POINT('Ctrl Pts',(37.3400896756765,2.93522267119771,-7.03215739799427));
#68841=CARTESIAN_POINT('Ctrl Pts',(37.4179661199614,2.94154014993231,-6.97405376857516));
#68842=CARTESIAN_POINT('Ctrl Pts',(37.4986512224208,2.94785762866692,-6.91954073561128));
#68843=CARTESIAN_POINT('Ctrl Pts',(37.5817781876478,2.95417510740152,-6.86889593221058));
#68844=CARTESIAN_POINT('Ctrl Pts',(37.6648461461997,2.96048810174993,-6.81828707841358));
#68845=CARTESIAN_POINT('Ctrl Pts',(37.7503521491603,2.96680109609834,-6.77154122221721));
#68846=CARTESIAN_POINT('Ctrl Pts',(37.8378999269094,2.97311409044675,-6.7288930557315));
#68847=CARTESIAN_POINT('Ctrl Pts',(37.9254160672524,2.97942480344924,-6.68626030114313));
#68848=CARTESIAN_POINT('Ctrl Pts',(38.0149721235363,2.98573551645172,-6.64772248523414));
#68849=CARTESIAN_POINT('Ctrl Pts',(38.1061475358688,2.99204622945421,-6.61346819704573));
#68850=CARTESIAN_POINT('Ctrl Pts',(38.1973146948333,2.99835637119921,-6.57921700961925));
#68851=CARTESIAN_POINT('Ctrl Pts',(38.2901005089509,3.00466651294421,-6.54924873257616));
#68852=CARTESIAN_POINT('Ctrl Pts',(38.3840657511376,3.0109766546892,-6.52370328783818));
#68853=CARTESIAN_POINT('Ctrl Pts',(38.4780479376236,3.01728793431165,-6.49815323661327));
#68854=CARTESIAN_POINT('Ctrl Pts',(38.5732095525892,3.02359921393409,-6.47702771641294));
#68855=CARTESIAN_POINT('Ctrl Pts',(38.6690985951302,3.02991049355653,-6.4604161210358));
#68856=CARTESIAN_POINT('Ctrl Pts',(38.7650901840176,3.03622852263282,-6.44378676076741));
#68857=CARTESIAN_POINT('Ctrl Pts',(38.861810321972,3.0425465517091,-6.43168103756005));
#68858=CARTESIAN_POINT('Ctrl Pts',(38.9587994574682,3.04886458078539,-6.42413674097319));
#68859=CARTESIAN_POINT('Ctrl Pts',(39.0558454251575,3.05518631200261,-6.41658802369614));
#68860=CARTESIAN_POINT('Ctrl Pts',(39.1531602673442,3.06150804321983,-6.41360606877045));
#68861=CARTESIAN_POINT('Ctrl Pts',(39.250284088696,3.06782977443705,-6.41517650608206));
#68862=CARTESIAN_POINT('Ctrl Pts',(39.3475636404491,3.07416164205258,-6.41674946146625));
#68863=CARTESIAN_POINT('Ctrl Pts',(39.4446511236004,3.08049350966811,-6.42288935713051));
#68864=CARTESIAN_POINT('Ctrl Pts',(39.5410914598249,3.08682537728365,-6.43352991783286));
#68865=CARTESIAN_POINT('Ctrl Pts',(39.597105489185,3.09050302330196,-6.43971011901137));
#68866=CARTESIAN_POINT('Ctrl Pts',(39.6529013713708,3.09418066932027,-6.44740764080296));
#68867=CARTESIAN_POINT('Ctrl Pts',(39.7083918981512,3.09785831533858,-6.4566016668636));
#68868=CARTESIAN_POINT('Ctrl Pts',(39.8039423757478,3.10419094279536,-6.47243308227991));
#68869=CARTESIAN_POINT('Ctrl Pts',(39.8989186247315,3.11052357025214,-6.49275943423228));
#68870=CARTESIAN_POINT('Ctrl Pts',(39.992865506002,3.11685619770893,-6.5175268176936));
#68871=CARTESIAN_POINT('Ctrl Pts',(40.0866859504796,3.12318030250806,-6.54226086839825));
#68872=CARTESIAN_POINT('Ctrl Pts',(40.1794793614124,3.12950440730719,-6.57142396073292));
#68873=CARTESIAN_POINT('Ctrl Pts',(40.2707986742641,3.13582851210632,-6.60491081435956));
#68874=CARTESIAN_POINT('Ctrl Pts',(40.3620224035563,3.14214599749026,-6.63836261743045));
#68875=CARTESIAN_POINT('Ctrl Pts',(40.4517746937712,3.14846348287419,-6.67612903478748));
#68876=CARTESIAN_POINT('Ctrl Pts',(40.5396225621817,3.15478096825812,-6.71805467744851));
#68877=CARTESIAN_POINT('Ctrl Pts',(40.6274080734803,3.16109396929713,-6.75995056000221));
#68878=CARTESIAN_POINT('Ctrl Pts',(40.7132914569184,3.16740697033614,-6.80599961059708));
#68879=CARTESIAN_POINT('Ctrl Pts',(40.7968595766655,3.17371997137514,-6.85599828675372));
#68880=CARTESIAN_POINT('Ctrl Pts',(40.8803974974827,3.18003069109112,-6.9059788949375));
#68881=CARTESIAN_POINT('Ctrl Pts',(40.9616214421778,3.1863414108071,-6.95990606837964));
#68882=CARTESIAN_POINT('Ctrl Pts',(41.0401436033027,3.19265213052307,-7.0175307235932));
#68883=CARTESIAN_POINT('Ctrl Pts',(41.1186586566432,3.19896227899604,-7.07515016265347));
#68884=CARTESIAN_POINT('Ctrl Pts',(41.1944720602269,3.205272427469,-7.13646615913693));
#68885=CARTESIAN_POINT('Ctrl Pts',(41.2672265557435,3.21158257594197,-7.20118739565153));
#68886=CARTESIAN_POINT('Ctrl Pts',(41.3399941707842,3.21789386229851,-7.26592030308511));
#68887=CARTESIAN_POINT('Ctrl Pts',(41.4097014554993,3.22420514865504,-7.33405937945335));
#68888=CARTESIAN_POINT('Ctrl Pts',(41.4760264805007,3.23051643501158,-7.40527499119348));
#68889=CARTESIAN_POINT('Ctrl Pts',(41.5424224348733,3.23683447078997,-7.4765667624008));
#68890=CARTESIAN_POINT('Ctrl Pts',(41.6054286097377,3.24315250656836,-7.55094131696089));
#68891=CARTESIAN_POINT('Ctrl Pts',(41.6647621608396,3.24947054234675,-7.62803449072118));
#68892=CARTESIAN_POINT('Ctrl Pts',(41.724130479183,3.25579228025778,-7.7051728381976));
#68893=CARTESIAN_POINT('Ctrl Pts',(41.7798216384679,3.2621140181688,-7.78503261844524));
#68894=CARTESIAN_POINT('Ctrl Pts',(41.8315962840512,3.26843575607983,-7.8672208679477));
#68895=CARTESIAN_POINT('Ctrl Pts',(41.8834539454656,3.27476763030993,-7.94954089866794));
#68896=CARTESIAN_POINT('Ctrl Pts',(41.9313823382706,3.28109950454002,-8.03419647344177));
#68897=CARTESIAN_POINT('Ctrl Pts',(41.9751882052804,3.28743137877011,-8.1207702900976));
#68898=CARTESIAN_POINT('Ctrl Pts',(42.0006308381811,3.29110895811293,-8.17105272910263));
#68899=CARTESIAN_POINT('Ctrl Pts',(42.0246837016427,3.29478653745574,-8.22198186775086));
#68900=CARTESIAN_POINT('Ctrl Pts',(42.0473165588172,3.29846411679856,-8.2734733056041));
#68901=CARTESIAN_POINT('Ctrl Pts',(42.0862891694655,3.30479671841183,-8.36213890110126));
#68902=CARTESIAN_POINT('Ctrl Pts',(42.1211839554828,3.31112932002509,-8.45278065774558));
#68903=CARTESIAN_POINT('Ctrl Pts',(42.1517972678665,3.31746192163836,-8.54498798868783));
#68904=CARTESIAN_POINT('Ctrl Pts',(42.1823693794774,3.32378600055154,-8.63707122285675));
#68905=CARTESIAN_POINT('Ctrl Pts',(42.2086713334622,3.33011007946473,-8.7307154319889));
#68906=CARTESIAN_POINT('Ctrl Pts',(42.2305469151543,3.33643415837791,-8.82548870777606));
#68907=CARTESIAN_POINT('Ctrl Pts',(42.2523995996431,3.34275161786848,-8.92016278423733));
#68908=CARTESIAN_POINT('Ctrl Pts',(42.269835024806,3.34906907735905,-9.01596315401371));
#68909=CARTESIAN_POINT('Ctrl Pts',(42.2827466333479,3.35538653684961,-9.11244231011624));
#68910=CARTESIAN_POINT('Ctrl Pts',(42.2956490769913,3.36169951209061,-9.20885298352962));
#68911=CARTESIAN_POINT('Ctrl Pts',(42.3040340300051,3.36801248733161,-9.30594105316998));
#68912=CARTESIAN_POINT('Ctrl Pts',(42.3078461066003,3.3743254625726,-9.40324930969573));
#68913=CARTESIAN_POINT('Ctrl Pts',(42.3116568056648,3.38063615655918,-9.50052240294554));
#68914=CARTESIAN_POINT('Ctrl Pts',(42.3108978946503,3.38694685054575,-9.59801508844345));
#68915=CARTESIAN_POINT('Ctrl Pts',(42.3055659679321,3.39325754453233,-9.6952664726896));
#68916=CARTESIAN_POINT('Ctrl Pts',(42.3002345237747,3.39956766737561,-9.79250905529271));
#68917=CARTESIAN_POINT('Ctrl Pts',(42.2903309109435,3.40587779021889,-9.88950994341774));
#68918=CARTESIAN_POINT('Ctrl Pts',(42.2759037884449,3.41218791306218,-9.98581073894882));
#68919=CARTESIAN_POINT('Ctrl Pts',(42.2614740640517,3.41849917391991,-10.0821289020811));
#68920=CARTESIAN_POINT('Ctrl Pts',(42.2425192745294,3.42481043477765,-10.177746289373));
#68921=CARTESIAN_POINT('Ctrl Pts',(42.2191394755936,3.43112169563538,-10.2722131421572));
#68922=CARTESIAN_POINT('Ctrl Pts',(42.1957346723996,3.43743970626871,-10.3667810254758));
#68923=CARTESIAN_POINT('Ctrl Pts',(42.1678955169209,3.44375771690205,-10.4601954925031));
#68924=CARTESIAN_POINT('Ctrl Pts',(42.1357723448205,3.45007572753538,-10.5520206386862));
#68925=CARTESIAN_POINT('Ctrl Pts',(42.1036303488395,3.45639744046426,-10.6438995935521));
#68926=CARTESIAN_POINT('Ctrl Pts',(42.0671995009236,3.46271915339315,-10.7341869676802));
#68927=CARTESIAN_POINT('Ctrl Pts',(42.0266780249898,3.46904086632204,-10.8224675317479));
#68928=CARTESIAN_POINT('Ctrl Pts',(41.9860915731618,3.47537271607198,-10.9108896530629));
#68929=CARTESIAN_POINT('Ctrl Pts',(41.9414015963321,3.48170456582192,-10.9972981505316));
#68930=CARTESIAN_POINT('Ctrl Pts',(41.8928518968493,3.48803641557186,-11.0813030921177));
#68931=CARTESIAN_POINT('Ctrl Pts',(41.8646519626102,3.49171424980076,-11.1300970878319));
#68932=CARTESIAN_POINT('Ctrl Pts',(41.8351506388072,3.49539208402966,-11.1780807039365));
#68933=CARTESIAN_POINT('Ctrl Pts',(41.8044020846547,3.49906991825855,-11.2251824708973));
#68934=CARTESIAN_POINT('Ctrl Pts',(41.7514580799431,3.50540255008824,-11.3062840459346));
#68935=CARTESIAN_POINT('Ctrl Pts',(41.6946302290773,3.51173518191792,-11.3850511066296));
#68936=CARTESIAN_POINT('Ctrl Pts',(41.6341510345655,3.51806781374761,-11.4610886843902));
#68937=CARTESIAN_POINT('Ctrl Pts',(41.5737532364699,3.5243919227532,-11.5370239263577));
#68938=CARTESIAN_POINT('Ctrl Pts',(41.5097141318353,3.53071603175879,-11.6102366472761));
#68939=CARTESIAN_POINT('Ctrl Pts',(41.4423100057695,3.53704014076438,-11.6803599446325));
#68940=CARTESIAN_POINT('Ctrl Pts',(41.3749764330928,3.54335763018524,-11.750409842383));
#68941=CARTESIAN_POINT('Ctrl Pts',(41.3042851428335,3.54967511960611,-11.8173764318364));
#68942=CARTESIAN_POINT('Ctrl Pts',(41.2305526257222,3.55599260902697,-11.880925866209));
#68943=CARTESIAN_POINT('Ctrl Pts',(41.1568724492895,3.56230561383648,-11.9444301885924));
#68944=CARTESIAN_POINT('Ctrl Pts',(41.0801556683079,3.56861861864599,-12.0045218937258));
#68945=CARTESIAN_POINT('Ctrl Pts',(41.0007548693125,3.5749316234555,-12.060904681479));
#68946=CARTESIAN_POINT('Ctrl Pts',(40.9213827653735,3.58124234677628,-12.1172670927714));
#68947=CARTESIAN_POINT('Ctrl Pts',(40.8393289270005,3.58755307009705,-12.1699229971051));
#68948=CARTESIAN_POINT('Ctrl Pts',(40.7549774391038,3.59386379341783,-12.2186176077495));
#68949=CARTESIAN_POINT('Ctrl Pts',(40.6706335889134,3.6001739453266,-12.2673078092821));
#68950=CARTESIAN_POINT('Ctrl Pts',(40.5839928816742,3.60648409723538,-12.3120372118093));
#68951=CARTESIAN_POINT('Ctrl Pts',(40.4954657722599,3.61279424914416,-12.3525959905551));
#68952=CARTESIAN_POINT('Ctrl Pts',(40.4069227015372,3.6191055387641,-12.3931620819893));
#68953=CARTESIAN_POINT('Ctrl Pts',(40.3164929507085,3.62541682838404,-12.4295558740468));
#68954=CARTESIAN_POINT('Ctrl Pts',(40.2246078346454,3.63172811800398,-12.4616153030459));
#68955=CARTESIAN_POINT('Ctrl Pts',(40.1326244588472,3.6380461567654,-12.4937090156279));
#68956=CARTESIAN_POINT('Ctrl Pts',(40.0391830242623,3.64436419552681,-12.5214589671988));
#68957=CARTESIAN_POINT('Ctrl Pts',(39.9447307286541,3.65068223428822,-12.5447527704596));
#68958=CARTESIAN_POINT('Ctrl Pts',(39.8502230898586,3.6570039750285,-12.5680602224444));
#68959=CARTESIAN_POINT('Ctrl Pts',(39.7547038394558,3.66332571576878,-12.5869062422387));
#68960=CARTESIAN_POINT('Ctrl Pts',(39.6586290390159,3.66964745650906,-12.6012298447079));
#68961=CARTESIAN_POINT('Ctrl Pts',(39.5624001957111,3.67597933330011,-12.6155764131239));
#68962=CARTESIAN_POINT('Ctrl Pts',(39.4656144585077,3.68231121009117,-12.6253860410088));
#68963=CARTESIAN_POINT('Ctrl Pts',(39.3687316197421,3.68864308688222,-12.6306497377198));
#68964=CARTESIAN_POINT('Ctrl Pts',(39.3124622163455,3.69232063116099,-12.6337068846549));
#68965=CARTESIAN_POINT('Ctrl Pts',(39.2561600520151,3.69599817543976,-12.6352315439811));
#68966=CARTESIAN_POINT('Ctrl Pts',(39.199914556952,3.69967571971853,-12.6352299988264));
#68967=CARTESIAN_POINT('Ctrl Pts',(39.1030608108006,3.7060083858216,-12.6352273380973));
#68968=CARTESIAN_POINT('Ctrl Pts',(39.0060389757696,3.71234105192467,-12.6306962713217));
#68969=CARTESIAN_POINT('Ctrl Pts',(38.9093068864271,3.71867371802774,-12.6216155987822));
#68970=CARTESIAN_POINT('Ctrl Pts',(38.8127049775187,3.7249978617343,-12.6125471468605));
#68971=CARTESIAN_POINT('Ctrl Pts',(38.7163924709999,3.73132200544085,-12.5989412990248));
#68972=CARTESIAN_POINT('Ctrl Pts',(38.6208276312334,3.73764614914741,-12.5808288597625));
#68973=CARTESIAN_POINT('Ctrl Pts',(38.5253628150799,3.74396367364438,-12.5627353780124));
#68974=CARTESIAN_POINT('Ctrl Pts',(38.4306445373297,3.75028119814135,-12.540144763181));
#68975=CARTESIAN_POINT('Ctrl Pts',(38.3371253587336,3.75659872263832,-12.5131395560381));
#68976=CARTESIAN_POINT('Ctrl Pts',(38.2436725604007,3.76291176293274,-12.4861535172924));
#68977=CARTESIAN_POINT('Ctrl Pts',(38.1514175880817,3.76922480322716,-12.4547592367898));
#68978=CARTESIAN_POINT('Ctrl Pts',(38.0608012918966,3.77553784352159,-12.4190900048816));
#68979=CARTESIAN_POINT('Ctrl Pts',(37.9702177403851,3.78184860256581,-12.3834336622374));
#68980=CARTESIAN_POINT('Ctrl Pts',(37.8812720949134,3.78815936161003,-12.3435055976874));
#68981=CARTESIAN_POINT('Ctrl Pts',(37.7943876603095,3.79447012065425,-12.2994881696288));
#68982=CARTESIAN_POINT('Ctrl Pts',(37.7075110900579,3.80078030847957,-12.2554747258115));
#68983=CARTESIAN_POINT('Ctrl Pts',(37.6226957497321,3.80709049630489,-12.2073728522452));
#68984=CARTESIAN_POINT('Ctrl Pts',(37.5403417079127,3.8134006841302,-12.1554115659733));
#68985=CARTESIAN_POINT('Ctrl Pts',(37.4579728159357,3.81971200981447,-12.1034409099938));
#68986=CARTESIAN_POINT('Ctrl Pts',(37.3780664737735,3.82602333549874,-12.0476096924764));
#68987=CARTESIAN_POINT('Ctrl Pts',(37.3009941580418,3.832334661183,-11.9881905052409));
#68988=CARTESIAN_POINT('Ctrl Pts',(37.2238394234699,3.83865273601109,-11.9287077768952));
#68989=CARTESIAN_POINT('Ctrl Pts',(37.1495251127038,3.84497081083918,-11.8656296861786));
#68990=CARTESIAN_POINT('Ctrl Pts',(37.0783897860474,3.85128888566726,-11.7992692789008));
#68991=CARTESIAN_POINT('Ctrl Pts',(37.0072127781336,3.857610662528,-11.732869988197));
#68992=CARTESIAN_POINT('Ctrl Pts',(36.9392187687496,3.86393243938874,-11.6631848640705));
#68993=CARTESIAN_POINT('Ctrl Pts',(36.8747081200652,3.87025421624949,-11.5905624720664));
#68994=CARTESIAN_POINT('Ctrl Pts',(36.8100940407202,3.87658612888733,-11.517823643751));
#68995=CARTESIAN_POINT('Ctrl Pts',(36.7489747487376,3.88291804152518,-11.4421384838086));
#68996=CARTESIAN_POINT('Ctrl Pts',(36.691609106351,3.88924995416303,-11.3638871029943));
#68997=CARTESIAN_POINT('Ctrl Pts',(36.6582946370077,3.89292714316819,-11.31844346951));
#68998=CARTESIAN_POINT('Ctrl Pts',(36.6262452941534,3.89660433217334,-11.2721348868709));
#68999=CARTESIAN_POINT('Ctrl Pts',(36.5955046880318,3.9002815211785,-11.2250396533127));
#69000=CARTESIAN_POINT('Ctrl Pts',(36.5415325528662,3.90673766395039,-11.1423532449447));
#69001=CARTESIAN_POINT('Ctrl Pts',(36.4914152766448,3.91319380672228,-11.0569619124821));
#69002=CARTESIAN_POINT('Ctrl Pts',(36.4454280277222,3.91964994949417,-10.9692520217889));
#69003=CARTESIAN_POINT('Ctrl Pts',(36.3995096965043,3.92609641692012,-10.8816735754525));
#69004=CARTESIAN_POINT('Ctrl Pts',(36.3577092741141,3.93254288434608,-10.7917838452957));
#69005=CARTESIAN_POINT('Ctrl Pts',(36.3202585619524,3.93898935177203,-10.6999978310158));
#69006=CARTESIAN_POINT('Ctrl Pts',(36.2824093203582,3.9455044188816,-10.6072350815531));
#69007=CARTESIAN_POINT('Ctrl Pts',(36.2490031659417,3.95201948599117,-10.5125357975657));
#69008=CARTESIAN_POINT('Ctrl Pts',(36.2202319394877,3.95853455310074,-10.4163545638243));
#69009=CARTESIAN_POINT('Ctrl Pts',(36.1918352140922,3.96496481675109,-10.3214252744139));
#69010=CARTESIAN_POINT('Ctrl Pts',(36.1679536071212,3.97139508040143,-10.2250527921383));
#69011=CARTESIAN_POINT('Ctrl Pts',(36.1487230800705,3.97782534405178,-10.1276937952272));
#69012=CARTESIAN_POINT('Ctrl Pts',(36.1291121296098,3.98438281289096,-10.0284088166985));
#69013=CARTESIAN_POINT('Ctrl Pts',(36.1143383994277,3.99094028173014,-9.92809828583084));
#69014=CARTESIAN_POINT('Ctrl Pts',(36.1044921442325,3.99749775056932,-9.82726109207431));
#69015=CARTESIAN_POINT('Ctrl Pts',(36.0946458890374,4.0040552194085,-9.72642389831778));
#69016=CARTESIAN_POINT('Ctrl Pts',(36.0897271825286,4.01061268824768,-9.62506049549556));
#69017=CARTESIAN_POINT('Ctrl Pts',(36.0897702810343,4.01717015708686,-9.5236778189534));
#69018=CARTESIAN_POINT('Ctrl Pts',(36.0897702810346,4.01717015712308,-9.52367781839343));
#69019=CARTESIAN_POINT('Ctrl Pts',(36.0898161331557,4.0241465875827,-9.41581772632917));
#69020=CARTESIAN_POINT('Ctrl Pts',(36.0954771164379,4.03112301804231,-9.30813600171421));
#69021=CARTESIAN_POINT('Ctrl Pts',(36.1066715293551,4.03809944850193,-9.20119508095537));
#69022=CARTESIAN_POINT('Ctrl Pts',(36.1177674248493,4.045014482267,-9.09519530324727));
#69023=CARTESIAN_POINT('Ctrl Pts',(36.1342995664637,4.05192951603208,-8.98992360536198));
#69024=CARTESIAN_POINT('Ctrl Pts',(36.15613770959,4.05884454979716,-8.88591236131493));
#69025=CARTESIAN_POINT('Ctrl Pts',(36.1782666950712,4.06585167860405,-8.78051588616198));
#69026=CARTESIAN_POINT('Ctrl Pts',(36.2058439016662,4.07285880741093,-8.67641397761243));
#69027=CARTESIAN_POINT('Ctrl Pts',(36.2386833095558,4.07986593621782,-8.57414033012391));
#69028=CARTESIAN_POINT('Ctrl Pts',(36.2715227174455,4.08687306502472,-8.47186668263539));
#69029=CARTESIAN_POINT('Ctrl Pts',(36.3096241442889,4.09388019383161,-8.37142155394688));
#69030=CARTESIAN_POINT('Ctrl Pts',(36.3527533462547,4.10088732263849,-8.27331427840847));
#69031=CARTESIAN_POINT('Ctrl Pts',(36.3917317158068,4.10722007269381,-8.18464902453411));
#69032=CARTESIAN_POINT('Ctrl Pts',(36.4349233715946,4.11355282274913,-8.09765223533168));
#69033=CARTESIAN_POINT('Ctrl Pts',(36.4821634778366,4.11988557280445,-8.01275157738719));
#69034=CARTESIAN_POINT('Ctrl Pts',(36.5293400015044,4.12620979932791,-7.92796519103984));
#69035=CARTESIAN_POINT('Ctrl Pts',(36.5805539346683,4.13253402585137,-7.84526970742359));
#69036=CARTESIAN_POINT('Ctrl Pts',(36.6355926609841,4.13885825237482,-7.7650722592954));
#69037=CARTESIAN_POINT('Ctrl Pts',(36.6905737706915,4.14517585846012,-7.68495876487191));
#69038=CARTESIAN_POINT('Ctrl Pts',(36.7493714673799,4.15149346454541,-7.60733846576996));
#69039=CARTESIAN_POINT('Ctrl Pts',(36.8117280675142,4.15781107063071,-7.53259245398925));
#69040=CARTESIAN_POINT('Ctrl Pts',(36.8740403860956,4.164124190368,-7.4578995219062));
#69041=CARTESIAN_POINT('Ctrl Pts',(36.9399063043555,4.17043731010529,-7.38607715408355));
#69042=CARTESIAN_POINT('Ctrl Pts',(37.0090263921805,4.17675042984257,-7.31747529963123));
#69043=CARTESIAN_POINT('Ctrl Pts',(37.0781214885987,4.18306126697653,-7.24889824921049));
#69044=CARTESIAN_POINT('Ctrl Pts',(37.150468106614,4.18937210411049,-7.1835397061674));
#69045=CARTESIAN_POINT('Ctrl Pts',(37.2257289566207,4.19568294124446,-7.12171381226167));
#69046=CARTESIAN_POINT('Ctrl Pts',(37.3009829773001,4.20199320571983,-7.05989352856711));
#69047=CARTESIAN_POINT('Ctrl Pts',(37.379150366166,4.20830347019521,-7.00160553407963));
#69048=CARTESIAN_POINT('Ctrl Pts',(37.4598604697883,4.21461373467058,-6.94712392301442));
#69049=CARTESIAN_POINT('Ctrl Pts',(37.5405851074183,4.22092513547745,-6.89263250108144));
#69050=CARTESIAN_POINT('Ctrl Pts',(37.6238530067577,4.22723653628432,-6.84194906857085));
#69051=CARTESIAN_POINT('Ctrl Pts',(37.709265128746,4.23354793709118,-6.79530401023717));
#69052=CARTESIAN_POINT('Ctrl Pts',(37.7947685493868,4.23986608427522,-6.74860909210754));
#69053=CARTESIAN_POINT('Ctrl Pts',(37.8824203841084,4.24618423145925,-6.7059613761455));
#69054=CARTESIAN_POINT('Ctrl Pts',(37.9717978053915,4.25250237864328,-6.66754483463716));
#69055=CARTESIAN_POINT('Ctrl Pts',(38.0612275755798,4.25882422640497,-6.62910579232423));
#69056=CARTESIAN_POINT('Ctrl Pts',(38.1523845356437,4.26514607416666,-6.5949030128498));
#69057=CARTESIAN_POINT('Ctrl Pts',(38.2448287117249,4.27146792192835,-6.56507120643841));
#69058=CARTESIAN_POINT('Ctrl Pts',(38.3374210594344,4.27779990249144,-6.53519158492911));
#69059=CARTESIAN_POINT('Ctrl Pts',(38.4313043212246,4.28413188305452,-6.50969704056112));
#69060=CARTESIAN_POINT('Ctrl Pts',(38.5260263442078,4.29046386361761,-6.48867159809778));
#69061=CARTESIAN_POINT('Ctrl Pts',(38.5810230314921,4.2941402837779,-6.4764639863117));
#69062=CARTESIAN_POINT('Ctrl Pts',(38.636302319507,4.29781670393818,-6.46576198716194));
#69063=CARTESIAN_POINT('Ctrl Pts',(38.691775037217,4.30149312409847,-6.45657401260773));
#69064=CARTESIAN_POINT('Ctrl Pts',(38.787330651996,4.30782601354583,-6.44074708734889));
#69065=CARTESIAN_POINT('Ctrl Pts',(38.8837921438038,4.31415890299318,-6.42936056874551));
#69066=CARTESIAN_POINT('Ctrl Pts',(38.9807112641447,4.32049179244054,-6.42251017677302));
#69067=CARTESIAN_POINT('Ctrl Pts',(39.0774999881135,4.32681616152776,-6.41566900141597));
#69068=CARTESIAN_POINT('Ctrl Pts',(39.1747446843783,4.33314053061498,-6.41335185329256));
#69069=CARTESIAN_POINT('Ctrl Pts',(39.2719881846059,4.33946489970221,-6.41560321699254));
#69070=CARTESIAN_POINT('Ctrl Pts',(39.3691299341042,4.3457826512863,-6.41785222497828));
#69071=CARTESIAN_POINT('Ctrl Pts',(39.466270055195,4.3521004028704,-6.4246602313055));
#69072=CARTESIAN_POINT('Ctrl Pts',(39.5629485540092,4.3584181544545,-6.43601974754732));
#69073=CARTESIAN_POINT('Ctrl Pts',(39.659558456741,4.36473142341822,-6.44737120389659));
#69074=CARTESIAN_POINT('Ctrl Pts',(39.7557069553029,4.37104469238195,-6.4632676989785));
#69075=CARTESIAN_POINT('Ctrl Pts',(39.8509373172772,4.37735796134568,-6.48364976336563));
#69076=CARTESIAN_POINT('Ctrl Pts',(39.9461332819041,4.38366894994734,-6.504024465721));
#69077=CARTESIAN_POINT('Ctrl Pts',(40.0404113417497,4.389979938549,-6.52888142660613));
#69078=CARTESIAN_POINT('Ctrl Pts',(40.1333240564461,4.39629092715066,-6.55810990116603));
#69079=CARTESIAN_POINT('Ctrl Pts',(40.2262283702829,4.40260134513366,-6.58733573298422));
#69080=CARTESIAN_POINT('Ctrl Pts',(40.3177671673656,4.40891176311666,-6.6209321611959));
#69081=CARTESIAN_POINT('Ctrl Pts',(40.4075083070617,4.41522218109967,-6.65873861253428));
#69082=CARTESIAN_POINT('Ctrl Pts',(40.4972656328219,4.42153373725442,-6.69655188279255));
#69083=CARTESIAN_POINT('Ctrl Pts',(40.5852242542767,4.42784529340916,-6.73857651452453));
#69084=CARTESIAN_POINT('Ctrl Pts',(40.6709731177269,4.43415684956391,-6.78460427313412));
#69085=CARTESIAN_POINT('Ctrl Pts',(40.7568136623554,4.44047515392361,-6.83068124381455));
#69086=CARTESIAN_POINT('Ctrl Pts',(40.8404393461987,4.44679345828331,-6.88076967916138));
#69087=CARTESIAN_POINT('Ctrl Pts',(40.9214649784174,4.45311176264302,-6.93461605529556));
#69088=CARTESIAN_POINT('Ctrl Pts',(41.0025380828147,4.4594337688396,-6.98849397953026));
#69089=CARTESIAN_POINT('Ctrl Pts',(41.0810077499224,4.46575577503618,-7.04613397008788));
#69090=CARTESIAN_POINT('Ctrl Pts',(41.1565206683713,4.47207778123276,-7.10724121816591));
#69091=CARTESIAN_POINT('Ctrl Pts',(41.2321546223702,4.47840992062922,-7.16844641172832));
#69092=CARTESIAN_POINT('Ctrl Pts',(41.3048220379171,4.48474206002569,-7.2331296695793));
#69093=CARTESIAN_POINT('Ctrl Pts',(41.3742053900307,4.49107419942216,-7.30095827942425));
#69094=CARTESIAN_POINT('Ctrl Pts',(41.4144725839746,4.49474910813426,-7.34032316601978));
#69095=CARTESIAN_POINT('Ctrl Pts',(41.4536343775838,4.49842401684636,-7.38074680055014));
#69096=CARTESIAN_POINT('Ctrl Pts',(41.4916350544945,4.50209892555846,-7.42215920005528));
#69097=CARTESIAN_POINT('Ctrl Pts',(41.5571069112291,4.50843047321161,-7.49350915768401));
#69098=CARTESIAN_POINT('Ctrl Pts',(41.6193573245284,4.51476202086475,-7.56804390007884));
#69099=CARTESIAN_POINT('Ctrl Pts',(41.67806115532,4.5210935685179,-7.64544059327879));
#69100=CARTESIAN_POINT('Ctrl Pts',(41.7366859502706,4.5274165916985,-7.72273308352204));
#69101=CARTESIAN_POINT('Ctrl Pts',(41.7917733909051,4.53373961487911,-7.8028795206477));
#69102=CARTESIAN_POINT('Ctrl Pts',(41.8430363558471,4.54006263805971,-7.8855215845976));
#69103=CARTESIAN_POINT('Ctrl Pts',(41.8942456519932,4.54637904147026,-7.96807712799477));
#69104=CARTESIAN_POINT('Ctrl Pts',(41.9416382030586,4.5526954448808,-8.05312273418323));
#69105=CARTESIAN_POINT('Ctrl Pts',(41.984968857296,4.55901184829135,-8.14026929809751));
#69106=CARTESIAN_POINT('Ctrl Pts',(42.0282687756684,4.56532377126821,-8.22735404607401));
#69107=CARTESIAN_POINT('Ctrl Pts',(42.0675123309939,4.57163569424508,-8.31653639843586));
#69108=CARTESIAN_POINT('Ctrl Pts',(42.1024996774301,4.57794761722194,-8.40740155895853));
#69109=CARTESIAN_POINT('Ctrl Pts',(42.137474393984,4.58425726169381,-8.49823391858623));
#69110=CARTESIAN_POINT('Ctrl Pts',(42.1681957974673,4.59056690616567,-8.59074747149895));
#69111=CARTESIAN_POINT('Ctrl Pts',(42.1945120558889,4.59687655063754,-8.68450716836111));
#69112=CARTESIAN_POINT('Ctrl Pts',(42.2208259489294,4.60318562798039,-8.77825843783179));
#69113=CARTESIAN_POINT('Ctrl Pts',(42.2427353661126,4.60949470532325,-8.87325520730227));
#69114=CARTESIAN_POINT('Ctrl Pts',(42.2601385630211,4.6158037826661,-8.96904799846442));
#69115=CARTESIAN_POINT('Ctrl Pts',(42.2775449136437,4.6221140033062,-9.06485814868369));
#69116=CARTESIAN_POINT('Ctrl Pts',(42.2904433439776,4.6284242239463,-9.16146417666143));
#69117=CARTESIAN_POINT('Ctrl Pts',(42.2987835467469,4.6347344445864,-9.25840820847109));
#69118=CARTESIAN_POINT('Ctrl Pts',(42.3071326896345,4.64105142934484,-9.35545615755111));
#69119=CARTESIAN_POINT('Ctrl Pts',(42.3109138125849,4.64736841410328,-9.45284239722024));
#69120=CARTESIAN_POINT('Ctrl Pts',(42.3101286699969,4.65368539886173,-9.55010595474015));
#69121=CARTESIAN_POINT('Ctrl Pts',(42.3093430664287,4.66000609250672,-9.64742661854001));
#69122=CARTESIAN_POINT('Ctrl Pts',(42.30398588289,4.66632678615171,-9.74462402014482));
#69123=CARTESIAN_POINT('Ctrl Pts',(42.2941108707343,4.67264747979671,-9.84124132004542));
#69124=CARTESIAN_POINT('Ctrl Pts',(42.2842199896438,4.67897833066205,-9.93801388189351));
#69125=CARTESIAN_POINT('Ctrl Pts',(42.2697968477625,4.68530918152739,-10.0342040482199));
#69126=CARTESIAN_POINT('Ctrl Pts',(42.2509464970116,4.69164003239273,-10.1293642322908));
#69127=CARTESIAN_POINT('Ctrl Pts',(42.2399646464367,4.69532826393463,-10.184802719137));
#69128=CARTESIAN_POINT('Ctrl Pts',(42.2274811480986,4.69901649547654,-10.2398918777559));
#69129=CARTESIAN_POINT('Ctrl Pts',(42.2135244854079,4.70270472701844,-10.2945458587682));
#69130=CARTESIAN_POINT('Ctrl Pts',(42.1895563876361,4.70903861185608,-10.3884043971266));
#69131=CARTESIAN_POINT('Ctrl Pts',(42.1611576037167,4.71537249669373,-10.4813048909988));
#69132=CARTESIAN_POINT('Ctrl Pts',(42.1284209443368,4.72170638153138,-10.5727983707133));
#69133=CARTESIAN_POINT('Ctrl Pts',(42.0957283609005,4.72803173856088,-10.6641686655481));
#69134=CARTESIAN_POINT('Ctrl Pts',(42.0587096562478,4.73435709559038,-10.7541353033115));
#69135=CARTESIAN_POINT('Ctrl Pts',(42.0175081333417,4.74068245261988,-10.8422617702846));
#69136=CARTESIAN_POINT('Ctrl Pts',(41.9763497712833,4.74700118349209,-10.9302959199659));
#69137=CARTESIAN_POINT('Ctrl Pts',(41.9310174863046,4.7533199143643,-11.0164933373018));
#69138=CARTESIAN_POINT('Ctrl Pts',(41.8817032966851,4.75963864523652,-11.1004358385692));
#69139=CARTESIAN_POINT('Ctrl Pts',(41.8324242224,4.76595287670706,-11.1843185665945));
#69140=CARTESIAN_POINT('Ctrl Pts',(41.7791691013338,4.7722671081776,-11.2659491949411));
#69141=CARTESIAN_POINT('Ctrl Pts',(41.7221762247401,4.77858133964815,-11.3449334450072));
#69142=CARTESIAN_POINT('Ctrl Pts',(41.6652040276702,4.78489328003764,-11.4238890361114));
#69143=CARTESIAN_POINT('Ctrl Pts',(41.6044970254573,4.79120522042714,-11.5001998028149));
#69144=CARTESIAN_POINT('Ctrl Pts',(41.5403367113354,4.79751716081663,-11.573500605437));
#69145=CARTESIAN_POINT('Ctrl Pts',(41.4761823176237,4.80382851877014,-11.6467946442079));
#69146=CARTESIAN_POINT('Ctrl Pts',(41.4085755336306,4.81013987672365,-11.7170789423427));
#69147=CARTESIAN_POINT('Ctrl Pts',(41.3378373137875,4.81645123467716,-11.7840224152668));
#69148=CARTESIAN_POINT('Ctrl Pts',(41.267086482095,4.82276371787663,-11.8509778234785));
#69149=CARTESIAN_POINT('Ctrl Pts',(41.1932034232146,4.82907620107611,-11.9145909230486));
#69150=CARTESIAN_POINT('Ctrl Pts',(41.1165442418502,4.83538868427558,-11.9745691094417));
#69151=CARTESIAN_POINT('Ctrl Pts',(41.0398034158875,4.8417078904813,-12.0346111746142));
#69152=CARTESIAN_POINT('Ctrl Pts',(40.9602809094415,4.84802709668702,-12.0910103279271));
#69153=CARTESIAN_POINT('Ctrl Pts',(40.8783638840763,4.85434630289274,-12.1435158631424));
#69154=CARTESIAN_POINT('Ctrl Pts',(40.7963990384143,4.86066919803022,-12.1960520492543));
#69155=CARTESIAN_POINT('Ctrl Pts',(40.7120372688379,4.8669920931677,-12.2446898728526));
#69156=CARTESIAN_POINT('Ctrl Pts',(40.6256907113392,4.87331498830518,-12.2892244207917));
#69157=CARTESIAN_POINT('Ctrl Pts',(40.5392061685772,4.87964798768277,-12.3338301367251));
#69158=CARTESIAN_POINT('Ctrl Pts',(40.4507309016318,4.88598098706036,-12.3743193015679));
#69159=CARTESIAN_POINT('Ctrl Pts',(40.3606973525431,4.89231398643795,-12.4105350125582));
#69160=CARTESIAN_POINT('Ctrl Pts',(40.3085863043348,4.89597950045144,-12.4314965172464));
#69161=CARTESIAN_POINT('Ctrl Pts',(40.2559535325021,4.89964501446493,-12.4510273184645));
#69162=CARTESIAN_POINT('Ctrl Pts',(40.2028848447455,4.90331052847842,-12.4691047265815));
#69163=CARTESIAN_POINT('Ctrl Pts',(40.1111819264513,4.90964455229351,-12.500342564742));
#69164=CARTESIAN_POINT('Ctrl Pts',(40.0178595226294,4.9159785761086,-12.5273458107243));
#69165=CARTESIAN_POINT('Ctrl Pts',(39.9233444150091,4.92231259992369,-12.5499468607192));
#69166=CARTESIAN_POINT('Ctrl Pts',(39.828956215711,4.92863811885151,-12.5725175635939));
#69167=CARTESIAN_POINT('Ctrl Pts',(39.7333789172025,4.93496363777933,-12.5906977181596));
#69168=CARTESIAN_POINT('Ctrl Pts',(39.6370564555585,4.94128915670716,-12.6043688164224));
#69169=CARTESIAN_POINT('Ctrl Pts',(39.5408345538429,4.9476080718406,-12.618025642161));
#69170=CARTESIAN_POINT('Ctrl Pts',(39.4438694660887,4.95392698697405,-12.6271827092045));
#69171=CARTESIAN_POINT('Ctrl Pts',(39.3466163926442,4.96024590210749,-12.631772326114));
#69172=CARTESIAN_POINT('Ctrl Pts',(39.2494320730791,4.96656035003066,-12.6363586983552));
#69173=CARTESIAN_POINT('Ctrl Pts',(39.151960607948,4.97287479795382,-12.636384019408));
#69174=CARTESIAN_POINT('Ctrl Pts',(39.0546624609442,4.97918924587698,-12.6318324146373));
#69175=CARTESIAN_POINT('Ctrl Pts',(38.9573993122324,4.98550142248359,-12.6272824470858));
#69176=CARTESIAN_POINT('Ctrl Pts',(38.8603097939336,4.9918135990902,-12.6181588454324));
#69177=CARTESIAN_POINT('Ctrl Pts',(38.763853569696,4.99812577569682,-12.6044978396214));
#69178=CARTESIAN_POINT('Ctrl Pts',(38.6674059501631,5.0044373892043,-12.5908380524869));
#69179=CARTESIAN_POINT('Ctrl Pts',(38.5715919450938,5.01074900271178,-12.5726417274938));
#69180=CARTESIAN_POINT('Ctrl Pts',(38.4768642573544,5.01706061621927,-12.5499967521649));
#69181=CARTESIAN_POINT('Ctrl Pts',(38.3821193973506,5.02337337389799,-12.527347671748));
#69182=CARTESIAN_POINT('Ctrl Pts',(38.2884616708947,5.02968613157671,-12.5002484409021));
#69183=CARTESIAN_POINT('Ctrl Pts',(38.1963307592554,5.03599888925543,-12.4688374119647));
#69184=CARTESIAN_POINT('Ctrl Pts',(38.1041013369121,5.04231839683157,-12.4373927968778));
#69185=CARTESIAN_POINT('Ctrl Pts',(38.0134024030467,5.04863790440772,-12.4016273205991));
#69186=CARTESIAN_POINT('Ctrl Pts',(37.9246555201598,5.05495741198386,-12.3617282405336));
#69187=CARTESIAN_POINT('Ctrl Pts',(37.8358566132894,5.06128062409527,-12.3218057713754));
#69188=CARTESIAN_POINT('Ctrl Pts',(37.7490124256655,5.06760383620668,-12.277745070888));
#69189=CARTESIAN_POINT('Ctrl Pts',(37.6645198138637,5.07392704831809,-12.2297793349704));
#69190=CARTESIAN_POINT('Ctrl Pts',(37.5798919025376,5.08026038590169,-12.1817367906655));
#69191=CARTESIAN_POINT('Ctrl Pts',(37.4976234556511,5.08659372348529,-12.1297769575985));
#69192=CARTESIAN_POINT('Ctrl Pts',(37.4180822176767,5.09292706106889,-12.0741762728262));
#69193=CARTESIAN_POINT('Ctrl Pts',(37.3720769827445,5.09659015069206,-12.0420178273395));
#69194=CARTESIAN_POINT('Ctrl Pts',(37.3269834651792,5.10025324031523,-12.0086421846129));
#69195=CARTESIAN_POINT('Ctrl Pts',(37.282867422968,5.1039163299384,-11.9741086817417));
#69196=CARTESIAN_POINT('Ctrl Pts',(37.2075507939534,5.11017009950536,-11.9151517378737));
#69197=CARTESIAN_POINT('Ctrl Pts',(37.1348090320424,5.11642386907233,-11.852601735732));
#69198=CARTESIAN_POINT('Ctrl Pts',(37.0650108769628,5.12267763863929,-11.7867144155293));
#69199=CARTESIAN_POINT('Ctrl Pts',(36.9953073460977,5.12892293007339,-11.7209164176863));
#69200=CARTESIAN_POINT('Ctrl Pts',(36.9285398189936,5.13516822150749,-11.6517903943124));
#69201=CARTESIAN_POINT('Ctrl Pts',(36.865045801067,5.14141351294159,-11.5796336758131));
#69202=CARTESIAN_POINT('Ctrl Pts',(36.8016225896781,5.14765183982254,-11.5075574242235));
#69203=CARTESIAN_POINT('Ctrl Pts',(36.741465925958,5.15389016670348,-11.4324575313063));
#69204=CARTESIAN_POINT('Ctrl Pts',(36.6848771847878,5.16012849358443,-11.3546687889613));
#69205=CARTESIAN_POINT('Ctrl Pts',(36.6283229200577,5.16636301979234,-11.2769274390632));
#69206=CARTESIAN_POINT('Ctrl Pts',(36.5753325256378,5.17259754600025,-11.1965008544694));
#69207=CARTESIAN_POINT('Ctrl Pts',(36.5261671199786,5.17883207220816,-11.1137568670557));
#69208=CARTESIAN_POINT('Ctrl Pts',(36.4770175409623,5.18506459148419,-11.0310395154344));
#69209=CARTESIAN_POINT('Ctrl Pts',(36.4316907342995,5.19129711076023,-10.9460066287224));
#69210=CARTESIAN_POINT('Ctrl Pts',(36.3904038200082,5.19752963003626,-10.8590539562835));
#69211=CARTESIAN_POINT('Ctrl Pts',(36.3491183334319,5.20376193378974,-10.7721042906964));
#69212=CARTESIAN_POINT('Ctrl Pts',(36.3118726529036,5.20999423754321,-10.6832353778791));
#69213=CARTESIAN_POINT('Ctrl Pts',(36.2788368271283,5.21622654129669,-10.5928653334379));
#69214=CARTESIAN_POINT('Ctrl Pts',(36.2457731565261,5.22246409805704,-10.5024191190146));
#69215=CARTESIAN_POINT('Ctrl Pts',(36.2169265823318,5.22870165481739,-10.4104696687024));
#69216=CARTESIAN_POINT('Ctrl Pts',(36.192417926031,5.23493921157774,-10.3174523463531));
#69217=CARTESIAN_POINT('Ctrl Pts',(36.1678988187396,5.24117942815947,-10.2243953595211));
#69218=CARTESIAN_POINT('Ctrl Pts',(36.1477214069243,5.24741964474119,-10.1302700334956));
#69219=CARTESIAN_POINT('Ctrl Pts',(36.1319553452258,5.25365986132292,-10.0355219380313));
#69220=CARTESIAN_POINT('Ctrl Pts',(36.1161650415883,5.25990967287845,-9.94062815764062));
#69221=CARTESIAN_POINT('Ctrl Pts',(36.1047996883591,5.26615948443398,-9.84511014177736));
#69222=CARTESIAN_POINT('Ctrl Pts',(36.0978770168524,5.27240929598951,-9.7494184714492));
#69223=CARTESIAN_POINT('Ctrl Pts',(36.0924270076094,5.27732958300767,-9.67408332268855));
#69224=CARTESIAN_POINT('Ctrl Pts',(36.0897295006916,5.28224987002584,-9.59864067588427));
#69225=CARTESIAN_POINT('Ctrl Pts',(36.0897704597331,5.287170157044,-9.52330892006468));
#69226=CARTESIAN_POINT('Origin',(39.2,8.05522481984854,-9.525));
#69227=CARTESIAN_POINT('',(37.4444040758239,-12.75,-7.88069592367579));
#69228=CARTESIAN_POINT('Ctrl Pts',(36.9580196848654,-11.5570870138823,-8.65357747851634));
#69229=CARTESIAN_POINT('Ctrl Pts',(36.9542985205578,-11.557947724717,-8.663151223653));
#69230=CARTESIAN_POINT('Ctrl Pts',(36.9506385991756,-11.5588049799687,-8.67274901000278));
#69231=CARTESIAN_POINT('Ctrl Pts',(36.9352241227137,-11.5624633818171,-8.71396307409524));
#69232=CARTESIAN_POINT('Ctrl Pts',(36.9240730287327,-11.5652325766466,-8.7458033405071));
#69233=CARTESIAN_POINT('Ctrl Pts',(36.8979053716304,-11.5720812690608,-8.82588294209961));
#69234=CARTESIAN_POINT('Ctrl Pts',(36.8837311827434,-11.5761258191705,-8.87438192035425));
#69235=CARTESIAN_POINT('Ctrl Pts',(36.8423114898232,-11.5892702188433,-9.03469727488616));
#69236=CARTESIAN_POINT('Ctrl Pts',(36.8215583821953,-11.5982148740058,-9.14802569727867));
#69237=CARTESIAN_POINT('Ctrl Pts',(36.7956053791119,-11.616882243002,-9.38433838841497));
#69238=CARTESIAN_POINT('Ctrl Pts',(36.7915623109317,-11.6265924990067,-9.50709725972053));
#69239=CARTESIAN_POINT('Ctrl Pts',(36.7982888662892,-11.6392030548517,-9.6616087596262));
#69240=CARTESIAN_POINT('Ctrl Pts',(36.8003201963094,-11.6418316248682,-9.69356739931507));
#69241=CARTESIAN_POINT('Ctrl Pts',(36.8047004161722,-11.6461782353672,-9.74594032721957));
#69242=CARTESIAN_POINT('Ctrl Pts',(36.8066740602457,-11.6478845913681,-9.76638271696718));
#69243=CARTESIAN_POINT('Ctrl Pts',(36.8110469375735,-11.6512389786805,-9.80632190538292));
#69244=CARTESIAN_POINT('Ctrl Pts',(36.813423732069,-11.6528861841482,-9.82581957615525));
#69245=CARTESIAN_POINT('Ctrl Pts',(36.8196798901244,-11.6568445914328,-9.87238566856782));
#69246=CARTESIAN_POINT('Ctrl Pts',(36.8237824919044,-11.6591625577661,-9.89942068546272));
#69247=CARTESIAN_POINT('Ctrl Pts',(36.8403323400121,-11.6676229754151,-9.99720995508508));
#69248=CARTESIAN_POINT('Ctrl Pts',(36.8554854622904,-11.6738473742196,-10.0674601710637));
#69249=CARTESIAN_POINT('Ctrl Pts',(36.9045075744349,-11.6907706574786,-10.2538200777191));
#69250=CARTESIAN_POINT('Ctrl Pts',(36.9440231356249,-11.7016071449136,-10.3682238871745));
#69251=CARTESIAN_POINT('Ctrl Pts',(37.0387193834495,-11.7230626201159,-10.5873618517877));
#69252=CARTESIAN_POINT('Ctrl Pts',(37.0933714377716,-11.7336507598302,-10.6919912608123));
#69253=CARTESIAN_POINT('Ctrl Pts',(37.1689967801852,-11.7461543447625,-10.8140062125811));
#69254=CARTESIAN_POINT('Ctrl Pts',(37.1828608603123,-11.7483726700347,-10.835595645731));
#69255=CARTESIAN_POINT('Ctrl Pts',(37.2042927663781,-11.7516887121019,-10.8678238101491));
#69256=CARTESIAN_POINT('Ctrl Pts',(37.2116055136549,-11.7528012424656,-10.8786286560699));
#69257=CARTESIAN_POINT('Ctrl Pts',(37.2251723074942,-11.7548302060971,-10.8983268760363));
#69258=CARTESIAN_POINT('Ctrl Pts',(37.2313990079435,-11.7557482382746,-10.9072377754715));
#69259=CARTESIAN_POINT('Ctrl Pts',(37.2460845102195,-11.7578832488629,-10.927953339875));
#69260=CARTESIAN_POINT('Ctrl Pts',(37.2545901159273,-11.7590970984721,-10.9397240829371));
#69261=CARTESIAN_POINT('Ctrl Pts',(37.2832570807654,-11.7631162780797,-10.9786482515421));
#69262=CARTESIAN_POINT('Ctrl Pts',(37.3038856051206,-11.7658927168098,-11.0054550667182));
#69263=CARTESIAN_POINT('Ctrl Pts',(37.356826811098,-11.7727628157233,-11.0713294528352));
#69264=CARTESIAN_POINT('Ctrl Pts',(37.3898228482146,-11.7768212967455,-11.1098285859429));
#69265=CARTESIAN_POINT('Ctrl Pts',(37.551333793215,-11.7958314022693,-11.2866445501831));
#69266=CARTESIAN_POINT('Ctrl Pts',(37.6946177563593,-11.8103250271822,-11.4105552888389));
#69267=CARTESIAN_POINT('Ctrl Pts',(37.9014668303761,-11.8303116032354,-11.5506831630786));
#69268=CARTESIAN_POINT('Ctrl Pts',(37.9532960784354,-11.8352462138195,-11.582986596297));
#69269=CARTESIAN_POINT('Ctrl Pts',(38.0271003349675,-11.8422149766932,-11.6251746770269));
#69270=CARTESIAN_POINT('Ctrl Pts',(38.0480824477401,-11.8441897623893,-11.6367559441532));
#69271=CARTESIAN_POINT('Ctrl Pts',(38.0865951250313,-11.8478054532929,-11.6572686209035));
#69272=CARTESIAN_POINT('Ctrl Pts',(38.1040691245242,-11.8494426482533,-11.6663022568855));
#69273=CARTESIAN_POINT('Ctrl Pts',(38.139724365488,-11.8527779100226,-11.6841844092006));
#69274=CARTESIAN_POINT('Ctrl Pts',(38.1579102718375,-11.8544762643177,-11.6930199904905));
#69275=CARTESIAN_POINT('Ctrl Pts',(38.2036633044304,-11.8587435547332,-11.7145403418167));
#69276=CARTESIAN_POINT('Ctrl Pts',(38.2313623233122,-11.861322076058,-11.7269342837391));
#69277=CARTESIAN_POINT('Ctrl Pts',(38.3527240647931,-11.8726045705189,-11.77850467994));
#69278=CARTESIAN_POINT('Ctrl Pts',(38.4485660379483,-11.8814821245231,-11.8122474505715));
#69279=CARTESIAN_POINT('Ctrl Pts',(38.6374174237369,-11.8989100996508,-11.8655833436182));
#69280=CARTESIAN_POINT('Ctrl Pts',(38.7300329845701,-11.9074273574035,-11.8859232634944));
#69281=CARTESIAN_POINT('Ctrl Pts',(38.9293821509118,-11.9255604574588,-11.9175069451102));
#69282=CARTESIAN_POINT('Ctrl Pts',(39.0361764765007,-11.9351562801561,-11.9271844909143));
#69283=CARTESIAN_POINT('Ctrl Pts',(39.1690701439768,-11.9467353044458,-11.9303195787957));
#69284=CARTESIAN_POINT('Ctrl Pts',(39.1948794316064,-11.948966857592,-11.930513016968));
#69285=CARTESIAN_POINT('Ctrl Pts',(39.2337790608165,-11.9522997847906,-11.9301784337741));
#69286=CARTESIAN_POINT('Ctrl Pts',(39.2468690871447,-11.9534161388058,-11.9299589677455));
#69287=CARTESIAN_POINT('Ctrl Pts',(39.2708594388396,-11.9554518212718,-11.9293607920759));
#69288=CARTESIAN_POINT('Ctrl Pts',(39.2817594849541,-11.9563727568259,-11.9290148242498));
#69289=CARTESIAN_POINT('Ctrl Pts',(39.3072141849367,-11.958514509633,-11.9280335564926));
#69290=CARTESIAN_POINT('Ctrl Pts',(39.3217659933897,-11.9597321884348,-11.9273401572075));
#69291=CARTESIAN_POINT('Ctrl Pts',(39.370164713456,-11.9637625725864,-11.9245930216666));
#69292=CARTESIAN_POINT('Ctrl Pts',(39.4039764097716,-11.9665463685107,-11.9219557087851));
#69293=CARTESIAN_POINT('Ctrl Pts',(39.4883340751097,-11.9734380490757,-11.9135776308246));
#69294=CARTESIAN_POINT('Ctrl Pts',(39.5387764133877,-11.9775106941544,-11.9069468858319));
#69295=CARTESIAN_POINT('Ctrl Pts',(39.7027259655225,-11.9907012891413,-11.8800809894981));
#69296=CARTESIAN_POINT('Ctrl Pts',(39.8149949525048,-11.9996664520673,-11.8532876252156));
#69297=CARTESIAN_POINT('Ctrl Pts',(40.039942156662,-12.0182052933104,-11.7821892860208));
#69298=CARTESIAN_POINT('Ctrl Pts',(40.1520570783395,-12.0277635842373,-11.7372358215556));
#69299=CARTESIAN_POINT('Ctrl Pts',(40.2890355860524,-12.040209152254,-11.6699657473404));
#69300=CARTESIAN_POINT('Ctrl Pts',(40.3174678003802,-12.0428358696885,-11.6552915496957));
#69301=CARTESIAN_POINT('Ctrl Pts',(40.3636886544239,-12.047183785104,-11.6302565078068));
#69302=CARTESIAN_POINT('Ctrl Pts',(40.3816526497544,-12.0488934035409,-11.6202262905939));
#69303=CARTESIAN_POINT('Ctrl Pts',(40.4165784399783,-12.0522577458837,-11.6001334235476));
#69304=CARTESIAN_POINT('Ctrl Pts',(40.433549542327,-12.0539116748263,-11.5900901441492));
#69305=CARTESIAN_POINT('Ctrl Pts',(40.4739117351212,-12.0578926762898,-11.5655292629567));
#69306=CARTESIAN_POINT('Ctrl Pts',(40.4971802652047,-12.060226624361,-11.5508168738512));
#69307=CARTESIAN_POINT('Ctrl Pts',(40.5811334762645,-12.0687951380098,-11.4956949233973));
#69308=CARTESIAN_POINT('Ctrl Pts',(40.6402187445438,-12.0751140828492,-11.4529356275011));
#69309=CARTESIAN_POINT('Ctrl Pts',(40.7916473972912,-12.0921134150615,-11.3324994366157));
#69310=CARTESIAN_POINT('Ctrl Pts',(40.8802411136818,-12.1029264986396,-11.2504505332821));
#69311=CARTESIAN_POINT('Ctrl Pts',(41.0419365771646,-12.1242778842078,-11.0763907470312));
#69312=CARTESIAN_POINT('Ctrl Pts',(41.1152197595652,-12.134785735661,-10.9849598283339));
#69313=CARTESIAN_POINT('Ctrl Pts',(41.1961239216403,-12.1472166947,-10.8673867156619));
#69314=CARTESIAN_POINT('Ctrl Pts',(41.2103466305909,-12.1494378545524,-10.8459918208529));
#69315=CARTESIAN_POINT('Ctrl Pts',(41.2312801438623,-12.1527579369728,-10.8133805766081));
#69316=CARTESIAN_POINT('Ctrl Pts',(41.2382462108354,-12.1538716991374,-10.8023315707104));
#69317=CARTESIAN_POINT('Ctrl Pts',(41.250820859159,-12.1558979985074,-10.7820218529997));
#69318=CARTESIAN_POINT('Ctrl Pts',(41.2564572447194,-12.156812192493,-10.7727795271475));
#69319=CARTESIAN_POINT('Ctrl Pts',(41.2694441309307,-12.1589328417281,-10.751157085998));
#69320=CARTESIAN_POINT('Ctrl Pts',(41.2767461628105,-12.1601362415648,-10.7387485810905));
#69321=CARTESIAN_POINT('Ctrl Pts',(41.3006340515201,-12.1641129604191,-10.697308565048));
#69322=CARTESIAN_POINT('Ctrl Pts',(41.316726997804,-12.1668578200936,-10.6679951637524));
#69323=CARTESIAN_POINT('Ctrl Pts',(41.3553199040437,-12.1736356949638,-10.5940851516062));
#69324=CARTESIAN_POINT('Ctrl Pts',(41.3770526974665,-12.1776343025331,-10.5491041302539));
#69325=CARTESIAN_POINT('Ctrl Pts',(41.4797329462882,-12.1976687799414,-10.3185142802863));
#69326=CARTESIAN_POINT('Ctrl Pts',(41.5384117329997,-12.2131619472121,-10.1238994860267));
#69327=CARTESIAN_POINT('Ctrl Pts',(41.5810553100192,-12.233789200857,-9.87053374643876));
#69328=CARTESIAN_POINT('Ctrl Pts',(41.5882662592702,-12.2382042405221,-9.81654993145718));
#69329=CARTESIAN_POINT('Ctrl Pts',(41.5960536419447,-12.2446847965724,-9.73802254120953));
#69330=CARTESIAN_POINT('Ctrl Pts',(41.598096524861,-12.2467050853659,-9.7136388749689));
#69331=CARTESIAN_POINT('Ctrl Pts',(41.6010772989839,-12.2503306552236,-9.67008289410366));
#69332=CARTESIAN_POINT('Ctrl Pts',(41.602158361476,-12.2519313497961,-9.6509222097963));
#69333=CARTESIAN_POINT('Ctrl Pts',(41.6039573638322,-12.2553278036847,-9.61042599211918));
#69334=CARTESIAN_POINT('Ctrl Pts',(41.6046207670379,-12.2571251179227,-9.58908986309842));
#69335=CARTESIAN_POINT('Ctrl Pts',(41.6056458849351,-12.2620061855472,-9.53141740654411));
#69336=CARTESIAN_POINT('Ctrl Pts',(41.6054682928594,-12.2651062661373,-9.49507863599632));
#69337=CARTESIAN_POINT('Ctrl Pts',(41.6009106761434,-12.2793409981676,-9.32964044030008));
#69338=CARTESIAN_POINT('Ctrl Pts',(41.5869597132131,-12.2907587977928,-9.20104068670405));
#69339=CARTESIAN_POINT('Ctrl Pts',(41.5355817193552,-12.3153184634751,-8.93175332990722));
#69340=CARTESIAN_POINT('Ctrl Pts',(41.4955760701008,-12.328453828886,-8.79204859779349));
#69341=CARTESIAN_POINT('Ctrl Pts',(41.4298817969084,-12.3444564890413,-8.62231109335828));
#69342=CARTESIAN_POINT('Ctrl Pts',(41.4157415344472,-12.3476791858735,-8.58813822961163));
#69343=CARTESIAN_POINT('Ctrl Pts',(41.3952154240443,-12.3520573452491,-8.54160032733227));
#69344=CARTESIAN_POINT('Ctrl Pts',(41.3895029488942,-12.3532466731366,-8.52894651786372));
#69345=CARTESIAN_POINT('Ctrl Pts',(41.3790550832277,-12.3553697599223,-8.50632753749832));
#69346=CARTESIAN_POINT('Ctrl Pts',(41.3743601148742,-12.3563057991912,-8.49634419965886));
#69347=CARTESIAN_POINT('Ctrl Pts',(41.3644268802704,-12.3582487602414,-8.47559418640268));
#69348=CARTESIAN_POINT('Ctrl Pts',(41.3591766728751,-12.3592549599153,-8.46483378841859));
#69349=CARTESIAN_POINT('Ctrl Pts',(41.3447819967961,-12.3619597428809,-8.43588217296116));
#69350=CARTESIAN_POINT('Ctrl Pts',(41.3354862753539,-12.3636495283759,-8.4177665526253));
#69351=CARTESIAN_POINT('Ctrl Pts',(41.2761571438391,-12.3741028293089,-8.30567261891157));
#69352=CARTESIAN_POINT('Ctrl Pts',(41.2201527380048,-12.3825522531078,-8.21497037392307));
#69353=CARTESIAN_POINT('Ctrl Pts',(41.0492926771049,-12.4056986323015,-7.97541328310945));
#69354=CARTESIAN_POINT('Ctrl Pts',(40.9227637462089,-12.4202092474583,-7.83586401618057));
#69355=CARTESIAN_POINT('Ctrl Pts',(40.7532744278501,-12.4384258546061,-7.68799838300081));
#69356=CARTESIAN_POINT('Ctrl Pts',(40.724684921271,-12.4414604690287,-7.66420124951601));
#69357=CARTESIAN_POINT('Ctrl Pts',(40.6769628977446,-12.4464743624698,-7.62631699612608));
#69358=CARTESIAN_POINT('Ctrl Pts',(40.6581523369864,-12.4484380790744,-7.61183293190663));
#69359=CARTESIAN_POINT('Ctrl Pts',(40.6236715780633,-12.4520173563612,-7.58608679145969));
#69360=CARTESIAN_POINT('Ctrl Pts',(40.6080741642415,-12.4536291199562,-7.57473019949258));
#69361=CARTESIAN_POINT('Ctrl Pts',(40.5739516915968,-12.4571406310443,-7.55050808214353));
#69362=CARTESIAN_POINT('Ctrl Pts',(40.5553790834878,-12.4590428391348,-7.53771314334845));
#69363=CARTESIAN_POINT('Ctrl Pts',(40.5020877305708,-12.4644773917166,-7.50209449756052));
#69364=CARTESIAN_POINT('Ctrl Pts',(40.4669555296242,-12.4680323829678,-7.47990773785733));
#69365=CARTESIAN_POINT('Ctrl Pts',(40.3852718029824,-12.4762415433406,-7.43123530336788));
#69366=CARTESIAN_POINT('Ctrl Pts',(40.338376337735,-12.4809144674893,-7.40537307695799));
#69367=CARTESIAN_POINT('Ctrl Pts',(40.1897859182684,-12.4955986458467,-7.32978110848318));
#69368=CARTESIAN_POINT('Ctrl Pts',(40.0854237972828,-12.5057474472962,-7.28565134676141));
#69369=CARTESIAN_POINT('Ctrl Pts',(39.8697500032924,-12.5262173819618,-7.21189339745932));
#69370=CARTESIAN_POINT('Ctrl Pts',(39.7586152099203,-12.5365129999654,-7.18256924199442));
#69371=CARTESIAN_POINT('Ctrl Pts',(39.620464619881,-12.5487532419623,-7.15651373448423));
#69372=CARTESIAN_POINT('Ctrl Pts',(39.595051947083,-12.5509817951602,-7.15214269141626));
#69373=CARTESIAN_POINT('Ctrl Pts',(39.5565743628291,-12.5543169193844,-7.14615979900953));
#69374=CARTESIAN_POINT('Ctrl Pts',(39.5435594968635,-12.5554382780791,-7.14424531398136));
#69375=CARTESIAN_POINT('Ctrl Pts',(39.5206185163224,-12.5574023128386,-7.14106274794722));
#69376=CARTESIAN_POINT('Ctrl Pts',(39.5106996979998,-12.558247301484,-7.13974974928353));
#69377=CARTESIAN_POINT('Ctrl Pts',(39.4865116585258,-12.5602981459257,-7.13670131409115));
#69378=CARTESIAN_POINT('Ctrl Pts',(39.4722345493033,-12.561500471632,-7.13503181508051));
#69379=CARTESIAN_POINT('Ctrl Pts',(39.4264324052607,-12.565333948092,-7.13009169993544));
#69380=CARTESIAN_POINT('Ctrl Pts',(39.3948557097709,-12.5679409247018,-7.12731592313843));
#69381=CARTESIAN_POINT('Ctrl Pts',(39.3172598772165,-12.574280245338,-7.1220380347081));
#69382=CARTESIAN_POINT('Ctrl Pts',(39.2712048696586,-12.5779852351098,-7.12023253672798));
#69383=CARTESIAN_POINT('Ctrl Pts',(39.0438074194755,-12.5961208970095,-7.11785732402667));
#69384=CARTESIAN_POINT('Ctrl Pts',(38.8628584655863,-12.6101013178022,-7.13647084063742));
#69385=CARTESIAN_POINT('Ctrl Pts',(38.6215062701294,-12.6298519186568,-7.18929492595988));
#69386=CARTESIAN_POINT('Ctrl Pts',(38.5579062998381,-12.6351596976618,-7.20597272850991));
#69387=CARTESIAN_POINT('Ctrl Pts',(38.4715313540076,-12.6425645278997,-7.2324484318039));
#69388=CARTESIAN_POINT('Ctrl Pts',(38.4481020751502,-12.6445932590993,-7.24002545235607));
#69389=CARTESIAN_POINT('Ctrl Pts',(38.4075512877431,-12.6481424746626,-7.25383075134866));
#69390=CARTESIAN_POINT('Ctrl Pts',(38.3903762332926,-12.6496577159095,-7.25989646229953));
#69391=CARTESIAN_POINT('Ctrl Pts',(38.3543861507293,-12.6528593266299,-7.27306869023705));
#69392=CARTESIAN_POINT('Ctrl Pts',(38.3355881555246,-12.6545469494113,-7.28021726720911));
#69393=CARTESIAN_POINT('Ctrl Pts',(38.2902116694931,-12.6586596465065,-7.29812768702052));
#69394=CARTESIAN_POINT('Ctrl Pts',(38.2637323861268,-12.661092416769,-7.30913043956218));
#69395=CARTESIAN_POINT('Ctrl Pts',(38.1634397132502,-12.6704378217172,-7.35292291351868));
#69396=CARTESIAN_POINT('Ctrl Pts',(38.0911066283019,-12.6774549325123,-7.3889455844176));
#69397=CARTESIAN_POINT('Ctrl Pts',(37.9220293917355,-12.6945533234796,-7.48405211883646));
#69398=CARTESIAN_POINT('Ctrl Pts',(37.827381440119,-12.7047153723466,-7.54646748654571));
#69399=CARTESIAN_POINT('Ctrl Pts',(37.6505455582212,-12.7247361284071,-7.68189478509101));
#69400=CARTESIAN_POINT('Ctrl Pts',(37.568241289525,-12.734570146411,-7.75434644945453));
#69401=CARTESIAN_POINT('Ctrl Pts',(37.4771610585272,-12.7458843881036,-7.84628790424061));
#69402=CARTESIAN_POINT('Ctrl Pts',(37.4633423278758,-12.7476136262563,-7.86058763598447));
#69403=CARTESIAN_POINT('Ctrl Pts',(37.4479329618307,-12.7495548577216,-7.87693425832693));
#69404=CARTESIAN_POINT('Ctrl Pts',(37.4461670091522,-12.7497775229632,-7.87881366928609));
#69405=CARTESIAN_POINT('Ctrl Pts',(37.4444040758239,-12.75,-7.88069592367579));
#69406=CARTESIAN_POINT('',(40.3181783974771,-12.75,-7.39532161681262));
#69407=CARTESIAN_POINT('Origin',(39.2,-12.75,-9.525));
#69408=CARTESIAN_POINT('',(36.7946210610025,-11.8952248199035,-9.52725925364505));
#69409=CARTESIAN_POINT('Ctrl Pts',(36.7946210610025,-11.8952248199035,-9.52725925364505));
#69410=CARTESIAN_POINT('Ctrl Pts',(36.7947186589564,-11.9039501489463,-9.63116970366884));
#69411=CARTESIAN_POINT('Ctrl Pts',(36.8015536899245,-11.912675477989,-9.73478128463119));
#69412=CARTESIAN_POINT('Ctrl Pts',(36.8149857633701,-11.9214008070318,-9.83734601882026));
#69413=CARTESIAN_POINT('Ctrl Pts',(36.8284178368158,-11.9301261360746,-9.93991075300932));
#69414=CARTESIAN_POINT('Ctrl Pts',(36.8484467666642,-11.9388514651173,-10.0414289472041));
#69415=CARTESIAN_POINT('Ctrl Pts',(36.8748810013598,-11.9475767941601,-10.1411773986139));
#69416=CARTESIAN_POINT('Ctrl Pts',(36.8953762218173,-11.9543417920635,-10.2185152343967));
#69417=CARTESIAN_POINT('Ctrl Pts',(36.9197715899412,-11.961106789967,-10.2949704447773));
#69418=CARTESIAN_POINT('Ctrl Pts',(36.9479738992011,-11.9678717878704,-10.3701221129046));
#69419=CARTESIAN_POINT('Ctrl Pts',(36.9761359648038,-11.9746271323709,-10.445166542368));
#69420=CARTESIAN_POINT('Ctrl Pts',(37.0080940195322,-11.9813824768713,-10.5189106928252));
#69421=CARTESIAN_POINT('Ctrl Pts',(37.0437045982079,-11.9881378213718,-10.5909470364939));
#69422=CARTESIAN_POINT('Ctrl Pts',(37.0792739104633,-11.9948853376118,-10.6628999026641));
#69423=CARTESIAN_POINT('Ctrl Pts',(37.1184871288128,-12.0016328538518,-10.7331484813702));
#69424=CARTESIAN_POINT('Ctrl Pts',(37.1611526010783,-12.0083803700919,-10.8013049119667));
#69425=CARTESIAN_POINT('Ctrl Pts',(37.2037909501032,-12.0151235968093,-10.8694180142423));
#69426=CARTESIAN_POINT('Ctrl Pts',(37.2498769501429,-12.0218668235267,-10.9354412162069));
#69427=CARTESIAN_POINT('Ctrl Pts',(37.2991734512255,-12.0286100502441,-10.9990119999084));
#69428=CARTESIAN_POINT('Ctrl Pts',(37.3484536494874,-12.0353510469125,-11.0625617601484));
#69429=CARTESIAN_POINT('Ctrl Pts',(37.4009419555341,-12.0420920435809,-11.1236603462121));
#69430=CARTESIAN_POINT('Ctrl Pts',(37.456359245328,-12.0488330402492,-11.1819761202404));
#69431=CARTESIAN_POINT('Ctrl Pts',(37.5117751102101,-12.0555738635903,-11.2402903948299));
#69432=CARTESIAN_POINT('Ctrl Pts',(37.5701194881866,-12.0623146869315,-11.2958216638355));
#69433=CARTESIAN_POINT('Ctrl Pts',(37.6310754912959,-12.0690555102726,-11.3482742060336));
#69434=CARTESIAN_POINT('Ctrl Pts',(37.6920891892273,-12.0758027137992,-11.400776394533));
#69435=CARTESIAN_POINT('Ctrl Pts',(37.7557190975019,-12.0825499173258,-11.4501937312609));
#69436=CARTESIAN_POINT('Ctrl Pts',(37.8216146789238,-12.0892971208523,-11.4962703647754));
#69437=CARTESIAN_POINT('Ctrl Pts',(37.8875405388679,-12.096047424668,-11.5423681701551));
#69438=CARTESIAN_POINT('Ctrl Pts',(37.9557337525196,-12.1027977284837,-11.5851219661566));
#69439=CARTESIAN_POINT('Ctrl Pts',(38.0258162750942,-12.1095480322993,-11.6243202529786));
#69440=CARTESIAN_POINT('Ctrl Pts',(38.0960202739729,-12.116310036635,-11.6635864834596));
#69441=CARTESIAN_POINT('Ctrl Pts',(38.1681197084572,-12.1230720409707,-11.6992846828844));
#69442=CARTESIAN_POINT('Ctrl Pts',(38.2417136926401,-12.1298340453064,-11.7312502798927));
#69443=CARTESIAN_POINT('Ctrl Pts',(38.3082789127791,-12.1359502287443,-11.7601629284652));
#69444=CARTESIAN_POINT('Ctrl Pts',(38.3760663357046,-12.1420664121822,-11.7860224535644));
#69445=CARTESIAN_POINT('Ctrl Pts',(38.444769163389,-12.1481825956201,-11.8087423952434));
#69446=CARTESIAN_POINT('Ctrl Pts',(38.5207016312425,-12.1549423887456,-11.8338531701462));
#69447=CARTESIAN_POINT('Ctrl Pts',(38.5980250033347,-12.161702181871,-11.8552181838809));
#69448=CARTESIAN_POINT('Ctrl Pts',(38.6763360263255,-12.1684619749965,-11.8726858791319));
#69449=CARTESIAN_POINT('Ctrl Pts',(38.7545372919926,-12.17521229389,-11.8901290924211));
#69450=CARTESIAN_POINT('Ctrl Pts',(38.8337230087439,-12.1819626127834,-11.9036857361839));
#69451=CARTESIAN_POINT('Ctrl Pts',(38.9134737198311,-12.1887129316769,-11.9132536789823));
#69452=CARTESIAN_POINT('Ctrl Pts',(38.993135366358,-12.1954557119017,-11.9228109364263));
#69453=CARTESIAN_POINT('Ctrl Pts',(39.0733602935979,-12.2021984921265,-11.928388291076));
#69454=CARTESIAN_POINT('Ctrl Pts',(39.1537192200424,-12.2089412723513,-11.9299347254773));
#69455=CARTESIAN_POINT('Ctrl Pts',(39.2340291491899,-12.2156799412966,-11.9314802169702));
#69456=CARTESIAN_POINT('Ctrl Pts',(39.314472451482,-12.222418610242,-11.9289996585284));
#69457=CARTESIAN_POINT('Ctrl Pts',(39.3946162739486,-12.2291572791873,-11.9224939938015));
#69458=CARTESIAN_POINT('Ctrl Pts',(39.4747357506959,-12.235893901091,-11.9159903053353));
#69459=CARTESIAN_POINT('Ctrl Pts',(39.5545554650489,-12.2426305229946,-11.9054639766861));
#69460=CARTESIAN_POINT('Ctrl Pts',(39.6336455636557,-12.2493671448983,-11.8909679772815));
#69461=CARTESIAN_POINT('Ctrl Pts',(39.7127358338636,-12.2561037814183,-11.8764719464251));
#69462=CARTESIAN_POINT('Ctrl Pts',(39.7910960279766,-12.2628404179384,-11.8580063129897));
#69463=CARTESIAN_POINT('Ctrl Pts',(39.8683058174271,-12.2695770544585,-11.8356752863164));
#69464=CARTESIAN_POINT('Ctrl Pts',(39.945592404757,-12.2763203916754,-11.8133220477512));
#69465=CARTESIAN_POINT('Ctrl Pts',(40.0217258539102,-12.2830637288924,-11.7870958654182));
#69466=CARTESIAN_POINT('Ctrl Pts',(40.0963009027855,-12.2898070661094,-11.7571508990357));
#69467=CARTESIAN_POINT('Ctrl Pts',(40.1709121142176,-12.2965536732715,-11.7271914118911));
#69468=CARTESIAN_POINT('Ctrl Pts',(40.2439629968681,-12.3033002804336,-11.6935097428903));
#69469=CARTESIAN_POINT('Ctrl Pts',(40.315070495802,-12.3100468875956,-11.6563072828177));
#69470=CARTESIAN_POINT('Ctrl Pts',(40.3863047468538,-12.3168055208697,-11.61903850779));
#69471=CARTESIAN_POINT('Ctrl Pts',(40.4555882903888,-12.3235641541437,-11.5782366376932));
#69472=CARTESIAN_POINT('Ctrl Pts',(40.5225649641608,-12.3303227874178,-11.5341477944577));
#69473=CARTESIAN_POINT('Ctrl Pts',(40.5835617694908,-12.3364779906385,-11.4939953288812));
#69474=CARTESIAN_POINT('Ctrl Pts',(40.6426454031471,-12.3426331938593,-11.4511173257771));
#69475=CARTESIAN_POINT('Ctrl Pts',(40.6995715373854,-12.34878839708,-11.4057280900395));
#69476=CARTESIAN_POINT('Ctrl Pts',(40.7614038109521,-12.3554740822138,-11.3564270145552));
#69477=CARTESIAN_POINT('Ctrl Pts',(40.8209297575957,-12.3621597673477,-11.3039715293003));
#69478=CARTESIAN_POINT('Ctrl Pts',(40.8778053802409,-12.3688454524815,-11.2486072784816));
#69479=CARTESIAN_POINT('Ctrl Pts',(40.9345989025398,-12.3755214867836,-11.1933229463338));
#69480=CARTESIAN_POINT('Ctrl Pts',(40.9887493562766,-12.3821975210857,-11.1351385120028));
#69481=CARTESIAN_POINT('Ctrl Pts',(41.039944698374,-12.3888735553877,-11.0743406505108));
#69482=CARTESIAN_POINT('Ctrl Pts',(41.0912345614128,-12.3955619155191,-11.0134305391371));
#69483=CARTESIAN_POINT('Ctrl Pts',(41.139558021386,-12.4022502756504,-10.9498976508583));
#69484=CARTESIAN_POINT('Ctrl Pts',(41.1846376443065,-12.4089386357818,-10.8840681974064));
#69485=CARTESIAN_POINT('Ctrl Pts',(41.2295564640133,-12.4156031379095,-10.8184735637464));
#69486=CARTESIAN_POINT('Ctrl Pts',(41.2712542670028,-12.4222676400373,-10.7505991077033));
#69487=CARTESIAN_POINT('Ctrl Pts',(41.3094974475735,-12.4289321421651,-10.6807999234647));
#69488=CARTESIAN_POINT('Ctrl Pts',(41.3477297928876,-12.4355947560716,-10.6110205150935));
#69489=CARTESIAN_POINT('Ctrl Pts',(41.3825092293477,-12.442257369978,-10.5393178783685));
#69490=CARTESIAN_POINT('Ctrl Pts',(41.4136472332856,-12.4489199838844,-10.4660732548356));
#69491=CARTESIAN_POINT('Ctrl Pts',(41.4447864767208,-12.4555828630067,-10.3928257156854));
#69492=CARTESIAN_POINT('Ctrl Pts',(41.4722838147315,-12.462245742129,-10.3180365069909));
#69493=CARTESIAN_POINT('Ctrl Pts',(41.4959988032221,-12.4689086212512,-10.2421069934135));
#69494=CARTESIAN_POINT('Ctrl Pts',(41.5198712976804,-12.4756157526919,-10.1656731847775));
#69495=CARTESIAN_POINT('Ctrl Pts',(41.5399108594295,-12.4823228841327,-10.0880843317876));
#69496=CARTESIAN_POINT('Ctrl Pts',(41.5560257516827,-12.4890300155734,-10.0097634493319));
#69497=CARTESIAN_POINT('Ctrl Pts',(41.5720613477695,-12.4957041433923,-9.93182795857612));
#69498=CARTESIAN_POINT('Ctrl Pts',(41.58421080047,-12.5023782712112,-9.85316811001779));
#69499=CARTESIAN_POINT('Ctrl Pts',(41.5924357484883,-12.50905239903,-9.7742070098437));
#69500=CARTESIAN_POINT('Ctrl Pts',(41.600721705169,-12.5157760322817,-9.69466021464805));
#69501=CARTESIAN_POINT('Ctrl Pts',(41.6050246821397,-12.5224996655334,-9.61480817148));
#69502=CARTESIAN_POINT('Ctrl Pts',(41.6053588685275,-12.529223298785,-9.53508255900005));
#69503=CARTESIAN_POINT('Ctrl Pts',(41.6056930549153,-12.5359469320367,-9.45535694652009));
#69504=CARTESIAN_POINT('Ctrl Pts',(41.6020585501418,-12.5426705652883,-9.37575824569389));
#69505=CARTESIAN_POINT('Ctrl Pts',(41.5945222031575,-12.54939419854,-9.29670991483252));
#69506=CARTESIAN_POINT('Ctrl Pts',(41.5867483123806,-12.5563297590485,-9.21517000013748));
#69507=CARTESIAN_POINT('Ctrl Pts',(41.574793301892,-12.5632653195569,-9.1339033638181));
#69508=CARTESIAN_POINT('Ctrl Pts',(41.5586876183147,-12.5702008800654,-9.05335854337322));
#69509=CARTESIAN_POINT('Ctrl Pts',(41.5426074010974,-12.5771254740426,-8.97294108066456));
#69510=CARTESIAN_POINT('Ctrl Pts',(41.5223896476239,-12.5840500680199,-8.89324358831412));
#69511=CARTESIAN_POINT('Ctrl Pts',(41.4981164888731,-12.5909746619971,-8.81470882874016));
#69512=CARTESIAN_POINT('Ctrl Pts',(41.473881501497,-12.5978883665275,-8.73629757100507));
#69513=CARTESIAN_POINT('Ctrl Pts',(41.4456039330987,-12.6048020710579,-8.65904581993135));
#69514=CARTESIAN_POINT('Ctrl Pts',(41.4134164805572,-12.6117157755884,-8.58338413989683));
#69515=CARTESIAN_POINT('Ctrl Pts',(41.3812588456174,-12.6186230754464,-8.50779255083449));
#69516=CARTESIAN_POINT('Ctrl Pts',(41.3451986982026,-12.6255303753044,-8.43378850320112));
#69517=CARTESIAN_POINT('Ctrl Pts',(41.3054176952937,-12.6324376751625,-8.36178494131817));
#69518=CARTESIAN_POINT('Ctrl Pts',(41.2656638151787,-12.639340265605,-8.28983047165588));
#69519=CARTESIAN_POINT('Ctrl Pts',(41.2221943354176,-12.6462428560476,-8.21987415539018));
#69520=CARTESIAN_POINT('Ctrl Pts',(41.1752374670053,-12.6531454464902,-8.15230560817845));
#69521=CARTESIAN_POINT('Ctrl Pts',(41.1283011405467,-12.6600450172958,-8.08476661979401));
#69522=CARTESIAN_POINT('Ctrl Pts',(41.0778807094616,-12.6669445881015,-8.01961367923981));
#69523=CARTESIAN_POINT('Ctrl Pts',(41.0242478569796,-12.6738441589071,-7.95720769847997));
#69524=CARTESIAN_POINT('Ctrl Pts',(40.9706098995415,-12.6807443864373,-7.8947957777081));
#69525=CARTESIAN_POINT('Ctrl Pts',(40.913759186687,-12.6876446139674,-7.83513167569318));
#69526=CARTESIAN_POINT('Ctrl Pts',(40.854007437666,-12.6945448414975,-7.77854291763422));
#69527=CARTESIAN_POINT('Ctrl Pts',(40.7942556066665,-12.7014450784946,-7.72195408193639));
#69528=CARTESIAN_POINT('Ctrl Pts',(40.7316030523931,-12.7083453154917,-7.66844089369298));
#69529=CARTESIAN_POINT('Ctrl Pts',(40.6663969572748,-12.7152455524888,-7.61829265274002));
#69530=CARTESIAN_POINT('Ctrl Pts',(40.6011444758808,-12.7221506981727,-7.56810873735922));
#69531=CARTESIAN_POINT('Ctrl Pts',(40.5333351737933,-12.7290558438566,-7.52129481301359));
#69532=CARTESIAN_POINT('Ctrl Pts',(40.4633474192269,-12.7359609895405,-7.47809837981088));
#69533=CARTESIAN_POINT('Ctrl Pts',(40.4159161815491,-12.7406406596937,-7.44882382595842));
#69534=CARTESIAN_POINT('Ctrl Pts',(40.3674850379813,-12.7453203298468,-7.42120985453868));
#69535=CARTESIAN_POINT('Ctrl Pts',(40.3181783974771,-12.75,-7.39532161681263));
#69536=CARTESIAN_POINT('Ctrl Pts',(36.7946210320027,-11.8956214580413,-9.52722816428394));
#69537=CARTESIAN_POINT('Ctrl Pts',(36.7945104667753,-11.8862658381917,-9.40786924872099));
#69538=CARTESIAN_POINT('Ctrl Pts',(36.8032839374915,-11.8768622465317,-9.28867798243652));
#69539=CARTESIAN_POINT('Ctrl Pts',(36.8251651662405,-11.8648356185918,-9.14177147686941));
#69540=CARTESIAN_POINT('Ctrl Pts',(36.8299891894927,-11.8624587560463,-9.11298882687568));
#69541=CARTESIAN_POINT('Ctrl Pts',(36.8390759405276,-11.8583923497813,-9.06423179043359));
#69542=CARTESIAN_POINT('Ctrl Pts',(36.8430716794022,-11.8567109743571,-9.0442104438046));
#69543=CARTESIAN_POINT('Ctrl Pts',(36.8515198883864,-11.8533529365506,-9.00451870099323));
#69544=CARTESIAN_POINT('Ctrl Pts',(36.8559658566946,-11.8516766043042,-8.98484863204398));
#69545=CARTESIAN_POINT('Ctrl Pts',(36.8651906959268,-11.8483656869082,-8.94629648569365));
#69546=CARTESIAN_POINT('Ctrl Pts',(36.8699526424761,-11.8467317600666,-8.92741192479448));
#69547=CARTESIAN_POINT('Ctrl Pts',(36.8809762653888,-11.8431062195011,-8.88583171043609));
#69548=CARTESIAN_POINT('Ctrl Pts',(36.8873428245448,-11.8411113778412,-8.86316626886844));
#69549=CARTESIAN_POINT('Ctrl Pts',(36.9107217626599,-11.8341110687762,-8.78439540198754));
#69550=CARTESIAN_POINT('Ctrl Pts',(36.9294502714909,-11.829051585831,-8.7288262188455));
#69551=CARTESIAN_POINT('Ctrl Pts',(36.9527678797602,-11.8232961015687,-8.66718071860874));
#69552=CARTESIAN_POINT('Ctrl Pts',(36.9553784964742,-11.8226584942794,-8.66037268072647));
#69553=CARTESIAN_POINT('Ctrl Pts',(36.9580196917093,-11.8220201063326,-8.65357746090844));
#69554=CARTESIAN_POINT('Origin',(39.2,-12.75,-9.525));
#69555=CARTESIAN_POINT('',(41.1084785589541,-12.75,-11.9808583515571));
#69556=CARTESIAN_POINT('',(36.08977,-12.75,-9.525));
#69557=CARTESIAN_POINT('Origin',(39.2,-12.75,-9.525));
#69558=CARTESIAN_POINT('Ctrl Pts',(41.1084785589541,-12.75,-11.9808583515571));
#69559=CARTESIAN_POINT('Ctrl Pts',(41.1177983966318,-12.75,-11.9717669582536));
#69560=CARTESIAN_POINT('Ctrl Pts',(41.1270543353679,-12.75,-11.9626123445009));
#69561=CARTESIAN_POINT('Ctrl Pts',(41.1362455536515,-12.75,-11.9533945855071));
#69562=CARTESIAN_POINT('Ctrl Pts',(41.2078661956446,-12.75,-11.8815671305931));
#69563=CARTESIAN_POINT('Ctrl Pts',(41.2755608385581,-12.75,-11.8059075492844));
#69564=CARTESIAN_POINT('Ctrl Pts',(41.3392177633947,-12.75,-11.7268202136986));
#69565=CARTESIAN_POINT('Ctrl Pts',(41.3943876820438,-12.75,-11.6582771308897));
#69566=CARTESIAN_POINT('Ctrl Pts',(41.4465241253691,-12.75,-11.5871584953386));
#69567=CARTESIAN_POINT('Ctrl Pts',(41.4955251476878,-12.75,-11.5137175255415));
#69568=CARTESIAN_POINT('Ctrl Pts',(41.5101767234174,-12.75,-11.4917582708215));
#69569=CARTESIAN_POINT('Ctrl Pts',(41.5245486734672,-12.75,-11.4695899646366));
#69570=CARTESIAN_POINT('Ctrl Pts',(41.5386355217927,-12.75,-11.4472228736974));
#69571=CARTESIAN_POINT('Ctrl Pts',(41.5519504183468,-12.75,-11.4260814874063));
#69572=CARTESIAN_POINT('Ctrl Pts',(41.5650061724716,-12.75,-11.404769422587));
#69573=CARTESIAN_POINT('Ctrl Pts',(41.5777948568304,-12.75,-11.3833028614934));
#69574=CARTESIAN_POINT('Ctrl Pts',(41.6294048341385,-12.75,-11.2966724701383));
#69575=CARTESIAN_POINT('Ctrl Pts',(41.6766999371217,-12.75,-11.2074785188293));
#69576=CARTESIAN_POINT('Ctrl Pts',(41.7195470841769,-12.75,-11.1161137346045));
#69577=CARTESIAN_POINT('Ctrl Pts',(41.7620308413559,-12.75,-11.025523821985));
#69578=CARTESIAN_POINT('Ctrl Pts',(41.8001418510265,-12.75,-10.9327987519571));
#69579=CARTESIAN_POINT('Ctrl Pts',(41.8336996271297,-12.75,-10.8383186854066));
#69580=CARTESIAN_POINT('Ctrl Pts',(41.8380607202485,-12.75,-10.8260402684213));
#69581=CARTESIAN_POINT('Ctrl Pts',(41.8423448419313,-12.75,-10.813732219562));
#69582=CARTESIAN_POINT('Ctrl Pts',(41.8465515312897,-12.75,-10.8013953832721));
#69583=CARTESIAN_POINT('Ctrl Pts',(41.8519573108627,-12.75,-10.7855420097684));
#69584=CARTESIAN_POINT('Ctrl Pts',(41.857235428307,-12.75,-10.7696402235551));
#69585=CARTESIAN_POINT('Ctrl Pts',(41.8623800097954,-12.75,-10.7537076086219));
#69586=CARTESIAN_POINT('Ctrl Pts',(41.8924329745631,-12.75,-10.6606344759834));
#69587=CARTESIAN_POINT('Ctrl Pts',(41.9179769286029,-12.75,-10.5663842906978));
#69588=CARTESIAN_POINT('Ctrl Pts',(41.9388991726743,-12.75,-10.4713165340972));
#69589=CARTESIAN_POINT('Ctrl Pts',(41.9595829880513,-12.7499999999999,-10.3773321642029));
#69590=CARTESIAN_POINT('Ctrl Pts',(41.9757498406875,-12.75,-10.282547834876));
#69591=CARTESIAN_POINT('Ctrl Pts',(41.9872405753498,-12.75,-10.1873132752954));
#69592=CARTESIAN_POINT('Ctrl Pts',(41.998401906114,-12.75,-10.0948087966098));
#69593=CARTESIAN_POINT('Ctrl Pts',(42.0051512351925,-12.75,-10.0018788103257));
#69594=CARTESIAN_POINT('Ctrl Pts',(42.0072961959229,-12.75,-9.90885796114165));
#69595=CARTESIAN_POINT('Ctrl Pts',(42.0085525980484,-12.75,-9.85437137265856));
#69596=CARTESIAN_POINT('Ctrl Pts',(42.0082283810938,-12.75,-9.79985393080354));
#69597=CARTESIAN_POINT('Ctrl Pts',(42.0062774111146,-12.75,-9.74537669181848));
#69598=CARTESIAN_POINT('Ctrl Pts',(42.0056087070014,-12.75,-9.7267043625824));
#69599=CARTESIAN_POINT('Ctrl Pts',(42.0047488424704,-12.7499999999999,-9.70803678557931));
#69600=CARTESIAN_POINT('Ctrl Pts',(42.0036958084692,-12.75,-9.68937691893248));
#69601=CARTESIAN_POINT('Ctrl Pts',(42.0029149036918,-12.75,-9.67553920904492));
#69602=CARTESIAN_POINT('Ctrl Pts',(42.0020282962605,-12.75,-9.66171521265807));
#69603=CARTESIAN_POINT('Ctrl Pts',(42.0010356525435,-12.75,-9.64790697816443));
#69604=CARTESIAN_POINT('Ctrl Pts',(41.9945063923453,-12.75,-9.55708128276281));
#69605=CARTESIAN_POINT('Ctrl Pts',(41.9833925950157,-12.7499999999999,-9.46692217583271));
#69606=CARTESIAN_POINT('Ctrl Pts',(41.9675554099829,-12.75,-9.37773775964327));
#69607=CARTESIAN_POINT('Ctrl Pts',(41.9607505630484,-12.75,-9.33941742052689));
#69608=CARTESIAN_POINT('Ctrl Pts',(41.9530730683015,-12.75,-9.30127722046684));
#69609=CARTESIAN_POINT('Ctrl Pts',(41.9445091332559,-12.75,-9.26334269611395));
#69610=CARTESIAN_POINT('Ctrl Pts',(41.9237890194308,-12.75,-9.1715615629886));
#69611=CARTESIAN_POINT('Ctrl Pts',(41.897882700181,-12.7499999999999,-9.08098197605832));
#69612=CARTESIAN_POINT('Ctrl Pts',(41.8670374313203,-12.75,-8.99192525440121));
#69613=CARTESIAN_POINT('Ctrl Pts',(41.8361921624596,-12.75,-8.90286853274409));
#69614=CARTESIAN_POINT('Ctrl Pts',(41.8004070957505,-12.75,-8.81533391622066));
#69615=CARTESIAN_POINT('Ctrl Pts',(41.7598933162349,-12.75,-8.72968369143849));
#69616=CARTESIAN_POINT('Ctrl Pts',(41.7520217401559,-12.75,-8.71304238399647));
#69617=CARTESIAN_POINT('Ctrl Pts',(41.7439715676172,-12.75,-8.69647235644754));
#69618=CARTESIAN_POINT('Ctrl Pts',(41.7357442304968,-12.75,-8.67997648296463));
#69619=CARTESIAN_POINT('Ctrl Pts',(41.729514813746,-12.75,-8.66748645501395));
#69620=CARTESIAN_POINT('Ctrl Pts',(41.7231878371419,-12.7499999999999,-8.65504700546118));
#69621=CARTESIAN_POINT('Ctrl Pts',(41.7167654750851,-12.75,-8.64266142135632));
#69622=CARTESIAN_POINT('Ctrl Pts',(41.6752249123853,-12.75,-8.56255006535911));
#69623=CARTESIAN_POINT('Ctrl Pts',(41.6296810084744,-12.75,-8.48465727580426));
#69624=CARTESIAN_POINT('Ctrl Pts',(41.580378827968,-12.75,-8.40925152491517));
#69625=CARTESIAN_POINT('Ctrl Pts',(41.5314354814769,-12.7499999999999,-8.33439459657495));
#69626=CARTESIAN_POINT('Ctrl Pts',(41.4787875447868,-12.75,-8.26198804712867));
#69627=CARTESIAN_POINT('Ctrl Pts',(41.4226420462153,-12.75,-8.19233310842445));
#69628=CARTESIAN_POINT('Ctrl Pts',(41.3670515962938,-12.75,-8.12336677131231));
#69629=CARTESIAN_POINT('Ctrl Pts',(41.3080316361269,-12.75,-8.05709740682041));
#69630=CARTESIAN_POINT('Ctrl Pts',(41.2457626467438,-12.75,-7.99386341792389));
#69631=CARTESIAN_POINT('Ctrl Pts',(41.2267639300686,-12.75,-7.97457027295411));
#69632=CARTESIAN_POINT('Ctrl Pts',(41.2074626579876,-12.75,-7.95556004729628));
#69633=CARTESIAN_POINT('Ctrl Pts',(41.1878637361297,-12.75,-7.93684332516778));
#69634=CARTESIAN_POINT('Ctrl Pts',(41.1712853455817,-12.75,-7.9210111721812));
#69635=CARTESIAN_POINT('Ctrl Pts',(41.1544939793358,-12.75,-7.90538903367538));
#69636=CARTESIAN_POINT('Ctrl Pts',(41.1374925744962,-12.75,-7.88998358950291));
#69637=CARTESIAN_POINT('Ctrl Pts',(41.1276172064111,-12.75,-7.88103524475422));
#69638=CARTESIAN_POINT('Ctrl Pts',(41.1176718130391,-12.75,-7.87216086334629));
#69639=CARTESIAN_POINT('Ctrl Pts',(41.1076664155748,-12.75,-7.86336977076331));
#69640=CARTESIAN_POINT('Ctrl Pts',(41.0432046529541,-12.75,-7.80673140879069));
#69641=CARTESIAN_POINT('Ctrl Pts',(40.9761510753172,-12.75,-7.75345252931226));
#69642=CARTESIAN_POINT('Ctrl Pts',(40.9066975736398,-12.75,-7.70379730514819));
#69643=CARTESIAN_POINT('Ctrl Pts',(40.8383344183618,-12.75,-7.65492161540032));
#69644=CARTESIAN_POINT('Ctrl Pts',(40.7676453780882,-12.75,-7.60955634955628));
#69645=CARTESIAN_POINT('Ctrl Pts',(40.694798190339,-12.75,-7.56800068927081));
#69646=CARTESIAN_POINT('Ctrl Pts',(40.6241249698281,-12.75,-7.52768516806028));
#69647=CARTESIAN_POINT('Ctrl Pts',(40.5514198830853,-12.75,-7.49095512491116));
#69648=CARTESIAN_POINT('Ctrl Pts',(40.4768312911088,-12.75,-7.45813193578272));
#69649=CARTESIAN_POINT('Ctrl Pts',(40.4248450302792,-12.75,-7.4352550476947));
#69650=CARTESIAN_POINT('Ctrl Pts',(40.3719437125909,-12.75,-7.41427698771476));
#69651=CARTESIAN_POINT('Ctrl Pts',(40.3181783974771,-12.75,-7.39532161681262));
#69652=CARTESIAN_POINT('',(37.423659425391,-12.7512312321065,-7.90004131257367));
#69653=CARTESIAN_POINT('Ctrl Pts',(37.4444040758239,-12.75,-7.88069592367579));
#69654=CARTESIAN_POINT('Ctrl Pts',(37.4379608436199,-12.7504104107022,-7.88757525479146));
#69655=CARTESIAN_POINT('Ctrl Pts',(37.4315580470395,-12.7508208214043,-7.89449245820598));
#69656=CARTESIAN_POINT('Ctrl Pts',(37.4251961284841,-12.7512312321065,-7.90144705597498));
#69657=CARTESIAN_POINT('Ctrl Pts',(37.4219896448371,-12.75,-7.89867535481033));
#69658=CARTESIAN_POINT('Ctrl Pts',(37.4041800318868,-12.75,-7.91315252990336));
#69659=CARTESIAN_POINT('Ctrl Pts',(37.3866079915316,-12.75,-7.92789833873796));
#69660=CARTESIAN_POINT('Ctrl Pts',(37.3692807783977,-12.75,-7.94290979008526));
#69661=CARTESIAN_POINT('Ctrl Pts',(37.3073978200408,-12.75,-7.99652216337458));
#69662=CARTESIAN_POINT('Ctrl Pts',(37.2486361525171,-12.75,-8.05351884266802));
#69663=CARTESIAN_POINT('Ctrl Pts',(37.1930196554172,-12.75,-8.11352008911787));
#69664=CARTESIAN_POINT('Ctrl Pts',(37.1575846699701,-12.75,-8.15174873359617));
#69665=CARTESIAN_POINT('Ctrl Pts',(37.1234267578552,-12.75,-8.19119811603227));
#69666=CARTESIAN_POINT('Ctrl Pts',(37.0905565908903,-12.75,-8.23178001255319));
#69667=CARTESIAN_POINT('Ctrl Pts',(37.0738455802734,-12.75,-8.25241162371415));
#69668=CARTESIAN_POINT('Ctrl Pts',(37.0574674682131,-12.75,-8.27333606608347));
#69669=CARTESIAN_POINT('Ctrl Pts',(37.0414240687244,-12.75,-8.29454242346543));
#69670=CARTESIAN_POINT('Ctrl Pts',(37.0265574148782,-12.75,-8.314193344379));
#69671=CARTESIAN_POINT('Ctrl Pts',(37.0119749045712,-12.75,-8.33409122869043));
#69672=CARTESIAN_POINT('Ctrl Pts',(36.9976972145749,-12.75,-8.35420012550333));
#69673=CARTESIAN_POINT('Ctrl Pts',(36.9478117565662,-12.75,-8.42445949714009));
#69674=CARTESIAN_POINT('Ctrl Pts',(36.9016057374712,-12.75,-8.49734007805571));
#69675=CARTESIAN_POINT('Ctrl Pts',(36.8591144753857,-12.75,-8.57244354508648));
#69676=CARTESIAN_POINT('Ctrl Pts',(36.8225527531614,-12.75,-8.63706652790425));
#69677=CARTESIAN_POINT('Ctrl Pts',(36.7887415597637,-12.75,-8.70333641037004));
#69678=CARTESIAN_POINT('Ctrl Pts',(36.7577206548755,-12.75,-8.77102495961378));
#69679=CARTESIAN_POINT('Ctrl Pts',(36.748069517199,-12.75,-8.79208403284934));
#69680=CARTESIAN_POINT('Ctrl Pts',(36.7386885924217,-12.75,-8.81328057411961));
#69681=CARTESIAN_POINT('Ctrl Pts',(36.7295794455984,-12.75,-8.83460808988947));
#69682=CARTESIAN_POINT('Ctrl Pts',(36.7220483554448,-12.75,-8.85224085475003));
#69683=CARTESIAN_POINT('Ctrl Pts',(36.7147022785046,-12.75,-8.86996535756085));
#69684=CARTESIAN_POINT('Ctrl Pts',(36.7075507171553,-12.75,-8.88775585391959));
#69685=CARTESIAN_POINT('Ctrl Pts',(36.6740987028843,-12.75,-8.97097235854196));
#69686=CARTESIAN_POINT('Ctrl Pts',(36.644855758403,-12.75,-9.05573011267507));
#69687=CARTESIAN_POINT('Ctrl Pts',(36.6198544411057,-12.75,-9.14161810772437));
#69688=CARTESIAN_POINT('Ctrl Pts',(36.5943080999463,-12.75,-9.22937844438731));
#69689=CARTESIAN_POINT('Ctrl Pts',(36.5731897292325,-12.75,-9.31831956866093));
#69690=CARTESIAN_POINT('Ctrl Pts',(36.5565704314595,-12.75,-9.4080440570504));
#69691=CARTESIAN_POINT('Ctrl Pts',(36.5401253552976,-12.75,-9.49682795546161));
#69692=CARTESIAN_POINT('Ctrl Pts',(36.5280851134617,-12.75,-9.58637983259742));
#69693=CARTESIAN_POINT('Ctrl Pts',(36.5205611019666,-12.75,-9.67634142246066));
#69694=CARTESIAN_POINT('Ctrl Pts',(36.5158634381635,-12.75,-9.73250950575603));
#69695=CARTESIAN_POINT('Ctrl Pts',(36.5129271579462,-12.75,-9.78883778500213));
#69696=CARTESIAN_POINT('Ctrl Pts',(36.5117889942815,-12.75,-9.84524193459141));
#69697=CARTESIAN_POINT('Ctrl Pts',(36.5115191770569,-12.75,-9.85861330776889));
#69698=CARTESIAN_POINT('Ctrl Pts',(36.5113505718752,-12.75,-9.87198485331457));
#69699=CARTESIAN_POINT('Ctrl Pts',(36.5112834643196,-12.75,-9.88534723852641));
#69700=CARTESIAN_POINT('Ctrl Pts',(36.5108085549604,-12.75,-9.97991068595048));
#69701=CARTESIAN_POINT('Ctrl Pts',(36.5154106260062,-12.75,-10.074134730613));
#69702=CARTESIAN_POINT('Ctrl Pts',(36.5251526597289,-12.75,-10.1676019130765));
#69703=CARTESIAN_POINT('Ctrl Pts',(36.529414730784,-12.75,-10.2084931462955));
#69704=CARTESIAN_POINT('Ctrl Pts',(36.5346611529582,-12.75,-10.2492398965073));
#69705=CARTESIAN_POINT('Ctrl Pts',(36.5408999787326,-12.75,-10.2898086508596));
#69706=CARTESIAN_POINT('Ctrl Pts',(36.5547918865281,-12.75,-10.3801425398342));
#69707=CARTESIAN_POINT('Ctrl Pts',(36.5736003964838,-12.75,-10.4695937030868));
#69708=CARTESIAN_POINT('Ctrl Pts',(36.5970362254893,-12.75,-10.5579348213263));
#69709=CARTESIAN_POINT('Ctrl Pts',(36.6204720544947,-12.75,-10.6462759395658));
#69710=CARTESIAN_POINT('Ctrl Pts',(36.6485355160504,-12.75,-10.7335076916399));
#69711=CARTESIAN_POINT('Ctrl Pts',(36.6809898727762,-12.75,-10.8194022563315));
#69712=CARTESIAN_POINT('Ctrl Pts',(36.6899298075195,-12.75,-10.8430629256718));
#69713=CARTESIAN_POINT('Ctrl Pts',(36.699203211383,-12.75,-10.8666220939594));
#69714=CARTESIAN_POINT('Ctrl Pts',(36.7088057864774,-12.75,-10.8900748849566));
#69715=CARTESIAN_POINT('Ctrl Pts',(36.7144182844112,-12.75,-10.903782535219));
#69716=CARTESIAN_POINT('Ctrl Pts',(36.7201400708447,-12.75,-10.9174460470224));
#69717=CARTESIAN_POINT('Ctrl Pts',(36.725968063952,-12.75,-10.9310603421251));
#69718=CARTESIAN_POINT('Ctrl Pts',(36.7632844244424,-12.75,-11.0182320210414));
#69719=CARTESIAN_POINT('Ctrl Pts',(36.8049729222028,-12.75,-11.1034402117559));
#69720=CARTESIAN_POINT('Ctrl Pts',(36.8507031457334,-12.75,-11.186447825772));
#69721=CARTESIAN_POINT('Ctrl Pts',(36.897242032023,-12.75,-11.2709232910466));
#69722=CARTESIAN_POINT('Ctrl Pts',(36.9479670801348,-12.75,-11.3531203940572));
#69723=CARTESIAN_POINT('Ctrl Pts',(37.0025849524151,-12.75,-11.4327882625403));
#69724=CARTESIAN_POINT('Ctrl Pts',(37.0579909527395,-12.75,-11.5136057269111));
#69725=CARTESIAN_POINT('Ctrl Pts',(37.1174032465806,-12.75,-11.5918212706129));
#69726=CARTESIAN_POINT('Ctrl Pts',(37.1805674478662,-12.75,-11.667160078329));
#69727=CARTESIAN_POINT('Ctrl Pts',(37.2181975830789,-12.75,-11.71204324733));
#69728=CARTESIAN_POINT('Ctrl Pts',(37.2571603082924,-12.75,-11.755905103373));
#69729=CARTESIAN_POINT('Ctrl Pts',(37.2974096407888,-12.75,-11.7986835008897));
#69730=CARTESIAN_POINT('Ctrl Pts',(37.3076886400212,-12.75,-11.8096083805825));
#69731=CARTESIAN_POINT('Ctrl Pts',(37.3180531561345,-12.75,-11.8204642006903));
#69732=CARTESIAN_POINT('Ctrl Pts',(37.3284973899992,-12.75,-11.831244642987));
#69733=CARTESIAN_POINT('Ctrl Pts',(37.399176916415,-12.75,-11.9041994011775));
#69734=CARTESIAN_POINT('Ctrl Pts',(37.4733055554982,-12.75,-11.9735015455736));
#69735=CARTESIAN_POINT('Ctrl Pts',(37.5505563567699,-12.75,-12.0388871187713));
#69736=CARTESIAN_POINT('Ctrl Pts',(37.6282447166439,-12.75,-12.1046430443735));
#69737=CARTESIAN_POINT('Ctrl Pts',(37.7090911707722,-12.75,-12.1664387621244));
#69738=CARTESIAN_POINT('Ctrl Pts',(37.7928131421831,-12.75,-12.2239879195989));
#69739=CARTESIAN_POINT('Ctrl Pts',(37.8752801154996,-12.75,-12.2806744112551));
#69740=CARTESIAN_POINT('Ctrl Pts',(37.9605376456359,-12.75,-12.333241449453));
#69741=CARTESIAN_POINT('Ctrl Pts',(38.0483558365738,-12.75,-12.3813862473665));
#69742=CARTESIAN_POINT('Ctrl Pts',(38.1254402939299,-12.75,-12.4236464622724));
#69743=CARTESIAN_POINT('Ctrl Pts',(38.2044985066156,-12.75,-12.462499334437));
#69744=CARTESIAN_POINT('Ctrl Pts',(38.2853957334118,-12.75,-12.4977141955524));
#69745=CARTESIAN_POINT('Origin',(39.2,-12.75,-9.525));
#69746=CARTESIAN_POINT('Ctrl Pts',(38.1090601293427,6.10939317307034,-7.3859991646148));
#69747=CARTESIAN_POINT('Ctrl Pts',(37.4014250801391,6.04252457258368,-7.74690939722429));
#69748=CARTESIAN_POINT('Ctrl Pts',(36.3842966957365,5.90878737161036,-9.2198489270829));
#69749=CARTESIAN_POINT('Ctrl Pts',(37.4068122137656,5.70818157015037,-11.7207065033657));
#69750=CARTESIAN_POINT('Ctrl Pts',(40.0578012994608,5.5075757686904,-12.224479871604));
#69751=CARTESIAN_POINT('Ctrl Pts',(41.9297097031944,5.3069699672304,-10.2834563771707));
#69752=CARTESIAN_POINT('Ctrl Pts',(41.3270630938264,5.10636416577043,-7.6531776804645));
#69753=CARTESIAN_POINT('Ctrl Pts',(38.7953478358015,4.90575836431044,-6.72097002802451));
#69754=CARTESIAN_POINT('Ctrl Pts',(36.6307235789104,4.70515256285046,-8.33095570597218));
#69755=CARTESIAN_POINT('Ctrl Pts',(36.795736350814,4.50454676139048,-11.0238574475027));
#69756=CARTESIAN_POINT('Ctrl Pts',(39.1408882915444,4.3039409599305,-12.3575487902617));
#69757=CARTESIAN_POINT('Ctrl Pts',(41.5396181212764,4.10333515847052,-11.12284467284));
#69758=CARTESIAN_POINT('Ctrl Pts',(41.8168821219755,3.90272935701054,-8.43924848869504));
#69759=CARTESIAN_POINT('Ctrl Pts',(39.7212505068437,3.70212355555055,-6.74018448494738));
#69760=CARTESIAN_POINT('Ctrl Pts',(37.1529716231046,3.50151775409057,-7.5662788780741));
#69761=CARTESIAN_POINT('Ctrl Pts',(36.4408591567146,3.30091195263059,-10.1684711251898));
#69762=CARTESIAN_POINT('Ctrl Pts',(38.2306320743938,3.10030615117061,-12.1871862476963));
#69763=CARTESIAN_POINT('Ctrl Pts',(40.8993907810134,2.89970034971063,-11.7919324649524));
#69764=CARTESIAN_POINT('Ctrl Pts',(42.0272063778795,2.69909454825064,-9.34110954729177));
#69765=CARTESIAN_POINT('Ctrl Pts',(40.5914180124664,2.49848874679066,-7.05703178483132));
#69766=CARTESIAN_POINT('Ctrl Pts',(37.8939444502983,2.29788294533068,-7.01081417098301));
#69767=CARTESIAN_POINT('Ctrl Pts',(36.3807526568316,2.0972771438707,-9.24436527970491));
#69768=CARTESIAN_POINT('Ctrl Pts',(37.4239477837834,1.89667134241071,-11.7323853104763));
#69769=CARTESIAN_POINT('Ctrl Pts',(40.0775999080307,1.69606554095074,-12.218831810624));
#69770=CARTESIAN_POINT('Ctrl Pts',(41.9354776177662,1.49545973949075,-10.262613459155));
#69771=CARTESIAN_POINT('Ctrl Pts',(41.3129276391037,1.29485393803077,-7.63755511343507));
#69772=CARTESIAN_POINT('Ctrl Pts',(38.7744547594159,1.09424813657079,-6.72396043203959));
#69773=CARTESIAN_POINT('Ctrl Pts',(36.6218502152785,0.893642335110802,-8.35024253613623));
#69774=CARTESIAN_POINT('Ctrl Pts',(36.8070144268541,0.693036533650818,-11.0417502950991));
#69775=CARTESIAN_POINT('Ctrl Pts',(39.1620474870164,0.492430732190839,-12.3579262289002));
#69776=CARTESIAN_POINT('Ctrl Pts',(41.5514944511869,0.291824930730855,-11.1053117595593));
#69777=CARTESIAN_POINT('Ctrl Pts',(41.8086951473945,0.0912191292708744,
-8.41973033186413));
#69778=CARTESIAN_POINT('Ctrl Pts',(39.7004297080759,-0.109386672189109,
-6.7363656534607));
#69779=CARTESIAN_POINT('Ctrl Pts',(37.1383935286702,-0.30999247364909,-7.5816291736382));
#69780=CARTESIAN_POINT('Ctrl Pts',(36.4457441565455,-0.510598275109072,
-10.1890678882323));
#69781=CARTESIAN_POINT('Ctrl Pts',(38.2505498560931,-0.711204076569056,
-12.1943549474788));
#69782=CARTESIAN_POINT('Ctrl Pts',(40.9162810513022,-0.911809878029036,
-11.7791718577627));
#69783=CARTESIAN_POINT('Ctrl Pts',(42.0257534747706,-1.11241567948902,-9.31999094846492));
#69784=CARTESIAN_POINT('Ctrl Pts',(40.572939477521,-1.313021480949,-7.04670449654313));
#69785=CARTESIAN_POINT('Ctrl Pts',(37.8751958672925,-1.51362728240898,-7.02064271292006));
#69786=CARTESIAN_POINT('Ctrl Pts',(36.378734559167,-1.71423308386896,-9.26543743769494));
#69787=CARTESIAN_POINT('Ctrl Pts',(37.4404900922592,-1.91483888532894,-11.7455936809672));
#69788=CARTESIAN_POINT('Ctrl Pts',(40.0977026898037,-2.11544468678892,-12.2121995259207));
#69789=CARTESIAN_POINT('Ctrl Pts',(41.9409124267084,-2.3160504882489,-10.242154432814));
#69790=CARTESIAN_POINT('Ctrl Pts',(41.2987663977842,-2.51665628970889,-7.6218208127131));
#69791=CARTESIAN_POINT('Ctrl Pts',(38.7535383451392,-2.71726209116887,-6.72721812820788));
#69792=CARTESIAN_POINT('Ctrl Pts',(36.6131448422295,-2.91786789262886,-8.36953827233206));
#69793=CARTESIAN_POINT('Ctrl Pts',(36.8184137979523,-3.11847369408883,-11.0595874278143));
#69794=CARTESIAN_POINT('Ctrl Pts',(39.1832150836397,-3.31907949554882,-12.3581307202409));
#69795=CARTESIAN_POINT('Ctrl Pts',(41.5632362969134,-3.5196852970088,-11.0876981846604));
#69796=CARTESIAN_POINT('Ctrl Pts',(41.8003641804634,-3.72029109846878,-8.4002700144691));
#69797=CARTESIAN_POINT('Ctrl Pts',(39.6795801343239,-3.92089689992876,-6.73270447370779));
#69798=CARTESIAN_POINT('Ctrl Pts',(37.1239309533467,-4.12150270138875,-7.59708695089287));
#69799=CARTESIAN_POINT('Ctrl Pts',(36.4507826961788,-4.32210850284872,-10.2096280944859));
#69800=CARTESIAN_POINT('Ctrl Pts',(38.2705207534323,-4.52271430430871,-12.2013743649926));
#69801=CARTESIAN_POINT('Ctrl Pts',(40.9330754516574,-4.72332010576869,-11.7662855441136));
#69802=CARTESIAN_POINT('Ctrl Pts',(42.0241428508277,-4.92392590722868,-9.29888372568953));
#69803=CARTESIAN_POINT('Ctrl Pts',(40.5543842821803,-5.12453170868865,-7.03651559627705));
#69804=CARTESIAN_POINT('Ctrl Pts',(37.8565212501926,-5.32513751014864,-7.03061104472332));
#69805=CARTESIAN_POINT('Ctrl Pts',(36.3768739570832,-5.52574331160863,-9.28652409515082));
#69806=CARTESIAN_POINT('Ctrl Pts',(37.457130628819,-5.72634911306861,-11.7586780802944));
#69807=CARTESIAN_POINT('Ctrl Pts',(40.1177553555661,-5.92695491452858,-12.2054172284784));
#69808=CARTESIAN_POINT('Ctrl Pts',(41.9461942224683,-6.12756071598857,-10.2216553695093));
#69809=CARTESIAN_POINT('Ctrl Pts',(41.2844879908318,-6.32816651744855,-7.60619275917001));
#69810=CARTESIAN_POINT('Ctrl Pts',(38.7326468550866,-6.52877231890854,-6.73063201253607));
#69811=CARTESIAN_POINT('Ctrl Pts',(36.6045838824426,-6.72937812036851,-8.38889851330806));
#69812=CARTESIAN_POINT('Ctrl Pts',(36.8299461230947,-6.9299839218285,-11.077338890813));
#69813=CARTESIAN_POINT('Ctrl Pts',(39.2043836172943,-7.13058972328848,-12.3581770498033));
#69814=CARTESIAN_POINT('Ctrl Pts',(41.5748462129954,-7.33119552474845,-11.0699973707383));
#69815=CARTESIAN_POINT('Ctrl Pts',(41.7918880461159,-7.53180132620844,-8.38087248623012));
#69816=CARTESIAN_POINT('Ctrl Pts',(39.6587037874852,-7.73240712766843,-6.72919917583345));
#69817=CARTESIAN_POINT('Ctrl Pts',(37.1095842765501,-7.93301292912841,-7.6126523561178));
#69818=CARTESIAN_POINT('Ctrl Pts',(36.4559747126355,-8.13361873058839,-10.2301500795792));
#69819=CARTESIAN_POINT('Ctrl Pts',(38.2905435407064,-8.33422453204837,-12.2082443741029));
#69820=CARTESIAN_POINT('Ctrl Pts',(40.9497730997094,-8.53483033350836,-11.7532741041371));
#69821=CARTESIAN_POINT('Ctrl Pts',(42.0223745705614,-8.73543613496833,-9.27778913525879));
#69822=CARTESIAN_POINT('Ctrl Pts',(40.5357534698105,-8.93604193642833,-7.02646559967134));
#69823=CARTESIAN_POINT('Ctrl Pts',(37.8379216484013,-9.13664773788829,-7.04071866315316));
#69824=CARTESIAN_POINT('Ctrl Pts',(36.3751709299713,-9.33725353934829,-9.30762399663186));
#69825=CARTESIAN_POINT('Ctrl Pts',(37.4738685180293,-9.53785934080825,-11.7716379179115));
#69826=CARTESIAN_POINT('Ctrl Pts',(40.1377566782039,-9.73846514226827,-12.1984850299003));
#69827=CARTESIAN_POINT('Ctrl Pts',(41.9513229223509,-9.93907094372821,-10.2011179327488));
#69828=CARTESIAN_POINT('Ctrl Pts',(41.2700927993691,-10.1396767451883,-7.59067081103199));
#69829=CARTESIAN_POINT('Ctrl Pts',(38.7117822700447,-10.3402825466482,-6.73420387847481));
#69830=CARTESIAN_POINT('Ctrl Pts',(36.596166219581,-10.5408883481082,-8.40831829576861));
#69831=CARTESIAN_POINT('Ctrl Pts',(36.8416138787086,-10.7414941495682,-11.095011291306));
#69832=CARTESIAN_POINT('Ctrl Pts',(39.225545799572,-10.9420999510282,-12.3580503446663));
#69833=CARTESIAN_POINT('Ctrl Pts',(41.5863355026778,-11.1427057524881,-11.0522394086686));
#69834=CARTESIAN_POINT('Ctrl Pts',(41.7832438274538,-11.3433115539481,-8.36148187294322));
#69835=CARTESIAN_POINT('Ctrl Pts',(39.6378476098593,-11.5439173554081,-6.72596142787065));
#69836=CARTESIAN_POINT('Ctrl Pts',(37.095264708429,-11.7445231568681,-7.62810634102885));
#69837=CARTESIAN_POINT('Ctrl Pts',(36.4614952627569,-11.9451289583281,-10.2510598762372));
#69838=CARTESIAN_POINT('Ctrl Pts',(38.3102738378103,-12.1457347597881,-12.2141266245507));
#69839=CARTESIAN_POINT('Ctrl Pts',(40.9670458444618,-12.346340561248,-11.741799149493));
#69840=CARTESIAN_POINT('Ctrl Pts',(42.0192942539946,-12.5469793475859,-9.25282332578296));
#69841=CARTESIAN_POINT('Ctrl Pts',(41.0190233754115,-12.6807495334372,-7.76761236952371));
#69842=CARTESIAN_POINT('Ctrl Pts',(40.3151665400905,-12.7476511188018,-7.39852924898774));
#69843=CARTESIAN_POINT('Ctrl Pts',(38.0010709531129,5.97216720292314,-7.17426527865005));
#69844=CARTESIAN_POINT('Ctrl Pts',(37.2233890314003,5.90529860243647,-7.57090103542516));
#69845=CARTESIAN_POINT('Ctrl Pts',(36.1055778694168,5.77156140146314,-9.1896428507662));
#69846=CARTESIAN_POINT('Ctrl Pts',(37.2293094227601,5.57095560000318,-11.9380535294654));
#69847=CARTESIAN_POINT('Ctrl Pts',(40.1427127214274,5.37034979854318,-12.4916940558357));
#69848=CARTESIAN_POINT('Ctrl Pts',(42.1999162563905,5.16974399708322,-10.3585339149708));
#69849=CARTESIAN_POINT('Ctrl Pts',(41.5376152951616,4.96913819562322,-7.46789107047617));
#69850=CARTESIAN_POINT('Ctrl Pts',(38.7552924165738,4.76853239416325,-6.44340671317846));
#69851=CARTESIAN_POINT('Ctrl Pts',(36.3763978807827,4.56792659270326,-8.21276050276974));
#69852=CARTESIAN_POINT('Ctrl Pts',(36.5577448190182,4.36732079124328,-11.1722252772934));
#69853=CARTESIAN_POINT('Ctrl Pts',(39.1350369839945,4.1667149897833,-12.6379351055101));
#69854=CARTESIAN_POINT('Ctrl Pts',(41.7712105677572,3.96610918832332,-11.281010979347));
#69855=CARTESIAN_POINT('Ctrl Pts',(42.0759201791991,3.76550338686334,-8.33177289407273));
#69856=CARTESIAN_POINT('Ctrl Pts',(39.7728476794813,3.56489758540335,-6.46452315703079));
#69857=CARTESIAN_POINT('Ctrl Pts',(36.9503418411289,3.36429178394337,-7.37239039154066));
#69858=CARTESIAN_POINT('Ctrl Pts',(36.1677392948574,3.16368598248338,-10.232166585046));
#69859=CARTESIAN_POINT('Ctrl Pts',(38.1346769749741,2.96308018102341,-12.450708837338));
#69860=CARTESIAN_POINT('Ctrl Pts',(41.067608861102,2.76247437956342,-12.0163299556329));
#69861=CARTESIAN_POINT('Ctrl Pts',(42.3070638622291,2.56186857810344,-9.32290673058429));
#69862=CARTESIAN_POINT('Ctrl Pts',(40.7291507042482,2.36126277664346,-6.81273431098717));
#69863=CARTESIAN_POINT('Ctrl Pts',(37.7646615569729,2.16065697518348,-6.76194174101064));
#69864=CARTESIAN_POINT('Ctrl Pts',(36.1016830157217,1.9600511737235,-9.21658601057989));
#69865=CARTESIAN_POINT('Ctrl Pts',(37.2481411963361,1.75944537226351,-11.9508883899875));
#69866=CARTESIAN_POINT('Ctrl Pts',(40.1644711405125,1.55883957080353,-12.485486908632));
#69867=CARTESIAN_POINT('Ctrl Pts',(42.2062551211676,1.35823376934355,-10.3356278130829));
#69868=CARTESIAN_POINT('Ctrl Pts',(41.5220806101492,1.15762796788356,-7.45072206794696));
#69869=CARTESIAN_POINT('Ctrl Pts',(38.7323311912751,0.957022166423585,-6.44669312916898));
#69870=CARTESIAN_POINT('Ctrl Pts',(36.3666461669734,0.7564163649636,-8.2339564838939));
#69871=CARTESIAN_POINT('Ctrl Pts',(36.5701392811891,0.555810563503619,-11.1918892892999));
#69872=CARTESIAN_POINT('Ctrl Pts',(39.1582906707855,0.355204762043637,-12.6383499057747));
#69873=CARTESIAN_POINT('Ctrl Pts',(41.784262503325,0.154598960583655,-11.2617425305772));
#69874=CARTESIAN_POINT('Ctrl Pts',(42.0669227982292,-0.0460068408763262,
-8.31032268788294));
#69875=CARTESIAN_POINT('Ctrl Pts',(39.7499658863656,-0.246612642336309,
-6.46032630978219));
#69876=CARTESIAN_POINT('Ctrl Pts',(36.9343207007013,-0.44721844379629,-7.38926017119132));
#69877=CARTESIAN_POINT('Ctrl Pts',(36.1731078475604,-0.647824245256273,
-10.2548021657482));
#69878=CARTESIAN_POINT('Ctrl Pts',(38.1565663638131,-0.848430046716256,
-12.4585871472511));
#69879=CARTESIAN_POINT('Ctrl Pts',(41.0861710533949,-1.04903584817623,-12.0023062105786));
#69880=CARTESIAN_POINT('Ctrl Pts',(42.3054671401856,-1.24964164963622,-9.29969765899009));
#69881=CARTESIAN_POINT('Ctrl Pts',(40.7088430292921,-1.4502474510962,-6.80138475246677));
#69882=CARTESIAN_POINT('Ctrl Pts',(37.7440571026318,-1.65085325255618,-6.77274318363257));
#69883=CARTESIAN_POINT('Ctrl Pts',(36.0994651520476,-1.85145905401616,-9.23974404428493));
#69884=CARTESIAN_POINT('Ctrl Pts',(37.2663209830207,-2.05206485547615,-11.9654042212166));
#69885=CARTESIAN_POINT('Ctrl Pts',(40.1865638420804,-2.25267065693612,-12.4781981120706));
#69886=CARTESIAN_POINT('Ctrl Pts',(42.2122279070932,-2.45327645839611,-10.3131436032643));
#69887=CARTESIAN_POINT('Ctrl Pts',(41.5065175859948,-2.65388225985609,-7.43343027151031));
#69888=CARTESIAN_POINT('Ctrl Pts',(38.7093443179308,-2.85448806131607,-6.45027329583733));
#69889=CARTESIAN_POINT('Ctrl Pts',(36.3570790726787,-3.05509386277605,-8.25516225263374));
#69890=CARTESIAN_POINT('Ctrl Pts',(36.5826670450864,-3.25569966423604,-11.2114920713602));
#69891=CARTESIAN_POINT('Ctrl Pts',(39.181553590335,-3.45630546569602,-12.6385746391581));
#69892=CARTESIAN_POINT('Ctrl Pts',(41.7971666424844,-3.656911267156,-11.2423854357145));
#69893=CARTESIAN_POINT('Ctrl Pts',(42.0577671714977,-3.85751706861598,-8.28893604649776));
#69894=CARTESIAN_POINT('Ctrl Pts',(39.727052469908,-4.05812287007596,-6.45630271978454));
#69895=CARTESIAN_POINT('Ctrl Pts',(36.9184265143081,-4.25872867153595,-7.40624807185329));
#69896=CARTESIAN_POINT('Ctrl Pts',(36.1786451385538,-4.45933447299593,-10.277397571004));
#69897=CARTESIAN_POINT('Ctrl Pts',(38.1785141260651,-4.65994027445591,-12.4663013978492));
#69898=CARTESIAN_POINT('Ctrl Pts',(41.1046278858496,-4.8605460759159,-11.9881443157238));
#69899=CARTESIAN_POINT('Ctrl Pts',(42.3036970849511,-5.06115187737588,-9.27650108953178));
#69900=CARTESIAN_POINT('Ctrl Pts',(40.6884511055362,-5.26175767883585,-6.79018728062308));
#69901=CARTESIAN_POINT('Ctrl Pts',(37.7235339358813,-5.46236348029585,-6.78369825354006));
#69902=CARTESIAN_POINT('Ctrl Pts',(36.0974203740146,-5.66296928175581,-9.26291801271858));
#69903=CARTESIAN_POINT('Ctrl Pts',(37.2846087211206,-5.86357508321581,-11.9797838097131));
#69904=CARTESIAN_POINT('Ctrl Pts',(40.2086014667897,-6.06418088467578,-12.4707444534163));
#69905=CARTESIAN_POINT('Ctrl Pts',(42.2180325334768,-6.26478668613577,-10.2906153933317));
#69906=CARTESIAN_POINT('Ctrl Pts',(41.4908257982998,-6.46539248759575,-7.41625523937237));
#69907=CARTESIAN_POINT('Ctrl Pts',(38.6863848359917,-6.66599828905573,-6.45402511130751));
#69908=CARTESIAN_POINT('Ctrl Pts',(36.347670686723,-6.86660409051572,-8.27643891130687));
#69909=CARTESIAN_POINT('Ctrl Pts',(36.5953409237878,-7.06720989197569,-11.2310007034914));
#69910=CARTESIAN_POINT('Ctrl Pts',(39.2048175396701,-7.26781569343568,-12.6386255547581));
#69911=CARTESIAN_POINT('Ctrl Pts',(41.8099257926419,-7.46842149489566,-11.2229324662745));
#69912=CARTESIAN_POINT('Ctrl Pts',(42.0484520076212,-7.66902729635564,-8.26761840959673));
#69913=CARTESIAN_POINT('Ctrl Pts',(39.7041096301685,-7.86963309781562,-6.45245044198942));
#69914=CARTESIAN_POINT('Ctrl Pts',(36.9026596989223,-8.07023889927561,-7.42335425428616));
#69915=CARTESIAN_POINT('Ctrl Pts',(36.1843510986247,-8.27084470073558,-10.2999509716909));
#69916=CARTESIAN_POINT('Ctrl Pts',(38.2005189146958,-8.47145050219558,-12.4738514505113));
#69917=CARTESIAN_POINT('Ctrl Pts',(41.1229783887533,-8.67205630365554,-11.9738449086261));
#69918=CARTESIAN_POINT('Ctrl Pts',(42.3017537674215,-8.87266210511554,-9.25331840285964));
#69919=CARTESIAN_POINT('Ctrl Pts',(40.6679760796267,-9.07326790657551,-6.77914246213601));
#69920=CARTESIAN_POINT('Ctrl Pts',(37.7030932100009,-9.2738737080355,-6.79480639767921));
#69921=CARTESIAN_POINT('Ctrl Pts',(36.0955487688721,-9.47447950949547,-9.28610653616747));
#69922=CARTESIAN_POINT('Ctrl Pts',(37.3030034485457,-9.67508531095546,-11.9940265064739));
#69923=CARTESIAN_POINT('Ctrl Pts',(40.2305826660579,-9.87569111241545,-12.4631260553198));
#69924=CARTESIAN_POINT('Ctrl Pts',(42.2236689094381,-10.0762969138754,-10.2680450114592));
#69925=CARTESIAN_POINT('Ctrl Pts',(41.4750056659128,-10.2769027153354,-7.39919681572548));
#69926=CARTESIAN_POINT('Ctrl Pts',(38.6634549223176,-10.4775085167954,-6.457950546559));
#69927=CARTESIAN_POINT('Ctrl Pts',(36.338419782266,-10.6781143182554,-8.29778100531444));
#69928=CARTESIAN_POINT('Ctrl Pts',(36.6081636388556,-10.8787201197154,-11.2504224469341));
#69929=CARTESIAN_POINT('Ctrl Pts',(39.2280745089226,-11.0793259211754,-12.6384863074236));
#69930=CARTESIAN_POINT('Ctrl Pts',(41.8225523759202,-11.2799317226353,-11.203416691747));
#69931=CARTESIAN_POINT('Ctrl Pts',(42.0389521212201,-11.4805375240954,-8.24630837214011));
#69932=CARTESIAN_POINT('Ctrl Pts',(39.6811889561377,-11.6811433255553,-6.44889219814528));
#69933=CARTESIAN_POINT('Ctrl Pts',(36.886922675626,-11.8817491270153,-7.44033798721073));
#69934=CARTESIAN_POINT('Ctrl Pts',(36.1904181130162,-12.0823549284753,-10.3229305723563));
#69935=CARTESIAN_POINT('Ctrl Pts',(38.2222022603483,-12.2829607299353,-12.4803159689624));
#69936=CARTESIAN_POINT('Ctrl Pts',(41.1419609156184,-12.4835665313952,-11.9612340793728));
#69937=CARTESIAN_POINT('Ctrl Pts',(42.2983685386799,-12.6842053177331,-9.22588129567827));
#69938=CARTESIAN_POINT('Ctrl Pts',(41.1990835612539,-12.8179755035844,-7.59365333875032));
#69939=CARTESIAN_POINT('Ctrl Pts',(40.4255538485596,-12.884877088949,-7.18803568205975));
#69940=CARTESIAN_POINT('Ctrl Pts',(37.8930817768831,5.83494123277593,-6.9625313926853));
#69941=CARTESIAN_POINT('Ctrl Pts',(37.0453529826617,5.76807263228927,-7.39489267362603));
#69942=CARTESIAN_POINT('Ctrl Pts',(35.826859043097,5.63433543131595,-9.15943677444951));
#69943=CARTESIAN_POINT('Ctrl Pts',(37.0518066317547,5.43372962985597,-12.155400555565));
#69944=CARTESIAN_POINT('Ctrl Pts',(40.227624143394,5.23312382839599,-12.7589082400674));
#69945=CARTESIAN_POINT('Ctrl Pts',(42.4701228095865,5.03251802693601,-10.433611452771));
#69946=CARTESIAN_POINT('Ctrl Pts',(41.7481674964967,4.83191222547602,-7.28260446048784));
#69947=CARTESIAN_POINT('Ctrl Pts',(38.7152369973462,4.63130642401604,-6.16584339833242));
#69948=CARTESIAN_POINT('Ctrl Pts',(36.1220721826552,4.43070062255606,-8.09456529956729));
#69949=CARTESIAN_POINT('Ctrl Pts',(36.3197532872223,4.23009482109608,-11.3205931070843));
#69950=CARTESIAN_POINT('Ctrl Pts',(39.1291856764446,4.02948901963609,-12.9183214207584));
#69951=CARTESIAN_POINT('Ctrl Pts',(42.0028030142381,3.82888321817611,-11.4391772858541));
#69952=CARTESIAN_POINT('Ctrl Pts',(42.3349582364225,3.62827741671613,-8.22429729945043));
#69953=CARTESIAN_POINT('Ctrl Pts',(39.8244448521188,3.42767161525615,-6.18886182911421));
#69954=CARTESIAN_POINT('Ctrl Pts',(36.7477120591531,3.22706581379617,-7.17850190500721));
#69955=CARTESIAN_POINT('Ctrl Pts',(35.8946194330003,3.02646001233618,-10.2958620449021));
#69956=CARTESIAN_POINT('Ctrl Pts',(38.0387218755544,2.8258542108762,-12.7142314269797));
#69957=CARTESIAN_POINT('Ctrl Pts',(41.2358269411907,2.62524840941622,-12.2407274463135));
#69958=CARTESIAN_POINT('Ctrl Pts',(42.5869213465787,2.42464260795624,-9.30470391387682));
#69959=CARTESIAN_POINT('Ctrl Pts',(40.8668833960298,2.22403680649626,-6.56843683714305));
#69960=CARTESIAN_POINT('Ctrl Pts',(37.6353786636475,2.02343100503627,-6.51306931103826));
#69961=CARTESIAN_POINT('Ctrl Pts',(35.8226133746117,1.82282520357629,-9.18880674145491));
#69962=CARTESIAN_POINT('Ctrl Pts',(37.0723346088889,1.62221940211631,-12.1693914694987));
#69963=CARTESIAN_POINT('Ctrl Pts',(40.2513423729944,1.42161360065633,-12.75214200664));
#69964=CARTESIAN_POINT('Ctrl Pts',(42.4770326245692,1.22100779919635,-10.4086421670107));
#69965=CARTESIAN_POINT('Ctrl Pts',(41.7312335811948,1.02040199773636,-7.26388902245885));
#69966=CARTESIAN_POINT('Ctrl Pts',(38.6902076231343,0.819796196276384,-6.16942582629837));
#69967=CARTESIAN_POINT('Ctrl Pts',(36.1114421186684,0.6191903948164,-8.11767043165157));
#69968=CARTESIAN_POINT('Ctrl Pts',(36.3332641355238,0.418584593356419,-11.3420282835007));
#69969=CARTESIAN_POINT('Ctrl Pts',(39.1545338545546,0.217978791896437,-12.9187735826493));
#69970=CARTESIAN_POINT('Ctrl Pts',(42.0170305554631,0.0173729904364543,
-11.4181733015951));
#69971=CARTESIAN_POINT('Ctrl Pts',(42.325150449064,-0.183232811023527,-8.20091504390175));
#69972=CARTESIAN_POINT('Ctrl Pts',(39.7995020646551,-0.383838612483509,
-6.1842869661037));
#69973=CARTESIAN_POINT('Ctrl Pts',(36.7302478727325,-0.584444413943491,
-7.19689116874442));
#69974=CARTESIAN_POINT('Ctrl Pts',(35.9004715385751,-0.785050215403473,
-10.320536443264));
#69975=CARTESIAN_POINT('Ctrl Pts',(38.0625828715332,-0.985656016863457,
-12.7228193470235));
#69976=CARTESIAN_POINT('Ctrl Pts',(41.2560610554877,-1.18626181832344,-12.2254405633946));
#69977=CARTESIAN_POINT('Ctrl Pts',(42.5851808056007,-1.38686761978342,-9.27940436951522));
#69978=CARTESIAN_POINT('Ctrl Pts',(40.844746581063,-1.5874734212434,-6.55606500839041));
#69979=CARTESIAN_POINT('Ctrl Pts',(37.6129183379714,-1.78807922270338,-6.52484365434506));
#69980=CARTESIAN_POINT('Ctrl Pts',(35.8201957449284,-1.98868502416336,-9.21405065087494));
#69981=CARTESIAN_POINT('Ctrl Pts',(37.0921518737822,-2.18929082562335,-12.185214761466));
#69982=CARTESIAN_POINT('Ctrl Pts',(40.2754249943571,-2.38989662708333,-12.7441966982204));
#69983=CARTESIAN_POINT('Ctrl Pts',(42.4835433874781,-2.59050242854331,-10.3841327737147));
#69984=CARTESIAN_POINT('Ctrl Pts',(41.7142687742056,-2.79110823000329,-7.24503973030753));
#69985=CARTESIAN_POINT('Ctrl Pts',(38.6651502907223,-2.99171403146327,-6.17332846346677));
#69986=CARTESIAN_POINT('Ctrl Pts',(36.1010133031279,-3.19231983292326,-8.14078623293544));
#69987=CARTESIAN_POINT('Ctrl Pts',(36.3469202922205,-3.39292563438324,-11.3633967149062));
#69988=CARTESIAN_POINT('Ctrl Pts',(39.1798920970303,-3.59353143584322,-12.9190185580753));
#69989=CARTESIAN_POINT('Ctrl Pts',(42.0310969880554,-3.79413723730321,-11.3970726867687));
#69990=CARTESIAN_POINT('Ctrl Pts',(42.3151701625321,-3.99474303876318,-8.17760207852641));
#69991=CARTESIAN_POINT('Ctrl Pts',(39.774524805492,-4.19534884022317,-6.17990096586128));
#69992=CARTESIAN_POINT('Ctrl Pts',(36.7129220752694,-4.39595464168314,-7.21540919281373));
#69993=CARTESIAN_POINT('Ctrl Pts',(35.9065075809288,-4.59656044314314,-10.3451670475223));
#69994=CARTESIAN_POINT('Ctrl Pts',(38.0865074986978,-4.79716624460311,-12.7312284307056));
#69995=CARTESIAN_POINT('Ctrl Pts',(41.2761803200418,-4.9977720460631,-12.210003087334));
#69996=CARTESIAN_POINT('Ctrl Pts',(42.5832513190743,-5.19837784752307,-9.25411845337402));
#69997=CARTESIAN_POINT('Ctrl Pts',(40.822517928892,-5.39898364898306,-6.54385896496911));
#69998=CARTESIAN_POINT('Ctrl Pts',(37.5905466215699,-5.59958945044304,-6.53678546235682));
#69999=CARTESIAN_POINT('Ctrl Pts',(35.817966790946,-5.80019525190303,-9.23931193028633));
#70000=CARTESIAN_POINT('Ctrl Pts',(37.1120868134222,-6.000801053363,-12.2008895391316));
#70001=CARTESIAN_POINT('Ctrl Pts',(40.2994475780133,-6.20140685482298,-12.7360716783542));
#70002=CARTESIAN_POINT('Ctrl Pts',(42.4898708444855,-6.40201265628298,-10.3595754171542));
#70003=CARTESIAN_POINT('Ctrl Pts',(41.6971636057678,-6.60261845774295,-7.22631771957472));
#70004=CARTESIAN_POINT('Ctrl Pts',(38.640122816897,-6.80322425920293,-6.17741821007895));
#70005=CARTESIAN_POINT('Ctrl Pts',(36.0907574910032,-7.00383006066292,-8.16397930930566));
#70006=CARTESIAN_POINT('Ctrl Pts',(36.3607357244811,-7.20443586212289,-11.3846625161698));
#70007=CARTESIAN_POINT('Ctrl Pts',(39.2052514620458,-7.40504166358289,-12.919074059713));
#70008=CARTESIAN_POINT('Ctrl Pts',(42.0450053722886,-7.60564746504285,-11.3758675618108));
#70009=CARTESIAN_POINT('Ctrl Pts',(42.3050159691265,-7.80625326650285,-8.15436433296333));
#70010=CARTESIAN_POINT('Ctrl Pts',(39.7495154728519,-8.00685906796282,-6.17570170814539));
#70011=CARTESIAN_POINT('Ctrl Pts',(36.6957351212943,-8.20746486942281,-7.2340561524545));
#70012=CARTESIAN_POINT('Ctrl Pts',(35.9127274846142,-8.40807067088279,-10.3697518638027));
#70013=CARTESIAN_POINT('Ctrl Pts',(38.1104942886851,-8.60867647234277,-12.7394585269196));
#70014=CARTESIAN_POINT('Ctrl Pts',(41.2961836777971,-8.80928227380275,-12.1944157131151));
#70015=CARTESIAN_POINT('Ctrl Pts',(42.5811329642816,-9.00988807526274,-9.22884767046046));
#70016=CARTESIAN_POINT('Ctrl Pts',(40.800198689443,-9.21049387672271,-6.5318193246007));
#70017=CARTESIAN_POINT('Ctrl Pts',(37.5682647716004,-9.4110996781827,-6.54889413220524));
#70018=CARTESIAN_POINT('Ctrl Pts',(35.815926607773,-9.61170547964268,-9.26458907570309));
#70019=CARTESIAN_POINT('Ctrl Pts',(37.132138379062,-9.81231128110266,-12.2164150950363));
#70020=CARTESIAN_POINT('Ctrl Pts',(40.323408653912,-10.0129170825627,-12.7277670807392));
#70021=CARTESIAN_POINT('Ctrl Pts',(42.4960148965253,-10.2135228840226,-10.3349720901695));
#70022=CARTESIAN_POINT('Ctrl Pts',(41.6799185324564,-10.4141286854826,-7.20772282041896));
#70023=CARTESIAN_POINT('Ctrl Pts',(38.6151275745906,-10.6147344869426,-6.1816972146432));
#70024=CARTESIAN_POINT('Ctrl Pts',(36.080673344951,-10.8153402884026,-8.18724371486027));
#70025=CARTESIAN_POINT('Ctrl Pts',(36.3747133990027,-11.0159460898626,-11.4058336025622));
#70026=CARTESIAN_POINT('Ctrl Pts',(39.2306032182732,-11.2165518913226,-12.9189222701809));
#70027=CARTESIAN_POINT('Ctrl Pts',(42.0587692491625,-11.4171576927825,-11.3545939748253));
#70028=CARTESIAN_POINT('Ctrl Pts',(42.2946604149865,-11.6177634942425,-8.131134871337));
#70029=CARTESIAN_POINT('Ctrl Pts',(39.7245303024159,-11.8183692957025,-6.1718229684199));
#70030=CARTESIAN_POINT('Ctrl Pts',(36.678580642823,-12.0189750971625,-7.2525696333926));
#70031=CARTESIAN_POINT('Ctrl Pts',(35.9193409632754,-12.2195808986225,-10.3948012684755));
#70032=CARTESIAN_POINT('Ctrl Pts',(38.1341306828862,-12.4201867000825,-12.7465053133741));
#70033=CARTESIAN_POINT('Ctrl Pts',(41.3168759867752,-12.6207925015424,-12.1806690092526));
#70034=CARTESIAN_POINT('Ctrl Pts',(42.5774428233651,-12.8214312878803,-9.19893926557358));
#70035=CARTESIAN_POINT('Ctrl Pts',(41.3791437470964,-12.9552014737316,-7.41969430797695));
#70036=CARTESIAN_POINT('Ctrl Pts',(40.5359411570286,-13.0221030590962,-6.97754211513178));
#70037=CARTESIAN_POINT('Ctrl Pts',(37.7850926006533,5.69771526262873,-6.75079750672056));
#70038=CARTESIAN_POINT('Ctrl Pts',(36.8673169339229,5.63084666214207,-7.2188843118269));
#70039=CARTESIAN_POINT('Ctrl Pts',(35.5481402167774,5.49710946116874,-9.12923069813283));
#70040=CARTESIAN_POINT('Ctrl Pts',(36.8743038407491,5.29650365970877,-12.3727475816646));
#70041=CARTESIAN_POINT('Ctrl Pts',(40.3125355653607,5.09589785824878,-13.0261224242991));
#70042=CARTESIAN_POINT('Ctrl Pts',(42.7403293627825,4.89529205678881,-10.5086889905711));
#70043=CARTESIAN_POINT('Ctrl Pts',(41.9587196978319,4.69468625532882,-7.09731785049951));
#70044=CARTESIAN_POINT('Ctrl Pts',(38.6751815781184,4.49408045386884,-5.88828008348638));
#70045=CARTESIAN_POINT('Ctrl Pts',(35.8677464845275,4.29347465240886,-7.97637009636483));
#70046=CARTESIAN_POINT('Ctrl Pts',(36.0817617554265,4.09286885094887,-11.468960936875));
#70047=CARTESIAN_POINT('Ctrl Pts',(39.1233343688946,3.89226304948889,-13.1987077360068));
#70048=CARTESIAN_POINT('Ctrl Pts',(42.2343954607189,3.69165724802891,-11.5973435923613));
#70049=CARTESIAN_POINT('Ctrl Pts',(42.5939962936459,3.49105144656893,-8.11682170482813));
#70050=CARTESIAN_POINT('Ctrl Pts',(39.8760420247564,3.29044564510895,-5.91320050119763));
#70051=CARTESIAN_POINT('Ctrl Pts',(36.5450822771773,3.08983984364896,-6.98461341847376));
#70052=CARTESIAN_POINT('Ctrl Pts',(35.6214995711431,2.88923404218898,-10.3595575047582));
#70053=CARTESIAN_POINT('Ctrl Pts',(37.9427667761347,2.688628240729,-12.9777540166216));
#70054=CARTESIAN_POINT('Ctrl Pts',(41.4040450212794,2.48802243926902,-12.465124936994));
#70055=CARTESIAN_POINT('Ctrl Pts',(42.8667788309283,2.28741663780904,-9.28650109716934));
#70056=CARTESIAN_POINT('Ctrl Pts',(41.0046160878115,2.08681083634905,-6.32413936329892));
#70057=CARTESIAN_POINT('Ctrl Pts',(37.506095770322,1.88620503488907,-6.26419688106589));
#70058=CARTESIAN_POINT('Ctrl Pts',(35.5435437335017,1.68559923342909,-9.1610274723299));
#70059=CARTESIAN_POINT('Ctrl Pts',(36.8965280214417,1.48499343196911,-12.3878945490098));
#70060=CARTESIAN_POINT('Ctrl Pts',(40.3382136054761,1.28438763050913,-13.018797104648));
#70061=CARTESIAN_POINT('Ctrl Pts',(42.7478101279706,1.08378182904914,-10.4816565209386));
#70062=CARTESIAN_POINT('Ctrl Pts',(41.9403865522403,0.883176027589163,-7.07705597697076));
#70063=CARTESIAN_POINT('Ctrl Pts',(38.6480840549934,0.682570226129183,-5.89215852342776));
#70064=CARTESIAN_POINT('Ctrl Pts',(35.8562380703633,0.481964424669198,-8.00138437940923));
#70065=CARTESIAN_POINT('Ctrl Pts',(36.0963889898587,0.281358623209219,-11.4921672777015));
#70066=CARTESIAN_POINT('Ctrl Pts',(39.1507770383239,0.0807528217492357,
-13.1991972595238));
#70067=CARTESIAN_POINT('Ctrl Pts',(42.249798607601,-0.119852979710745,-11.5746040726131));
#70068=CARTESIAN_POINT('Ctrl Pts',(42.5833780998989,-0.320458781170727,
-8.09150739992054));
#70069=CARTESIAN_POINT('Ctrl Pts',(39.8490382429447,-0.52106458263071,-5.90824762242522));
#70070=CARTESIAN_POINT('Ctrl Pts',(36.5261750447638,-0.721670384090691,
-7.00452216629751));
#70071=CARTESIAN_POINT('Ctrl Pts',(35.6278352295899,-0.922276185550674,
-10.3862707207798));
#70072=CARTESIAN_POINT('Ctrl Pts',(37.9685993792531,-1.12288198701066,-12.9870515467959));
#70073=CARTESIAN_POINT('Ctrl Pts',(41.4259510575803,-1.32348778847064,-12.4485749162106));
#70074=CARTESIAN_POINT('Ctrl Pts',(42.8648944710158,-1.52409358993062,-9.25911108004038));
#70075=CARTESIAN_POINT('Ctrl Pts',(40.980650132834,-1.72469939139061,-6.31074526431405));
#70076=CARTESIAN_POINT('Ctrl Pts',(37.4817795733109,-1.92530519285059,-6.27694412505756));
#70077=CARTESIAN_POINT('Ctrl Pts',(35.5409263378092,-2.12591099431056,-9.18835725746494));
#70078=CARTESIAN_POINT('Ctrl Pts',(36.9179827645437,-2.32651679577055,-12.4050253017153));
#70079=CARTESIAN_POINT('Ctrl Pts',(40.3642861466337,-2.52712259723053,-13.0101952843703));
#70080=CARTESIAN_POINT('Ctrl Pts',(42.7548588678629,-2.72772839869051,-10.455121944165));
#70081=CARTESIAN_POINT('Ctrl Pts',(41.9220199624163,-2.92833420015049,-7.05664918910476));
#70082=CARTESIAN_POINT('Ctrl Pts',(38.6209562635138,-3.12894000161048,-5.8963836310962));
#70083=CARTESIAN_POINT('Ctrl Pts',(35.8449475335771,-3.32954580307046,-8.02641021323713));
#70084=CARTESIAN_POINT('Ctrl Pts',(36.1111735393545,-3.53015160453044,-11.5153013584522));
#70085=CARTESIAN_POINT('Ctrl Pts',(39.1782306037257,-3.73075740599042,-13.1994624769925));
#70086=CARTESIAN_POINT('Ctrl Pts',(42.2650273336264,-3.93136320745041,-11.5517599378228));
#70087=CARTESIAN_POINT('Ctrl Pts',(42.5725731535664,-4.13196900891039,-8.06626811055506));
#70088=CARTESIAN_POINT('Ctrl Pts',(39.8219971410761,-4.33257481037037,-5.90349921193802));
#70089=CARTESIAN_POINT('Ctrl Pts',(36.5074176362308,-4.53318061183036,-7.02457031377417));
#70090=CARTESIAN_POINT('Ctrl Pts',(35.6343700233036,-4.73378641329033,-10.4129365240405));
#70091=CARTESIAN_POINT('Ctrl Pts',(37.9945008713306,-4.93439221475032,-12.9961554635622));
#70092=CARTESIAN_POINT('Ctrl Pts',(41.447732754234,-5.1349980162103,-12.4318618589442));
#70093=CARTESIAN_POINT('Ctrl Pts',(42.8628055531978,-5.33560381767028,-9.23173581721625));
#70094=CARTESIAN_POINT('Ctrl Pts',(40.9565847522478,-5.53620961913025,-6.29753064931515));
#70095=CARTESIAN_POINT('Ctrl Pts',(37.4575593072585,-5.73681542059025,-6.28987267117355));
#70096=CARTESIAN_POINT('Ctrl Pts',(35.5385132078774,-5.93742122205023,-9.2157058478541));
#70097=CARTESIAN_POINT('Ctrl Pts',(36.9395649057238,-6.13802702351021,-12.4219952685503));
#70098=CARTESIAN_POINT('Ctrl Pts',(40.3902936892369,-6.33863282497019,-13.0013989032921));
#70099=CARTESIAN_POINT('Ctrl Pts',(42.7617091554941,-6.53923862643018,-10.4285354409766));
#70100=CARTESIAN_POINT('Ctrl Pts',(41.9035014132359,-6.73984442789015,-7.03638019977707));
#70101=CARTESIAN_POINT('Ctrl Pts',(38.5938607978023,-6.94045022935015,-5.90081130885039));
#70102=CARTESIAN_POINT('Ctrl Pts',(35.8338442952836,-7.14105603081011,-8.05151970730447));
#70103=CARTESIAN_POINT('Ctrl Pts',(36.1261305251742,-7.3416618322701,-11.5383243288482));
#70104=CARTESIAN_POINT('Ctrl Pts',(39.2056853844216,-7.54226763373008,-13.1995225646678));
#70105=CARTESIAN_POINT('Ctrl Pts',(42.2800849519353,-7.74287343519007,-11.5288026573471));
#70106=CARTESIAN_POINT('Ctrl Pts',(42.561579930632,-7.94347923665003,-8.04111025632993));
#70107=CARTESIAN_POINT('Ctrl Pts',(39.7949213155352,-8.14408503811002,-5.89895297430136));
#70108=CARTESIAN_POINT('Ctrl Pts',(36.4888105436665,-8.34469083957002,-7.04475805062286));
#70109=CARTESIAN_POINT('Ctrl Pts',(35.6411038706034,-8.54529664102998,-10.4395527559144));
#70110=CARTESIAN_POINT('Ctrl Pts',(38.0204696626744,-8.74590244248998,-13.005065603328));
#70111=CARTESIAN_POINT('Ctrl Pts',(41.469388966841,-8.94650824394996,-12.4149865176041));
#70112=CARTESIAN_POINT('Ctrl Pts',(42.8605121611417,-9.14711404540993,-9.20437693806131));
#70113=CARTESIAN_POINT('Ctrl Pts',(40.9324212992594,-9.34771984686993,-6.28449618706538));
#70114=CARTESIAN_POINT('Ctrl Pts',(37.4334363331999,-9.5483256483299,-6.30298186673129));
#70115=CARTESIAN_POINT('Ctrl Pts',(35.5363044466738,-9.74893144978988,-9.2430716152387));
#70116=CARTESIAN_POINT('Ctrl Pts',(36.9612733095783,-9.94953725124986,-12.4388036835987));
#70117=CARTESIAN_POINT('Ctrl Pts',(40.4162346417662,-10.1501430527099,-12.9924081061586));
#70118=CARTESIAN_POINT('Ctrl Pts',(42.7683608836124,-10.3507488541699,-10.4018991688799));
#70119=CARTESIAN_POINT('Ctrl Pts',(41.8848313990001,-10.5513546556298,-7.01624882511245));
#70120=CARTESIAN_POINT('Ctrl Pts',(38.5668002268634,-10.7519604570898,-5.9054438827274));
#70121=CARTESIAN_POINT('Ctrl Pts',(35.822926907636,-10.9525662585498,-8.0767064244061));
#70122=CARTESIAN_POINT('Ctrl Pts',(36.1412631591497,-11.1531720600098,-11.5612447581902));
#70123=CARTESIAN_POINT('Ctrl Pts',(39.2331319276237,-11.3537778614698,-13.1993582329382));
#70124=CARTESIAN_POINT('Ctrl Pts',(42.294986122405,-11.5543836629298,-11.5057712579037));
#70125=CARTESIAN_POINT('Ctrl Pts',(42.5503687087529,-11.7549894643897,-8.0159613705339));
#70126=CARTESIAN_POINT('Ctrl Pts',(39.7678716486943,-11.9555952658497,-5.89475373869452));
#70127=CARTESIAN_POINT('Ctrl Pts',(36.47023861002,-12.1562010673097,-7.06480127957447));
#70128=CARTESIAN_POINT('Ctrl Pts',(35.6482638135347,-12.3568068687697,-10.4666719645947));
#70129=CARTESIAN_POINT('Ctrl Pts',(38.0460591054243,-12.5574126702297,-13.0126946577859));
#70130=CARTESIAN_POINT('Ctrl Pts',(41.4917910579318,-12.7580184716896,-12.4001039391323));
#70131=CARTESIAN_POINT('Ctrl Pts',(42.8565171080503,-12.9586572580275,-9.17199723546892));
#70132=CARTESIAN_POINT('Ctrl Pts',(41.5592039329389,-13.0924274438788,-7.24573527720356));
#70133=CARTESIAN_POINT('Ctrl Pts',(40.6463284654976,-13.1593290292434,-6.76704854820381));
#70134=CARTESIAN_POINT('Ctrl Pts',(41.0695067500478,-12.75,-12.0106538705994));
#70135=CARTESIAN_POINT('Ctrl Pts',(41.0824973530166,-12.75,-12.0007220309186));
#70136=CARTESIAN_POINT('Ctrl Pts',(41.0954879559853,-12.75,-11.9907901912378));
#70137=CARTESIAN_POINT('Ctrl Pts',(41.1084785589541,-12.75,-11.9808583515571));
#70138=CARTESIAN_POINT('Ctrl Pts',(37.728785320723,5.69999999999999,-11.4333446637284));
#70139=CARTESIAN_POINT('Ctrl Pts',(37.7087477093809,5.7,-11.4221525029985));
#70140=CARTESIAN_POINT('Ctrl Pts',(37.6888978346145,5.69999999999999,-11.4106547954623));
#70141=CARTESIAN_POINT('Ctrl Pts',(37.6692433579699,5.69999999999999,-11.398853237781));
#70142=CARTESIAN_POINT('Ctrl Pts',(37.5993515170885,5.69999999999998,-11.3568865852708));
#70143=CARTESIAN_POINT('Ctrl Pts',(37.5319297638091,5.70000000000001,-11.3110817734132));
#70144=CARTESIAN_POINT('Ctrl Pts',(37.4670658763312,5.70000000000001,-11.261804086503));
#70145=CARTESIAN_POINT('Ctrl Pts',(37.4252790635777,5.70000000000002,-11.2300582637362));
#70146=CARTESIAN_POINT('Ctrl Pts',(37.3845539662202,5.69999999999999,-11.1968700068083));
#70147=CARTESIAN_POINT('Ctrl Pts',(37.3449168132708,5.69999999999999,-11.1623261463859));
#70148=CARTESIAN_POINT('Ctrl Pts',(37.3249009813365,5.69999999999999,-11.1448823076354));
#70149=CARTESIAN_POINT('Ctrl Pts',(37.3051626180758,5.69999999999999,-11.1270926610294));
#70150=CARTESIAN_POINT('Ctrl Pts',(37.2857053911122,5.7,-11.1089676468229));
#70151=CARTESIAN_POINT('Ctrl Pts',(37.2676753613394,5.70000000000001,-11.0921721113448));
#70152=CARTESIAN_POINT('Ctrl Pts',(37.2498826753603,5.69999999999999,-11.0750843516763));
#70153=CARTESIAN_POINT('Ctrl Pts',(37.2323538947033,5.69999999999999,-11.0577362182599));
#70154=CARTESIAN_POINT('Ctrl Pts',(37.1711091481097,5.7,-10.9971226447461));
#70155=CARTESIAN_POINT('Ctrl Pts',(37.1130372095074,5.7,-10.9332931219723));
#70156=CARTESIAN_POINT('Ctrl Pts',(37.0582414952906,5.69999999999999,-10.8666339257479));
#70157=CARTESIAN_POINT('Ctrl Pts',(37.0110924346456,5.69999999999999,-10.809276912882));
#70158=CARTESIAN_POINT('Ctrl Pts',(36.9663690199974,5.7,-10.7498237353702));
#70159=CARTESIAN_POINT('Ctrl Pts',(36.9241497379828,5.69999999999999,-10.6884923583133));
#70160=CARTESIAN_POINT('Ctrl Pts',(36.9110147566815,5.69999999999998,-10.6694113495329));
#70161=CARTESIAN_POINT('Ctrl Pts',(36.8981222563253,5.7,-10.650148377145));
#70162=CARTESIAN_POINT('Ctrl Pts',(36.8854748972125,5.70000000000001,-10.6307095675714));
#70163=CARTESIAN_POINT('Ctrl Pts',(36.8750183316657,5.70000000000001,-10.6146379762895));
#70164=CARTESIAN_POINT('Ctrl Pts',(36.8647282092343,5.69999999999999,-10.5984441400613));
#70165=CARTESIAN_POINT('Ctrl Pts',(36.8546183260729,5.7,-10.5821517814802));
#70166=CARTESIAN_POINT('Ctrl Pts',(36.8071375712008,5.70000000000002,-10.5056352212263));
#70167=CARTESIAN_POINT('Ctrl Pts',(36.7635688418601,5.7,-10.4268571011546));
#70168=CARTESIAN_POINT('Ctrl Pts',(36.7240163215064,5.70000000000001,-10.346221435102));
#70169=CARTESIAN_POINT('Ctrl Pts',(36.6838955920464,5.70000000000001,-10.2644273619659));
#70170=CARTESIAN_POINT('Ctrl Pts',(36.6479066092487,5.7,-10.1807213198273));
#70171=CARTESIAN_POINT('Ctrl Pts',(36.6161866100473,5.7,-10.0954787389638));
#70172=CARTESIAN_POINT('Ctrl Pts',(36.584458411875,5.70000000000001,-10.010214124637));
#70173=CARTESIAN_POINT('Ctrl Pts',(36.557000760613,5.70000000000001,-9.92341135179696));
#70174=CARTESIAN_POINT('Ctrl Pts',(36.5339892249958,5.70000000000001,-9.83541163480388));
#70175=CARTESIAN_POINT('Ctrl Pts',(36.5199184927481,5.70000000000001,-9.78160295048657));
#70176=CARTESIAN_POINT('Ctrl Pts',(36.5075108969285,5.7,-9.72734611867408));
#70177=CARTESIAN_POINT('Ctrl Pts',(36.4968152084323,5.70000000000001,-9.67271484734734));
#70178=CARTESIAN_POINT('Ctrl Pts',(36.4942456073919,5.70000000000001,-9.65958987912383));
#70179=CARTESIAN_POINT('Ctrl Pts',(36.4917756758722,5.69999999999998,-9.64644730221114));
#70180=CARTESIAN_POINT('Ctrl Pts',(36.4894073031302,5.69999999999998,-9.63329626042469));
#70181=CARTESIAN_POINT('Ctrl Pts',(36.4726467923812,5.7,-9.54022890944844));
#70182=CARTESIAN_POINT('Ctrl Pts',(36.4609458027478,5.70000000000002,-9.4466211194787));
#70183=CARTESIAN_POINT('Ctrl Pts',(36.4544382976075,5.70000000000002,-9.35287324812201));
#70184=CARTESIAN_POINT('Ctrl Pts',(36.4515913175639,5.70000000000002,-9.31185932448558));
#70185=CARTESIAN_POINT('Ctrl Pts',(36.4497388534778,5.7,-9.27081811781351));
#70186=CARTESIAN_POINT('Ctrl Pts',(36.448894611127,5.7,-9.22978125151666));
#70187=CARTESIAN_POINT('Ctrl Pts',(36.4470147422982,5.70000000000001,-9.13840473420257));
#70188=CARTESIAN_POINT('Ctrl Pts',(36.4501300278111,5.7,-9.04705059907772));
#70189=CARTESIAN_POINT('Ctrl Pts',(36.457994679238,5.7,-8.95599261583192));
#70190=CARTESIAN_POINT('Ctrl Pts',(36.4658593306648,5.7,-8.86493463258612));
#70191=CARTESIAN_POINT('Ctrl Pts',(36.4784735398518,5.70000000000001,-8.77417207849568));
#70192=CARTESIAN_POINT('Ctrl Pts',(36.4956433647121,5.69999999999999,-8.68397016390274));
#70193=CARTESIAN_POINT('Ctrl Pts',(36.5003730644743,5.69999999999998,-8.65912262017583));
#70194=CARTESIAN_POINT('Ctrl Pts',(36.5054487442588,5.69999999999998,-8.63431760414533));
#70195=CARTESIAN_POINT('Ctrl Pts',(36.5108670105061,5.69999999999998,-8.60956066002757));
#70196=CARTESIAN_POINT('Ctrl Pts',(36.514033736065,5.69999999999998,-8.59509137333682));
#70197=CARTESIAN_POINT('Ctrl Pts',(36.5173157137729,5.69999999999999,-8.58064673454195));
#70198=CARTESIAN_POINT('Ctrl Pts',(36.5207107833831,5.69999999999999,-8.5662322749048));
#70199=CARTESIAN_POINT('Ctrl Pts',(36.5424498539559,5.69999999999998,-8.47393462233966));
#70200=CARTESIAN_POINT('Ctrl Pts',(36.5688339721789,5.70000000000001,-8.38281777898905));
#70201=CARTESIAN_POINT('Ctrl Pts',(36.5995785196194,5.7,-8.29317222432108));
#70202=CARTESIAN_POINT('Ctrl Pts',(36.6308667367852,5.69999999999999,-8.20194142680089));
#70203=CARTESIAN_POINT('Ctrl Pts',(36.6666710622638,5.7,-8.11223365464869));
#70204=CARTESIAN_POINT('Ctrl Pts',(36.706745771912,5.70000000000001,-8.02434657747373));
#70205=CARTESIAN_POINT('Ctrl Pts',(36.7473987381782,5.70000000000002,-7.93519133679955));
#70206=CARTESIAN_POINT('Ctrl Pts',(36.7924463811748,5.69999999999998,-7.84790883854002));
#70207=CARTESIAN_POINT('Ctrl Pts',(36.8416854714683,5.69999999999999,-7.76281362595471));
#70208=CARTESIAN_POINT('Ctrl Pts',(36.8710196912118,5.69999999999999,-7.71211809827107));
#70209=CARTESIAN_POINT('Ctrl Pts',(36.90184253833,5.70000000000001,-7.6621990125104));
#70210=CARTESIAN_POINT('Ctrl Pts',(36.9341194258415,5.70000000000001,-7.61312550909832));
#70211=CARTESIAN_POINT('Ctrl Pts',(36.9423623839345,5.70000000000002,-7.60059298619142));
#70212=CARTESIAN_POINT('Ctrl Pts',(36.950701478377,5.69999999999998,-7.58811375585398));
#70213=CARTESIAN_POINT('Ctrl Pts',(36.9591320851161,5.69999999999998,-7.57569504140518));
#70214=CARTESIAN_POINT('Ctrl Pts',(37.0161848823531,5.7,-7.49165335623092));
#70215=CARTESIAN_POINT('Ctrl Pts',(37.0772645446978,5.7,-7.4106154107815));
#70216=CARTESIAN_POINT('Ctrl Pts',(37.1420944926193,5.7,-7.33289755586651));
#70217=CARTESIAN_POINT('Ctrl Pts',(37.2072916133539,5.69999999999999,-7.25473953580667));
#70218=CARTESIAN_POINT('Ctrl Pts',(37.2762819290764,5.70000000000001,-7.17993839635292));
#70219=CARTESIAN_POINT('Ctrl Pts',(37.3488364291232,5.7,-7.10882490265184));
#70220=CARTESIAN_POINT('Ctrl Pts',(37.420303235415,5.69999999999999,-7.03877749999878));
#70221=CARTESIAN_POINT('Ctrl Pts',(37.4952286266382,5.69999999999999,-6.97230716483109));
#70222=CARTESIAN_POINT('Ctrl Pts',(37.5734383173599,5.7,-6.90975177261387));
#70223=CARTESIAN_POINT('Ctrl Pts',(37.642088746257,5.70000000000001,-6.85484227909835));
#70224=CARTESIAN_POINT('Ctrl Pts',(37.713270487887,5.70000000000001,-6.80294912851935));
#70225=CARTESIAN_POINT('Ctrl Pts',(37.7868905613917,5.7,-6.75432276015121));
#70226=CARTESIAN_POINT('Origin',(39.2,5.7,-9.525));
#70227=CARTESIAN_POINT('',(40.6568071307763,5.7,-6.77704737365809));
#70228=CARTESIAN_POINT('',(39.2,5.7,-12.63523));
#70229=CARTESIAN_POINT('Origin',(39.2,5.7,-9.525));
#70230=CARTESIAN_POINT('Ctrl Pts',(40.6568071307763,5.70000000000001,-6.77704737365808));
#70231=CARTESIAN_POINT('Ctrl Pts',(40.6675536326424,5.70000000000001,-6.78439681724126));
#70232=CARTESIAN_POINT('Ctrl Pts',(40.6782480875051,5.70000000000001,-6.79181954081017));
#70233=CARTESIAN_POINT('Ctrl Pts',(40.6888896732699,5.7,-6.79931561182634));
#70234=CARTESIAN_POINT('Ctrl Pts',(40.7723747072434,5.7,-6.85812355241729));
#70235=CARTESIAN_POINT('Ctrl Pts',(40.8526093240026,5.69999999999999,-6.92144304811511));
#70236=CARTESIAN_POINT('Ctrl Pts',(40.9294099877629,5.7,-6.98888738755383));
#70237=CARTESIAN_POINT('Ctrl Pts',(41.0059278390579,5.7,-7.05608336846313));
#70238=CARTESIAN_POINT('Ctrl Pts',(41.0790373165767,5.7,-7.12737486738236));
#70239=CARTESIAN_POINT('Ctrl Pts',(41.1485115022755,5.70000000000001,-7.2024036428382));
#70240=CARTESIAN_POINT('Ctrl Pts',(41.1673345977946,5.70000000000001,-7.22273167968936));
#70241=CARTESIAN_POINT('Ctrl Pts',(41.1858945771364,5.70000000000001,-7.24333894727815));
#70242=CARTESIAN_POINT('Ctrl Pts',(41.2041638506315,5.70000000000001,-7.26419219781226));
#70243=CARTESIAN_POINT('Ctrl Pts',(41.2706073697102,5.69999999999999,-7.3400333827441));
#70244=CARTESIAN_POINT('Ctrl Pts',(41.3332586489075,5.70000000000002,-7.41917632680374));
#70245=CARTESIAN_POINT('Ctrl Pts',(41.3919233565839,5.70000000000001,-7.50125544373537));
#70246=CARTESIAN_POINT('Ctrl Pts',(41.4388414115273,5.7,-7.5668995536343));
#70247=CARTESIAN_POINT('Ctrl Pts',(41.483208740423,5.70000000000001,-7.63442243831006));
#70248=CARTESIAN_POINT('Ctrl Pts',(41.5249027839362,5.70000000000002,-7.70364346292023));
#70249=CARTESIAN_POINT('Ctrl Pts',(41.5463341925284,5.70000000000002,-7.73922418228907));
#70250=CARTESIAN_POINT('Ctrl Pts',(41.5670589402089,5.70000000000001,-7.77525362777195));
#70251=CARTESIAN_POINT('Ctrl Pts',(41.5870581128508,5.70000000000002,-7.81170739628005));
#70252=CARTESIAN_POINT('Ctrl Pts',(41.5951145473919,5.70000000000002,-7.82639237375482));
#70253=CARTESIAN_POINT('Ctrl Pts',(41.6030535695938,5.70000000000002,-7.84114703580276));
#70254=CARTESIAN_POINT('Ctrl Pts',(41.6108663637285,5.70000000000002,-7.85595507323248));
#70255=CARTESIAN_POINT('Ctrl Pts',(41.6565060237786,5.70000000000002,-7.94245854211309));
#70256=CARTESIAN_POINT('Ctrl Pts',(41.697906904009,5.70000000000002,-8.03089833473493));
#70257=CARTESIAN_POINT('Ctrl Pts',(41.734896049887,5.70000000000001,-8.12093975713746));
#70258=CARTESIAN_POINT('Ctrl Pts',(41.7714636499846,5.70000000000001,-8.20995502495378));
#70259=CARTESIAN_POINT('Ctrl Pts',(41.8037196667702,5.69999999999999,-8.30053652523976));
#70260=CARTESIAN_POINT('Ctrl Pts',(41.8314470651491,5.7,-8.39236717500651));
#70261=CARTESIAN_POINT('Ctrl Pts',(41.8583795823913,5.70000000000002,-8.4815652499361));
#70262=CARTESIAN_POINT('Ctrl Pts',(41.8810393953456,5.70000000000003,-8.57194261465344));
#70263=CARTESIAN_POINT('Ctrl Pts',(41.8991793540274,5.70000000000002,-8.66320276814808));
#70264=CARTESIAN_POINT('Ctrl Pts',(41.9098047963858,5.70000000000002,-8.71665820967326));
#70265=CARTESIAN_POINT('Ctrl Pts',(41.9188785638188,5.70000000000001,-8.7704163693359));
#70266=CARTESIAN_POINT('Ctrl Pts',(41.926342968605,5.70000000000001,-8.82441520057859));
#70267=CARTESIAN_POINT('Ctrl Pts',(41.9289015008942,5.70000000000001,-8.84292407801371));
#70268=CARTESIAN_POINT('Ctrl Pts',(41.9312709007728,5.7,-8.86146121090835));
#70269=CARTESIAN_POINT('Ctrl Pts',(41.9334486793056,5.70000000000001,-8.88002403124186));
#70270=CARTESIAN_POINT('Ctrl Pts',(41.9350635864279,5.70000000000002,-8.89378908141335));
#70271=CARTESIAN_POINT('Ctrl Pts',(41.9365720127068,5.70000000000003,-8.90755883338214));
#70272=CARTESIAN_POINT('Ctrl Pts',(41.9379732767689,5.70000000000002,-8.92133132839933));
#70273=CARTESIAN_POINT('Ctrl Pts',(41.9471904729052,5.70000000000001,-9.01192366662318));
#70274=CARTESIAN_POINT('Ctrl Pts',(41.9517768375676,5.70000000000004,-9.10264924907603));
#70275=CARTESIAN_POINT('Ctrl Pts',(41.9515425093424,5.70000000000001,-9.19322849973003));
#70276=CARTESIAN_POINT('Ctrl Pts',(41.9514418239969,5.7,-9.23214828045617));
#70277=CARTESIAN_POINT('Ctrl Pts',(41.9504504972526,5.70000000000003,-9.27104096258455));
#70278=CARTESIAN_POINT('Ctrl Pts',(41.9485505426635,5.70000000000003,-9.30988376714684));
#70279=CARTESIAN_POINT('Ctrl Pts',(41.9439536835233,5.70000000000002,-9.40386227706026));
#70280=CARTESIAN_POINT('Ctrl Pts',(41.9340411346708,5.70000000000004,-9.49755072743953));
#70281=CARTESIAN_POINT('Ctrl Pts',(41.9190010975822,5.70000000000003,-9.59059001157079));
#70282=CARTESIAN_POINT('Ctrl Pts',(41.9039610604935,5.70000000000001,-9.68362929570204));
#70283=CARTESIAN_POINT('Ctrl Pts',(41.8837928305745,5.7,-9.77602030848649));
#70284=CARTESIAN_POINT('Ctrl Pts',(41.85864192099,5.70000000000002,-9.86736982038934));
#70285=CARTESIAN_POINT('Ctrl Pts',(41.8537552257159,5.70000000000003,-9.88511857124902));
#70286=CARTESIAN_POINT('Ctrl Pts',(41.8486803209392,5.70000000000003,-9.90282787810892));
#70287=CARTESIAN_POINT('Ctrl Pts',(41.8434181219726,5.7,-9.92049466307744));
#70288=CARTESIAN_POINT('Ctrl Pts',(41.8394338258671,5.69999999999999,-9.93387114370734));
#70289=CARTESIAN_POINT('Ctrl Pts',(41.8353447148482,5.70000000000001,-9.9472146109527));
#70290=CARTESIAN_POINT('Ctrl Pts',(41.8311523643973,5.70000000000001,-9.96052145256901));
#70291=CARTESIAN_POINT('Ctrl Pts',(41.804022806364,5.70000000000001,-10.0466327488685));
#70292=CARTESIAN_POINT('Ctrl Pts',(41.7725634087528,5.70000000000001,-10.1312469744334));
#70293=CARTESIAN_POINT('Ctrl Pts',(41.7369695874477,5.70000000000001,-10.2140570115954));
#70294=CARTESIAN_POINT('Ctrl Pts',(41.7014462364436,5.70000000000001,-10.2967030975987));
#70295=CARTESIAN_POINT('Ctrl Pts',(41.6618041288342,5.70000000000002,-10.3775528985299));
#70296=CARTESIAN_POINT('Ctrl Pts',(41.6181978547607,5.70000000000001,-10.4562680583345));
#70297=CARTESIAN_POINT('Ctrl Pts',(41.5754612696166,5.69999999999999,-10.5334133132456));
#70298=CARTESIAN_POINT('Ctrl Pts',(41.5289163600446,5.70000000000001,-10.6085087758867));
#70299=CARTESIAN_POINT('Ctrl Pts',(41.4786809385008,5.70000000000001,-10.6811946178604));
#70300=CARTESIAN_POINT('Ctrl Pts',(41.4633843153438,5.70000000000001,-10.703327366016));
#70301=CARTESIAN_POINT('Ctrl Pts',(41.447745351846,5.70000000000001,-10.7252363699564));
#70302=CARTESIAN_POINT('Ctrl Pts',(41.431766999022,5.70000000000001,-10.7469105719195));
#70303=CARTESIAN_POINT('Ctrl Pts',(41.4181638265902,5.70000000000001,-10.7653629061416));
#70304=CARTESIAN_POINT('Ctrl Pts',(41.4043146626224,5.70000000000001,-10.7836450498864));
#70305=CARTESIAN_POINT('Ctrl Pts',(41.3902212496529,5.7,-10.801749916543));
#70306=CARTESIAN_POINT('Ctrl Pts',(41.3820353977903,5.69999999999999,-10.8122657338801));
#70307=CARTESIAN_POINT('Ctrl Pts',(41.3737678280459,5.70000000000001,-10.8227207590788));
#70308=CARTESIAN_POINT('Ctrl Pts',(41.3654268033884,5.70000000000001,-10.833104081773));
#70309=CARTESIAN_POINT('Ctrl Pts',(41.3116872772203,5.70000000000001,-10.9000017189995));
#70310=CARTESIAN_POINT('Ctrl Pts',(41.254815874147,5.69999999999999,-10.964036668235));
#70311=CARTESIAN_POINT('Ctrl Pts',(41.1949561042646,5.69999999999999,-11.0249156502104));
#70312=CARTESIAN_POINT('Ctrl Pts',(41.1360360400568,5.7,-11.0848389264599));
#70313=CARTESIAN_POINT('Ctrl Pts',(41.0742200470205,5.70000000000001,-11.141705013839));
#70314=CARTESIAN_POINT('Ctrl Pts',(41.0096218112891,5.7,-11.1951903084968));
#70315=CARTESIAN_POINT('Ctrl Pts',(40.9469513398941,5.7,-11.2470794752977));
#70316=CARTESIAN_POINT('Ctrl Pts',(40.8816616316492,5.70000000000001,-11.2957868641724));
#70317=CARTESIAN_POINT('Ctrl Pts',(40.8138434619797,5.69999999999999,-11.3409703464158));
#70318=CARTESIAN_POINT('Ctrl Pts',(40.766577340876,5.69999999999998,-11.3724611394292));
#70319=CARTESIAN_POINT('Ctrl Pts',(40.7180827620352,5.7,-11.4022392586719));
#70320=CARTESIAN_POINT('Ctrl Pts',(40.6683886799114,5.7,-11.4301739104629));
#70321=CARTESIAN_POINT('Origin',(39.2,5.7,-9.525));
#70322=CARTESIAN_POINT('Ctrl Pts',(41.099774813423,6.10922971516948,-11.9923764941264));
#70323=CARTESIAN_POINT('Ctrl Pts',(41.9164782428699,6.04232813665392,-11.3635994721406));
#70324=CARTESIAN_POINT('Ctrl Pts',(42.8624587143743,5.90855795765171,-9.24274905943794));
#70325=CARTESIAN_POINT('Ctrl Pts',(40.9620531289813,5.70791917816281,-6.29820309169915));
#70326=CARTESIAN_POINT('Ctrl Pts',(37.4625022647654,5.50731337670284,-6.28846198413748));
#70327=CARTESIAN_POINT('Ctrl Pts',(35.5393356313202,5.30670757524286,-9.20937120381493));
#70328=CARTESIAN_POINT('Ctrl Pts',(36.9350656861766,5.10610177378287,-12.4185714191142));
#70329=CARTESIAN_POINT('Ctrl Pts',(40.3847855154406,4.90549597232289,-13.0029231033536));
#70330=CARTESIAN_POINT('Ctrl Pts',(42.7600675205086,4.70489017086291,-10.4341711122309));
#70331=CARTESIAN_POINT('Ctrl Pts',(41.9072757812719,4.50428436940293,-7.04073827364627));
#70332=CARTESIAN_POINT('Ctrl Pts',(38.5995975862866,4.30367856794295,-5.90008259990626));
#70333=CARTESIAN_POINT('Ctrl Pts',(35.8363575143004,4.10307276648297,-8.04629210832045));
#70334=CARTESIAN_POINT('Ctrl Pts',(36.1231331479275,3.90246696502298,-11.5333752820698));
#70335=CARTESIAN_POINT('Ctrl Pts',(39.1998994778117,3.701861163563,-13.1993206345152));
#70336=CARTESIAN_POINT('Ctrl Pts',(42.2767548315279,3.50125536210303,-11.5335406820516));
#70337=CARTESIAN_POINT('Ctrl Pts',(42.5637263103221,3.30064956064303,-8.0464869970296));
#70338=CARTESIAN_POINT('Ctrl Pts',(39.800597384115,3.10004375918305,-5.90009555072928));
#70339=CARTESIAN_POINT('Ctrl Pts',(36.4928697401343,2.89943795772307,-7.04062911559291));
#70340=CARTESIAN_POINT('Ctrl Pts',(35.6398653250698,2.69883215626309,-10.4338969393871));
#70341=CARTESIAN_POINT('Ctrl Pts',(38.0150565132925,2.49822635480311,-13.0030110403416));
#70342=CARTESIAN_POINT('Ctrl Pts',(41.4647096194439,2.29762055334312,-12.4183963930662));
#70343=CARTESIAN_POINT('Ctrl Pts',(42.8608096815054,2.09701475188314,-9.21015919524167));
#70344=CARTESIAN_POINT('Ctrl Pts',(40.9374259147327,1.89640895042316,-6.28740778173331));
#70345=CARTESIAN_POINT('Ctrl Pts',(37.4386100185307,1.69580314896318,-6.30038256839133));
#70346=CARTESIAN_POINT('Ctrl Pts',(35.5369559639688,1.4951973475032,-9.23731854427653));
#70347=CARTESIAN_POINT('Ctrl Pts',(36.9568117578627,1.29459154604321,-12.4351131820842));
#70348=CARTESIAN_POINT('Ctrl Pts',(40.410705843259,1.09398574458323,-12.9941272089789));
#70349=CARTESIAN_POINT('Ctrl Pts',(42.76677764218,0.893379943123255,-10.4074678347248));
#70350=CARTESIAN_POINT('Ctrl Pts',(41.8886303202978,0.692774141663271,-7.02061999125906));
#70351=CARTESIAN_POINT('Ctrl Pts',(38.5725346701973,0.492168340203288,-5.90464925892042));
#70352=CARTESIAN_POINT('Ctrl Pts',(35.8254008592128,0.291562538743307,-8.07147570812169));
#70353=CARTESIAN_POINT('Ctrl Pts',(36.1382259692999,0.090956737283325,-11.5563030332699));
#70354=CARTESIAN_POINT('Ctrl Pts',(39.227352017236,-0.109649064176656,-13.19922156318));
#70355=CARTESIAN_POINT('Ctrl Pts',(42.291676290017,-0.310254865636639,-11.510494886889));
#70356=CARTESIAN_POINT('Ctrl Pts',(42.5525853866673,-0.510860667096621,
-8.02139651063807));
#70357=CARTESIAN_POINT('Ctrl Pts',(39.7734968022572,-0.711466468556603,
-5.89570893342317));
#70358=CARTESIAN_POINT('Ctrl Pts',(36.4743829991325,-0.912072270016586,
-7.06092528670388));
#70359=CARTESIAN_POINT('Ctrl Pts',(35.6467556479424,-1.11267807147657,-10.4604714333933));
#70360=CARTESIAN_POINT('Ctrl Pts',(38.0410759415337,-1.31328387293655,-13.0117674506389));
#70361=CARTESIAN_POINT('Ctrl Pts',(41.4862647571546,-1.51388967439654,-12.4013945640885));
#70362=CARTESIAN_POINT('Ctrl Pts',(42.8583551253254,-1.71449547585652,-9.18281583155971));
#70363=CARTESIAN_POINT('Ctrl Pts',(40.9131873733246,-1.9151012773165,-6.27451676638583));
#70364=CARTESIAN_POINT('Ctrl Pts',(37.4145660798143,-2.11570707877648,-6.31363300995112));
#70365=CARTESIAN_POINT('Ctrl Pts',(35.5349087651602,-2.31631288023646,-9.26469543141597));
#70366=CARTESIAN_POINT('Ctrl Pts',(36.9786176201205,-2.51691868169644,-12.4517921946197));
#70367=CARTESIAN_POINT('Ctrl Pts',(40.4365920357559,-2.71752448315643,-12.9849844458076));
#70368=CARTESIAN_POINT('Ctrl Pts',(42.7732715438646,-2.91813028461641,-10.3807936094251));
#70369=CARTESIAN_POINT('Ctrl Pts',(41.8698435068077,-3.11873608607639,-7.00060148207879));
#70370=CARTESIAN_POINT('Ctrl Pts',(38.5455023136619,-3.31934188753637,-5.90943849358033));
#70371=CARTESIAN_POINT('Ctrl Pts',(35.8146348786017,-3.51994768899636,-8.09672998948182));
#70372=CARTESIAN_POINT('Ctrl Pts',(36.1534885487898,-3.72055349045633,-11.5791227338624));
#70373=CARTESIAN_POINT('Ctrl Pts',(39.2548036267735,-3.92115929191632,-13.198914641172));
#70374=CARTESIAN_POINT('Ctrl Pts',(42.3064248479004,-4.1217650933763,-11.4873396475821));
#70375=CARTESIAN_POINT('Ctrl Pts',(42.541257458194,-4.32237089483629,-7.99638924961627));
#70376=CARTESIAN_POINT('Ctrl Pts',(39.7463641247024,-4.52297669629626,-5.89152528956596));
#70377=CARTESIAN_POINT('Ctrl Pts',(36.4560484587279,-4.72358249775625,-7.08135883009064));
#70378=CARTESIAN_POINT('Ctrl Pts',(35.6538443127724,-4.92418829921622,-10.4869937993917));
#70379=CARTESIAN_POINT('Ctrl Pts',(38.067160078324,-5.12479410067622,-13.0203291604629));
#70380=CARTESIAN_POINT('Ctrl Pts',(41.5076922567986,-5.32539990213619,-12.3842321829538));
#70381=CARTESIAN_POINT('Ctrl Pts',(42.8556963412319,-5.52600570359617,-9.15549155783884));
#70382=CARTESIAN_POINT('Ctrl Pts',(40.8888531903923,-5.72661150505615,-6.26180721847069));
#70383=CARTESIAN_POINT('Ctrl Pts',(37.390621815149,-5.92721730651614,-6.3270627253933));
#70384=CARTESIAN_POINT('Ctrl Pts',(35.5330661727275,-6.12782310797612,-9.29208685197852));
#70385=CARTESIAN_POINT('Ctrl Pts',(37.0005474930735,-6.32842890943611,-12.4683078156879));
#70386=CARTESIAN_POINT('Ctrl Pts',(40.4624091943875,-6.52903471089608,-12.9756485265975));
#70387=CARTESIAN_POINT('Ctrl Pts',(42.7795659647536,-6.72964051235607,-10.354071608499));
#70388=CARTESIAN_POINT('Ctrl Pts',(41.8509076470888,-6.93024631381605,-6.98072389967437));
#70389=CARTESIAN_POINT('Ctrl Pts',(38.5185064949806,-7.13085211527603,-5.91442956983856));
#70390=CARTESIAN_POINT('Ctrl Pts',(35.8040578888541,-7.33145791673602,-8.12206400532603));
#70391=CARTESIAN_POINT('Ctrl Pts',(36.1689212021761,-7.532063718196,-11.6018277611446));
#70392=CARTESIAN_POINT('Ctrl Pts',(39.2822521770986,-7.73266951965597,-13.1984026202339));
#70393=CARTESIAN_POINT('Ctrl Pts',(42.3209999865671,-7.93327532111597,-11.4640748582897));
#70394=CARTESIAN_POINT('Ctrl Pts',(42.5297430022072,-8.13388112257593,-7.97146732602006));
#70395=CARTESIAN_POINT('Ctrl Pts',(39.7192009440691,-8.33448692403593,-5.88754448456992));
#70396=CARTESIAN_POINT('Ctrl Pts',(36.4378671053041,-8.5350927254959,-7.10192879737212));
#70397=CARTESIAN_POINT('Ctrl Pts',(35.6611309375955,-8.73569852695589,-10.513462450324));
#70398=CARTESIAN_POINT('Ctrl Pts',(38.093307470686,-8.93630432841588,-13.0286957621018));
#70399=CARTESIAN_POINT('Ctrl Pts',(41.5289909005289,-9.13691012987584,-12.3669101408529));
#70400=CARTESIAN_POINT('Ctrl Pts',(42.8528335278548,-9.33751593133584,-9.12818799432527));
#70401=CARTESIAN_POINT('Ctrl Pts',(40.8644246221869,-9.53812173279581,-6.24927968040188));
#70402=CARTESIAN_POINT('Ctrl Pts',(37.3667787632686,-9.73872753425581,-6.34067128246068));
#70403=CARTESIAN_POINT('Ctrl Pts',(35.5314278932901,-9.93933333571576,-9.31949066061397));
#70404=CARTESIAN_POINT('Ctrl Pts',(37.0226009281239,-10.1399391371757,-12.4846603262167));
#70405=CARTESIAN_POINT('Ctrl Pts',(40.4881543603094,-10.3405449386357,-12.9661176206786));
#70406=CARTESIAN_POINT('Ctrl Pts',(42.785663522224,-10.5411507400957,-10.3273079236824));
#70407=CARTESIAN_POINT('Ctrl Pts',(41.8318179907986,-10.7417565415557,-6.9609793558109));
#70408=CARTESIAN_POINT('Ctrl Pts',(38.4915600815517,-10.9423623430157,-5.91963981024859));
#70409=CARTESIAN_POINT('Ctrl Pts',(35.7936482578035,-11.1429681444757,-8.14744191072689));
#70410=CARTESIAN_POINT('Ctrl Pts',(36.1845665389655,-11.3435739459356,-11.6244841995046));
#70411=CARTESIAN_POINT('Ctrl Pts',(39.3096110991439,-11.5441797473956,-13.1975537759688));
#70412=CARTESIAN_POINT('Ctrl Pts',(42.3355672427447,-11.7447855488556,-11.4409595689041));
#70413=CARTESIAN_POINT('Ctrl Pts',(42.5177171990917,-11.9453913503156,-7.94612769865488));
#70414=CARTESIAN_POINT('Ctrl Pts',(39.6926460209969,-12.1459971517755,-5.88475596888554));
#70415=CARTESIAN_POINT('Ctrl Pts',(36.4185870787412,-12.3466029532356,-7.12067230223758));
#70416=CARTESIAN_POINT('Ctrl Pts',(35.6711340431576,-12.5472087546955,-10.5439995150024));
#70417=CARTESIAN_POINT('Ctrl Pts',(37.2996374022545,-12.6809459556688,-12.1983898865047));
#70418=CARTESIAN_POINT('Ctrl Pts',(38.2842826159495,-12.7478145561555,-12.5013321319679));
#70419=CARTESIAN_POINT('Ctrl Pts',(40.9548065210116,5.97203701228902,-11.8040955702177));
#70420=CARTESIAN_POINT('Ctrl Pts',(41.7091888265352,5.90513543377346,-11.2232993565576));
#70421=CARTESIAN_POINT('Ctrl Pts',(42.5829832828131,5.77136525477125,-9.26428710520824));
#70422=CARTESIAN_POINT('Ctrl Pts',(40.8275941228708,5.57072647528236,-6.54443397888103));
#70423=CARTESIAN_POINT('Ctrl Pts',(37.5950874943231,5.37012067382238,-6.53543619717014));
#70424=CARTESIAN_POINT('Ctrl Pts',(35.8186741396894,5.16951487236241,-9.2334562518404));
#70425=CARTESIAN_POINT('Ctrl Pts',(37.1078986227854,4.96890907090242,-12.1977683509632));
#70426=CARTESIAN_POINT('Ctrl Pts',(40.2943767302342,4.76830326944244,-12.7375292420027));
#70427=CARTESIAN_POINT('Ctrl Pts',(42.4884053710417,4.56769746798245,-10.3647939509386));
#70428=CARTESIAN_POINT('Ctrl Pts',(41.7006885877136,4.36709166652247,-7.23030767830835));
#70429=CARTESIAN_POINT('Ctrl Pts',(38.6454131808827,4.16648586506249,-6.17669332340427));
#70430=CARTESIAN_POINT('Ctrl Pts',(36.0930308336797,3.96588006360251,-8.15912956490612));
#70431=CARTESIAN_POINT('Ctrl Pts',(36.3579231506009,3.76527426214253,-11.3801198893222));
#70432=CARTESIAN_POINT('Ctrl Pts',(39.1999071484734,3.56466846068254,-12.918940041829));
#70433=CARTESIAN_POINT('Ctrl Pts',(42.0419733769346,3.36406265922256,-11.3802726679382));
#70434=CARTESIAN_POINT('Ctrl Pts',(42.3070465944413,3.16345685776258,-8.15930958201932));
#70435=CARTESIAN_POINT('Ctrl Pts',(39.7547669116891,2.9628510563026,-6.17670528597399));
#70436=CARTESIAN_POINT('Ctrl Pts',(36.6994458292241,2.76224525484262,-7.23020684990363));
#70437=CARTESIAN_POINT('Ctrl Pts',(35.9115325989661,2.56163945338263,-10.364540699716));
#70438=CARTESIAN_POINT('Ctrl Pts',(38.1054773529932,2.36103365192266,-12.7376104686823));
#70439=CARTESIAN_POINT('Ctrl Pts',(41.2918938288466,2.16042785046267,-12.1976066808283));
#70440=CARTESIAN_POINT('Ctrl Pts',(42.5814600845839,1.95982204900269,-9.23418411310284));
#70441=CARTESIAN_POINT('Ctrl Pts',(40.8048461656643,1.75921624754271,-6.53446243899614));
#70442=CARTESIAN_POINT('Ctrl Pts',(37.5730184210845,1.55861044608272,-6.54644714374924));
#70443=CARTESIAN_POINT('Ctrl Pts',(35.81647606034,1.35800464462275,-9.25927098258661));
#70444=CARTESIAN_POINT('Ctrl Pts',(37.1279852920744,1.15739884316276,-12.2130478426818));
#70445=CARTESIAN_POINT('Ctrl Pts',(40.3183191259124,0.956793041702779,-12.7294045460136));
#70446=CARTESIAN_POINT('Ctrl Pts',(42.4946034557738,0.756187240242797,-10.340128351011));
#70447=CARTESIAN_POINT('Ctrl Pts',(41.6834659272838,0.555581438782815,-7.21172458473581));
#70448=CARTESIAN_POINT('Ctrl Pts',(38.6204153857253,0.354975637322832,-6.18091150913903));
#70449=CARTESIAN_POINT('Ctrl Pts',(36.0829102606201,0.154369835862851,-8.18239145091573));
#70450=CARTESIAN_POINT('Ctrl Pts',(36.3718642667677,-0.0462359655971322,
-11.4012980663534));
#70451=CARTESIAN_POINT('Ctrl Pts',(39.2252648355318,-0.246841767057112,
-12.9188485304437));
#70452=CARTESIAN_POINT('Ctrl Pts',(42.0557562066018,-0.447447568517095,
-11.3589854546603));
#70453=CARTESIAN_POINT('Ctrl Pts',(42.2967558140069,-0.648053369977079,
-8.13613370410783));
#70454=CARTESIAN_POINT('Ctrl Pts',(39.7297343249682,-0.848659171437058,
-6.17265340329844));
#70455=CARTESIAN_POINT('Ctrl Pts',(36.6823697771398,-1.04926497289704,-7.24895425784137));
#70456=CARTESIAN_POINT('Ctrl Pts',(35.91789713408,-1.24987077435702,-10.3890873433735));
#70457=CARTESIAN_POINT('Ctrl Pts',(38.1295112869248,-1.45047657581701,-12.7456986935507));
#70458=CARTESIAN_POINT('Ctrl Pts',(41.3118041339779,-1.65108237727699,-12.1819022298859));
#70459=CARTESIAN_POINT('Ctrl Pts',(42.5791928310334,-1.85168817873697,-9.20892727078845));
#70460=CARTESIAN_POINT('Ctrl Pts',(40.7824572223946,-2.05229398019695,-6.52255511312024));
#70461=CARTESIAN_POINT('Ctrl Pts',(37.5508092307361,-2.25289978165693,-6.5586864686898));
#70462=CARTESIAN_POINT('Ctrl Pts',(35.8145850794753,-2.45350558311692,-9.28455879024563));
#70463=CARTESIAN_POINT('Ctrl Pts',(37.1481271894279,-2.65411138457689,-12.2284541107061));
#70464=CARTESIAN_POINT('Ctrl Pts',(40.3422299910721,-2.85471718603688,-12.7209594501424));
#70465=CARTESIAN_POINT('Ctrl Pts',(42.5006018198656,-3.05532298749686,-10.3154895863701));
#70466=CARTESIAN_POINT('Ctrl Pts',(41.6661127006862,-3.25592878895684,-7.19323365086183));
#70467=CARTESIAN_POINT('Ctrl Pts',(38.595445818179,-3.45653459041683,-6.18533528618488));
#70468=CARTESIAN_POINT('Ctrl Pts',(36.0729658120213,-3.65714039187681,-8.20571862490556));
#70469=CARTESIAN_POINT('Ctrl Pts',(36.3859621871249,-3.85774619333678,-11.4223764379185));
#70470=CARTESIAN_POINT('Ctrl Pts',(39.2506216636613,-4.05835199479678,-12.9185650290848));
#70471=CARTESIAN_POINT('Ctrl Pts',(42.0693793293881,-4.25895779625675,-11.3375971487179));
#70472=CARTESIAN_POINT('Ctrl Pts',(42.286292298745,-4.45956359771674,-8.11303470079247));
#70473=CARTESIAN_POINT('Ctrl Pts',(39.7046720917133,-4.66016939917672,-6.16878900554438));
#70474=CARTESIAN_POINT('Ctrl Pts',(36.6654343115076,-4.8607752006367,-7.26782855543132));
#70475=CARTESIAN_POINT('Ctrl Pts',(35.9244448760446,-5.06138100209668,-10.413585836815));
#70476=CARTESIAN_POINT('Ctrl Pts',(38.1536049916162,-5.26198680355667,-12.7536070751778));
#70477=CARTESIAN_POINT('Ctrl Pts',(41.3315965408666,-5.46259260501664,-12.1660494782237));
#70478=CARTESIAN_POINT('Ctrl Pts',(42.5767369338228,-5.66319840647663,-9.18368806171562));
#70479=CARTESIAN_POINT('Ctrl Pts',(40.7599799358282,-5.8638042079366,-6.51081540723351));
#70480=CARTESIAN_POINT('Ctrl Pts',(37.528692108497,-6.0644100093966,-6.57109138745532));
#70481=CARTESIAN_POINT('Ctrl Pts',(35.8128830918537,-6.26501581085657,-9.30986002230918));
#70482=CARTESIAN_POINT('Ctrl Pts',(37.16838363445,-6.46562161231656,-12.2437094553629));
#70483=CARTESIAN_POINT('Ctrl Pts',(40.3660770902129,-6.66622741377654,-12.7123359376115));
#70484=CARTESIAN_POINT('Ctrl Pts',(42.506415925171,-6.86683321523652,-10.2908066917722));
#70485=CARTESIAN_POINT('Ctrl Pts',(41.6486218013013,-7.06743901669651,-7.1748728899028));
#70486=CARTESIAN_POINT('Ctrl Pts',(38.5705100003509,-7.26804481815648,-6.18994550267102));
#70487=CARTESIAN_POINT('Ctrl Pts',(36.0631959327435,-7.46865061961647,-8.22911944898889));
#70488=CARTESIAN_POINT('Ctrl Pts',(36.400217203355,-7.66925642107645,-11.4433488866808));
#70489=CARTESIAN_POINT('Ctrl Pts',(39.2759756660211,-7.86986222253643,-12.9180920795149));
#70490=CARTESIAN_POINT('Ctrl Pts',(42.0828422662563,-8.07046802399641,-11.3161076523461));
#70491=CARTESIAN_POINT('Ctrl Pts',(42.2756564895382,-8.27107382545639,-8.09001452296202));
#70492=CARTESIAN_POINT('Ctrl Pts',(39.6795816830134,-8.47167962691638,-6.16511196839422));
#70493=CARTESIAN_POINT('Ctrl Pts',(36.6486403434418,-8.67228542837637,-7.28682886666163));
#70494=CARTESIAN_POINT('Ctrl Pts',(35.9311754720423,-8.87289122983634,-10.4380347140871));
#70495=CARTESIAN_POINT('Ctrl Pts',(38.1777571249638,-9.07349703129632,-12.7613352369636));
#70496=CARTESIAN_POINT('Ctrl Pts',(41.3512699245974,-9.27410283275631,-12.1500492490276));
#70497=CARTESIAN_POINT('Ctrl Pts',(42.5740925764247,-9.47470863421628,-9.15846798249258));
#70498=CARTESIAN_POINT('Ctrl Pts',(40.7374154663536,-9.67531443567627,-6.49924382235935));
#70499=CARTESIAN_POINT('Ctrl Pts',(37.5066684756828,-9.87592023713625,-6.58366150077329));
#70500=CARTESIAN_POINT('Ctrl Pts',(35.8113698264815,-10.0765260385962,-9.33517269713481));
#70501=CARTESIAN_POINT('Ctrl Pts',(37.1887542127754,-10.2771318400562,-12.2588141361429));
#70502=CARTESIAN_POINT('Ctrl Pts',(40.389857690274,-10.4777376415162,-12.7035323174459));
#70503=CARTESIAN_POINT('Ctrl Pts',(42.5120481893403,-10.6783434429762,-10.266085294104));
#70504=CARTESIAN_POINT('Ctrl Pts',(41.6309888412761,-10.8789492444362,-7.15663501556043));
#70505=CARTESIAN_POINT('Ctrl Pts',(38.5456198177521,-11.0795550458962,-6.19475815929904));
#70506=CARTESIAN_POINT('Ctrl Pts',(36.0535806413312,-11.2801608473562,-8.2525608134982));
#70507=CARTESIAN_POINT('Ctrl Pts',(36.4146686735121,-11.4807666488161,-11.4642764542515));
#70508=CARTESIAN_POINT('Ctrl Pts',(39.301246879469,-11.6813724502761,-12.9173080089812));
#70509=CARTESIAN_POINT('Ctrl Pts',(42.0962979221335,-11.8819782517361,-11.2947562478204));
#70510=CARTESIAN_POINT('Ctrl Pts',(42.2645483531536,-12.0825840531961,-8.06660851556254));
#70511=CARTESIAN_POINT('Ctrl Pts',(39.6550531168681,-12.2831898546561,-6.16253623916968));
#70512=CARTESIAN_POINT('Ctrl Pts',(36.6308315399463,-12.483795656116,-7.30414208943529));
#70513=CARTESIAN_POINT('Ctrl Pts',(35.9404152591722,-12.684401457576,-10.4662415519984));
#70514=CARTESIAN_POINT('Ctrl Pts',(37.4446505473975,-12.8181386585493,-11.9943884627264));
#70515=CARTESIAN_POINT('Ctrl Pts',(38.3541593111027,-12.885007259036,-12.2742137473193));
#70516=CARTESIAN_POINT('Ctrl Pts',(40.8098382286002,5.83484430940857,-11.6158146463091));
#70517=CARTESIAN_POINT('Ctrl Pts',(41.5018994102006,5.76794273089301,-11.0829992409746));
#70518=CARTESIAN_POINT('Ctrl Pts',(42.303507851252,5.63417255189079,-9.28582515097854));
#70519=CARTESIAN_POINT('Ctrl Pts',(40.6931351167602,5.43353377240191,-6.79066486606293));
#70520=CARTESIAN_POINT('Ctrl Pts',(37.7276727238809,5.23292797094192,-6.78241041020279));
#70521=CARTESIAN_POINT('Ctrl Pts',(36.0980126480587,5.03232216948195,-9.25754129986588));
#70522=CARTESIAN_POINT('Ctrl Pts',(37.280731559394,4.83171636802196,-11.9769652828124));
#70523=CARTESIAN_POINT('Ctrl Pts',(40.2039679450279,4.63111056656198,-12.4721353806518));
#70524=CARTESIAN_POINT('Ctrl Pts',(42.2167432215747,4.43050476510199,-10.2954167896462));
#70525=CARTESIAN_POINT('Ctrl Pts',(41.4941013941553,4.22989896364201,-7.41987708297046));
#70526=CARTESIAN_POINT('Ctrl Pts',(38.6912287754788,4.02929316218203,-6.45330404690225));
#70527=CARTESIAN_POINT('Ctrl Pts',(36.3497041530591,3.82868736072205,-8.27196702149181));
#70528=CARTESIAN_POINT('Ctrl Pts',(36.5927131532743,3.62808155926206,-11.2268644965746));
#70529=CARTESIAN_POINT('Ctrl Pts',(39.1999148191352,3.42747575780209,-12.6385594491428));
#70530=CARTESIAN_POINT('Ctrl Pts',(41.8071919223413,3.2268699563421,-11.2270046538248));
#70531=CARTESIAN_POINT('Ctrl Pts',(42.0503668785605,3.02626415488212,-8.27213216700902));
#70532=CARTESIAN_POINT('Ctrl Pts',(39.7089364392632,2.82565835342213,-6.4533150212187));
#70533=CARTESIAN_POINT('Ctrl Pts',(36.9060219183138,2.62505255196216,-7.41978458421434));
#70534=CARTESIAN_POINT('Ctrl Pts',(36.1831998728624,2.42444675050217,-10.2951844600449));
#70535=CARTESIAN_POINT('Ctrl Pts',(38.1958981926941,2.22384094904219,-12.4722098970229));
#70536=CARTESIAN_POINT('Ctrl Pts',(41.1190780382492,2.02323514758221,-11.9768169685905));
#70537=CARTESIAN_POINT('Ctrl Pts',(42.3021104876626,1.82262934612223,-9.25820903096404));
#70538=CARTESIAN_POINT('Ctrl Pts',(40.6722664165957,1.62202354466224,-6.78151709625895));
#70539=CARTESIAN_POINT('Ctrl Pts',(37.7074268236383,1.42141774320227,-6.79251171910715));
#70540=CARTESIAN_POINT('Ctrl Pts',(36.0959961567111,1.22081194174228,-9.28122342089669));
#70541=CARTESIAN_POINT('Ctrl Pts',(37.2991588262862,1.0202061402823,-11.9909825032795));
#70542=CARTESIAN_POINT('Ctrl Pts',(40.2259324085659,0.81960033882232,-12.4646818830482));
#70543=CARTESIAN_POINT('Ctrl Pts',(42.2224292693677,0.61899453736234,-10.2727888672974));
#70544=CARTESIAN_POINT('Ctrl Pts',(41.4783015342697,0.418388735902356,-7.40282917821255));
#70545=CARTESIAN_POINT('Ctrl Pts',(38.6682961012533,0.217782934442375,-6.45717375935766));
#70546=CARTESIAN_POINT('Ctrl Pts',(36.3404196620272,0.017177132982393,-8.29330719370977));
#70547=CARTESIAN_POINT('Ctrl Pts',(36.6055025642355,-0.183428668477588,
-11.246293099437));
#70548=CARTESIAN_POINT('Ctrl Pts',(39.2231776538277,-0.384034469937571,
-12.6384754977072));
#70549=CARTESIAN_POINT('Ctrl Pts',(41.8198361231866,-0.584640271397551,
-11.2074760224316));
#70550=CARTESIAN_POINT('Ctrl Pts',(42.0409262413466,-0.785246072857537,
-8.25087089757759));
#70551=CARTESIAN_POINT('Ctrl Pts',(39.6859718476791,-0.985851874317515,
-6.44959787317372));
#70552=CARTESIAN_POINT('Ctrl Pts',(36.8903565551472,-1.18645767577751,-7.43698322897887));
#70553=CARTESIAN_POINT('Ctrl Pts',(36.1890386202178,-1.38706347723748,-10.3177032533537));
#70554=CARTESIAN_POINT('Ctrl Pts',(38.217946632316,-1.58766927869747,-12.4796299364624));
#70555=CARTESIAN_POINT('Ctrl Pts',(41.1373435108012,-1.78827508015745,-11.9624098956833));
#70556=CARTESIAN_POINT('Ctrl Pts',(42.3000305367416,-1.98888088161743,-9.23503871001721));
#70557=CARTESIAN_POINT('Ctrl Pts',(40.6517270714646,-2.18948668307741,-6.77059345985466));
#70558=CARTESIAN_POINT('Ctrl Pts',(37.6870523816581,-2.3900924845374,-6.80373992742849));
#70559=CARTESIAN_POINT('Ctrl Pts',(36.0942613937905,-2.59069828599738,-9.30442214907529));
#70560=CARTESIAN_POINT('Ctrl Pts',(37.3176367587351,-2.79130408745736,-12.0051160267924));
#70561=CARTESIAN_POINT('Ctrl Pts',(40.2478679463885,-2.99190988891734,-12.4569344544771));
#70562=CARTESIAN_POINT('Ctrl Pts',(42.2279320958664,-3.19251569037733,-10.2501855633152));
#70563=CARTESIAN_POINT('Ctrl Pts',(41.4623818945649,-3.3931214918373,-7.38586581964484));
#70564=CARTESIAN_POINT('Ctrl Pts',(38.645389322696,-3.59372729329729,-6.46123207878943));
#70565=CARTESIAN_POINT('Ctrl Pts',(36.3312967454408,-3.79433309475727,-8.31470726032929));
#70566=CARTESIAN_POINT('Ctrl Pts',(36.61843582546,-3.99493889621725,-11.2656301419746));
#70567=CARTESIAN_POINT('Ctrl Pts',(39.246439700549,-4.19554469767724,-12.6382154169976));
#70568=CARTESIAN_POINT('Ctrl Pts',(41.8323338108756,-4.39615049913721,-11.1878546498535));
#70569=CARTESIAN_POINT('Ctrl Pts',(42.0313271392962,-4.5967563005972,-8.22968015196867));
#70570=CARTESIAN_POINT('Ctrl Pts',(39.6629800587242,-4.79736210205718,-6.4460527215228));
#70571=CARTESIAN_POINT('Ctrl Pts',(36.8748201642874,-4.99796790351717,-7.45429828077202));
#70572=CARTESIAN_POINT('Ctrl Pts',(36.1950454393167,-5.19857370497714,-10.3401778742381));
#70573=CARTESIAN_POINT('Ctrl Pts',(38.2400499049083,-5.39917950643713,-12.4868849898927));
#70574=CARTESIAN_POINT('Ctrl Pts',(41.1555008249347,-5.59978530789711,-11.9478667734935));
#70575=CARTESIAN_POINT('Ctrl Pts',(42.2977775264137,-5.80039110935709,-9.21188456559238));
#70576=CARTESIAN_POINT('Ctrl Pts',(40.631106681264,-6.00099691081707,-6.75982359599637));
#70577=CARTESIAN_POINT('Ctrl Pts',(37.6667624018449,-6.20160271227705,-6.81512004951732));
#70578=CARTESIAN_POINT('Ctrl Pts',(36.0927000109799,-6.40220851373704,-9.32763319263987));
#70579=CARTESIAN_POINT('Ctrl Pts',(37.3362197758266,-6.60281431519701,-12.0191110950378));
#70580=CARTESIAN_POINT('Ctrl Pts',(40.2697449860384,-6.803420116657,-12.4490233486254));
#70581=CARTESIAN_POINT('Ctrl Pts',(42.2332658855884,-7.00402591811698,-10.2275417750453));
#70582=CARTESIAN_POINT('Ctrl Pts',(41.4463359555139,-7.20463171957697,-7.36902188013124));
#70583=CARTESIAN_POINT('Ctrl Pts',(38.6225135057212,-7.40523752103695,-6.46546143550347));
#70584=CARTESIAN_POINT('Ctrl Pts',(36.322333976633,-7.60584332249693,-8.33617489265172));
#70585=CARTESIAN_POINT('Ctrl Pts',(36.631513204534,-7.8064491239569,-11.2848700122171));
#70586=CARTESIAN_POINT('Ctrl Pts',(39.2696991549437,-8.0070549254169,-12.6377815387958));
#70587=CARTESIAN_POINT('Ctrl Pts',(41.8446845459455,-8.20766072687687,-11.1681404464025));
#70588=CARTESIAN_POINT('Ctrl Pts',(42.0215699768691,-8.40826652833686,-8.208561719904));
#70589=CARTESIAN_POINT('Ctrl Pts',(39.6399624219577,-8.60887232979683,-6.44267945221849));
#70590=CARTESIAN_POINT('Ctrl Pts',(36.8594135815794,-8.80947813125683,-7.47172893595116));
#70591=CARTESIAN_POINT('Ctrl Pts',(36.2012200064891,-9.0100839327168,-10.3626069778503));
#70592=CARTESIAN_POINT('Ctrl Pts',(38.2622067792416,-9.21068973417679,-12.4939747118254));
#70593=CARTESIAN_POINT('Ctrl Pts',(41.173548948666,-9.41129553563677,-11.9331883572021));
#70594=CARTESIAN_POINT('Ctrl Pts',(42.2953516249946,-9.61190133709674,-9.18874797065989));
#70595=CARTESIAN_POINT('Ctrl Pts',(40.6104063105204,-9.81250713855674,-6.7492079643168));
#70596=CARTESIAN_POINT('Ctrl Pts',(37.6465581880969,-10.0131129400167,-6.82665171908593));
#70597=CARTESIAN_POINT('Ctrl Pts',(36.0913117596729,-10.2137187414767,-9.35085473365563));
#70598=CARTESIAN_POINT('Ctrl Pts',(37.3549074974267,-10.4143245429366,-12.0329679460693));
#70599=CARTESIAN_POINT('Ctrl Pts',(40.2915610202388,-10.6149303443966,-12.440947014213));
#70600=CARTESIAN_POINT('Ctrl Pts',(42.2384328564565,-10.8155361458566,-10.2048626645257));
#70601=CARTESIAN_POINT('Ctrl Pts',(41.4301596917537,-11.0161419473166,-7.35229067530997));
#70602=CARTESIAN_POINT('Ctrl Pts',(38.5996795539523,-11.2167477487766,-6.46987650834947));
#70603=CARTESIAN_POINT('Ctrl Pts',(36.313513024859,-11.4173535502366,-8.35767971626948));
#70604=CARTESIAN_POINT('Ctrl Pts',(36.6447708080588,-11.6179593516965,-11.3040687089986));
#70605=CARTESIAN_POINT('Ctrl Pts',(39.2928826597942,-11.8185651531565,-12.6370622419936));
#70606=CARTESIAN_POINT('Ctrl Pts',(41.8570286015223,-12.0191709546165,-11.1485529267368));
#70607=CARTESIAN_POINT('Ctrl Pts',(42.0113795072156,-12.2197767560765,-8.18708933247013));
#70608=CARTESIAN_POINT('Ctrl Pts',(39.6174602127394,-12.4203825575364,-6.44031650945386));
#70609=CARTESIAN_POINT('Ctrl Pts',(36.8430760011515,-12.6209883589965,-7.48761187663297));
#70610=CARTESIAN_POINT('Ctrl Pts',(36.2096964751867,-12.8215941604564,-10.3884835889945));
#70611=CARTESIAN_POINT('Ctrl Pts',(37.5896636925404,-12.9553313614297,-11.7903870389479));
#70612=CARTESIAN_POINT('Ctrl Pts',(38.4240360062559,-13.0221999619164,-12.0470953626707));
#70613=CARTESIAN_POINT('Ctrl Pts',(40.6648699361887,5.6976516065281,-11.4275337224004));
#70614=CARTESIAN_POINT('Ctrl Pts',(41.2946099938659,5.63075002801254,-10.9426991253916));
#70615=CARTESIAN_POINT('Ctrl Pts',(42.0240324196909,5.49697984901032,-9.30736319674886));
#70616=CARTESIAN_POINT('Ctrl Pts',(40.5586761106497,5.29634106952145,-7.03689575324481));
#70617=CARTESIAN_POINT('Ctrl Pts',(37.8602579534387,5.09573526806147,-7.02938462323545));
#70618=CARTESIAN_POINT('Ctrl Pts',(36.3773511564279,4.89512946660149,-9.28162634789135));
#70619=CARTESIAN_POINT('Ctrl Pts',(37.4535644960028,4.6945236651415,-11.7561622146614));
#70620=CARTESIAN_POINT('Ctrl Pts',(40.1135591598215,4.49391786368153,-12.2067415193008));
#70621=CARTESIAN_POINT('Ctrl Pts',(41.9450810721079,4.29331206222154,-10.2260396283539));
#70622=CARTESIAN_POINT('Ctrl Pts',(41.2875142005968,4.09270626076156,-7.60944648763255));
#70623=CARTESIAN_POINT('Ctrl Pts',(38.737044370075,3.89210045930158,-6.72991477040025));
#70624=CARTESIAN_POINT('Ctrl Pts',(36.6063774724384,3.6914946578416,-8.3848044780775));
#70625=CARTESIAN_POINT('Ctrl Pts',(36.8275031559477,3.49088885638161,-11.0736091038271));
#70626=CARTESIAN_POINT('Ctrl Pts',(39.199922489797,3.29028305492163,-12.3581788564566));
#70627=CARTESIAN_POINT('Ctrl Pts',(41.5724104677478,3.08967725346165,-11.0737366397114));
#70628=CARTESIAN_POINT('Ctrl Pts',(41.7936871626797,2.88907145200167,-8.38495475199873));
#70629=CARTESIAN_POINT('Ctrl Pts',(39.6631059668373,2.68846565054169,-6.72992475646342));
#70630=CARTESIAN_POINT('Ctrl Pts',(37.1125980074036,2.4878598490817,-7.60936231852505));
#70631=CARTESIAN_POINT('Ctrl Pts',(36.4548671467587,2.28725404762172,-10.2258282203738));
#70632=CARTESIAN_POINT('Ctrl Pts',(38.286319032395,2.08664824616174,-12.2068093253635));
#70633=CARTESIAN_POINT('Ctrl Pts',(40.9462622476518,1.88604244470176,-11.7560272563527));
#70634=CARTESIAN_POINT('Ctrl Pts',(42.0227608907411,1.68543664324178,-9.2822339488252));
#70635=CARTESIAN_POINT('Ctrl Pts',(40.5396866675272,1.48483084178179,-7.02857175352177));
#70636=CARTESIAN_POINT('Ctrl Pts',(37.8418352261923,1.28422504032181,-7.03857629446507));
#70637=CARTESIAN_POINT('Ctrl Pts',(36.3755162530822,1.08361923886183,-9.30317585920677));
#70638=CARTESIAN_POINT('Ctrl Pts',(37.470332360498,0.883013437401846,-11.7689171638771));
#70639=CARTESIAN_POINT('Ctrl Pts',(40.1335456912194,0.682407635941864,-12.1999592200829));
#70640=CARTESIAN_POINT('Ctrl Pts',(41.9502550829617,0.481801834481882,-10.2054493835837));
#70641=CARTESIAN_POINT('Ctrl Pts',(41.2731371412557,0.2811960330219,-7.59393377168929));
#70642=CARTESIAN_POINT('Ctrl Pts',(38.7161768167814,0.0805902315619172,
-6.73343600957629));
#70643=CARTESIAN_POINT('Ctrl Pts',(36.5979290634346,-0.120015569898064,
-8.4042229365038));
#70644=CARTESIAN_POINT('Ctrl Pts',(36.8391408617033,-0.320621371358047,
-11.0912881325205));
#70645=CARTESIAN_POINT('Ctrl Pts',(39.2210904721234,-0.521227172818027,
-12.3581024649709));
#70646=CARTESIAN_POINT('Ctrl Pts',(41.5839160397715,-0.72183297427801,-11.055966590203));
#70647=CARTESIAN_POINT('Ctrl Pts',(41.7850966686863,-0.922438775737993,
-8.36560809104734));
#70648=CARTESIAN_POINT('Ctrl Pts',(39.6422093703901,-1.12304457719797,-6.72654234304899));
#70649=CARTESIAN_POINT('Ctrl Pts',(37.0983433331545,-1.32365037865796,-7.62501220011637));
#70650=CARTESIAN_POINT('Ctrl Pts',(36.4601801063555,-1.52425618011794,-10.2463191633339));
#70651=CARTESIAN_POINT('Ctrl Pts',(38.3063819777072,-1.72486198157792,-12.2135611793742));
#70652=CARTESIAN_POINT('Ctrl Pts',(40.9628828876245,-1.9254677830379,-11.7429175614806));
#70653=CARTESIAN_POINT('Ctrl Pts',(42.0208682424496,-2.12607358449789,-9.26115014924594));
#70654=CARTESIAN_POINT('Ctrl Pts',(40.5209969205346,-2.32667938595786,-7.01863180658909));
#70655=CARTESIAN_POINT('Ctrl Pts',(37.82329553258,-2.52728518741785,-7.04879338616719));
#70656=CARTESIAN_POINT('Ctrl Pts',(36.3739377081057,-2.72789098887783,-9.32428550790495));
#70657=CARTESIAN_POINT('Ctrl Pts',(37.4871463280423,-2.92849679033781,-11.7817779428789));
#70658=CARTESIAN_POINT('Ctrl Pts',(40.1535059017048,-3.12910259179779,-12.1929094588119));
#70659=CARTESIAN_POINT('Ctrl Pts',(41.9552623718673,-3.32970839325778,-10.1848815402601));
#70660=CARTESIAN_POINT('Ctrl Pts',(41.2586510884434,-3.53031419471776,-7.57849798842788));
#70661=CARTESIAN_POINT('Ctrl Pts',(38.6953328272131,-3.73091999617774,-6.73712887139397));
#70662=CARTESIAN_POINT('Ctrl Pts',(36.5896276788603,-3.93152579763772,-8.42369589575305));
#70663=CARTESIAN_POINT('Ctrl Pts',(36.8509094637952,-4.1321315990977,-11.1088838460307));
#70664=CARTESIAN_POINT('Ctrl Pts',(39.2422577374368,-4.33273740055769,-12.3578658049104));
#70665=CARTESIAN_POINT('Ctrl Pts',(41.5952882923632,-4.53334320201766,-11.0381121509893));
#70666=CARTESIAN_POINT('Ctrl Pts',(41.7763619798471,-4.73394900347766,-8.34632560314489));
#70667=CARTESIAN_POINT('Ctrl Pts',(39.6212880257352,-4.93455480493762,-6.72331643750121));
#70668=CARTESIAN_POINT('Ctrl Pts',(37.084206017067,-5.13516060639762,-7.64076800611272));
#70669=CARTESIAN_POINT('Ctrl Pts',(36.465646002589,-5.33576640785759,-10.2667699116612));
#70670=CARTESIAN_POINT('Ctrl Pts',(38.3264948182005,-5.53637220931758,-12.2201629046076));
#70671=CARTESIAN_POINT('Ctrl Pts',(40.9794051090027,-5.73697801077756,-11.7296840687635));
#70672=CARTESIAN_POINT('Ctrl Pts',(42.0188181190045,-5.93758381223754,-9.24008106946917));
#70673=CARTESIAN_POINT('Ctrl Pts',(40.5022334266998,-6.13818961369753,-7.00883178475918));
#70674=CARTESIAN_POINT('Ctrl Pts',(37.8048326951929,-6.3387954151575,-7.05914871157936));
#70675=CARTESIAN_POINT('Ctrl Pts',(36.3725169301061,-6.53940121661749,-9.34540636297052));
#70676=CARTESIAN_POINT('Ctrl Pts',(37.5040559172031,-6.74000701807747,-11.7945127347128));
#70677=CARTESIAN_POINT('Ctrl Pts',(40.1734128818639,-6.94061281953745,-12.1857107596392));
#70678=CARTESIAN_POINT('Ctrl Pts',(41.9601158460058,-7.14121862099744,-10.1642768583185));
#70679=CARTESIAN_POINT('Ctrl Pts',(41.2440501097264,-7.34182442245742,-7.56317087035968));
#70680=CARTESIAN_POINT('Ctrl Pts',(38.6745170110914,-7.5424302239174,-6.74097736833593));
#70681=CARTESIAN_POINT('Ctrl Pts',(36.5814720205227,-7.74303602537738,-8.44323033631458));
#70682=CARTESIAN_POINT('Ctrl Pts',(36.8628092057128,-7.94364182683736,-11.1263911377534));
#70683=CARTESIAN_POINT('Ctrl Pts',(39.2634226438662,-8.14424762829735,-12.3574709980766));
#70684=CARTESIAN_POINT('Ctrl Pts',(41.6065268256346,-8.34485342975733,-11.0201732404588));
#70685=CARTESIAN_POINT('Ctrl Pts',(41.7674834642002,-8.54545923121731,-8.32710891684597));
#70686=CARTESIAN_POINT('Ctrl Pts',(39.6003431609019,-8.74606503267729,-6.72024693604278));
#70687=CARTESIAN_POINT('Ctrl Pts',(37.0701868197171,-8.94667083413728,-7.65662900524067));
#70688=CARTESIAN_POINT('Ctrl Pts',(36.4712645409359,-9.14727663559725,-10.2871792416134));
#70689=CARTESIAN_POINT('Ctrl Pts',(38.3466564335193,-9.34788243705725,-12.2266141866871));
#70690=CARTESIAN_POINT('Ctrl Pts',(40.9958279727346,-9.54848823851721,-11.7163274653768));
#70691=CARTESIAN_POINT('Ctrl Pts',(42.0166106735645,-9.74909403997722,-9.2190279588272));
#70692=CARTESIAN_POINT('Ctrl Pts',(40.4833971546871,-9.94969984143717,-6.99917210627425));
#70693=CARTESIAN_POINT('Ctrl Pts',(37.7864479005111,-10.1503056428972,-7.06964193739857));
#70694=CARTESIAN_POINT('Ctrl Pts',(36.3712536928645,-10.3509114443572,-9.36653677017645));
#70695=CARTESIAN_POINT('Ctrl Pts',(37.5210607820781,-10.5515172458171,-11.8071217559955));
#70696=CARTESIAN_POINT('Ctrl Pts',(40.1932643502035,-10.7521230472771,-12.1783617109801));
#70697=CARTESIAN_POINT('Ctrl Pts',(41.9648175235727,-10.9527288487371,-10.1436400349473));
#70698=CARTESIAN_POINT('Ctrl Pts',(41.2293305422313,-11.1533346501971,-7.54794633505948));
#70699=CARTESIAN_POINT('Ctrl Pts',(38.6537392901525,-11.3539404516571,-6.74499485739993));
#70700=CARTESIAN_POINT('Ctrl Pts',(36.5734454083867,-11.5545462531171,-8.46279861904078));
#70701=CARTESIAN_POINT('Ctrl Pts',(36.8748729426055,-11.755152054577,-11.1438609637455));
#70702=CARTESIAN_POINT('Ctrl Pts',(39.2845184401193,-11.955757856037,-12.356816475006));
#70703=CARTESIAN_POINT('Ctrl Pts',(41.6177592809111,-12.156363657497,-11.0023496056531));
#70704=CARTESIAN_POINT('Ctrl Pts',(41.7582106612774,-12.356969458957,-8.30757014937776));
#70705=CARTESIAN_POINT('Ctrl Pts',(39.5798673086106,-12.557575260417,-6.71809677973804));
#70706=CARTESIAN_POINT('Ctrl Pts',(37.0553204623567,-12.758181061877,-7.67108166383065));
#70707=CARTESIAN_POINT('Ctrl Pts',(36.4789776912014,-12.9587868633369,-10.3107256259906));
#70708=CARTESIAN_POINT('Ctrl Pts',(37.7346768376834,-13.0925240643102,-11.5863856151695));
#70709=CARTESIAN_POINT('Ctrl Pts',(38.4939127014091,-13.1593926647969,-11.8199769780221));
#70710=CARTESIAN_POINT('Ctrl Pts',(40.6132835138381,5.7,-6.75441154943334));
#70711=CARTESIAN_POINT('Ctrl Pts',(40.6277913861508,5.7,-6.76195682417492));
#70712=CARTESIAN_POINT('Ctrl Pts',(40.6422992584636,5.7,-6.7695020989165));
#70713=CARTESIAN_POINT('Ctrl Pts',(40.6568071307763,5.7,-6.77704737365809));
#70714=CARTESIAN_POINT('Origin',(39.2,5.7,-9.525));
#70715=CARTESIAN_POINT('',(39.2,5.9,-12.83523));
#70716=CARTESIAN_POINT('Origin',(39.2,5.9,-9.525));
#70717=CARTESIAN_POINT('Origin',(39.2,5.7,-12.83523));
#70718=CARTESIAN_POINT('Origin',(39.2,5.9,-9.525));
#70719=CARTESIAN_POINT('',(34.4375,5.9,-9.525));
#70720=CARTESIAN_POINT('Origin',(39.2,5.9,-9.525));
#70721=CARTESIAN_POINT('Origin',(39.2,-12.95,-9.525));
#70722=CARTESIAN_POINT('',(36.48977,-13.15,-9.525));
#70723=CARTESIAN_POINT('',(36.28977,-12.95,-9.525));
#70724=CARTESIAN_POINT('Origin',(39.2,-13.15,-9.525));
#70725=CARTESIAN_POINT('Origin',(39.2,-13.15,-9.525));
#70726=CARTESIAN_POINT('Origin',(44.2203188851577,12.25,-10.2071323488364));
#70727=CARTESIAN_POINT('',(43.9012309732892,6.5,-10.2864680464642));
#70728=CARTESIAN_POINT('',(43.9012309732892,11.85,-10.2864680464642));
#70729=CARTESIAN_POINT('',(43.9012309732892,5.9,-10.2864680464642));
#70730=CARTESIAN_POINT('',(43.7424257607688,6.5,-10.3259522194887));
#70731=CARTESIAN_POINT('',(44.2203188851577,6.5,-10.2071323488364));
#70732=CARTESIAN_POINT('',(43.7424257607688,12.,-10.3259522194887));
#70733=CARTESIAN_POINT('',(43.7424257607688,12.25,-10.3259522194887));
#70734=CARTESIAN_POINT('Ctrl Pts',(43.9012309732892,11.85,-10.2864680464642));
#70735=CARTESIAN_POINT('Ctrl Pts',(43.8205579253287,11.9264281650905,-10.3065260063607));
#70736=CARTESIAN_POINT('Ctrl Pts',(43.7424257607688,12.,-10.3259522194887));
#70737=CARTESIAN_POINT('Origin',(43.7424257607688,12.25,-10.3259522194887));
#70738=CARTESIAN_POINT('',(43.8781494645997,11.85,-10.4173697870648));
#70739=CARTESIAN_POINT('',(43.8781494645997,6.5,-10.4173697870648));
#70740=CARTESIAN_POINT('',(43.8781494645997,5.9,-10.4173697870648));
#70741=CARTESIAN_POINT('Ctrl Pts',(43.7424257607688,12.,-10.3259522194887));
#70742=CARTESIAN_POINT('Ctrl Pts',(43.8092018230531,11.9264281650909,-10.3709296627358));
#70743=CARTESIAN_POINT('Ctrl Pts',(43.8781494645997,11.85,-10.4173697870648));
#70744=CARTESIAN_POINT('',(43.7424257607688,6.5,-10.3259522194887));
#70745=CARTESIAN_POINT('Origin',(43.9640075051966,6.5,-10.3650230594638));
#70746=CARTESIAN_POINT('Origin',(39.2,6.5,-9.525));
#70747=CARTESIAN_POINT('Origin',(39.2,12.05,-9.525));
#70748=CARTESIAN_POINT('',(34.5875,12.,-9.525));
#70749=CARTESIAN_POINT('',(34.4379637501835,11.85,-9.45853944452601));
#70750=CARTESIAN_POINT('Ctrl Pts',(34.5875,12.,-9.525));
#70751=CARTESIAN_POINT('Ctrl Pts',(34.5139281650903,11.9264281650903,-9.49230140670682));
#70752=CARTESIAN_POINT('Ctrl Pts',(34.4379637501835,11.85,-9.45853944452601));
#70753=CARTESIAN_POINT('',(34.4987690267108,11.85,-8.76353195353579));
#70754=CARTESIAN_POINT('Origin',(39.2,11.85,-9.525));
#70755=CARTESIAN_POINT('',(34.6575742392312,12.,-8.72404778051128));
#70756=CARTESIAN_POINT('Ctrl Pts',(34.4987690267108,11.85,-8.76353195353579));
#70757=CARTESIAN_POINT('Ctrl Pts',(34.579442074671,11.9264281650901,-8.74347399363938));
#70758=CARTESIAN_POINT('Ctrl Pts',(34.6575742392312,12.,-8.72404778051128));
#70759=CARTESIAN_POINT('',(34.5218505354004,11.85,-8.63263021293523));
#70760=CARTESIAN_POINT('Ctrl Pts',(34.6575742392312,12.,-8.72404778051128));
#70761=CARTESIAN_POINT('Ctrl Pts',(34.5907981769464,11.9264281650903,-8.67907033726385));
#70762=CARTESIAN_POINT('Ctrl Pts',(34.5218505354003,11.85,-8.63263021293522));
#70763=CARTESIAN_POINT('',(34.7024188274238,11.85,-7.95874017286797));
#70764=CARTESIAN_POINT('Origin',(39.2,11.85,-9.525));
#70765=CARTESIAN_POINT('',(34.865667786625,12.,-7.94743208891035));
#70766=CARTESIAN_POINT('Ctrl Pts',(34.7024188274237,11.85,-7.95874017286797));
#70767=CARTESIAN_POINT('Ctrl Pts',(34.7853492986979,11.9264281650903,-7.9529956662175));
#70768=CARTESIAN_POINT('Ctrl Pts',(34.865667786625,12.,-7.94743208891035));
#70769=CARTESIAN_POINT('',(34.7478805248412,11.85,-7.8338351857635));
#70770=CARTESIAN_POINT('Ctrl Pts',(34.865667786625,12.,-7.94743208891035));
#70771=CARTESIAN_POINT('Ctrl Pts',(34.8077164538273,11.9264281650903,-7.89154241256207));
#70772=CARTESIAN_POINT('Ctrl Pts',(34.7478805248412,11.85,-7.83383518576349));
#70773=CARTESIAN_POINT('',(35.0427253561796,11.85,-7.20153840448186));
#70774=CARTESIAN_POINT('Origin',(39.2,11.85,-9.525));
#70775=CARTESIAN_POINT('',(35.2054578250443,12.,-7.21875));
#70776=CARTESIAN_POINT('Ctrl Pts',(35.0427253561796,11.85,-7.20153840448186));
#70777=CARTESIAN_POINT('Ctrl Pts',(35.1253934503629,11.9264281650903,-7.21028189500508));
#70778=CARTESIAN_POINT('Ctrl Pts',(35.2054578250443,12.,-7.21875));
#70779=CARTESIAN_POINT('',(35.1091859116536,11.85,-7.08642534570168));
#70780=CARTESIAN_POINT('Ctrl Pts',(35.2054578250443,12.,-7.21875));
#70781=CARTESIAN_POINT('Ctrl Pts',(35.1580920436562,11.9264281650905,-7.15364627008541));
#70782=CARTESIAN_POINT('Ctrl Pts',(35.1091859116536,11.85,-7.08642534570167));
#70783=CARTESIAN_POINT('',(35.5093485713054,11.85,-6.51493384094727));
#70784=CARTESIAN_POINT('Origin',(39.2,11.85,-9.525));
#70785=CARTESIAN_POINT('',(35.6666200061137,12.,-6.56014215032084));
#70786=CARTESIAN_POINT('Ctrl Pts',(35.5093485713054,11.85,-6.51493384094727));
#70787=CARTESIAN_POINT('Ctrl Pts',(35.5892424601881,11.9264281650904,-6.53789966210907));
#70788=CARTESIAN_POINT('Ctrl Pts',(35.6666200061137,12.,-6.56014215032084));
#70789=CARTESIAN_POINT('',(35.5947886144885,11.85,-6.41311036253237));
#70790=CARTESIAN_POINT('Ctrl Pts',(35.6666200061137,12.,-6.56014215032084));
#70791=CARTESIAN_POINT('Ctrl Pts',(35.6312789614341,11.9264281650902,-6.48780251072884));
#70792=CARTESIAN_POINT('Ctrl Pts',(35.5947886144885,11.85,-6.41311036253236));
#70793=CARTESIAN_POINT('',(36.0881103625324,11.85,-5.91978861448852));
#70794=CARTESIAN_POINT('Origin',(39.2,11.85,-9.525));
#70795=CARTESIAN_POINT('',(36.2351421503208,12.,-5.99162000611371));
#70796=CARTESIAN_POINT('Ctrl Pts',(36.0881103625324,11.85,-5.91978861448852));
#70797=CARTESIAN_POINT('Ctrl Pts',(36.1628025107291,11.9264281650905,-5.95627896143419));
#70798=CARTESIAN_POINT('Ctrl Pts',(36.2351421503208,12.,-5.99162000611371));
#70799=CARTESIAN_POINT('',(36.1899338409473,11.85,-5.83434857130539));
#70800=CARTESIAN_POINT('Ctrl Pts',(36.2351421503208,12.,-5.99162000611371));
#70801=CARTESIAN_POINT('Ctrl Pts',(36.2128996621091,11.9264281650904,-5.91424246018812));
#70802=CARTESIAN_POINT('Ctrl Pts',(36.1899338409473,11.85,-5.83434857130539));
#70803=CARTESIAN_POINT('',(36.7614253457017,11.85,-5.43418591165355));
#70804=CARTESIAN_POINT('Origin',(39.2,11.85,-9.525));
#70805=CARTESIAN_POINT('',(36.89375,12.,-5.53045782504427));
#70806=CARTESIAN_POINT('Ctrl Pts',(36.7614253457017,11.85,-5.43418591165355));
#70807=CARTESIAN_POINT('Ctrl Pts',(36.8286462700852,11.9264281650903,-5.48309204365601));
#70808=CARTESIAN_POINT('Ctrl Pts',(36.89375,12.,-5.53045782504428));
#70809=CARTESIAN_POINT('',(36.8765384044819,11.85,-5.36772535617957));
#70810=CARTESIAN_POINT('Ctrl Pts',(36.89375,12.,-5.53045782504427));
#70811=CARTESIAN_POINT('Ctrl Pts',(36.885281895005,11.9264281650899,-5.45039345036243));
#70812=CARTESIAN_POINT('Ctrl Pts',(36.8765384044819,11.85,-5.36772535617957));
#70813=CARTESIAN_POINT('',(37.5088351857635,11.85,-5.07288052484118));
#70814=CARTESIAN_POINT('Origin',(39.2,11.85,-9.525));
#70815=CARTESIAN_POINT('',(37.6224320889104,12.,-5.19066778662499));
#70816=CARTESIAN_POINT('Ctrl Pts',(37.5088351857635,11.85,-5.07288052484117));
#70817=CARTESIAN_POINT('Ctrl Pts',(37.5665424125622,11.9264281650904,-5.13271645382743));
#70818=CARTESIAN_POINT('Ctrl Pts',(37.6224320889104,12.,-5.19066778662499));
#70819=CARTESIAN_POINT('',(37.633740172868,11.85,-5.02741882742375));
#70820=CARTESIAN_POINT('Ctrl Pts',(37.6224320889104,12.,-5.19066778662499));
#70821=CARTESIAN_POINT('Ctrl Pts',(37.6279956662175,11.9264281650906,-5.11034929869827));
#70822=CARTESIAN_POINT('Ctrl Pts',(37.633740172868,11.85,-5.02741882742374));
#70823=CARTESIAN_POINT('',(38.3076302129352,11.85,-4.84685053540035));
#70824=CARTESIAN_POINT('Origin',(39.2,11.85,-9.525));
#70825=CARTESIAN_POINT('',(38.3990477805113,12.,-4.98257423923119));
#70826=CARTESIAN_POINT('Ctrl Pts',(38.3076302129352,11.85,-4.84685053540035));
#70827=CARTESIAN_POINT('Ctrl Pts',(38.354070337264,11.9264281650904,-4.91579817694654));
#70828=CARTESIAN_POINT('Ctrl Pts',(38.3990477805113,12.,-4.98257423923119));
#70829=CARTESIAN_POINT('',(38.4385319535358,11.85,-4.82376902671077));
#70830=CARTESIAN_POINT('Ctrl Pts',(38.3990477805113,12.,-4.98257423923119));
#70831=CARTESIAN_POINT('Ctrl Pts',(38.4184739936393,11.9264281650905,-4.90444207467138));
#70832=CARTESIAN_POINT('Ctrl Pts',(38.4385319535358,11.85,-4.82376902671077));
#70833=CARTESIAN_POINT('',(39.133539444526,11.85,-4.76296375018353));
#70834=CARTESIAN_POINT('Origin',(39.2,11.85,-9.525));
#70835=CARTESIAN_POINT('',(39.2,12.,-4.9125));
#70836=CARTESIAN_POINT('Ctrl Pts',(39.133539444526,11.85,-4.76296375018353));
#70837=CARTESIAN_POINT('Ctrl Pts',(39.1673014067068,11.9264281650904,-4.83892816509036));
#70838=CARTESIAN_POINT('Ctrl Pts',(39.2,12.,-4.9125));
#70839=CARTESIAN_POINT('',(39.266460555474,11.85,-4.76296375018353));
#70840=CARTESIAN_POINT('Ctrl Pts',(39.2,12.,-4.9125));
#70841=CARTESIAN_POINT('Ctrl Pts',(39.2326985932933,11.9264281650901,-4.83892816509014));
#70842=CARTESIAN_POINT('Ctrl Pts',(39.266460555474,11.85,-4.76296375018353));
#70843=CARTESIAN_POINT('',(39.9614680464642,11.85,-4.82376902671077));
#70844=CARTESIAN_POINT('Origin',(39.2,11.85,-9.525));
#70845=CARTESIAN_POINT('',(40.0009522194887,12.,-4.98257423923119));
#70846=CARTESIAN_POINT('Ctrl Pts',(39.9614680464642,11.85,-4.82376902671077));
#70847=CARTESIAN_POINT('Ctrl Pts',(39.9815260063607,11.9264281650903,-4.90444207467118));
#70848=CARTESIAN_POINT('Ctrl Pts',(40.0009522194887,12.,-4.98257423923119));
#70849=CARTESIAN_POINT('',(40.0923697870648,11.85,-4.84685053540035));
#70850=CARTESIAN_POINT('Ctrl Pts',(40.0009522194887,12.,-4.98257423923119));
#70851=CARTESIAN_POINT('Ctrl Pts',(40.0459296627363,11.92642816509,-4.91579817694619));
#70852=CARTESIAN_POINT('Ctrl Pts',(40.0923697870648,11.85,-4.84685053540035));
#70853=CARTESIAN_POINT('',(40.766259827132,11.85,-5.02741882742375));
#70854=CARTESIAN_POINT('Origin',(39.2,11.85,-9.525));
#70855=CARTESIAN_POINT('',(40.7775679110897,12.,-5.190667786625));
#70856=CARTESIAN_POINT('Ctrl Pts',(40.766259827132,11.85,-5.02741882742374));
#70857=CARTESIAN_POINT('Ctrl Pts',(40.7720043337825,11.9264281650901,-5.11034929869772));
#70858=CARTESIAN_POINT('Ctrl Pts',(40.7775679110897,12.,-5.190667786625));
#70859=CARTESIAN_POINT('',(40.8911648142365,11.85,-5.07288052484118));
#70860=CARTESIAN_POINT('Ctrl Pts',(40.7775679110897,12.,-5.190667786625));
#70861=CARTESIAN_POINT('Ctrl Pts',(40.8334575874378,11.9264281650904,-5.13271645382747));
#70862=CARTESIAN_POINT('Ctrl Pts',(40.8911648142365,11.85,-5.07288052484118));
#70863=CARTESIAN_POINT('',(41.5234615955181,11.85,-5.36772535617957));
#70864=CARTESIAN_POINT('Origin',(39.2,11.85,-9.525));
#70865=CARTESIAN_POINT('',(41.50625,12.,-5.53045782504427));
#70866=CARTESIAN_POINT('Ctrl Pts',(41.5234615955181,11.85,-5.36772535617957));
#70867=CARTESIAN_POINT('Ctrl Pts',(41.5147181049949,11.9264281650903,-5.45039345036284));
#70868=CARTESIAN_POINT('Ctrl Pts',(41.50625,12.,-5.53045782504428));
#70869=CARTESIAN_POINT('',(41.6385746542983,11.85,-5.43418591165355));
#70870=CARTESIAN_POINT('Ctrl Pts',(41.50625,12.,-5.53045782504427));
#70871=CARTESIAN_POINT('Ctrl Pts',(41.5713537299146,11.9264281650904,-5.48309204365614));
#70872=CARTESIAN_POINT('Ctrl Pts',(41.6385746542983,11.85,-5.43418591165355));
#70873=CARTESIAN_POINT('',(42.2100661590527,11.85,-5.83434857130539));
#70874=CARTESIAN_POINT('Origin',(39.2,11.85,-9.525));
#70875=CARTESIAN_POINT('',(42.1648578496792,12.,-5.99162000611371));
#70876=CARTESIAN_POINT('Ctrl Pts',(42.2100661590527,11.85,-5.83434857130539));
#70877=CARTESIAN_POINT('Ctrl Pts',(42.1871003378909,11.9264281650905,-5.91424246018825));
#70878=CARTESIAN_POINT('Ctrl Pts',(42.1648578496792,12.,-5.99162000611371));
#70879=CARTESIAN_POINT('',(42.3118896374676,11.85,-5.91978861448852));
#70880=CARTESIAN_POINT('Ctrl Pts',(42.1648578496792,12.,-5.99162000611371));
#70881=CARTESIAN_POINT('Ctrl Pts',(42.2371974892713,11.9264281650901,-5.956278961434));
#70882=CARTESIAN_POINT('Ctrl Pts',(42.3118896374676,11.85,-5.91978861448852));
#70883=CARTESIAN_POINT('',(42.8052113855115,11.85,-6.41311036253237));
#70884=CARTESIAN_POINT('Origin',(39.2,11.85,-9.525));
#70885=CARTESIAN_POINT('',(42.7333799938863,12.,-6.56014215032084));
#70886=CARTESIAN_POINT('Ctrl Pts',(42.8052113855115,11.85,-6.41311036253237));
#70887=CARTESIAN_POINT('Ctrl Pts',(42.7687210385659,11.9264281650903,-6.48780251072892));
#70888=CARTESIAN_POINT('Ctrl Pts',(42.7333799938863,12.,-6.56014215032084));
#70889=CARTESIAN_POINT('',(42.8906514286946,11.85,-6.51493384094727));
#70890=CARTESIAN_POINT('Ctrl Pts',(42.7333799938863,12.,-6.56014215032084));
#70891=CARTESIAN_POINT('Ctrl Pts',(42.8107575398122,11.9264281650901,-6.53789966210898));
#70892=CARTESIAN_POINT('Ctrl Pts',(42.8906514286946,11.85,-6.51493384094727));
#70893=CARTESIAN_POINT('',(43.2908140883465,11.85,-7.08642534570167));
#70894=CARTESIAN_POINT('Origin',(39.2,11.85,-9.525));
#70895=CARTESIAN_POINT('',(43.1945421749557,12.,-7.21875000000001));
#70896=CARTESIAN_POINT('Ctrl Pts',(43.2908140883465,11.85,-7.08642534570168));
#70897=CARTESIAN_POINT('Ctrl Pts',(43.2419079563444,11.9264281650897,-7.15364627008465));
#70898=CARTESIAN_POINT('Ctrl Pts',(43.1945421749557,12.,-7.21875000000001));
#70899=CARTESIAN_POINT('',(43.3572746438204,11.85,-7.20153840448187));
#70900=CARTESIAN_POINT('Ctrl Pts',(43.1945421749557,12.,-7.21875000000001));
#70901=CARTESIAN_POINT('Ctrl Pts',(43.2746065496371,11.9264281650904,-7.21028189500509));
#70902=CARTESIAN_POINT('Ctrl Pts',(43.3572746438204,11.85,-7.20153840448187));
#70903=CARTESIAN_POINT('',(43.6521194751588,11.85,-7.83383518576351));
#70904=CARTESIAN_POINT('Origin',(39.2,11.85,-9.525));
#70905=CARTESIAN_POINT('',(43.534332213375,12.,-7.94743208891035));
#70906=CARTESIAN_POINT('Ctrl Pts',(43.6521194751588,11.85,-7.83383518576351));
#70907=CARTESIAN_POINT('Ctrl Pts',(43.5922835461722,11.9264281650908,-7.89154241256252));
#70908=CARTESIAN_POINT('Ctrl Pts',(43.534332213375,12.,-7.94743208891035));
#70909=CARTESIAN_POINT('',(43.6975811725762,11.85,-7.95874017286797));
#70910=CARTESIAN_POINT('Ctrl Pts',(43.534332213375,12.,-7.94743208891035));
#70911=CARTESIAN_POINT('Ctrl Pts',(43.614650701302,11.9264281650903,-7.9529956662175));
#70912=CARTESIAN_POINT('Ctrl Pts',(43.6975811725763,11.85,-7.95874017286797));
#70913=CARTESIAN_POINT('',(43.8781494645997,11.85,-8.63263021293523));
#70914=CARTESIAN_POINT('Origin',(39.2,11.85,-9.525));
#70915=CARTESIAN_POINT('',(43.7424257607688,12.,-8.72404778051128));
#70916=CARTESIAN_POINT('Ctrl Pts',(43.8781494645997,11.85,-8.63263021293523));
#70917=CARTESIAN_POINT('Ctrl Pts',(43.8092018230542,11.9264281650896,-8.67907033726344));
#70918=CARTESIAN_POINT('Ctrl Pts',(43.7424257607688,12.,-8.72404778051128));
#70919=CARTESIAN_POINT('',(43.9012309732892,11.85,-8.76353195353579));
#70920=CARTESIAN_POINT('Ctrl Pts',(43.7424257607688,12.,-8.72404778051128));
#70921=CARTESIAN_POINT('Ctrl Pts',(43.8205579253292,11.92642816509,-8.74347399363942));
#70922=CARTESIAN_POINT('Ctrl Pts',(43.9012309732892,11.85,-8.76353195353579));
#70923=CARTESIAN_POINT('',(43.9620362498165,11.85,-9.45853944452601));
#70924=CARTESIAN_POINT('Origin',(39.2,11.85,-9.525));
#70925=CARTESIAN_POINT('',(43.8125,12.,-9.525));
#70926=CARTESIAN_POINT('Ctrl Pts',(43.9620362498165,11.85,-9.45853944452602));
#70927=CARTESIAN_POINT('Ctrl Pts',(43.8860718349096,11.9264281650904,-9.49230140670684));
#70928=CARTESIAN_POINT('Ctrl Pts',(43.8125,12.,-9.525));
#70929=CARTESIAN_POINT('',(43.9620362498165,11.85,-9.59146055547398));
#70930=CARTESIAN_POINT('Ctrl Pts',(43.8125,12.,-9.525));
#70931=CARTESIAN_POINT('Ctrl Pts',(43.8860718349093,11.9264281650907,-9.55769859329303));
#70932=CARTESIAN_POINT('Ctrl Pts',(43.9620362498165,11.85,-9.59146055547398));
#70933=CARTESIAN_POINT('Origin',(39.2,11.85,-9.525));
#70934=CARTESIAN_POINT('',(43.6975811725762,11.85,-11.091259827132));
#70935=CARTESIAN_POINT('Origin',(39.2,11.85,-9.525));
#70936=CARTESIAN_POINT('',(43.534332213375,12.,-11.1025679110897));
#70937=CARTESIAN_POINT('Ctrl Pts',(43.6975811725763,11.85,-11.091259827132));
#70938=CARTESIAN_POINT('Ctrl Pts',(43.6146507013022,11.9264281650902,-11.0970043337825));
#70939=CARTESIAN_POINT('Ctrl Pts',(43.534332213375,12.,-11.1025679110897));
#70940=CARTESIAN_POINT('',(43.6521194751588,11.85,-11.2161648142365));
#70941=CARTESIAN_POINT('Ctrl Pts',(43.534332213375,12.,-11.1025679110897));
#70942=CARTESIAN_POINT('Ctrl Pts',(43.5922835461725,11.9264281650904,-11.1584575874378));
#70943=CARTESIAN_POINT('Ctrl Pts',(43.6521194751588,11.85,-11.2161648142365));
#70944=CARTESIAN_POINT('',(43.3572746438204,11.85,-11.8484615955181));
#70945=CARTESIAN_POINT('Origin',(39.2,11.85,-9.525));
#70946=CARTESIAN_POINT('',(43.1945421749557,12.,-11.83125));
#70947=CARTESIAN_POINT('Ctrl Pts',(43.3572746438204,11.85,-11.8484615955181));
#70948=CARTESIAN_POINT('Ctrl Pts',(43.274606549637,11.9264281650904,-11.8397181049949));
#70949=CARTESIAN_POINT('Ctrl Pts',(43.1945421749557,12.,-11.83125));
#70950=CARTESIAN_POINT('',(43.2908140883465,11.85,-11.9635746542983));
#70951=CARTESIAN_POINT('Ctrl Pts',(43.1945421749557,12.,-11.83125));
#70952=CARTESIAN_POINT('Ctrl Pts',(43.2419079563437,11.9264281650907,-11.8963537299144));
#70953=CARTESIAN_POINT('Ctrl Pts',(43.2908140883465,11.85,-11.9635746542984));
#70954=CARTESIAN_POINT('',(42.8906514286946,11.85,-12.5350661590527));
#70955=CARTESIAN_POINT('Origin',(39.2,11.85,-9.525));
#70956=CARTESIAN_POINT('',(42.7333799938863,12.,-12.4898578496792));
#70957=CARTESIAN_POINT('Ctrl Pts',(42.8906514286946,11.85,-12.5350661590527));
#70958=CARTESIAN_POINT('Ctrl Pts',(42.8107575398114,11.9264281650908,-12.5121003378908));
#70959=CARTESIAN_POINT('Ctrl Pts',(42.7333799938863,12.,-12.4898578496792));
#70960=CARTESIAN_POINT('',(42.8052113855115,11.85,-12.6368896374676));
#70961=CARTESIAN_POINT('Ctrl Pts',(42.7333799938863,12.,-12.4898578496792));
#70962=CARTESIAN_POINT('Ctrl Pts',(42.7687210385655,11.9264281650911,-12.5621974892703));
#70963=CARTESIAN_POINT('Ctrl Pts',(42.8052113855115,11.85,-12.6368896374676));
#70964=CARTESIAN_POINT('',(42.3118896374676,11.85,-13.1302113855115));
#70965=CARTESIAN_POINT('Origin',(39.2,11.85,-9.525));
#70966=CARTESIAN_POINT('',(42.1648578496792,12.,-13.0583799938863));
#70967=CARTESIAN_POINT('Ctrl Pts',(42.3118896374676,11.85,-13.1302113855115));
#70968=CARTESIAN_POINT('Ctrl Pts',(42.2371974892713,11.9264281650901,-13.093721038566));
#70969=CARTESIAN_POINT('Ctrl Pts',(42.1648578496792,12.,-13.0583799938863));
#70970=CARTESIAN_POINT('',(42.2100661590527,11.85,-13.2156514286946));
#70971=CARTESIAN_POINT('Ctrl Pts',(42.1648578496792,12.,-13.0583799938863));
#70972=CARTESIAN_POINT('Ctrl Pts',(42.1871003378909,11.9264281650906,-13.1357575398117));
#70973=CARTESIAN_POINT('Ctrl Pts',(42.2100661590527,11.85,-13.2156514286946));
#70974=CARTESIAN_POINT('',(41.6385746542983,11.85,-13.6158140883464));
#70975=CARTESIAN_POINT('Origin',(39.2,11.85,-9.525));
#70976=CARTESIAN_POINT('',(41.50625,12.,-13.5195421749557));
#70977=CARTESIAN_POINT('Ctrl Pts',(41.6385746542983,11.85,-13.6158140883465));
#70978=CARTESIAN_POINT('Ctrl Pts',(41.5713537299148,11.9264281650902,-13.566907956344));
#70979=CARTESIAN_POINT('Ctrl Pts',(41.50625,12.,-13.5195421749557));
#70980=CARTESIAN_POINT('',(41.5234615955181,11.85,-13.6822746438204));
#70981=CARTESIAN_POINT('Ctrl Pts',(41.50625,12.,-13.5195421749557));
#70982=CARTESIAN_POINT('Ctrl Pts',(41.5147181049949,11.9264281650903,-13.5996065496372));
#70983=CARTESIAN_POINT('Ctrl Pts',(41.5234615955181,11.85,-13.6822746438204));
#70984=CARTESIAN_POINT('',(40.8911648142365,11.85,-13.9771194751588));
#70985=CARTESIAN_POINT('Origin',(39.2,11.85,-9.525));
#70986=CARTESIAN_POINT('',(40.7775679110896,12.,-13.859332213375));
#70987=CARTESIAN_POINT('Ctrl Pts',(40.8911648142365,11.85,-13.9771194751588));
#70988=CARTESIAN_POINT('Ctrl Pts',(40.8334575874381,11.92642816509,-13.9172835461729));
#70989=CARTESIAN_POINT('Ctrl Pts',(40.7775679110896,12.,-13.859332213375));
#70990=CARTESIAN_POINT('',(40.766259827132,11.85,-14.0225811725762));
#70991=CARTESIAN_POINT('Ctrl Pts',(40.7775679110896,12.,-13.859332213375));
#70992=CARTESIAN_POINT('Ctrl Pts',(40.7720043337825,11.9264281650902,-13.9396507013022));
#70993=CARTESIAN_POINT('Ctrl Pts',(40.766259827132,11.85,-14.0225811725763));
#70994=CARTESIAN_POINT('',(40.0923697870648,11.85,-14.2031494645996));
#70995=CARTESIAN_POINT('Origin',(39.2,11.85,-9.525));
#70996=CARTESIAN_POINT('',(40.0009522194887,12.,-14.0674257607688));
#70997=CARTESIAN_POINT('Ctrl Pts',(40.0923697870648,11.85,-14.2031494645997));
#70998=CARTESIAN_POINT('Ctrl Pts',(40.0459296627363,11.92642816509,-14.1342018230539));
#70999=CARTESIAN_POINT('Ctrl Pts',(40.0009522194887,12.,-14.0674257607688));
#71000=CARTESIAN_POINT('',(39.9614680464642,11.85,-14.2262309732892));
#71001=CARTESIAN_POINT('Ctrl Pts',(40.0009522194887,12.,-14.0674257607688));
#71002=CARTESIAN_POINT('Ctrl Pts',(39.9815260063607,11.9264281650904,-14.1455579253287));
#71003=CARTESIAN_POINT('Ctrl Pts',(39.9614680464642,11.85,-14.2262309732892));
#71004=CARTESIAN_POINT('',(39.266460555474,11.85,-14.2870362498165));
#71005=CARTESIAN_POINT('Origin',(39.2,11.85,-9.525));
#71006=CARTESIAN_POINT('',(39.2,12.,-14.1375));
#71007=CARTESIAN_POINT('Ctrl Pts',(39.266460555474,11.85,-14.2870362498165));
#71008=CARTESIAN_POINT('Ctrl Pts',(39.2326985932933,11.9264281650901,-14.2110718349099));
#71009=CARTESIAN_POINT('Ctrl Pts',(39.2,12.,-14.1375));
#71010=CARTESIAN_POINT('',(39.133539444526,11.85,-14.2870362498165));
#71011=CARTESIAN_POINT('Ctrl Pts',(39.2,12.,-14.1375));
#71012=CARTESIAN_POINT('Ctrl Pts',(39.1673014067067,11.9264281650901,-14.2110718349099));
#71013=CARTESIAN_POINT('Ctrl Pts',(39.133539444526,11.85,-14.2870362498165));
#71014=CARTESIAN_POINT('',(38.4385319535358,11.85,-14.2262309732892));
#71015=CARTESIAN_POINT('Origin',(39.2,11.85,-9.525));
#71016=CARTESIAN_POINT('',(38.3990477805113,12.,-14.0674257607688));
#71017=CARTESIAN_POINT('Ctrl Pts',(38.4385319535358,11.85,-14.2262309732892));
#71018=CARTESIAN_POINT('Ctrl Pts',(38.4184739936393,11.9264281650903,-14.1455579253288));
#71019=CARTESIAN_POINT('Ctrl Pts',(38.3990477805113,12.,-14.0674257607688));
#71020=CARTESIAN_POINT('',(38.3076302129352,11.85,-14.2031494645996));
#71021=CARTESIAN_POINT('Ctrl Pts',(38.3990477805113,12.,-14.0674257607688));
#71022=CARTESIAN_POINT('Ctrl Pts',(38.3540703372637,11.92642816509,-14.1342018230538));
#71023=CARTESIAN_POINT('Ctrl Pts',(38.3076302129352,11.85,-14.2031494645997));
#71024=CARTESIAN_POINT('',(37.633740172868,11.85,-14.0225811725762));
#71025=CARTESIAN_POINT('Origin',(39.2,11.85,-9.525));
#71026=CARTESIAN_POINT('',(37.6224320889104,12.,-13.859332213375));
#71027=CARTESIAN_POINT('Ctrl Pts',(37.633740172868,11.85,-14.0225811725763));
#71028=CARTESIAN_POINT('Ctrl Pts',(37.6279956662175,11.9264281650903,-13.9396507013021));
#71029=CARTESIAN_POINT('Ctrl Pts',(37.6224320889104,12.,-13.859332213375));
#71030=CARTESIAN_POINT('',(37.5088351857635,11.85,-13.9771194751588));
#71031=CARTESIAN_POINT('Ctrl Pts',(37.6224320889104,12.,-13.859332213375));
#71032=CARTESIAN_POINT('Ctrl Pts',(37.566542412562,11.9264281650902,-13.9172835461727));
#71033=CARTESIAN_POINT('Ctrl Pts',(37.5088351857635,11.85,-13.9771194751588));
#71034=CARTESIAN_POINT('',(36.8765384044819,11.85,-13.6822746438204));
#71035=CARTESIAN_POINT('Origin',(39.2,11.85,-9.525));
#71036=CARTESIAN_POINT('',(36.89375,12.,-13.5195421749557));
#71037=CARTESIAN_POINT('Ctrl Pts',(36.8765384044819,11.85,-13.6822746438204));
#71038=CARTESIAN_POINT('Ctrl Pts',(36.8852818950051,11.92642816509,-13.5996065496374));
#71039=CARTESIAN_POINT('Ctrl Pts',(36.89375,12.,-13.5195421749557));
#71040=CARTESIAN_POINT('',(36.7614253457017,11.85,-13.6158140883464));
#71041=CARTESIAN_POINT('Ctrl Pts',(36.89375,12.,-13.5195421749557));
#71042=CARTESIAN_POINT('Ctrl Pts',(36.8286462700851,11.9264281650902,-13.566907956344));
#71043=CARTESIAN_POINT('Ctrl Pts',(36.7614253457017,11.85,-13.6158140883465));
#71044=CARTESIAN_POINT('',(36.1899338409473,11.85,-13.2156514286946));
#71045=CARTESIAN_POINT('Origin',(39.2,11.85,-9.525));
#71046=CARTESIAN_POINT('',(36.2351421503208,12.,-13.0583799938863));
#71047=CARTESIAN_POINT('Ctrl Pts',(36.1899338409473,11.85,-13.2156514286946));
#71048=CARTESIAN_POINT('Ctrl Pts',(36.212899662109,11.9264281650902,-13.1357575398121));
#71049=CARTESIAN_POINT('Ctrl Pts',(36.2351421503208,12.,-13.0583799938863));
#71050=CARTESIAN_POINT('',(36.0881103625324,11.85,-13.1302113855115));
#71051=CARTESIAN_POINT('Ctrl Pts',(36.2351421503208,12.,-13.0583799938863));
#71052=CARTESIAN_POINT('Ctrl Pts',(36.1628025107289,11.9264281650903,-13.0937210385659));
#71053=CARTESIAN_POINT('Ctrl Pts',(36.0881103625324,11.85,-13.1302113855115));
#71054=CARTESIAN_POINT('',(35.5947886144885,11.85,-12.6368896374676));
#71055=CARTESIAN_POINT('Origin',(39.2,11.85,-9.525));
#71056=CARTESIAN_POINT('',(35.6666200061137,12.,-12.4898578496792));
#71057=CARTESIAN_POINT('Ctrl Pts',(35.5947886144885,11.85,-12.6368896374676));
#71058=CARTESIAN_POINT('Ctrl Pts',(35.6312789614341,11.9264281650903,-12.5621974892711));
#71059=CARTESIAN_POINT('Ctrl Pts',(35.6666200061137,12.,-12.4898578496792));
#71060=CARTESIAN_POINT('',(35.5093485713054,11.85,-12.5350661590527));
#71061=CARTESIAN_POINT('Ctrl Pts',(35.6666200061137,12.,-12.4898578496792));
#71062=CARTESIAN_POINT('Ctrl Pts',(35.589242460188,11.9264281650903,-12.512100337891));
#71063=CARTESIAN_POINT('Ctrl Pts',(35.5093485713054,11.85,-12.5350661590527));
#71064=CARTESIAN_POINT('',(35.1091859116536,11.85,-11.9635746542983));
#71065=CARTESIAN_POINT('Origin',(39.2,11.85,-9.525));
#71066=CARTESIAN_POINT('',(35.2054578250443,12.,-11.83125));
#71067=CARTESIAN_POINT('Ctrl Pts',(35.1091859116536,11.85,-11.9635746542983));
#71068=CARTESIAN_POINT('Ctrl Pts',(35.158092043656,11.9264281650902,-11.8963537299149));
#71069=CARTESIAN_POINT('Ctrl Pts',(35.2054578250443,12.,-11.83125));
#71070=CARTESIAN_POINT('',(35.0427253561796,11.85,-11.8484615955181));
#71071=CARTESIAN_POINT('Ctrl Pts',(35.2054578250443,12.,-11.83125));
#71072=CARTESIAN_POINT('Ctrl Pts',(35.1253934503631,11.9264281650906,-11.8397181049949));
#71073=CARTESIAN_POINT('Ctrl Pts',(35.0427253561796,11.85,-11.8484615955181));
#71074=CARTESIAN_POINT('',(34.7478805248412,11.85,-11.2161648142365));
#71075=CARTESIAN_POINT('Origin',(39.2,11.85,-9.525));
#71076=CARTESIAN_POINT('',(34.865667786625,12.,-11.1025679110896));
#71077=CARTESIAN_POINT('Ctrl Pts',(34.7478805248412,11.85,-11.2161648142365));
#71078=CARTESIAN_POINT('Ctrl Pts',(34.8077164538272,11.92642816509,-11.1584575874381));
#71079=CARTESIAN_POINT('Ctrl Pts',(34.865667786625,12.,-11.1025679110896));
#71080=CARTESIAN_POINT('',(34.7024188274238,11.85,-11.091259827132));
#71081=CARTESIAN_POINT('Ctrl Pts',(34.865667786625,12.,-11.1025679110896));
#71082=CARTESIAN_POINT('Ctrl Pts',(34.7853492986983,11.9264281650906,-11.0970043337825));
#71083=CARTESIAN_POINT('Ctrl Pts',(34.7024188274237,11.85,-11.091259827132));
#71084=CARTESIAN_POINT('',(34.5218505354004,11.85,-10.4173697870648));
#71085=CARTESIAN_POINT('Origin',(39.2,11.85,-9.525));
#71086=CARTESIAN_POINT('',(34.6575742392312,12.,-10.3259522194887));
#71087=CARTESIAN_POINT('Ctrl Pts',(34.5218505354003,11.85,-10.4173697870648));
#71088=CARTESIAN_POINT('Ctrl Pts',(34.5907981769464,11.9264281650903,-10.3709296627361));
#71089=CARTESIAN_POINT('Ctrl Pts',(34.6575742392312,12.,-10.3259522194887));
#71090=CARTESIAN_POINT('',(34.4987690267108,11.85,-10.2864680464642));
#71091=CARTESIAN_POINT('Ctrl Pts',(34.6575742392312,12.,-10.3259522194887));
#71092=CARTESIAN_POINT('Ctrl Pts',(34.5794420746714,11.9264281650906,-10.3065260063607));
#71093=CARTESIAN_POINT('Ctrl Pts',(34.4987690267108,11.85,-10.2864680464642));
#71094=CARTESIAN_POINT('',(34.4379637501835,11.85,-9.59146055547398));
#71095=CARTESIAN_POINT('Origin',(39.2,11.85,-9.525));
#71096=CARTESIAN_POINT('Ctrl Pts',(34.4379637501835,11.85,-9.59146055547399));
#71097=CARTESIAN_POINT('Ctrl Pts',(34.5139281650899,11.9264281650899,-9.55769859329336));
#71098=CARTESIAN_POINT('Ctrl Pts',(34.5875,12.,-9.525));
#71099=CARTESIAN_POINT('',(34.8375,12.25,-9.525));
#71100=CARTESIAN_POINT('',(34.6375,12.05,-9.525));
#71101=CARTESIAN_POINT('Origin',(39.2,12.25,-9.525));
#71102=CARTESIAN_POINT('Origin',(44.0255979213938,12.25,-11.068538451429));
#71103=CARTESIAN_POINT('',(43.6975811725762,6.5,-11.091259827132));
#71104=CARTESIAN_POINT('',(43.6975811725762,5.9,-11.091259827132));
#71105=CARTESIAN_POINT('',(43.534332213375,6.5,-11.1025679110896));
#71106=CARTESIAN_POINT('',(44.0255979213938,6.5,-11.068538451429));
#71107=CARTESIAN_POINT('',(43.534332213375,12.25,-11.1025679110896));
#71108=CARTESIAN_POINT('Origin',(43.534332213375,12.25,-11.1025679110896));
#71109=CARTESIAN_POINT('',(43.6521194751588,6.5,-11.2161648142365));
#71110=CARTESIAN_POINT('',(43.6521194751588,5.9,-11.2161648142365));
#71111=CARTESIAN_POINT('',(43.534332213375,6.5,-11.1025679110896));
#71112=CARTESIAN_POINT('Origin',(43.7457630530518,6.5,-11.1795224433379));
#71113=CARTESIAN_POINT('Origin',(39.2,6.5,-9.525));
#71114=CARTESIAN_POINT('Origin',(43.6842536066587,12.25,-11.8830449192431));
#71115=CARTESIAN_POINT('',(43.3572746438204,6.5,-11.8484615955181));
#71116=CARTESIAN_POINT('',(43.3572746438204,5.9,-11.8484615955181));
#71117=CARTESIAN_POINT('',(43.1945421749557,6.5,-11.83125));
#71118=CARTESIAN_POINT('',(43.6842536066587,6.5,-11.8830449192431));
#71119=CARTESIAN_POINT('',(43.1945421749557,12.25,-11.83125));
#71120=CARTESIAN_POINT('Origin',(43.1945421749557,12.25,-11.83125));
#71121=CARTESIAN_POINT('',(43.2908140883465,6.5,-11.9635746542983));
#71122=CARTESIAN_POINT('',(43.2908140883465,5.9,-11.9635746542983));
#71123=CARTESIAN_POINT('',(43.1945421749557,6.5,-11.83125));
#71124=CARTESIAN_POINT('Origin',(43.3893978908072,6.5,-11.94375));
#71125=CARTESIAN_POINT('Origin',(39.2,6.5,-9.525));
#71126=CARTESIAN_POINT('Origin',(43.2066575152271,12.25,-12.6259033854143));
#71127=CARTESIAN_POINT('',(42.8906514286946,6.5,-12.5350661590527));
#71128=CARTESIAN_POINT('',(42.8906514286946,5.9,-12.5350661590527));
#71129=CARTESIAN_POINT('',(42.7333799938863,6.5,-12.4898578496792));
#71130=CARTESIAN_POINT('',(43.2066575152271,6.5,-12.6259033854143));
#71131=CARTESIAN_POINT('',(42.7333799938863,12.25,-12.4898578496792));
#71132=CARTESIAN_POINT('Origin',(42.7333799938863,12.25,-12.4898578496792));
#71133=CARTESIAN_POINT('',(42.8052113855115,6.5,-12.6368896374676));
#71134=CARTESIAN_POINT('',(42.8052113855115,5.9,-12.6368896374676));
#71135=CARTESIAN_POINT('',(42.7333799938863,6.5,-12.4898578496792));
#71136=CARTESIAN_POINT('Origin',(42.9057399935881,6.5,-12.6344850618586));
#71137=CARTESIAN_POINT('Origin',(39.2,6.5,-9.525));
#71138=CARTESIAN_POINT('Origin',(42.6073211626619,12.25,-13.2745424713525));
#71139=CARTESIAN_POINT('',(42.3118896374676,6.5,-13.1302113855115));
#71140=CARTESIAN_POINT('',(42.3118896374676,5.9,-13.1302113855115));
#71141=CARTESIAN_POINT('',(42.1648578496792,6.5,-13.0583799938863));
#71142=CARTESIAN_POINT('',(42.6073211626619,6.5,-13.2745424713525));
#71143=CARTESIAN_POINT('',(42.1648578496792,12.25,-13.0583799938863));
#71144=CARTESIAN_POINT('Origin',(42.1648578496792,12.25,-13.0583799938863));
#71145=CARTESIAN_POINT('',(42.2100661590527,6.5,-13.2156514286946));
#71146=CARTESIAN_POINT('',(42.2100661590527,5.9,-13.2156514286946));
#71147=CARTESIAN_POINT('',(42.1648578496792,6.5,-13.0583799938863));
#71148=CARTESIAN_POINT('Origin',(42.3094850618586,6.5,-13.2307399935881));
#71149=CARTESIAN_POINT('Origin',(39.2,6.5,-9.525));
#71150=CARTESIAN_POINT('Origin',(41.9044550807569,12.25,-13.8092536066587));
#71151=CARTESIAN_POINT('',(41.6385746542983,6.5,-13.6158140883464));
#71152=CARTESIAN_POINT('',(41.6385746542983,5.9,-13.6158140883464));
#71153=CARTESIAN_POINT('',(41.50625,6.5,-13.5195421749557));
#71154=CARTESIAN_POINT('',(41.9044550807569,6.5,-13.8092536066587));
#71155=CARTESIAN_POINT('',(41.50625,12.25,-13.5195421749557));
#71156=CARTESIAN_POINT('Origin',(41.50625,12.25,-13.5195421749557));
#71157=CARTESIAN_POINT('',(41.5234615955181,6.5,-13.6822746438204));
#71158=CARTESIAN_POINT('',(41.5234615955181,5.9,-13.6822746438204));
#71159=CARTESIAN_POINT('',(41.50625,6.5,-13.5195421749557));
#71160=CARTESIAN_POINT('Origin',(41.61875,6.5,-13.7143978908072));
#71161=CARTESIAN_POINT('Origin',(39.2,6.5,-9.525));
#71162=CARTESIAN_POINT('Origin',(41.1194154997434,12.25,-14.2137898640635));
#71163=CARTESIAN_POINT('',(40.8911648142365,6.5,-13.9771194751588));
#71164=CARTESIAN_POINT('',(40.8911648142365,5.9,-13.9771194751588));
#71165=CARTESIAN_POINT('',(40.7775679110896,6.5,-13.859332213375));
#71166=CARTESIAN_POINT('',(41.1194154997434,6.5,-14.2137898640635));
#71167=CARTESIAN_POINT('',(40.7775679110896,12.25,-13.859332213375));
#71168=CARTESIAN_POINT('Origin',(40.7775679110896,12.25,-13.859332213375));
#71169=CARTESIAN_POINT('',(40.766259827132,6.5,-14.0225811725762));
#71170=CARTESIAN_POINT('',(40.766259827132,5.9,-14.0225811725762));
#71171=CARTESIAN_POINT('',(40.7775679110896,6.5,-13.859332213375));
#71172=CARTESIAN_POINT('Origin',(40.8545224433379,6.5,-14.0707630530518));
#71173=CARTESIAN_POINT('Origin',(39.2,6.5,-9.525));
#71174=CARTESIAN_POINT('Origin',(40.2760554500413,12.25,-14.4758596140909));
#71175=CARTESIAN_POINT('',(40.0923697870648,6.5,-14.2031494645996));
#71176=CARTESIAN_POINT('',(40.0923697870648,5.9,-14.2031494645996));
#71177=CARTESIAN_POINT('',(40.0009522194887,6.5,-14.0674257607688));
#71178=CARTESIAN_POINT('',(40.2760554500413,6.5,-14.4758596140909));
#71179=CARTESIAN_POINT('',(40.0009522194887,12.25,-14.0674257607688));
#71180=CARTESIAN_POINT('Origin',(40.0009522194887,12.25,-14.0674257607688));
#71181=CARTESIAN_POINT('',(39.9614680464642,6.5,-14.2262309732892));
#71182=CARTESIAN_POINT('',(39.9614680464642,5.9,-14.2262309732892));
#71183=CARTESIAN_POINT('',(40.0009522194887,6.5,-14.0674257607688));
#71184=CARTESIAN_POINT('Origin',(40.0400230594638,6.5,-14.2890075051966));
#71185=CARTESIAN_POINT('Origin',(39.2,6.5,-9.525));
#71186=CARTESIAN_POINT('Origin',(39.4,12.25,-14.5875));
#71187=CARTESIAN_POINT('',(39.266460555474,6.5,-14.2870362498165));
#71188=CARTESIAN_POINT('',(39.266460555474,5.9,-14.2870362498165));
#71189=CARTESIAN_POINT('',(39.2,6.5,-14.1375));
#71190=CARTESIAN_POINT('',(39.4,6.5,-14.5875));
#71191=CARTESIAN_POINT('',(39.2,12.25,-14.1375));
#71192=CARTESIAN_POINT('Origin',(39.2,12.25,-14.1375));
#71193=CARTESIAN_POINT('',(39.133539444526,6.5,-14.2870362498165));
#71194=CARTESIAN_POINT('',(39.133539444526,5.9,-14.2870362498165));
#71195=CARTESIAN_POINT('',(39.2,6.5,-14.1375));
#71196=CARTESIAN_POINT('Origin',(39.2,6.5,-14.3625));
#71197=CARTESIAN_POINT('Origin',(39.2,6.5,-9.525));
#71198=CARTESIAN_POINT('Origin',(38.5178676511636,12.25,-14.5453188851577));
#71199=CARTESIAN_POINT('',(38.4385319535358,6.5,-14.2262309732892));
#71200=CARTESIAN_POINT('',(38.4385319535358,5.9,-14.2262309732892));
#71201=CARTESIAN_POINT('',(38.3990477805113,6.5,-14.0674257607688));
#71202=CARTESIAN_POINT('',(38.5178676511636,6.5,-14.5453188851577));
#71203=CARTESIAN_POINT('',(38.3990477805113,12.25,-14.0674257607688));
#71204=CARTESIAN_POINT('Origin',(38.3990477805113,12.25,-14.0674257607688));
#71205=CARTESIAN_POINT('',(38.3076302129352,6.5,-14.2031494645996));
#71206=CARTESIAN_POINT('',(38.3076302129352,5.9,-14.2031494645996));
#71207=CARTESIAN_POINT('',(38.3990477805113,6.5,-14.0674257607688));
#71208=CARTESIAN_POINT('Origin',(38.3599769405362,6.5,-14.2890075051966));
#71209=CARTESIAN_POINT('Origin',(39.2,6.5,-9.525));
#71210=CARTESIAN_POINT('Origin',(37.656461548571,12.25,-14.3505979213938));
#71211=CARTESIAN_POINT('',(37.633740172868,6.5,-14.0225811725762));
#71212=CARTESIAN_POINT('',(37.633740172868,5.9,-14.0225811725762));
#71213=CARTESIAN_POINT('',(37.6224320889104,6.5,-13.859332213375));
#71214=CARTESIAN_POINT('',(37.656461548571,6.5,-14.3505979213938));
#71215=CARTESIAN_POINT('',(37.6224320889104,12.25,-13.859332213375));
#71216=CARTESIAN_POINT('Origin',(37.6224320889104,12.25,-13.859332213375));
#71217=CARTESIAN_POINT('',(37.5088351857635,6.5,-13.9771194751588));
#71218=CARTESIAN_POINT('',(37.5088351857635,5.9,-13.9771194751588));
#71219=CARTESIAN_POINT('',(37.6224320889104,6.5,-13.859332213375));
#71220=CARTESIAN_POINT('Origin',(37.5454775566621,6.5,-14.0707630530518));
#71221=CARTESIAN_POINT('Origin',(39.2,6.5,-9.525));
#71222=CARTESIAN_POINT('Origin',(36.8419550807569,12.25,-14.0092536066587));
#71223=CARTESIAN_POINT('',(36.8765384044819,6.5,-13.6822746438204));
#71224=CARTESIAN_POINT('',(36.8765384044819,5.9,-13.6822746438204));
#71225=CARTESIAN_POINT('',(36.89375,6.5,-13.5195421749557));
#71226=CARTESIAN_POINT('',(36.8419550807569,6.5,-14.0092536066587));
#71227=CARTESIAN_POINT('',(36.89375,12.25,-13.5195421749557));
#71228=CARTESIAN_POINT('Origin',(36.89375,12.25,-13.5195421749557));
#71229=CARTESIAN_POINT('',(36.7614253457017,6.5,-13.6158140883464));
#71230=CARTESIAN_POINT('',(36.7614253457017,5.9,-13.6158140883464));
#71231=CARTESIAN_POINT('',(36.89375,6.5,-13.5195421749557));
#71232=CARTESIAN_POINT('Origin',(36.78125,6.5,-13.7143978908072));
#71233=CARTESIAN_POINT('Origin',(39.2,6.5,-9.525));
#71234=CARTESIAN_POINT('Origin',(36.0990966145857,12.25,-13.5316575152271));
#71235=CARTESIAN_POINT('',(36.1899338409473,6.5,-13.2156514286946));
#71236=CARTESIAN_POINT('',(36.1899338409473,5.9,-13.2156514286946));
#71237=CARTESIAN_POINT('',(36.2351421503208,6.5,-13.0583799938863));
#71238=CARTESIAN_POINT('',(36.0990966145857,6.5,-13.5316575152271));
#71239=CARTESIAN_POINT('',(36.2351421503208,12.25,-13.0583799938863));
#71240=CARTESIAN_POINT('Origin',(36.2351421503208,12.25,-13.0583799938863));
#71241=CARTESIAN_POINT('',(36.0881103625324,6.5,-13.1302113855115));
#71242=CARTESIAN_POINT('',(36.0881103625324,5.9,-13.1302113855115));
#71243=CARTESIAN_POINT('',(36.2351421503208,6.5,-13.0583799938863));
#71244=CARTESIAN_POINT('Origin',(36.0905149381414,6.5,-13.2307399935881));
#71245=CARTESIAN_POINT('Origin',(39.2,6.5,-9.525));
#71246=CARTESIAN_POINT('Origin',(35.4504575286475,12.25,-12.9323211626619));
#71247=CARTESIAN_POINT('',(35.5947886144885,6.5,-12.6368896374676));
#71248=CARTESIAN_POINT('',(35.5947886144885,5.9,-12.6368896374676));
#71249=CARTESIAN_POINT('',(35.6666200061137,6.5,-12.4898578496792));
#71250=CARTESIAN_POINT('',(35.4504575286475,6.5,-12.9323211626619));
#71251=CARTESIAN_POINT('',(35.6666200061137,12.25,-12.4898578496792));
#71252=CARTESIAN_POINT('Origin',(35.6666200061137,12.25,-12.4898578496792));
#71253=CARTESIAN_POINT('',(35.5093485713054,6.5,-12.5350661590527));
#71254=CARTESIAN_POINT('',(35.5093485713054,5.9,-12.5350661590527));
#71255=CARTESIAN_POINT('',(35.6666200061137,6.5,-12.4898578496792));
#71256=CARTESIAN_POINT('Origin',(35.4942600064119,6.5,-12.6344850618586));
#71257=CARTESIAN_POINT('Origin',(39.2,6.5,-9.525));
#71258=CARTESIAN_POINT('Origin',(34.9157463933413,12.25,-12.2294550807569));
#71259=CARTESIAN_POINT('',(35.1091859116536,6.5,-11.9635746542983));
#71260=CARTESIAN_POINT('',(35.1091859116536,5.9,-11.9635746542983));
#71261=CARTESIAN_POINT('',(35.2054578250443,6.5,-11.83125));
#71262=CARTESIAN_POINT('',(34.9157463933413,6.5,-12.2294550807569));
#71263=CARTESIAN_POINT('',(35.2054578250443,12.25,-11.83125));
#71264=CARTESIAN_POINT('Origin',(35.2054578250443,12.25,-11.83125));
#71265=CARTESIAN_POINT('',(35.0427253561796,6.5,-11.8484615955181));
#71266=CARTESIAN_POINT('',(35.0427253561796,5.9,-11.8484615955181));
#71267=CARTESIAN_POINT('',(35.2054578250443,6.5,-11.83125));
#71268=CARTESIAN_POINT('Origin',(35.0106021091928,6.5,-11.94375));
#71269=CARTESIAN_POINT('Origin',(39.2,6.5,-9.525));
#71270=CARTESIAN_POINT('Origin',(34.5112101359365,12.25,-11.4444154997434));
#71271=CARTESIAN_POINT('',(34.7478805248412,6.5,-11.2161648142365));
#71272=CARTESIAN_POINT('',(34.7478805248412,5.9,-11.2161648142365));
#71273=CARTESIAN_POINT('',(34.865667786625,6.5,-11.1025679110896));
#71274=CARTESIAN_POINT('',(34.5112101359365,6.5,-11.4444154997434));
#71275=CARTESIAN_POINT('',(34.865667786625,12.25,-11.1025679110896));
#71276=CARTESIAN_POINT('Origin',(34.865667786625,12.25,-11.1025679110896));
#71277=CARTESIAN_POINT('',(34.7024188274238,6.5,-11.091259827132));
#71278=CARTESIAN_POINT('',(34.7024188274238,5.9,-11.091259827132));
#71279=CARTESIAN_POINT('',(34.865667786625,6.5,-11.1025679110896));
#71280=CARTESIAN_POINT('Origin',(34.6542369469482,6.5,-11.1795224433379));
#71281=CARTESIAN_POINT('Origin',(39.2,6.5,-9.525));
#71282=CARTESIAN_POINT('Origin',(34.2491403859091,12.25,-10.6010554500413));
#71283=CARTESIAN_POINT('',(34.5218505354004,6.5,-10.4173697870648));
#71284=CARTESIAN_POINT('',(34.5218505354004,5.9,-10.4173697870648));
#71285=CARTESIAN_POINT('',(34.6575742392312,6.5,-10.3259522194887));
#71286=CARTESIAN_POINT('',(34.2491403859091,6.5,-10.6010554500413));
#71287=CARTESIAN_POINT('',(34.6575742392312,12.25,-10.3259522194887));
#71288=CARTESIAN_POINT('Origin',(34.6575742392312,12.25,-10.3259522194887));
#71289=CARTESIAN_POINT('',(34.4987690267108,6.5,-10.2864680464642));
#71290=CARTESIAN_POINT('',(34.4987690267108,5.9,-10.2864680464642));
#71291=CARTESIAN_POINT('',(34.6575742392312,6.5,-10.3259522194887));
#71292=CARTESIAN_POINT('Origin',(34.4359924948034,6.5,-10.3650230594638));
#71293=CARTESIAN_POINT('Origin',(39.2,6.5,-9.525));
#71294=CARTESIAN_POINT('Origin',(34.1375,12.25,-9.725));
#71295=CARTESIAN_POINT('',(34.4379637501835,6.5,-9.59146055547398));
#71296=CARTESIAN_POINT('',(34.4379637501835,5.9,-9.59146055547398));
#71297=CARTESIAN_POINT('',(34.5875,6.5,-9.525));
#71298=CARTESIAN_POINT('',(34.1375,6.5,-9.725));
#71299=CARTESIAN_POINT('',(34.5875,12.25,-9.525));
#71300=CARTESIAN_POINT('Origin',(34.5875,12.25,-9.525));
#71301=CARTESIAN_POINT('',(34.4379637501835,6.5,-9.45853944452601));
#71302=CARTESIAN_POINT('',(34.4379637501835,5.9,-9.45853944452601));
#71303=CARTESIAN_POINT('',(34.5875,6.5,-9.525));
#71304=CARTESIAN_POINT('Origin',(34.3625,6.5,-9.525));
#71305=CARTESIAN_POINT('',(34.4375,6.5,-9.525));
#71306=CARTESIAN_POINT('Origin',(39.2,6.5,-9.525));
#71307=CARTESIAN_POINT('Origin',(39.2,6.5,-9.525));
#71308=CARTESIAN_POINT('Origin',(34.1796811148423,12.25,-8.84286765116361));
#71309=CARTESIAN_POINT('',(34.4987690267108,6.5,-8.76353195353579));
#71310=CARTESIAN_POINT('',(34.4987690267108,5.9,-8.76353195353579));
#71311=CARTESIAN_POINT('',(34.6575742392312,6.5,-8.72404778051128));
#71312=CARTESIAN_POINT('',(34.1796811148423,6.5,-8.84286765116361));
#71313=CARTESIAN_POINT('',(34.6575742392312,12.25,-8.72404778051128));
#71314=CARTESIAN_POINT('Origin',(34.6575742392312,12.25,-8.72404778051128));
#71315=CARTESIAN_POINT('',(34.5218505354004,6.5,-8.63263021293523));
#71316=CARTESIAN_POINT('',(34.5218505354004,5.9,-8.63263021293523));
#71317=CARTESIAN_POINT('',(34.6575742392312,6.5,-8.72404778051128));
#71318=CARTESIAN_POINT('Origin',(34.4359924948035,6.5,-8.68497694053623));
#71319=CARTESIAN_POINT('Origin',(39.2,6.5,-9.525));
#71320=CARTESIAN_POINT('Origin',(34.3744020786062,12.25,-7.98146154857098));
#71321=CARTESIAN_POINT('',(34.7024188274238,6.5,-7.95874017286797));
#71322=CARTESIAN_POINT('',(34.7024188274238,5.9,-7.95874017286797));
#71323=CARTESIAN_POINT('',(34.865667786625,6.5,-7.94743208891035));
#71324=CARTESIAN_POINT('',(34.3744020786062,6.5,-7.98146154857098));
#71325=CARTESIAN_POINT('',(34.865667786625,12.25,-7.94743208891035));
#71326=CARTESIAN_POINT('Origin',(34.865667786625,12.25,-7.94743208891035));
#71327=CARTESIAN_POINT('',(34.7478805248412,6.5,-7.8338351857635));
#71328=CARTESIAN_POINT('',(34.7478805248412,5.9,-7.8338351857635));
#71329=CARTESIAN_POINT('',(34.865667786625,6.5,-7.94743208891035));
#71330=CARTESIAN_POINT('Origin',(34.6542369469482,6.5,-7.87047755666207));
#71331=CARTESIAN_POINT('Origin',(39.2,6.5,-9.525));
#71332=CARTESIAN_POINT('Origin',(34.7157463933413,12.25,-7.16695508075689));
#71333=CARTESIAN_POINT('',(35.0427253561796,6.5,-7.20153840448186));
#71334=CARTESIAN_POINT('',(35.0427253561796,5.9,-7.20153840448186));
#71335=CARTESIAN_POINT('',(35.2054578250443,6.5,-7.21875));
#71336=CARTESIAN_POINT('',(34.7157463933413,6.5,-7.16695508075689));
#71337=CARTESIAN_POINT('',(35.2054578250443,12.25,-7.21875));
#71338=CARTESIAN_POINT('Origin',(35.2054578250443,12.25,-7.21875));
#71339=CARTESIAN_POINT('',(35.1091859116536,6.5,-7.08642534570167));
#71340=CARTESIAN_POINT('',(35.1091859116536,5.9,-7.08642534570168));
#71341=CARTESIAN_POINT('',(35.2054578250443,6.5,-7.21875));
#71342=CARTESIAN_POINT('Origin',(35.0106021091928,6.5,-7.10625));
#71343=CARTESIAN_POINT('Origin',(39.2,6.5,-9.525));
#71344=CARTESIAN_POINT('Origin',(35.1933424847729,12.25,-6.42409661458569));
#71345=CARTESIAN_POINT('',(35.5093485713054,6.5,-6.51493384094727));
#71346=CARTESIAN_POINT('',(35.5093485713054,5.9,-6.51493384094727));
#71347=CARTESIAN_POINT('',(35.6666200061137,6.5,-6.56014215032084));
#71348=CARTESIAN_POINT('',(35.1933424847729,6.5,-6.42409661458569));
#71349=CARTESIAN_POINT('',(35.6666200061137,12.25,-6.56014215032084));
#71350=CARTESIAN_POINT('Origin',(35.6666200061137,12.25,-6.56014215032084));
#71351=CARTESIAN_POINT('',(35.5947886144885,6.5,-6.41311036253237));
#71352=CARTESIAN_POINT('',(35.5947886144885,5.9,-6.41311036253237));
#71353=CARTESIAN_POINT('',(35.6666200061137,6.5,-6.56014215032084));
#71354=CARTESIAN_POINT('Origin',(35.4942600064119,6.5,-6.41551493814136));
#71355=CARTESIAN_POINT('Origin',(39.2,6.5,-9.525));
#71356=CARTESIAN_POINT('Origin',(35.7926788373381,12.25,-5.77545752864748));
#71357=CARTESIAN_POINT('',(36.0881103625324,6.5,-5.91978861448852));
#71358=CARTESIAN_POINT('',(36.0881103625324,5.9,-5.91978861448852));
#71359=CARTESIAN_POINT('',(36.2351421503208,6.5,-5.99162000611371));
#71360=CARTESIAN_POINT('',(35.7926788373381,6.5,-5.77545752864748));
#71361=CARTESIAN_POINT('',(36.2351421503208,12.25,-5.99162000611371));
#71362=CARTESIAN_POINT('Origin',(36.2351421503208,12.25,-5.99162000611371));
#71363=CARTESIAN_POINT('',(36.1899338409473,6.5,-5.83434857130539));
#71364=CARTESIAN_POINT('',(36.1899338409473,5.9,-5.83434857130539));
#71365=CARTESIAN_POINT('',(36.2351421503208,6.5,-5.99162000611371));
#71366=CARTESIAN_POINT('Origin',(36.0905149381414,6.5,-5.81926000641194));
#71367=CARTESIAN_POINT('Origin',(39.2,6.5,-9.525));
#71368=CARTESIAN_POINT('Origin',(36.4955449192431,12.25,-5.24074639334128));
#71369=CARTESIAN_POINT('',(36.7614253457017,6.5,-5.43418591165355));
#71370=CARTESIAN_POINT('',(36.7614253457017,5.9,-5.43418591165355));
#71371=CARTESIAN_POINT('',(36.89375,6.5,-5.53045782504427));
#71372=CARTESIAN_POINT('',(36.4955449192431,6.5,-5.24074639334128));
#71373=CARTESIAN_POINT('',(36.89375,12.25,-5.53045782504427));
#71374=CARTESIAN_POINT('Origin',(36.89375,12.25,-5.53045782504427));
#71375=CARTESIAN_POINT('',(36.8765384044819,6.5,-5.36772535617957));
#71376=CARTESIAN_POINT('',(36.8765384044819,5.9,-5.36772535617957));
#71377=CARTESIAN_POINT('',(36.89375,6.5,-5.53045782504427));
#71378=CARTESIAN_POINT('Origin',(36.78125,6.5,-5.33560210919277));
#71379=CARTESIAN_POINT('Origin',(39.2,6.5,-9.525));
#71380=CARTESIAN_POINT('Origin',(37.2805845002566,12.25,-4.83621013593647));
#71381=CARTESIAN_POINT('',(37.5088351857635,6.5,-5.07288052484118));
#71382=CARTESIAN_POINT('',(37.5088351857635,5.9,-5.07288052484118));
#71383=CARTESIAN_POINT('',(37.6224320889104,6.5,-5.19066778662499));
#71384=CARTESIAN_POINT('',(37.2805845002566,6.5,-4.83621013593647));
#71385=CARTESIAN_POINT('',(37.6224320889104,12.25,-5.19066778662499));
#71386=CARTESIAN_POINT('Origin',(37.6224320889104,12.25,-5.19066778662499));
#71387=CARTESIAN_POINT('',(37.633740172868,6.5,-5.02741882742375));
#71388=CARTESIAN_POINT('',(37.633740172868,5.9,-5.02741882742375));
#71389=CARTESIAN_POINT('',(37.6224320889104,6.5,-5.19066778662499));
#71390=CARTESIAN_POINT('Origin',(37.5454775566621,6.5,-4.97923694694816));
#71391=CARTESIAN_POINT('Origin',(39.2,6.5,-9.525));
#71392=CARTESIAN_POINT('Origin',(38.1239445499587,12.25,-4.57414038590907));
#71393=CARTESIAN_POINT('',(38.3076302129352,6.5,-4.84685053540035));
#71394=CARTESIAN_POINT('',(38.3076302129352,5.9,-4.84685053540035));
#71395=CARTESIAN_POINT('',(38.3990477805113,6.5,-4.98257423923119));
#71396=CARTESIAN_POINT('',(38.1239445499587,6.5,-4.57414038590907));
#71397=CARTESIAN_POINT('',(38.3990477805113,12.25,-4.98257423923119));
#71398=CARTESIAN_POINT('Origin',(38.3990477805113,12.25,-4.98257423923119));
#71399=CARTESIAN_POINT('',(38.4385319535358,6.5,-4.82376902671077));
#71400=CARTESIAN_POINT('',(38.4385319535358,5.9,-4.82376902671077));
#71401=CARTESIAN_POINT('',(38.3990477805113,6.5,-4.98257423923119));
#71402=CARTESIAN_POINT('Origin',(38.3599769405362,6.5,-4.76099249480344));
#71403=CARTESIAN_POINT('Origin',(39.2,6.5,-9.525));
#71404=CARTESIAN_POINT('Origin',(39.,12.25,-4.4625));
#71405=CARTESIAN_POINT('',(39.133539444526,6.5,-4.76296375018353));
#71406=CARTESIAN_POINT('',(39.133539444526,5.9,-4.76296375018353));
#71407=CARTESIAN_POINT('',(39.2,6.5,-4.9125));
#71408=CARTESIAN_POINT('',(39.,6.5,-4.4625));
#71409=CARTESIAN_POINT('',(39.2,12.25,-4.9125));
#71410=CARTESIAN_POINT('Origin',(39.2,12.25,-4.9125));
#71411=CARTESIAN_POINT('',(39.266460555474,6.5,-4.76296375018353));
#71412=CARTESIAN_POINT('',(39.266460555474,5.9,-4.76296375018353));
#71413=CARTESIAN_POINT('',(39.2,6.5,-4.9125));
#71414=CARTESIAN_POINT('Origin',(39.2,6.5,-4.6875));
#71415=CARTESIAN_POINT('Origin',(39.2,6.5,-9.525));
#71416=CARTESIAN_POINT('Origin',(39.8821323488364,12.25,-4.50468111484231));
#71417=CARTESIAN_POINT('',(39.9614680464642,6.5,-4.82376902671077));
#71418=CARTESIAN_POINT('',(39.9614680464642,5.9,-4.82376902671077));
#71419=CARTESIAN_POINT('',(40.0009522194887,6.5,-4.98257423923119));
#71420=CARTESIAN_POINT('',(39.8821323488364,6.5,-4.50468111484231));
#71421=CARTESIAN_POINT('',(40.0009522194887,12.25,-4.98257423923119));
#71422=CARTESIAN_POINT('Origin',(40.0009522194887,12.25,-4.98257423923119));
#71423=CARTESIAN_POINT('',(40.0923697870648,6.5,-4.84685053540035));
#71424=CARTESIAN_POINT('',(40.0923697870648,5.9,-4.84685053540035));
#71425=CARTESIAN_POINT('',(40.0009522194887,6.5,-4.98257423923119));
#71426=CARTESIAN_POINT('Origin',(40.0400230594638,6.5,-4.76099249480344));
#71427=CARTESIAN_POINT('Origin',(39.2,6.5,-9.525));
#71428=CARTESIAN_POINT('Origin',(40.743538451429,12.25,-4.69940207860621));
#71429=CARTESIAN_POINT('',(40.766259827132,6.5,-5.02741882742375));
#71430=CARTESIAN_POINT('',(40.766259827132,5.9,-5.02741882742375));
#71431=CARTESIAN_POINT('',(40.7775679110897,6.5,-5.190667786625));
#71432=CARTESIAN_POINT('',(40.743538451429,6.5,-4.69940207860621));
#71433=CARTESIAN_POINT('',(40.7775679110897,12.25,-5.190667786625));
#71434=CARTESIAN_POINT('Origin',(40.7775679110897,12.25,-5.190667786625));
#71435=CARTESIAN_POINT('',(40.8911648142365,6.5,-5.07288052484118));
#71436=CARTESIAN_POINT('',(40.8911648142365,5.9,-5.07288052484118));
#71437=CARTESIAN_POINT('',(40.7775679110897,6.5,-5.190667786625));
#71438=CARTESIAN_POINT('Origin',(40.8545224433379,6.5,-4.97923694694817));
#71439=CARTESIAN_POINT('Origin',(39.2,6.5,-9.525));
#71440=CARTESIAN_POINT('Origin',(41.5580449192431,12.25,-5.04074639334128));
#71441=CARTESIAN_POINT('',(41.5234615955181,6.5,-5.36772535617957));
#71442=CARTESIAN_POINT('',(41.5234615955181,5.9,-5.36772535617957));
#71443=CARTESIAN_POINT('',(41.50625,6.5,-5.53045782504427));
#71444=CARTESIAN_POINT('',(41.5580449192431,6.5,-5.04074639334128));
#71445=CARTESIAN_POINT('',(41.50625,12.25,-5.53045782504427));
#71446=CARTESIAN_POINT('Origin',(41.50625,12.25,-5.53045782504427));
#71447=CARTESIAN_POINT('',(41.6385746542983,6.5,-5.43418591165355));
#71448=CARTESIAN_POINT('',(41.6385746542983,5.9,-5.43418591165355));
#71449=CARTESIAN_POINT('',(41.50625,6.5,-5.53045782504427));
#71450=CARTESIAN_POINT('Origin',(41.61875,6.5,-5.33560210919277));
#71451=CARTESIAN_POINT('Origin',(39.2,6.5,-9.525));
#71452=CARTESIAN_POINT('Origin',(42.3009033854143,12.25,-5.51834248477286));
#71453=CARTESIAN_POINT('',(42.2100661590527,6.5,-5.83434857130539));
#71454=CARTESIAN_POINT('',(42.2100661590527,5.9,-5.83434857130539));
#71455=CARTESIAN_POINT('',(42.1648578496792,6.5,-5.99162000611371));
#71456=CARTESIAN_POINT('',(42.3009033854143,6.5,-5.51834248477286));
#71457=CARTESIAN_POINT('',(42.1648578496792,12.25,-5.99162000611371));
#71458=CARTESIAN_POINT('Origin',(42.1648578496792,12.25,-5.99162000611371));
#71459=CARTESIAN_POINT('',(42.3118896374676,6.5,-5.91978861448852));
#71460=CARTESIAN_POINT('',(42.3118896374676,5.9,-5.91978861448852));
#71461=CARTESIAN_POINT('',(42.1648578496792,6.5,-5.99162000611371));
#71462=CARTESIAN_POINT('Origin',(42.3094850618586,6.5,-5.81926000641194));
#71463=CARTESIAN_POINT('Origin',(39.2,6.5,-9.525));
#71464=CARTESIAN_POINT('Origin',(42.9495424713525,12.25,-6.1176788373381));
#71465=CARTESIAN_POINT('',(42.8052113855115,6.5,-6.41311036253237));
#71466=CARTESIAN_POINT('',(42.8052113855115,5.9,-6.41311036253237));
#71467=CARTESIAN_POINT('',(42.7333799938863,6.5,-6.56014215032084));
#71468=CARTESIAN_POINT('',(42.9495424713525,6.5,-6.1176788373381));
#71469=CARTESIAN_POINT('',(42.7333799938863,12.25,-6.56014215032084));
#71470=CARTESIAN_POINT('Origin',(42.7333799938863,12.25,-6.56014215032084));
#71471=CARTESIAN_POINT('',(42.8906514286946,6.5,-6.51493384094727));
#71472=CARTESIAN_POINT('',(42.8906514286946,5.9,-6.51493384094727));
#71473=CARTESIAN_POINT('',(42.7333799938863,6.5,-6.56014215032084));
#71474=CARTESIAN_POINT('Origin',(42.9057399935881,6.5,-6.41551493814136));
#71475=CARTESIAN_POINT('Origin',(39.2,6.5,-9.525));
#71476=CARTESIAN_POINT('Origin',(43.4842536066587,12.25,-6.82054491924312));
#71477=CARTESIAN_POINT('',(43.2908140883465,6.5,-7.08642534570167));
#71478=CARTESIAN_POINT('',(43.2908140883465,5.9,-7.08642534570167));
#71479=CARTESIAN_POINT('',(43.1945421749557,6.5,-7.21875));
#71480=CARTESIAN_POINT('',(43.4842536066587,6.5,-6.82054491924312));
#71481=CARTESIAN_POINT('',(43.1945421749557,12.25,-7.21875));
#71482=CARTESIAN_POINT('Origin',(43.1945421749557,12.25,-7.21875));
#71483=CARTESIAN_POINT('',(43.3572746438204,6.5,-7.20153840448187));
#71484=CARTESIAN_POINT('',(43.3572746438204,5.9,-7.20153840448187));
#71485=CARTESIAN_POINT('',(43.1945421749557,6.5,-7.21875));
#71486=CARTESIAN_POINT('Origin',(43.3893978908072,6.5,-7.10625));
#71487=CARTESIAN_POINT('Origin',(39.2,6.5,-9.525));
#71488=CARTESIAN_POINT('Origin',(43.8887898640635,12.25,-7.60558450025662));
#71489=CARTESIAN_POINT('',(43.6521194751588,6.5,-7.83383518576351));
#71490=CARTESIAN_POINT('',(43.6521194751588,5.9,-7.83383518576351));
#71491=CARTESIAN_POINT('',(43.534332213375,6.5,-7.94743208891035));
#71492=CARTESIAN_POINT('',(43.8887898640635,6.5,-7.60558450025662));
#71493=CARTESIAN_POINT('',(43.534332213375,12.25,-7.94743208891035));
#71494=CARTESIAN_POINT('Origin',(43.534332213375,12.25,-7.94743208891035));
#71495=CARTESIAN_POINT('',(43.6975811725762,6.5,-7.95874017286797));
#71496=CARTESIAN_POINT('',(43.6975811725762,5.9,-7.95874017286797));
#71497=CARTESIAN_POINT('',(43.534332213375,6.5,-7.94743208891035));
#71498=CARTESIAN_POINT('Origin',(43.7457630530518,6.5,-7.87047755666208));
#71499=CARTESIAN_POINT('Origin',(39.2,6.5,-9.525));
#71500=CARTESIAN_POINT('Origin',(44.1508596140909,12.25,-8.44894454995872));
#71501=CARTESIAN_POINT('',(43.8781494645997,6.5,-8.63263021293523));
#71502=CARTESIAN_POINT('',(43.8781494645997,5.9,-8.63263021293523));
#71503=CARTESIAN_POINT('',(43.7424257607688,6.5,-8.72404778051128));
#71504=CARTESIAN_POINT('',(44.1508596140909,6.5,-8.44894454995872));
#71505=CARTESIAN_POINT('',(43.7424257607688,12.25,-8.72404778051128));
#71506=CARTESIAN_POINT('Origin',(43.7424257607688,12.25,-8.72404778051128));
#71507=CARTESIAN_POINT('',(43.9012309732892,6.5,-8.76353195353578));
#71508=CARTESIAN_POINT('',(43.9012309732892,5.9,-8.76353195353579));
#71509=CARTESIAN_POINT('',(43.7424257607688,6.5,-8.72404778051128));
#71510=CARTESIAN_POINT('Origin',(43.9640075051965,6.5,-8.68497694053622));
#71511=CARTESIAN_POINT('Origin',(39.2,6.5,-9.525));
#71512=CARTESIAN_POINT('Origin',(44.2625,12.25,-9.325));
#71513=CARTESIAN_POINT('',(43.9620362498165,6.5,-9.45853944452601));
#71514=CARTESIAN_POINT('',(43.9620362498165,5.9,-9.45853944452601));
#71515=CARTESIAN_POINT('',(43.8125,6.5,-9.525));
#71516=CARTESIAN_POINT('',(44.2625,6.5,-9.325));
#71517=CARTESIAN_POINT('',(43.8125,12.25,-9.525));
#71518=CARTESIAN_POINT('Origin',(43.8125,12.25,-9.525));
#71519=CARTESIAN_POINT('',(43.9620362498165,6.5,-9.59146055547398));
#71520=CARTESIAN_POINT('',(43.9620362498165,5.9,-9.59146055547398));
#71521=CARTESIAN_POINT('',(43.8125,6.5,-9.525));
#71522=CARTESIAN_POINT('Origin',(44.0375,6.5,-9.525));
#71523=CARTESIAN_POINT('Origin',(39.2,6.5,-9.525));
#71524=CARTESIAN_POINT('Origin',(39.2,5.9,-9.525));
#71525=CARTESIAN_POINT('',(34.4375,5.9,-9.525));
#71526=CARTESIAN_POINT('Origin',(39.2,12.25,-9.525));
#71527=CARTESIAN_POINT('',(36.4503693429844,12.25,-9.525));
#71528=CARTESIAN_POINT('',(37.8251846714922,12.25,-11.90625));
#71529=CARTESIAN_POINT('',(36.7940731751114,12.25,-10.1203125));
#71530=CARTESIAN_POINT('',(40.5748153285078,12.25,-11.90625));
#71531=CARTESIAN_POINT('',(38.5125923357461,12.25,-11.90625));
#71532=CARTESIAN_POINT('',(41.9496306570156,12.25,-9.525));
#71533=CARTESIAN_POINT('',(40.9185191606347,12.25,-11.3109375));
#71534=CARTESIAN_POINT('',(40.5748153285078,12.25,-7.14375));
#71535=CARTESIAN_POINT('',(41.6059268248886,12.25,-8.9296875));
#71536=CARTESIAN_POINT('',(37.8251846714922,12.25,-7.14375));
#71537=CARTESIAN_POINT('',(39.8874076642539,12.25,-7.14375));
#71538=CARTESIAN_POINT('',(37.4814808393653,12.25,-7.7390625));
#71539=CARTESIAN_POINT('Origin',(41.9496306570156,9.05,-9.525));
#71540=CARTESIAN_POINT('',(36.4503693429844,9.05,-9.525));
#71541=CARTESIAN_POINT('',(37.8251846714922,9.05,-11.90625));
#71542=CARTESIAN_POINT('',(36.4503693429844,9.05,-9.525));
#71543=CARTESIAN_POINT('Origin',(39.2,9.05,-9.525));
#71544=CARTESIAN_POINT('Origin',(41.9496306570156,9.05,-9.525));
#71545=CARTESIAN_POINT('',(40.5748153285078,9.05,-11.90625));
#71546=CARTESIAN_POINT('',(37.8251846714922,9.05,-11.90625));
#71547=CARTESIAN_POINT('Origin',(39.2,9.05,-9.525));
#71548=CARTESIAN_POINT('Origin',(41.9496306570156,9.05,-9.525));
#71549=CARTESIAN_POINT('',(41.9496306570156,9.05,-9.525));
#71550=CARTESIAN_POINT('',(40.5748153285078,9.05,-11.90625));
#71551=CARTESIAN_POINT('Origin',(39.2,9.05,-9.525));
#71552=CARTESIAN_POINT('Origin',(41.9496306570156,9.05,-9.525));
#71553=CARTESIAN_POINT('',(40.5748153285078,9.05,-7.14375));
#71554=CARTESIAN_POINT('',(41.9496306570156,9.05,-9.525));
#71555=CARTESIAN_POINT('Origin',(39.2,9.05,-9.525));
#71556=CARTESIAN_POINT('Origin',(41.9496306570156,9.05,-9.525));
#71557=CARTESIAN_POINT('',(37.8251846714922,9.05,-7.14375));
#71558=CARTESIAN_POINT('',(40.5748153285078,9.05,-7.14375));
#71559=CARTESIAN_POINT('Origin',(39.2,9.05,-9.525));
#71560=CARTESIAN_POINT('Origin',(41.9496306570156,9.05,-9.525));
#71561=CARTESIAN_POINT('',(37.8251846714922,9.05,-7.14375));
#71562=CARTESIAN_POINT('Origin',(39.2,9.05,-9.525));
#71563=CARTESIAN_POINT('Origin',(39.2,9.05,-9.525));
#71564=CARTESIAN_POINT('',(39.2,7.39785522132845,-9.525));
#71565=CARTESIAN_POINT('',(36.4503693429844,9.05,-9.525));
#71566=CARTESIAN_POINT('Origin',(36.4503693429844,12.25,-9.525));
#71567=CARTESIAN_POINT('',(36.4503693429844,12.25,-9.525));
#71568=CARTESIAN_POINT('',(37.8251846714922,12.25,-11.90625));
#71569=CARTESIAN_POINT('Origin',(37.8251846714922,12.25,-7.14375));
#71570=CARTESIAN_POINT('',(37.8251846714922,12.25,-7.14375));
#71571=CARTESIAN_POINT('Origin',(40.5748153285078,12.25,-7.14375));
#71572=CARTESIAN_POINT('',(40.5748153285078,12.25,-7.14375));
#71573=CARTESIAN_POINT('Origin',(41.9496306570156,12.25,-9.525));
#71574=CARTESIAN_POINT('',(41.9496306570156,12.25,-9.525));
#71575=CARTESIAN_POINT('Origin',(40.5748153285078,12.25,-11.90625));
#71576=CARTESIAN_POINT('',(40.5748153285078,12.25,-11.90625));
#71577=CARTESIAN_POINT('Origin',(37.8251846714922,12.25,-11.90625));
#71578=CARTESIAN_POINT('',(0.,0.,0.));
#71579=CARTESIAN_POINT('',(0.,0.,0.));
#71580=CARTESIAN_POINT('',(0.,0.,0.));
#71581=CARTESIAN_POINT('',(0.,0.,0.));
#71582=CARTESIAN_POINT('',(0.,0.,0.));
#71583=CARTESIAN_POINT('',(0.,0.,0.));
#71584=CARTESIAN_POINT('',(0.,0.,0.));
#71585=CARTESIAN_POINT('',(0.,0.,0.));
#71586=CARTESIAN_POINT('',(0.,0.,0.));
#71587=CARTESIAN_POINT('',(0.,33.4503201513364,-4.55621657507847));
#71588=CARTESIAN_POINT('',(180.,0.,1.10218211923262E-14));
#71589=CARTESIAN_POINT('',(76.2,0.,0.));
#71590=CARTESIAN_POINT('',(180.,0.,1.10218211923262E-14));
#71591=CARTESIAN_POINT('',(103.8,0.,1.69001258282335E-15));
#71592=CARTESIAN_POINT('',(76.2,0.,0.));
#71593=CARTESIAN_POINT('',(180.,0.,1.10218211923262E-14));
#71594=CARTESIAN_POINT('',(103.8,0.,1.69001258282335E-15));
#71595=CARTESIAN_POINT('',(76.2,0.,0.));
#71596=CARTESIAN_POINT('',(180.,0.,1.10218211923262E-14));
#71597=CARTESIAN_POINT('',(103.8,0.,1.69001258282335E-15));
#71598=CARTESIAN_POINT('',(2.6,0.,0.));
#71599=CARTESIAN_POINT('',(5.2,0.,0.));
#71600=CARTESIAN_POINT('',(7.8,0.,0.));
#71601=CARTESIAN_POINT('',(10.4,0.,0.));
#71602=CARTESIAN_POINT('',(13.,0.,0.));
#71603=CARTESIAN_POINT('',(15.6,0.,0.));
#71604=CARTESIAN_POINT('',(18.2,0.,0.));
#71605=CARTESIAN_POINT('',(0.,-21.8830678841871,38.2974145991091));
#71606=CARTESIAN_POINT('',(2.6,-21.8830678841871,38.2974145991091));
#71607=CARTESIAN_POINT('',(5.2,-21.8830678841871,38.2974145991091));
#71608=CARTESIAN_POINT('',(7.8,-21.8830678841871,38.2974145991091));
#71609=CARTESIAN_POINT('',(10.4,-21.8830678841871,38.2974145991091));
#71610=CARTESIAN_POINT('',(13.,-21.8830678841871,38.2974145991091));
#71611=CARTESIAN_POINT('',(15.6,-21.8830678841871,38.2974145991091));
#71612=CARTESIAN_POINT('',(18.2,-21.8830678841871,38.2974145991091));
#71613=CARTESIAN_POINT('',(0.,0.3419321158129,76.3974145991091));
#71614=CARTESIAN_POINT('',(2.6,0.3419321158129,76.3974145991091));
#71615=CARTESIAN_POINT('',(5.2,0.3419321158129,76.3974145991091));
#71616=CARTESIAN_POINT('',(7.8,0.3419321158129,76.3974145991091));
#71617=CARTESIAN_POINT('',(10.4,0.3419321158129,76.3974145991091));
#71618=CARTESIAN_POINT('',(13.,0.3419321158129,76.3974145991091));
#71619=CARTESIAN_POINT('',(15.6,0.3419321158129,76.3974145991091));
#71620=CARTESIAN_POINT('',(18.2,0.3419321158129,76.3974145991091));
#71621=CARTESIAN_POINT('',(0.,44.45,76.2));
#71622=CARTESIAN_POINT('',(2.6,44.45,76.2));
#71623=CARTESIAN_POINT('',(5.2,44.45,76.2));
#71624=CARTESIAN_POINT('',(7.8,44.45,76.2));
#71625=CARTESIAN_POINT('',(10.4,44.45,76.2));
#71626=CARTESIAN_POINT('',(13.,44.45,76.2));
#71627=CARTESIAN_POINT('',(15.6,44.45,76.2));
#71628=CARTESIAN_POINT('',(18.2,44.45,76.2));
#71629=CARTESIAN_POINT('',(0.,66.3330678841871,37.9025854008908));
#71630=CARTESIAN_POINT('',(2.6,66.3330678841871,37.9025854008908));
#71631=CARTESIAN_POINT('',(5.2,66.3330678841871,37.9025854008908));
#71632=CARTESIAN_POINT('',(7.8,66.3330678841871,37.9025854008908));
#71633=CARTESIAN_POINT('',(10.4,66.3330678841871,37.9025854008908));
#71634=CARTESIAN_POINT('',(13.,66.3330678841871,37.9025854008908));
#71635=CARTESIAN_POINT('',(15.6,66.3330678841871,37.9025854008908));
#71636=CARTESIAN_POINT('',(18.2,66.3330678841871,37.9025854008908));
#71637=CARTESIAN_POINT('',(76.2,0.,0.));
#71638=CARTESIAN_POINT('',(78.8,0.,0.));
#71639=CARTESIAN_POINT('',(81.4,0.,0.));
#71640=CARTESIAN_POINT('',(84.,0.,0.));
#71641=CARTESIAN_POINT('',(86.6,0.,0.));
#71642=CARTESIAN_POINT('',(89.2,0.,0.));
#71643=CARTESIAN_POINT('',(91.8,0.,0.));
#71644=CARTESIAN_POINT('',(94.4,0.,0.));
#71645=CARTESIAN_POINT('',(76.2,-21.8830678841871,38.2974145991091));
#71646=CARTESIAN_POINT('',(78.8,-21.8830678841871,38.2974145991091));
#71647=CARTESIAN_POINT('',(81.4,-21.8830678841871,38.2974145991091));
#71648=CARTESIAN_POINT('',(84.,-21.8830678841871,38.2974145991091));
#71649=CARTESIAN_POINT('',(86.6,-21.8830678841871,38.2974145991091));
#71650=CARTESIAN_POINT('',(89.2,-21.8830678841871,38.2974145991091));
#71651=CARTESIAN_POINT('',(91.8,-21.8830678841871,38.2974145991091));
#71652=CARTESIAN_POINT('',(94.4,-21.8830678841871,38.2974145991091));
#71653=CARTESIAN_POINT('',(76.2,0.3419321158129,76.3974145991091));
#71654=CARTESIAN_POINT('',(78.8,0.3419321158129,76.3974145991091));
#71655=CARTESIAN_POINT('',(81.4,0.3419321158129,76.3974145991091));
#71656=CARTESIAN_POINT('',(84.,0.3419321158129,76.3974145991091));
#71657=CARTESIAN_POINT('',(86.6,0.3419321158129,76.3974145991091));
#71658=CARTESIAN_POINT('',(89.2,0.3419321158129,76.3974145991091));
#71659=CARTESIAN_POINT('',(91.8,0.3419321158129,76.3974145991091));
#71660=CARTESIAN_POINT('',(94.4,0.3419321158129,76.3974145991091));
#71661=CARTESIAN_POINT('',(76.2,44.45,76.2));
#71662=CARTESIAN_POINT('',(78.8,44.45,76.2));
#71663=CARTESIAN_POINT('',(81.4,44.45,76.2));
#71664=CARTESIAN_POINT('',(84.,44.45,76.2));
#71665=CARTESIAN_POINT('',(86.6,44.45,76.2));
#71666=CARTESIAN_POINT('',(89.2,44.45,76.2));
#71667=CARTESIAN_POINT('',(91.8,44.45,76.2));
#71668=CARTESIAN_POINT('',(94.4,44.45,76.2));
#71669=CARTESIAN_POINT('',(76.2,66.3330678841871,37.9025854008908));
#71670=CARTESIAN_POINT('',(78.8,66.3330678841871,37.9025854008908));
#71671=CARTESIAN_POINT('',(81.4,66.3330678841871,37.9025854008908));
#71672=CARTESIAN_POINT('',(84.,66.3330678841871,37.9025854008908));
#71673=CARTESIAN_POINT('',(86.6,66.3330678841871,37.9025854008908));
#71674=CARTESIAN_POINT('',(89.2,66.3330678841871,37.9025854008908));
#71675=CARTESIAN_POINT('',(91.8,66.3330678841871,37.9025854008908));
#71676=CARTESIAN_POINT('',(94.4,66.3330678841871,37.9025854008908));
#71677=CARTESIAN_POINT('',(180.,0.,1.10218211923262E-14));
#71678=CARTESIAN_POINT('',(177.4,0.,1.07034130245479E-14));
#71679=CARTESIAN_POINT('',(174.8,0.,1.03850048567696E-14));
#71680=CARTESIAN_POINT('',(172.2,0.,1.00665966889912E-14));
#71681=CARTESIAN_POINT('',(169.6,0.,9.74818852121293E-15));
#71682=CARTESIAN_POINT('',(167.,0.,9.42978035343462E-15));
#71683=CARTESIAN_POINT('',(164.4,0.,9.11137218565631E-15));
#71684=CARTESIAN_POINT('',(161.8,0.,8.79296401787799E-15));
#71685=CARTESIAN_POINT('',(180.,-21.8830678841871,-38.2974145991091));
#71686=CARTESIAN_POINT('',(177.4,-21.8830678841871,-38.2974145991091));
#71687=CARTESIAN_POINT('',(174.8,-21.8830678841871,-38.2974145991091));
#71688=CARTESIAN_POINT('',(172.2,-21.8830678841871,-38.2974145991091));
#71689=CARTESIAN_POINT('',(169.6,-21.8830678841871,-38.2974145991091));
#71690=CARTESIAN_POINT('',(167.,-21.8830678841871,-38.2974145991091));
#71691=CARTESIAN_POINT('',(164.4,-21.8830678841871,-38.2974145991091));
#71692=CARTESIAN_POINT('',(161.8,-21.8830678841871,-38.2974145991091));
#71693=CARTESIAN_POINT('',(180.,0.3419321158129,-76.3974145991091));
#71694=CARTESIAN_POINT('',(177.4,0.3419321158129,-76.3974145991091));
#71695=CARTESIAN_POINT('',(174.8,0.3419321158129,-76.3974145991091));
#71696=CARTESIAN_POINT('',(172.2,0.3419321158129,-76.3974145991091));
#71697=CARTESIAN_POINT('',(169.6,0.3419321158129,-76.3974145991091));
#71698=CARTESIAN_POINT('',(167.,0.3419321158129,-76.3974145991091));
#71699=CARTESIAN_POINT('',(164.4,0.3419321158129,-76.3974145991091));
#71700=CARTESIAN_POINT('',(161.8,0.3419321158129,-76.3974145991091));
#71701=CARTESIAN_POINT('',(180.,44.45,-76.2));
#71702=CARTESIAN_POINT('',(177.4,44.45,-76.2));
#71703=CARTESIAN_POINT('',(174.8,44.45,-76.2));
#71704=CARTESIAN_POINT('',(172.2,44.45,-76.2));
#71705=CARTESIAN_POINT('',(169.6,44.45,-76.2));
#71706=CARTESIAN_POINT('',(167.,44.45,-76.2));
#71707=CARTESIAN_POINT('',(164.4,44.45,-76.2));
#71708=CARTESIAN_POINT('',(161.8,44.45,-76.2));
#71709=CARTESIAN_POINT('',(180.,66.3330678841871,-37.9025854008908));
#71710=CARTESIAN_POINT('',(177.4,66.3330678841871,-37.9025854008908));
#71711=CARTESIAN_POINT('',(174.8,66.3330678841871,-37.9025854008908));
#71712=CARTESIAN_POINT('',(172.2,66.3330678841871,-37.9025854008908));
#71713=CARTESIAN_POINT('',(169.6,66.3330678841871,-37.9025854008908));
#71714=CARTESIAN_POINT('',(167.,66.3330678841871,-37.9025854008908));
#71715=CARTESIAN_POINT('',(164.4,66.3330678841871,-37.9025854008908));
#71716=CARTESIAN_POINT('',(161.8,66.3330678841871,-37.9025854008908));
#71717=CARTESIAN_POINT('',(103.8,0.,1.69001258282335E-15));
#71718=CARTESIAN_POINT('',(101.2,0.,1.37160441504503E-15));
#71719=CARTESIAN_POINT('',(98.6,0.,1.05319624726672E-15));
#71720=CARTESIAN_POINT('',(96.,0.,7.34788079488409E-16));
#71721=CARTESIAN_POINT('',(93.4,0.,4.16379911710098E-16));
#71722=CARTESIAN_POINT('',(90.8,0.,9.79717439317861E-17));
#71723=CARTESIAN_POINT('',(88.2,0.,-2.20436423846526E-16));
#71724=CARTESIAN_POINT('',(85.6,0.,-5.38844591624837E-16));
#71725=CARTESIAN_POINT('',(103.8,-21.8830678841871,-38.2974145991091));
#71726=CARTESIAN_POINT('',(101.2,-21.8830678841871,-38.2974145991091));
#71727=CARTESIAN_POINT('',(98.6,-21.8830678841871,-38.2974145991091));
#71728=CARTESIAN_POINT('',(96.,-21.8830678841871,-38.2974145991091));
#71729=CARTESIAN_POINT('',(93.4,-21.8830678841871,-38.2974145991091));
#71730=CARTESIAN_POINT('',(90.8,-21.8830678841871,-38.2974145991091));
#71731=CARTESIAN_POINT('',(88.2,-21.8830678841871,-38.2974145991091));
#71732=CARTESIAN_POINT('',(85.6,-21.8830678841871,-38.2974145991091));
#71733=CARTESIAN_POINT('',(103.8,0.3419321158129,-76.3974145991091));
#71734=CARTESIAN_POINT('',(101.2,0.3419321158129,-76.3974145991091));
#71735=CARTESIAN_POINT('',(98.6,0.3419321158129,-76.3974145991091));
#71736=CARTESIAN_POINT('',(96.,0.3419321158129,-76.3974145991091));
#71737=CARTESIAN_POINT('',(93.4,0.3419321158129,-76.3974145991091));
#71738=CARTESIAN_POINT('',(90.8,0.3419321158129,-76.3974145991091));
#71739=CARTESIAN_POINT('',(88.2,0.3419321158129,-76.3974145991091));
#71740=CARTESIAN_POINT('',(85.6,0.3419321158129,-76.3974145991091));
#71741=CARTESIAN_POINT('',(103.8,44.45,-76.2));
#71742=CARTESIAN_POINT('',(101.2,44.45,-76.2));
#71743=CARTESIAN_POINT('',(98.6,44.45,-76.2));
#71744=CARTESIAN_POINT('',(96.,44.45,-76.2));
#71745=CARTESIAN_POINT('',(93.4,44.45,-76.2));
#71746=CARTESIAN_POINT('',(90.8,44.45,-76.2));
#71747=CARTESIAN_POINT('',(88.2,44.45,-76.2));
#71748=CARTESIAN_POINT('',(85.6,44.45,-76.2));
#71749=CARTESIAN_POINT('',(103.8,66.3330678841871,-37.9025854008908));
#71750=CARTESIAN_POINT('',(101.2,66.3330678841871,-37.9025854008908));
#71751=CARTESIAN_POINT('',(98.6,66.3330678841871,-37.9025854008908));
#71752=CARTESIAN_POINT('',(96.,66.3330678841871,-37.9025854008908));
#71753=CARTESIAN_POINT('',(93.4,66.3330678841871,-37.9025854008908));
#71754=CARTESIAN_POINT('',(90.8,66.3330678841871,-37.9025854008908));
#71755=CARTESIAN_POINT('',(88.2,66.3330678841871,-37.9025854008908));
#71756=CARTESIAN_POINT('',(85.6,66.3330678841871,-37.9025854008908));
#71757=CARTESIAN_POINT('',(19.,0.,0.));
#71758=CARTESIAN_POINT('',(76.2,0.,0.));
#71759=CARTESIAN_POINT('',(95.2,0.,0.));
#71760=CARTESIAN_POINT('',(180.,0.,1.10218211923262E-14));
#71761=CARTESIAN_POINT('',(161.,0.,8.69499227394621E-15));
#71762=CARTESIAN_POINT('',(103.8,0.,1.69001258282335E-15));
#71763=CARTESIAN_POINT('',(84.8,0.,-6.36816335556625E-16));
#71764=CARTESIAN_POINT('',(180.,33.4503201513364,4.55621657507848));
#71765=CARTESIAN_POINT('',(70.,33.4503201513364,-4.55621657507847));
#71766=CARTESIAN_POINT('',(110.,33.4503201513364,4.55621657507847));
#71767=CARTESIAN_POINT('',(140.,33.4503201513364,-4.55621657507847));
#71768=CARTESIAN_POINT('',(40.,33.4503201513364,4.55621657507846));
#71769=CARTESIAN_POINT('',(0.,0.,19.05));
#71770=CARTESIAN_POINT('',(101.6,0.,0.));
#71771=CARTESIAN_POINT('',(101.6,0.,19.05));
#71772=UNCERTAINTY_MEASURE_WITH_UNIT(LENGTH_MEASURE(0.01),#71796,
'DISTANCE_ACCURACY_VALUE',
'Maximum model space distance between geometric entities at asserted c
onnectivities');
#71773=UNCERTAINTY_MEASURE_WITH_UNIT(LENGTH_MEASURE(0.01),#71796,
'DISTANCE_ACCURACY_VALUE',
'Maximum model space distance between geometric entities at asserted c
onnectivities');
#71774=UNCERTAINTY_MEASURE_WITH_UNIT(LENGTH_MEASURE(0.01),#71796,
'DISTANCE_ACCURACY_VALUE',
'Maximum model space distance between geometric entities at asserted c
onnectivities');
#71775=UNCERTAINTY_MEASURE_WITH_UNIT(LENGTH_MEASURE(0.01),#71796,
'DISTANCE_ACCURACY_VALUE',
'Maximum model space distance between geometric entities at asserted c
onnectivities');
#71776=UNCERTAINTY_MEASURE_WITH_UNIT(LENGTH_MEASURE(0.01),#71796,
'DISTANCE_ACCURACY_VALUE',
'Maximum model space distance between geometric entities at asserted c
onnectivities');
#71777=UNCERTAINTY_MEASURE_WITH_UNIT(LENGTH_MEASURE(0.01),#71796,
'DISTANCE_ACCURACY_VALUE',
'Maximum model space distance between geometric entities at asserted c
onnectivities');
#71778=UNCERTAINTY_MEASURE_WITH_UNIT(LENGTH_MEASURE(0.01),#71796,
'DISTANCE_ACCURACY_VALUE',
'Maximum model space distance between geometric entities at asserted c
onnectivities');
#71779=UNCERTAINTY_MEASURE_WITH_UNIT(LENGTH_MEASURE(0.01),#71796,
'DISTANCE_ACCURACY_VALUE',
'Maximum model space distance between geometric entities at asserted c
onnectivities');
#71780=UNCERTAINTY_MEASURE_WITH_UNIT(LENGTH_MEASURE(0.01),#71796,
'DISTANCE_ACCURACY_VALUE',
'Maximum model space distance between geometric entities at asserted c
onnectivities');
#71781=UNCERTAINTY_MEASURE_WITH_UNIT(LENGTH_MEASURE(0.01),#71796,
'DISTANCE_ACCURACY_VALUE',
'Maximum model space distance between geometric entities at asserted c
onnectivities');
#71782=UNCERTAINTY_MEASURE_WITH_UNIT(LENGTH_MEASURE(0.01),#71796,
'DISTANCE_ACCURACY_VALUE',
'Maximum model space distance between geometric entities at asserted c
onnectivities');
#71783=UNCERTAINTY_MEASURE_WITH_UNIT(LENGTH_MEASURE(0.01),#71796,
'DISTANCE_ACCURACY_VALUE',
'Maximum model space distance between geometric entities at asserted c
onnectivities');
#71784=(
GEOMETRIC_REPRESENTATION_CONTEXT(3)
GLOBAL_UNCERTAINTY_ASSIGNED_CONTEXT((#71772))
GLOBAL_UNIT_ASSIGNED_CONTEXT((#71796,#71798,#71799))
REPRESENTATION_CONTEXT('','3D')
);
#71785=(
GEOMETRIC_REPRESENTATION_CONTEXT(3)
GLOBAL_UNCERTAINTY_ASSIGNED_CONTEXT((#71773))
GLOBAL_UNIT_ASSIGNED_CONTEXT((#71796,#71798,#71799))
REPRESENTATION_CONTEXT('','3D')
);
#71786=(
GEOMETRIC_REPRESENTATION_CONTEXT(3)
GLOBAL_UNCERTAINTY_ASSIGNED_CONTEXT((#71774))
GLOBAL_UNIT_ASSIGNED_CONTEXT((#71796,#71798,#71799))
REPRESENTATION_CONTEXT('','3D')
);
#71787=(
GEOMETRIC_REPRESENTATION_CONTEXT(3)
GLOBAL_UNCERTAINTY_ASSIGNED_CONTEXT((#71775))
GLOBAL_UNIT_ASSIGNED_CONTEXT((#71796,#71798,#71799))
REPRESENTATION_CONTEXT('','3D')
);
#71788=(
GEOMETRIC_REPRESENTATION_CONTEXT(3)
GLOBAL_UNCERTAINTY_ASSIGNED_CONTEXT((#71776))
GLOBAL_UNIT_ASSIGNED_CONTEXT((#71796,#71798,#71799))
REPRESENTATION_CONTEXT('','3D')
);
#71789=(
GEOMETRIC_REPRESENTATION_CONTEXT(3)
GLOBAL_UNCERTAINTY_ASSIGNED_CONTEXT((#71777))
GLOBAL_UNIT_ASSIGNED_CONTEXT((#71796,#71798,#71799))
REPRESENTATION_CONTEXT('','3D')
);
#71790=(
GEOMETRIC_REPRESENTATION_CONTEXT(3)
GLOBAL_UNCERTAINTY_ASSIGNED_CONTEXT((#71778))
GLOBAL_UNIT_ASSIGNED_CONTEXT((#71796,#71798,#71799))
REPRESENTATION_CONTEXT('','3D')
);
#71791=(
GEOMETRIC_REPRESENTATION_CONTEXT(3)
GLOBAL_UNCERTAINTY_ASSIGNED_CONTEXT((#71779))
GLOBAL_UNIT_ASSIGNED_CONTEXT((#71796,#71798,#71799))
REPRESENTATION_CONTEXT('','3D')
);
#71792=(
GEOMETRIC_REPRESENTATION_CONTEXT(3)
GLOBAL_UNCERTAINTY_ASSIGNED_CONTEXT((#71780))
GLOBAL_UNIT_ASSIGNED_CONTEXT((#71796,#71798,#71799))
REPRESENTATION_CONTEXT('','3D')
);
#71793=(
GEOMETRIC_REPRESENTATION_CONTEXT(3)
GLOBAL_UNCERTAINTY_ASSIGNED_CONTEXT((#71781))
GLOBAL_UNIT_ASSIGNED_CONTEXT((#71796,#71798,#71799))
REPRESENTATION_CONTEXT('','3D')
);
#71794=(
GEOMETRIC_REPRESENTATION_CONTEXT(3)
GLOBAL_UNCERTAINTY_ASSIGNED_CONTEXT((#71782))
GLOBAL_UNIT_ASSIGNED_CONTEXT((#71796,#71798,#71799))
REPRESENTATION_CONTEXT('','3D')
);
#71795=(
GEOMETRIC_REPRESENTATION_CONTEXT(3)
GLOBAL_UNCERTAINTY_ASSIGNED_CONTEXT((#71783))
GLOBAL_UNIT_ASSIGNED_CONTEXT((#71796,#71798,#71799))
REPRESENTATION_CONTEXT('','3D')
);
#71796=(
LENGTH_UNIT()
NAMED_UNIT(*)
SI_UNIT(.MILLI.,.METRE.)
);
#71797=(
LENGTH_UNIT()
NAMED_UNIT(*)
SI_UNIT($,.METRE.)
);
#71798=(
NAMED_UNIT(*)
PLANE_ANGLE_UNIT()
SI_UNIT($,.RADIAN.)
);
#71799=(
NAMED_UNIT(*)
SI_UNIT($,.STERADIAN.)
SOLID_ANGLE_UNIT()
);
#71800=SHAPE_DEFINITION_REPRESENTATION(#71811,#72016);
#71801=SHAPE_DEFINITION_REPRESENTATION(#71812,#72017);
#71802=SHAPE_DEFINITION_REPRESENTATION(#71813,#72018);
#71803=SHAPE_DEFINITION_REPRESENTATION(#71814,#72019);
#71804=SHAPE_DEFINITION_REPRESENTATION(#71815,#72020);
#71805=SHAPE_DEFINITION_REPRESENTATION(#71816,#72021);
#71806=SHAPE_DEFINITION_REPRESENTATION(#71817,#72022);
#71807=SHAPE_DEFINITION_REPRESENTATION(#71818,#72023);
#71808=SHAPE_DEFINITION_REPRESENTATION(#71819,#72024);
#71809=SHAPE_DEFINITION_REPRESENTATION(#71820,#72025);
#71810=SHAPE_DEFINITION_REPRESENTATION(#71821,#72026);
#71811=PRODUCT_DEFINITION_SHAPE('',$,#72028);
#71812=PRODUCT_DEFINITION_SHAPE('',$,#72029);
#71813=PRODUCT_DEFINITION_SHAPE('',$,#72030);
#71814=PRODUCT_DEFINITION_SHAPE('',$,#72031);
#71815=PRODUCT_DEFINITION_SHAPE('',$,#72032);
#71816=PRODUCT_DEFINITION_SHAPE('',$,#72033);
#71817=PRODUCT_DEFINITION_SHAPE('',$,#72034);
#71818=PRODUCT_DEFINITION_SHAPE('',$,#72035);
#71819=PRODUCT_DEFINITION_SHAPE('',$,#72036);
#71820=PRODUCT_DEFINITION_SHAPE('',$,#72037);
#71821=PRODUCT_DEFINITION_SHAPE('',$,#72038);
#71822=PRODUCT_DEFINITION_SHAPE($,$,#593);
#71823=PRODUCT_DEFINITION_SHAPE($,$,#594);
#71824=PRODUCT_DEFINITION_SHAPE($,$,#595);
#71825=PRODUCT_DEFINITION_SHAPE($,$,#596);
#71826=PRODUCT_DEFINITION_SHAPE($,$,#597);
#71827=PRODUCT_DEFINITION_SHAPE($,$,#598);
#71828=PRODUCT_DEFINITION_SHAPE($,$,#599);
#71829=PRODUCT_DEFINITION_SHAPE($,$,#600);
#71830=PRODUCT_DEFINITION_SHAPE($,$,#601);
#71831=PRODUCT_DEFINITION_SHAPE($,$,#602);
#71832=PRODUCT_DEFINITION_SHAPE($,$,#603);
#71833=PRODUCT_DEFINITION_SHAPE($,$,#604);
#71834=PRODUCT_DEFINITION_SHAPE($,$,#605);
#71835=PRODUCT_DEFINITION_SHAPE($,$,#606);
#71836=PRODUCT_DEFINITION_SHAPE($,$,#607);
#71837=PRODUCT_DEFINITION_SHAPE($,$,#608);
#71838=PRODUCT_DEFINITION_SHAPE($,$,#609);
#71839=PRODUCT_DEFINITION_SHAPE($,$,#610);
#71840=PRODUCT_DEFINITION_SHAPE($,$,#611);
#71841=PRODUCT_DEFINITION_SHAPE($,$,#612);
#71842=PRODUCT_DEFINITION_SHAPE($,$,#613);
#71843=PRODUCT_DEFINITION_SHAPE($,$,#614);
#71844=PRODUCT_DEFINITION_SHAPE($,$,#615);
#71845=PRODUCT_DEFINITION_SHAPE($,$,#616);
#71846=PRODUCT_DEFINITION_SHAPE($,$,#617);
#71847=PRODUCT_DEFINITION_SHAPE($,$,#618);
#71848=PRODUCT_DEFINITION_SHAPE($,$,#619);
#71849=PRODUCT_DEFINITION_SHAPE($,$,#620);
#71850=PRODUCT_DEFINITION_SHAPE($,$,#621);
#71851=PRODUCT_DEFINITION_SHAPE($,$,#622);
#71852=PRODUCT_DEFINITION_SHAPE($,$,#623);
#71853=PRODUCT_DEFINITION_SHAPE($,$,#624);
#71854=PRODUCT_DEFINITION_SHAPE($,$,#625);
#71855=PRODUCT_DEFINITION_SHAPE($,$,#626);
#71856=PRODUCT_DEFINITION_SHAPE($,$,#627);
#71857=PRODUCT_DEFINITION_SHAPE($,$,#628);
#71858=PRODUCT_DEFINITION_SHAPE($,$,#629);
#71859=PRODUCT_DEFINITION_SHAPE($,$,#630);
#71860=PRODUCT_DEFINITION_SHAPE($,$,#631);
#71861=PRODUCT_DEFINITION_SHAPE($,$,#632);
#71862=PRODUCT_DEFINITION_SHAPE($,$,#633);
#71863=PRODUCT_DEFINITION_SHAPE($,$,#634);
#71864=PRODUCT_DEFINITION_SHAPE($,$,#635);
#71865=PRODUCT_DEFINITION_SHAPE($,$,#636);
#71866=PRODUCT_DEFINITION_SHAPE($,$,#637);
#71867=PRODUCT_DEFINITION_SHAPE($,$,#638);
#71868=PRODUCT_DEFINITION_SHAPE($,$,#639);
#71869=PRODUCT_DEFINITION_SHAPE($,$,#640);
#71870=PRODUCT_DEFINITION_SHAPE($,$,#641);
#71871=PRODUCT_DEFINITION_SHAPE($,$,#642);
#71872=PRODUCT_DEFINITION_SHAPE($,$,#643);
#71873=PRODUCT_DEFINITION_SHAPE($,$,#644);
#71874=PRODUCT_DEFINITION_SHAPE($,$,#645);
#71875=PRODUCT_DEFINITION_SHAPE($,$,#646);
#71876=PRODUCT_DEFINITION_SHAPE($,$,#647);
#71877=PRODUCT_DEFINITION_SHAPE($,$,#648);
#71878=PRODUCT_DEFINITION_SHAPE($,$,#649);
#71879=PRODUCT_DEFINITION_SHAPE($,$,#650);
#71880=PRODUCT_DEFINITION_SHAPE($,$,#651);
#71881=PRODUCT_DEFINITION_SHAPE($,$,#652);
#71882=PRODUCT_DEFINITION_SHAPE($,$,#653);
#71883=PRODUCT_DEFINITION_SHAPE($,$,#654);
#71884=PRODUCT_DEFINITION_SHAPE($,$,#655);
#71885=PRODUCT_DEFINITION_SHAPE($,$,#656);
#71886=PRODUCT_DEFINITION_SHAPE($,$,#657);
#71887=PRODUCT_DEFINITION_SHAPE($,$,#658);
#71888=PRODUCT_DEFINITION_SHAPE($,$,#659);
#71889=PRODUCT_DEFINITION_SHAPE($,$,#660);
#71890=PRODUCT_DEFINITION_SHAPE($,$,#661);
#71891=PRODUCT_DEFINITION_SHAPE($,$,#662);
#71892=PRODUCT_DEFINITION_SHAPE($,$,#663);
#71893=PRODUCT_DEFINITION_SHAPE($,$,#664);
#71894=PRODUCT_DEFINITION_SHAPE($,$,#665);
#71895=PRODUCT_DEFINITION_SHAPE($,$,#666);
#71896=PRODUCT_DEFINITION_SHAPE($,$,#667);
#71897=PRODUCT_DEFINITION_SHAPE($,$,#668);
#71898=PRODUCT_DEFINITION_SHAPE($,$,#669);
#71899=PRODUCT_DEFINITION_SHAPE($,$,#670);
#71900=PRODUCT_DEFINITION_SHAPE($,$,#671);
#71901=PRODUCT_DEFINITION_SHAPE($,$,#672);
#71902=PRODUCT_DEFINITION_SHAPE($,$,#673);
#71903=PRODUCT_DEFINITION_SHAPE($,$,#674);
#71904=PRODUCT_DEFINITION_SHAPE($,$,#675);
#71905=PRODUCT_DEFINITION_SHAPE($,$,#676);
#71906=PRODUCT_DEFINITION_SHAPE($,$,#677);
#71907=PRODUCT_DEFINITION_SHAPE($,$,#678);
#71908=PRODUCT_DEFINITION_SHAPE($,$,#679);
#71909=PRODUCT_DEFINITION_SHAPE($,$,#680);
#71910=PRODUCT_DEFINITION_SHAPE($,$,#681);
#71911=PRODUCT_DEFINITION_SHAPE($,$,#682);
#71912=PRODUCT_DEFINITION_SHAPE($,$,#683);
#71913=PRODUCT_DEFINITION_SHAPE($,$,#684);
#71914=PRODUCT_DEFINITION_SHAPE($,$,#685);
#71915=PRODUCT_DEFINITION_SHAPE($,$,#686);
#71916=PRODUCT_DEFINITION_SHAPE($,$,#687);
#71917=PRODUCT_DEFINITION_SHAPE($,$,#688);
#71918=PRODUCT_DEFINITION_SHAPE($,$,#689);
#71919=PRODUCT_DEFINITION_SHAPE($,$,#690);
#71920=PRODUCT_DEFINITION_SHAPE($,$,#691);
#71921=PRODUCT_DEFINITION_SHAPE($,$,#692);
#71922=PRODUCT_DEFINITION_SHAPE($,$,#693);
#71923=PRODUCT_DEFINITION_SHAPE($,$,#694);
#71924=PRODUCT_DEFINITION_SHAPE($,$,#695);
#71925=PRODUCT_DEFINITION_SHAPE($,$,#696);
#71926=PRODUCT_DEFINITION_SHAPE($,$,#697);
#71927=PRODUCT_DEFINITION_SHAPE($,$,#698);
#71928=PRODUCT_DEFINITION_SHAPE($,$,#699);
#71929=PRODUCT_DEFINITION_SHAPE($,$,#700);
#71930=PRODUCT_DEFINITION_SHAPE($,$,#701);
#71931=PRODUCT_DEFINITION_SHAPE($,$,#702);
#71932=PRODUCT_DEFINITION_SHAPE($,$,#703);
#71933=PRODUCT_DEFINITION_SHAPE($,$,#704);
#71934=PRODUCT_DEFINITION_SHAPE($,$,#705);
#71935=PRODUCT_DEFINITION_SHAPE($,$,#706);
#71936=PRODUCT_DEFINITION_SHAPE($,$,#707);
#71937=PRODUCT_DEFINITION_SHAPE($,$,#708);
#71938=PRODUCT_DEFINITION_SHAPE($,$,#709);
#71939=PRODUCT_DEFINITION_SHAPE($,$,#710);
#71940=PRODUCT_DEFINITION_SHAPE($,$,#711);
#71941=PRODUCT_DEFINITION_SHAPE($,$,#712);
#71942=PRODUCT_DEFINITION_SHAPE($,$,#713);
#71943=PRODUCT_DEFINITION_SHAPE($,$,#714);
#71944=PRODUCT_DEFINITION_SHAPE($,$,#715);
#71945=PRODUCT_DEFINITION_SHAPE($,$,#716);
#71946=PRODUCT_DEFINITION_SHAPE($,$,#717);
#71947=PRODUCT_DEFINITION_SHAPE($,$,#718);
#71948=PRODUCT_DEFINITION_SHAPE($,$,#719);
#71949=PRODUCT_DEFINITION_SHAPE($,$,#720);
#71950=PRODUCT_DEFINITION_SHAPE($,$,#721);
#71951=PRODUCT_DEFINITION_SHAPE($,$,#722);
#71952=PRODUCT_DEFINITION_SHAPE($,$,#723);
#71953=PRODUCT_DEFINITION_SHAPE($,$,#724);
#71954=PRODUCT_DEFINITION_SHAPE($,$,#725);
#71955=PRODUCT_DEFINITION_SHAPE($,$,#726);
#71956=PRODUCT_DEFINITION_SHAPE($,$,#727);
#71957=PRODUCT_DEFINITION_SHAPE($,$,#728);
#71958=PRODUCT_DEFINITION_SHAPE($,$,#729);
#71959=PRODUCT_DEFINITION_SHAPE($,$,#730);
#71960=PRODUCT_DEFINITION_SHAPE($,$,#731);
#71961=PRODUCT_DEFINITION_SHAPE($,$,#732);
#71962=PRODUCT_DEFINITION_SHAPE($,$,#733);
#71963=PRODUCT_DEFINITION_SHAPE($,$,#734);
#71964=PRODUCT_DEFINITION_SHAPE($,$,#735);
#71965=PRODUCT_DEFINITION_SHAPE($,$,#736);
#71966=PRODUCT_DEFINITION_SHAPE($,$,#737);
#71967=PRODUCT_DEFINITION_SHAPE($,$,#738);
#71968=PRODUCT_DEFINITION_SHAPE($,$,#739);
#71969=PRODUCT_DEFINITION_SHAPE($,$,#740);
#71970=PRODUCT_DEFINITION_SHAPE($,$,#741);
#71971=PRODUCT_DEFINITION_SHAPE($,$,#742);
#71972=PRODUCT_DEFINITION_SHAPE($,$,#743);
#71973=PRODUCT_DEFINITION_SHAPE($,$,#744);
#71974=PRODUCT_DEFINITION_SHAPE($,$,#745);
#71975=PRODUCT_DEFINITION_SHAPE($,$,#746);
#71976=PRODUCT_DEFINITION_SHAPE($,$,#747);
#71977=PRODUCT_DEFINITION_SHAPE($,$,#748);
#71978=PRODUCT_DEFINITION_SHAPE($,$,#749);
#71979=PRODUCT_DEFINITION_SHAPE($,$,#750);
#71980=PRODUCT_DEFINITION_SHAPE($,$,#751);
#71981=PRODUCT_DEFINITION_SHAPE($,$,#752);
#71982=PRODUCT_DEFINITION_SHAPE($,$,#753);
#71983=PRODUCT_DEFINITION_SHAPE($,$,#754);
#71984=PRODUCT_DEFINITION_SHAPE($,$,#755);
#71985=PRODUCT_DEFINITION_SHAPE($,$,#756);
#71986=PRODUCT_DEFINITION_SHAPE($,$,#757);
#71987=PRODUCT_DEFINITION_SHAPE($,$,#758);
#71988=PRODUCT_DEFINITION_SHAPE($,$,#759);
#71989=PRODUCT_DEFINITION_SHAPE($,$,#760);
#71990=PRODUCT_DEFINITION_SHAPE($,$,#761);
#71991=PRODUCT_DEFINITION_SHAPE($,$,#762);
#71992=PRODUCT_DEFINITION_SHAPE($,$,#763);
#71993=PRODUCT_DEFINITION_SHAPE($,$,#764);
#71994=PRODUCT_DEFINITION_SHAPE($,$,#765);
#71995=PRODUCT_DEFINITION_SHAPE($,$,#766);
#71996=PRODUCT_DEFINITION_SHAPE($,$,#767);
#71997=PRODUCT_DEFINITION_SHAPE($,$,#768);
#71998=PRODUCT_DEFINITION_SHAPE($,$,#769);
#71999=PRODUCT_DEFINITION_SHAPE($,$,#770);
#72000=PRODUCT_DEFINITION_SHAPE($,$,#771);
#72001=PRODUCT_DEFINITION_SHAPE($,$,#772);
#72002=PRODUCT_DEFINITION_SHAPE($,$,#773);
#72003=PRODUCT_DEFINITION_SHAPE($,$,#774);
#72004=PRODUCT_DEFINITION_SHAPE($,$,#775);
#72005=PRODUCT_DEFINITION_SHAPE($,$,#776);
#72006=PRODUCT_DEFINITION_SHAPE($,$,#777);
#72007=PRODUCT_DEFINITION_SHAPE($,$,#778);
#72008=PRODUCT_DEFINITION_SHAPE($,$,#779);
#72009=PRODUCT_DEFINITION_SHAPE($,$,#780);
#72010=PRODUCT_DEFINITION_SHAPE($,$,#781);
#72011=PRODUCT_DEFINITION_SHAPE($,$,#782);
#72012=PRODUCT_DEFINITION_SHAPE($,$,#783);
#72013=PRODUCT_DEFINITION_SHAPE($,$,#784);
#72014=PRODUCT_DEFINITION_SHAPE($,$,#785);
#72015=PRODUCT_DEFINITION_SHAPE($,$,#786);
#72016=SHAPE_REPRESENTATION('',(#13756,#14849,#14850,#14851,#14852,#14853,
#14854,#14855,#14856,#14857,#14858,#14859,#14860,#14861,#14862,#14863,#14864,
#14865,#14866,#14867,#14868,#14869,#14870,#14871,#14872,#14873,#14874,#14875,
#14876,#14877,#14878,#14879,#14880,#14881,#14882,#14883,#14884,#14885,#14886,
#14887,#14888,#14889,#14890,#14891,#14892,#14893,#14894,#14895,#14896,#14897,
#14898,#14899,#14900,#14901,#14902,#14903,#14904,#14905,#14906,#14907,#14908,
#14909,#14910,#14911,#14912,#14913,#14914,#14915,#14916,#14917,#14918,#14919,
#14920,#14921,#14922,#14923,#14924,#14925,#14926,#14927,#14928,#14929,#14930,
#14931,#14932,#14933,#14934,#14935,#14936,#14937,#14938,#14939,#14940,#14941,
#14942,#14943,#14944,#14945,#14946,#14947,#14948,#14949,#14950,#14951,#14952,
#14953,#14954,#14955,#14956,#14957,#14958,#14959,#14960,#14961,#14962,#14963,
#14964,#14965,#14966,#14967,#14968,#14969,#14970,#14971,#14972,#14973,#14974,
#14975,#14976,#14977,#14978,#14979,#14980,#14981,#14982,#14983,#14984,#14985,
#14986,#14987,#14988,#14989,#14990,#14991,#14992,#14993,#14994,#14995,#14996,
#14997,#14998,#14999,#15000,#15001,#15002,#15003,#15004,#15005,#15006,#15007,
#15008,#15009,#15010,#15011,#15012,#15013,#15014,#15015,#15016,#15017,#15018,
#15019,#15020,#15021,#15022,#15023,#15024,#15025,#15026,#15027,#15028,#15029,
#15030,#15031,#15032,#15033,#15034,#15035,#15036,#15037,#15038,#15039,#15040,
#15041,#15042),#71784);
#72017=SHAPE_REPRESENTATION('',(#13757),#71785);
#72018=SHAPE_REPRESENTATION('',(#13854),#71786);
#72019=SHAPE_REPRESENTATION('',(#13993),#71787);
#72020=SHAPE_REPRESENTATION('',(#14012),#71788);
#72021=SHAPE_REPRESENTATION('',(#14045),#71789);
#72022=SHAPE_REPRESENTATION('',(#14060),#71790);
#72023=SHAPE_REPRESENTATION('',(#14111),#71791);
#72024=SHAPE_REPRESENTATION('',(#14114),#71792);
#72025=SHAPE_REPRESENTATION('',(#14358),#71793);
#72026=SHAPE_REPRESENTATION('',(#14610),#71794);
#72027=PRODUCT_DEFINITION_CONTEXT('part definition',#72062,'design');
#72028=PRODUCT_DEFINITION('MAS-259',
'MAS-259',#72039,#72027);
#72029=PRODUCT_DEFINITION('Dual Shaft Rail Support x 180',
'Dual Shaft Rail Support x 180',#72040,#72027);
#72030=PRODUCT_DEFINITION('Modular Carriage Plate 4.5 x 4.5',
'Modular Carriage Plate 4.5 x 4.5',#72041,#72027);
#72031=PRODUCT_DEFINITION('Hardened Ground Chrome Shaft 0.500 in x 180',
'Hardened Ground Chrome Shaft 0.500 in x 180',#72042,#72027);
#72032=PRODUCT_DEFINITION('Open Pillow Block Bushing Housing',
'Open Pillow Block Bushing Housing',#72043,#72027);
#72033=PRODUCT_DEFINITION('Super Smart Ball Bushing Open Sleeve',
'Super Smart Ball Bushing Open Sleeve',#72044,#72027);
#72034=PRODUCT_DEFINITION('Super Smart Ball Retainer',
'Super Smart Ball Retainer',#72045,#72027);
#72035=PRODUCT_DEFINITION('Steel Ball 3-32 in','Steel Ball 3-32 in',#72046,
#72027);
#72036=PRODUCT_DEFINITION('ASME B18.3 SHCS 10-32 UNF x 0.625',
'ASME B18.3 SHCS 10-32 UNF x 0.625',#72047,#72027);
#72037=PRODUCT_DEFINITION('ASME B18.3 SHCS 10-32 UNF x 0.875',
'ASME B18.3 SHCS 10-32 UNF x 0.875',#72048,#72027);
#72038=PRODUCT_DEFINITION('ASME B18.3 SHCS 1-4-20 UNC x 0.75',
'ASME B18.3 SHCS 1-4-20 UNC x 0.75',#72049,#72027);
#72039=PRODUCT_DEFINITION_FORMATION('',$,#72064);
#72040=PRODUCT_DEFINITION_FORMATION('',$,#72065);
#72041=PRODUCT_DEFINITION_FORMATION('',$,#72066);
#72042=PRODUCT_DEFINITION_FORMATION('',$,#72067);
#72043=PRODUCT_DEFINITION_FORMATION('',$,#72068);
#72044=PRODUCT_DEFINITION_FORMATION('',$,#72069);
#72045=PRODUCT_DEFINITION_FORMATION('',$,#72070);
#72046=PRODUCT_DEFINITION_FORMATION('',$,#72071);
#72047=PRODUCT_DEFINITION_FORMATION('',$,#72072);
#72048=PRODUCT_DEFINITION_FORMATION('',$,#72073);
#72049=PRODUCT_DEFINITION_FORMATION('',$,#72074);
#72050=PRODUCT_RELATED_PRODUCT_CATEGORY(
'MAS-259','MAS-259',(#72064));
#72051=PRODUCT_RELATED_PRODUCT_CATEGORY('Dual Shaft Rail Support x 180',
'Dual Shaft Rail Support x 180',(#72065));
#72052=PRODUCT_RELATED_PRODUCT_CATEGORY(
'Modular Carriage Plate 4.5 x 4.5','Modular Carriage Plate 4.5 x 4.5',(#72066));
#72053=PRODUCT_RELATED_PRODUCT_CATEGORY(
'Hardened Ground Chrome Shaft 0.500 in x 180',
'Hardened Ground Chrome Shaft 0.500 in x 180',(#72067));
#72054=PRODUCT_RELATED_PRODUCT_CATEGORY(
'Open Pillow Block Bushing Housing','Open Pillow Block Bushing Housing',
(#72068));
#72055=PRODUCT_RELATED_PRODUCT_CATEGORY(
'Super Smart Ball Bushing Open Sleeve',
'Super Smart Ball Bushing Open Sleeve',(#72069));
#72056=PRODUCT_RELATED_PRODUCT_CATEGORY('Super Smart Ball Retainer',
'Super Smart Ball Retainer',(#72070));
#72057=PRODUCT_RELATED_PRODUCT_CATEGORY('Steel Ball 3-32 in',
'Steel Ball 3-32 in',(#72071));
#72058=PRODUCT_RELATED_PRODUCT_CATEGORY(
'ASME B18.3 SHCS 10-32 UNF x 0.625','ASME B18.3 SHCS 10-32 UNF x 0.625',
(#72072));
#72059=PRODUCT_RELATED_PRODUCT_CATEGORY(
'ASME B18.3 SHCS 10-32 UNF x 0.875','ASME B18.3 SHCS 10-32 UNF x 0.875',
(#72073));
#72060=PRODUCT_RELATED_PRODUCT_CATEGORY(
'ASME B18.3 SHCS 1-4-20 UNC x 0.75','ASME B18.3 SHCS 1-4-20 UNC x 0.75',
(#72074));
#72061=APPLICATION_PROTOCOL_DEFINITION('international standard',
'automotive_design',2009,#72062);
#72062=APPLICATION_CONTEXT(
'Core Data for Automotive Mechanical Design Process');
#72063=PRODUCT_CONTEXT('part definition',#72062,'mechanical');
#72064=PRODUCT('MAS-259',
'MAS-259',$,(#72063));
#72065=PRODUCT('Dual Shaft Rail Support x 180',
'Dual Shaft Rail Support x 180',$,(#72063));
#72066=PRODUCT('Modular Carriage Plate 4.5 x 4.5',
'Modular Carriage Plate 4.5 x 4.5',$,(#72063));
#72067=PRODUCT('Hardened Ground Chrome Shaft 0.500 in x 180',
'Hardened Ground Chrome Shaft 0.500 in x 180',$,(#72063));
#72068=PRODUCT('Open Pillow Block Bushing Housing',
'Open Pillow Block Bushing Housing',$,(#72063));
#72069=PRODUCT('Super Smart Ball Bushing Open Sleeve',
'Super Smart Ball Bushing Open Sleeve',$,(#72063));
#72070=PRODUCT('Super Smart Ball Retainer','Super Smart Ball Retainer',
$,(#72063));
#72071=PRODUCT('Steel Ball 3-32 in','Steel Ball 3-32 in',$,(#72063));
#72072=PRODUCT('ASME B18.3 SHCS 10-32 UNF x 0.625',
'ASME B18.3 SHCS 10-32 UNF x 0.625',$,(#72063));
#72073=PRODUCT('ASME B18.3 SHCS 10-32 UNF x 0.875',
'ASME B18.3 SHCS 10-32 UNF x 0.875',$,(#72063));
#72074=PRODUCT('ASME B18.3 SHCS 1-4-20 UNC x 0.75',
'ASME B18.3 SHCS 1-4-20 UNC x 0.75',$,(#72063));
#72075=PRESENTATION_STYLE_ASSIGNMENT((#72086));
#72076=PRESENTATION_STYLE_ASSIGNMENT((#72087));
#72077=PRESENTATION_STYLE_ASSIGNMENT((#72088));
#72078=PRESENTATION_STYLE_ASSIGNMENT((#72089));
#72079=PRESENTATION_STYLE_ASSIGNMENT((#72090));
#72080=PRESENTATION_STYLE_ASSIGNMENT((#72091));
#72081=PRESENTATION_STYLE_ASSIGNMENT((#72092));
#72082=PRESENTATION_STYLE_ASSIGNMENT((#72093));
#72083=PRESENTATION_STYLE_ASSIGNMENT((#72094));
#72084=PRESENTATION_STYLE_ASSIGNMENT((#72095));
#72085=PRESENTATION_STYLE_ASSIGNMENT((#72096));
#72086=SURFACE_STYLE_USAGE(.BOTH.,#72097);
#72087=SURFACE_STYLE_USAGE(.BOTH.,#72098);
#72088=SURFACE_STYLE_USAGE(.BOTH.,#72099);
#72089=SURFACE_STYLE_USAGE(.BOTH.,#72100);
#72090=SURFACE_STYLE_USAGE(.BOTH.,#72101);
#72091=SURFACE_STYLE_USAGE(.BOTH.,#72102);
#72092=SURFACE_STYLE_USAGE(.BOTH.,#72103);
#72093=SURFACE_STYLE_USAGE(.BOTH.,#72104);
#72094=SURFACE_STYLE_USAGE(.BOTH.,#72105);
#72095=SURFACE_STYLE_USAGE(.BOTH.,#72106);
#72096=SURFACE_STYLE_USAGE(.BOTH.,#72107);
#72097=SURFACE_SIDE_STYLE('',(#72108));
#72098=SURFACE_SIDE_STYLE('',(#72109));
#72099=SURFACE_SIDE_STYLE('',(#72110));
#72100=SURFACE_SIDE_STYLE('',(#72111));
#72101=SURFACE_SIDE_STYLE('',(#72112));
#72102=SURFACE_SIDE_STYLE('',(#72113));
#72103=SURFACE_SIDE_STYLE('',(#72114));
#72104=SURFACE_SIDE_STYLE('',(#72115));
#72105=SURFACE_SIDE_STYLE('',(#72116));
#72106=SURFACE_SIDE_STYLE('',(#72117));
#72107=SURFACE_SIDE_STYLE('',(#72118));
#72108=SURFACE_STYLE_FILL_AREA(#72119);
#72109=SURFACE_STYLE_FILL_AREA(#72120);
#72110=SURFACE_STYLE_FILL_AREA(#72121);
#72111=SURFACE_STYLE_FILL_AREA(#72122);
#72112=SURFACE_STYLE_FILL_AREA(#72123);
#72113=SURFACE_STYLE_FILL_AREA(#72124);
#72114=SURFACE_STYLE_FILL_AREA(#72125);
#72115=SURFACE_STYLE_FILL_AREA(#72126);
#72116=SURFACE_STYLE_FILL_AREA(#72127);
#72117=SURFACE_STYLE_FILL_AREA(#72128);
#72118=SURFACE_STYLE_FILL_AREA(#72129);
#72119=FILL_AREA_STYLE('Steel - Satin',(#72130));
#72120=FILL_AREA_STYLE('Opaque(206,210,216)',(#72131));
#72121=FILL_AREA_STYLE('Opaque(222,225,230)',(#72132));
#72122=FILL_AREA_STYLE('Opaque(236,238,241)',(#72133));
#72123=FILL_AREA_STYLE('Opaque(214,217,222)',(#72134));
#72124=FILL_AREA_STYLE('Opaque(226,229,233)',(#72135));
#72125=FILL_AREA_STYLE('Opaque(70,72,76)',(#72136));
#72126=FILL_AREA_STYLE('Opaque(240,241,243)',(#72137));
#72127=FILL_AREA_STYLE('Opaque(199,204,210)',(#72138));
#72128=FILL_AREA_STYLE('Opaque(201,205,211)',(#72139));
#72129=FILL_AREA_STYLE('Opaque(196,201,207)',(#72140));
#72130=FILL_AREA_STYLE_COLOUR('Steel - Satin',#72141);
#72131=FILL_AREA_STYLE_COLOUR('Opaque(206,210,216)',#72142);
#72132=FILL_AREA_STYLE_COLOUR('Opaque(222,225,230)',#72143);
#72133=FILL_AREA_STYLE_COLOUR('Opaque(236,238,241)',#72144);
#72134=FILL_AREA_STYLE_COLOUR('Opaque(214,217,222)',#72145);
#72135=FILL_AREA_STYLE_COLOUR('Opaque(226,229,233)',#72146);
#72136=FILL_AREA_STYLE_COLOUR('Opaque(70,72,76)',#72147);
#72137=FILL_AREA_STYLE_COLOUR('Opaque(240,241,243)',#72148);
#72138=FILL_AREA_STYLE_COLOUR('Opaque(199,204,210)',#72149);
#72139=FILL_AREA_STYLE_COLOUR('Opaque(201,205,211)',#72150);
#72140=FILL_AREA_STYLE_COLOUR('Opaque(196,201,207)',#72151);
#72141=COLOUR_RGB('Steel - Satin', 0.09019608, 0.27058824, 0.51372549);
#72142=COLOUR_RGB('Opaque(206,210,216)', 0.09019608, 0.27058824, 0.51372549);
#72143=COLOUR_RGB('Opaque(222,225,230)', 0.66274510, 0.83137255, 0.94901961);
#72144=COLOUR_RGB('Opaque(236,238,241)', 0.31764706, 0.68627451, 0.89019608);
#72145=COLOUR_RGB('Opaque(214,217,222)', 0.40784314, 0.44705882, 0.49803922);
#72146=COLOUR_RGB('Opaque(226,229,233)', 0.72549020, 0.75294118, 0.79215686);
#72147=COLOUR_RGB('Opaque(70,72,76)', 0.08235294, 0.09019608, 0.10196078);
#72148=COLOUR_RGB('Opaque(240,241,243)', 0.09019608, 0.27058824, 0.51372549);
#72149=COLOUR_RGB('Opaque(199,204,210)', 0.66274510, 0.83137255, 0.94901961);
#72150=COLOUR_RGB('Opaque(201,205,211)', 0.31764706, 0.68627451, 0.89019608);
#72151=COLOUR_RGB('Opaque(196,201,207)', 0.40784314, 0.44705882, 0.49803922);
ENDSEC;
END-ISO-10303-21;
